#88047=DIRECTION('center_axis',(-0.0980734470899598,0.987363722027219,-0.124476822744034));
#88048=DIRECTION('ref_axis',(-0.744510117580016,0.0102046851999408,0.667533182112291));
#88049=DIRECTION('',(0.160317479600262,0.,-0.987065502251304));
#88050=DIRECTION('center_axis',(5.51791714416026E-15,-1.,-4.96514234470038E-15));
#88051=DIRECTION('ref_axis',(1.,5.51791714416026E-15,-2.12802080022765E-32));
#88052=DIRECTION('center_axis',(-0.0798423016345343,-0.987363723490078,
-0.136887122862264));
#88053=DIRECTION('ref_axis',(-0.793512025280663,-0.020156453595699,0.60822066975188));
#88054=DIRECTION('center_axis',(0.115688518554701,-0.987363722502104,0.10830072096439));
#88055=DIRECTION('ref_axis',(-0.741540431297166,-0.0133103684642173,0.6707761346701));
#88056=DIRECTION('center_axis',(0.0995325357866225,0.987363722369425,0.123313235577846));
#88057=DIRECTION('ref_axis',(-0.692946129975743,-0.0201568006358742,0.720707544250625));
#88058=DIRECTION('',(-0.998451978423991,0.,0.0556205607776269));
#88059=DIRECTION('center_axis',(-0.122539379018189,0.987363722035633,-0.100483734991179));
#88060=DIRECTION('ref_axis',(-0.583603983803612,0.0102046893186796,0.811974294177138));
#88061=DIRECTION('',(-0.0556205582211081,0.,-0.998451978566407));
#88062=DIRECTION('center_axis',(-1.72862098727961E-14,-1.,2.41409965901936E-14));
#88063=DIRECTION('ref_axis',(9.88397516767577E-33,-2.41409965901936E-14,
-1.));
#88064=DIRECTION('center_axis',(-0.107402317354723,-0.987363723483623,-0.116523043967242));
#88065=DIRECTION('ref_axis',(-0.644210689681965,-0.0201564546481271,0.764582438089906));
#88066=DIRECTION('center_axis',(0.136265238378703,-0.987363722512312,0.0808990993536073));
#88067=DIRECTION('ref_axis',(-0.580006587686311,-0.0133103675608265,0.814503033975858));
#88068=DIRECTION('center_axis',(0.123714219117736,0.987363722312337,0.0990336904776107));
#88069=DIRECTION('ref_axis',(-0.521814617623308,-0.0201568038489919,0.852820736200307));
#88070=DIRECTION('',(-0.963151949602078,0.,0.268957844239047));
#88071=DIRECTION('center_axis',(-0.141275510311441,0.987363722055667,-0.0717921343506458));
#88072=DIRECTION('ref_axis',(-0.395409175669361,0.0102046865097965,0.918448391674629));
#88073=DIRECTION('',(-0.268957842517579,0.,-0.963151950082794));
#88074=DIRECTION('center_axis',(-2.92311680908922E-15,-1.,6.8231544174374E-15));
#88075=DIRECTION('ref_axis',(2.66748257699467E-34,-6.8231544174374E-15,
-1.));
#88076=DIRECTION('center_axis',(-0.129940323516781,-0.987363723620263,-0.0907104712978803));
#88077=DIRECTION('ref_axis',(-0.464786779218364,-0.020156448623246,0.885193180860945));
#88078=DIRECTION('center_axis',(0.15047034847597,-0.987363722496393,0.0497147234487595));
#88079=DIRECTION('ref_axis',(-0.391352279647315,-0.0133103692467653,0.920144677366209));
#88080=DIRECTION('center_axis',(0.142111168500603,0.987363722413081,0.0701234301070469));
#88081=DIRECTION('ref_axis',(-0.326283630981388,-0.0201567959017054,0.945056980151238));
#88082=DIRECTION('',(-0.882816006173181,0.,0.469718957723056));
#88083=DIRECTION('center_axis',(-0.153405753362529,0.987363721980081,-0.0397436202794466));
#88084=DIRECTION('ref_axis',(-0.188725472417248,0.0102046916293933,0.981976863439071));
#88085=DIRECTION('',(-0.469718957703103,0.,-0.882816006183797));
#88086=DIRECTION('center_axis',(-5.55199781974273E-15,-1.,2.91680662988243E-14));
#88087=DIRECTION('ref_axis',(2.33192543151121E-32,-2.91680662988243E-14,
-1.));
#88088=DIRECTION('center_axis',(-0.146402458494853,-0.98736372329281,-0.0606563934966637));
#88089=DIRECTION('ref_axis',(-0.263629954398167,-0.0201564602306307,0.964413274615707));
#88090=DIRECTION('center_axis',(0.157639630785437,-0.987363722515614,0.0162057479290574));
#88091=DIRECTION('ref_axis',(-0.184398776981366,-0.013310365432533,0.982761377558067));
#88092=DIRECTION('center_axis',(0.153863152643811,0.987363722405411,0.0379342844434553));
#88093=DIRECTION('ref_axis',(-0.115495988358612,-0.0201567971821641,0.993103408613838));
#88094=DIRECTION('',(-0.761200566737353,0.,0.648516535794372));
#88095=DIRECTION('center_axis',(4.24038427100572E-16,-1.,1.48398242449089E-14));
#88096=DIRECTION('ref_axis',(0.0285626985677906,1.48458813213445E-14,0.999592002894444));
#88097=DIRECTION('center_axis',(-0.156018981952462,-0.987363723488661,-0.027766072987104));
#88098=DIRECTION('ref_axis',(-0.0501460873759626,-0.020156453209744,0.998538475630702));
#88099=DIRECTION('center_axis',(0.157437859804754,-0.987363722525233,-0.0180610005596111));
#88100=DIRECTION('ref_axis',(0.0311770128597521,-0.0133103713432087,0.999425248772438));
#88101=DIRECTION('center_axis',(-0.15836291534669,0.987363722037061,-0.00583673264922174));
#88102=DIRECTION('ref_axis',(0.0267828210981455,0.0102046897763596,0.999589188017054));
#88103=DIRECTION('',(-0.648516533598721,0.,-0.761200568607971));
#88104=DIRECTION('center_axis',(-0.152772347587519,-0.987363722802381,-0.0421128092914994));
#88105=DIRECTION('ref_axis',(-0.157501995156474,-0.0177427248486509,0.98735926452162));
#88106=DIRECTION('',(0.562367402337263,0.,0.826887480125585));
#88107=DIRECTION('',(0.826887478900179,0.,-0.562367404139061));
#88108=DIRECTION('center_axis',(0.154431764554222,-0.987363722245923,0.0355487002483153));
#88109=DIRECTION('ref_axis',(-0.290069428666578,-0.0109157762395627,0.956943348575104));
#88110=DIRECTION('center_axis',(-0.140147600738479,-0.987363722297262,-0.073969790445442));
#88111=DIRECTION('ref_axis',(-0.366072744817863,-0.017742741678619,0.930417078851867));
#88112=DIRECTION('',(0.371463198744195,1.74545579967425E-14,0.928447678643622));
#88113=DIRECTION('center_axis',(-6.93975744812286E-14,-1.,2.27170476996506E-13));
#88114=DIRECTION('ref_axis',(-2.59199074825716E-30,-2.27170476996506E-13,
-1.));
#88115=DIRECTION('center_axis',(0.149682997529586,0.98736372254829,0.0520372909185504));
#88116=DIRECTION('ref_axis',(-0.221888126663152,-0.0177430369618895,0.974910685081093));
#88117=DIRECTION('center_axis',(-0.147323592067659,0.987363722382119,-0.0583835502860794));
#88118=DIRECTION('ref_axis',(-0.294137870802051,0.0126220186732162,0.955679652187201));
#88119=DIRECTION('',(0.928447676446041,0.,-0.371463204236903));
#88120=DIRECTION('center_axis',(0.14317931371119,-0.987363722302444,0.0679158597549498));
#88121=DIRECTION('ref_axis',(-0.489002301735146,-0.0109157720263509,0.872214190906567));
#88122=DIRECTION('center_axis',(-0.120969709374198,-0.987363722292978,-0.102368009229828));
#88123=DIRECTION('ref_axis',(-0.557526335016047,-0.0177427418820099,0.829969626476827));
#88124=DIRECTION('',(0.163189789191805,1.74545580137922E-14,0.986594695254102));
#88125=DIRECTION('center_axis',(1.45762543762546E-14,-1.,-2.58676162557461E-14));
#88126=DIRECTION('ref_axis',(5.47887179583638E-31,2.58676162557461E-14,
-1.));
#88127=DIRECTION('center_axis',(0.134997009526047,0.987363722493814,0.0829981139676269));
#88128=DIRECTION('ref_axis',(-0.426277486400253,-0.0177430437136482,0.904418425834004));
#88129=DIRECTION('center_axis',(-0.131328509014908,0.987363722362473,-0.0886887956984518));
#88130=DIRECTION('ref_axis',(-0.492703966323166,0.0126220221773717,0.87010544540623));
#88131=DIRECTION('',(0.986594694898509,0.,-0.16318979134161));
#88132=DIRECTION('center_axis',(0.125231962048202,-0.987363722236187,0.0971073410894351));
#88133=DIRECTION('ref_axis',(-0.665069967527274,-0.0109157769681648,0.746701268317158));
#88134=DIRECTION('center_axis',(-0.0961354101537728,-0.98736372234748,-0.125979612266014));
#88135=DIRECTION('ref_axis',(-0.72291061702561,-0.0177427394115162,0.690713714204247));
#88136=DIRECTION('',(-0.0527141905833193,1.74545580647872E-14,0.998609640505811));
#88137=DIRECTION('center_axis',(0.,-1.,0.));
#88138=DIRECTION('ref_axis',(0.,0.,-1.));
#88139=DIRECTION('center_axis',(0.113998717626461,0.987363722533795,0.110078025980343));
#88140=DIRECTION('ref_axis',(-0.610734581675629,-0.0177430374931817,0.791636567729163));
#88141=DIRECTION('center_axis',(-0.109192650142314,0.987363722346366,-0.114847050241731));
#88142=DIRECTION('ref_axis',(-0.668231773767008,0.0126220244917432,0.743846073476179));
#88143=DIRECTION('',(0.998609640477331,0.,0.0527141911228425));
#88144=DIRECTION('center_axis',(0.10142890137495,-0.987363722244127,0.121758194640415));
#88145=DIRECTION('ref_axis',(-0.810039701366378,-0.0109157780792778,0.586273424264817));
#88146=DIRECTION('center_axis',(-0.0668059229653221,-0.98736372227003,-0.143700551849403));
#88147=DIRECTION('ref_axis',(-0.854492399176007,-0.0177427420873099,0.519160798648795));
#88148=DIRECTION('',(-0.266153317126965,1.74545580075932E-14,0.963930709015079));
#88149=DIRECTION('center_axis',(-7.22717411294479E-14,-1.,5.20692070645034E-14));
#88150=DIRECTION('ref_axis',(1.,-7.22717411294479E-14,-4.37574147480012E-31));
#88151=DIRECTION('center_axis',(0.0876699694622647,0.987363722548048,0.132010817172483));
#88152=DIRECTION('ref_axis',(-0.766634408653477,-0.0177430370136917,0.641838662053062));
#88153=DIRECTION('center_axis',(-0.0819510665657728,0.987363722349466,-0.135635181560458));
#88154=DIRECTION('ref_axis',(-0.812513804304486,0.0126220234218375,0.582805286814893));
#88155=DIRECTION('',(0.963930709595031,0.,0.266153315026547));
#88156=DIRECTION('center_axis',(0.072883141041351,-0.987363722228438,0.140715769475741));
#88157=DIRECTION('ref_axis',(-0.917132878973961,-0.0109157821110874,0.398432087068595));
#88158=DIRECTION('center_axis',(-0.034352670340833,-0.987363722390964,-0.154702209896024));
#88159=DIRECTION('ref_axis',(-0.946119067924401,-0.0177427377607601,0.323332498469633));
#88160=DIRECTION('',(-0.467147409756163,0.,0.884179448730917));
#88161=DIRECTION('center_axis',(-1.90809286004832E-13,-1.,8.24029964450493E-14));
#88162=DIRECTION('ref_axis',(1.,-1.90809286004832E-13,-8.4845030837726E-31));
#88163=DIRECTION('center_axis',(0.0572418717109346,0.987363722545232,0.147770929227133));
#88164=DIRECTION('ref_axis',(-0.886687261996754,-0.0177430360388344,0.462029094413786));
#88165=DIRECTION('center_axis',(-0.0508775416265985,0.987363722375924,-0.150081163021854));
#88166=DIRECTION('ref_axis',(-0.918803591807643,0.0126220233357556,0.394513173681547));
#88167=DIRECTION('',(0.884179450376195,0.,0.467147406642111));
#88168=DIRECTION('center_axis',(0.0409294380513989,-0.987363722261476,0.153093634951816));
#88169=DIRECTION('ref_axis',(-0.981341943275492,-0.0109157773140059,0.191960506807813));
#88170=DIRECTION('center_axis',(-0.000293123762934843,-0.98736372243561,
-0.15847016658209));
#88171=DIRECTION('ref_axis',(-0.99350625910852,-0.0177427362610183,0.112385534754992));
#88172=DIRECTION('',(-0.646298209424309,0.,0.763084939240012));
#88173=DIRECTION('center_axis',(-5.83035654598321E-14,-1.,1.12737439807136E-14));
#88174=DIRECTION('ref_axis',(1.,-5.83035654598321E-14,1.9003774831539E-31));
#88175=DIRECTION('center_axis',(0.0241372029392072,0.987363722544784,0.156621437985924));
#88176=DIRECTION('ref_axis',(-0.96527960424997,-0.017743040055254,0.260615560066199));
#88177=DIRECTION('center_axis',(-0.0174250414748936,0.987363722392953,-0.157509516004368));
#88178=DIRECTION('ref_axis',(-0.982131145014957,0.0126220211409558,0.187774062569692));
#88179=DIRECTION('',(0.763084941849124,0.,0.646298206343728));
#88180=DIRECTION('center_axis',(0.0070619211713651,-0.987363722269307,0.158313010254586));
#88181=DIRECTION('ref_axis',(-0.999664548667799,-0.0109157740318901,-0.0234869328370264));
#88182=DIRECTION('center_axis',(0.0337801346917581,-0.987363722339333,-0.154828234855351));
#88183=DIRECTION('ref_axis',(-0.994438202640106,-0.0177427401627641,-0.103816454868353));
#88184=DIRECTION('',(-0.795228820662645,0.,0.606309428252191));
#88185=DIRECTION('center_axis',(-1.48409955798332E-13,-1.,-3.80843256108542E-15));
#88186=DIRECTION('ref_axis',(-0.999670904433375,1.48458812936906E-13,-0.0256531251382206));
#88187=DIRECTION('center_axis',(-0.0100960892824427,0.987363722538594,0.158148501086578));
#88188=DIRECTION('ref_axis',(-0.998736545245237,-0.0177430383254438,0.0470159311573217));
#88189=DIRECTION('center_axis',(0.0168422419368752,0.987363722326255,-0.157572899702271));
#88190=DIRECTION('ref_axis',(-0.999535337432634,0.0126220267804277,-0.0277451556741776));
#88191=DIRECTION('',(0.606309431371119,0.,0.795228818284669));
#88192=DIRECTION('center_axis',(-0.0271357980096675,-0.987363722266527,
0.156129844739459));
#88193=DIRECTION('ref_axis',(-0.971243950925299,-0.0109157760761481,-0.237836148689955));
#88194=DIRECTION('center_axis',(0.0662738680381684,-0.987363722346358,-0.143946706143641));
#88195=DIRECTION('ref_axis',(-0.948871320917237,-0.017742740453389,-0.315164102495797));
#88196=DIRECTION('',(-0.906975416896829,0.,0.421183562291816));
#88197=DIRECTION('center_axis',(-5.76486051496427E-14,-1.,-1.4249258802016E-14));
#88198=DIRECTION('ref_axis',(1.,-5.76486051496427E-14,-7.94905549468724E-31));
#88199=DIRECTION('center_axis',(-0.0438573035860945,0.987363722504216,0.152280715800702));
#88200=DIRECTION('ref_axis',(-0.98549367499417,-0.0177430405640933,-0.168782111190805));
#88201=DIRECTION('center_axis',(0.0503219900885229,0.987363722369066,-0.150268350170727));
#88202=DIRECTION('ref_axis',(-0.970202368722082,0.0126220214997916,-0.241967039696155));
#88203=DIRECTION('',(0.421183564268127,0.,0.906975415979064));
#88204=DIRECTION('center_axis',(-0.0600646816443866,-0.98736372228547,0.146646220317949));
#88205=DIRECTION('ref_axis',(-0.897409065200425,-0.0109157738880786,-0.441064412049447));
#88206=DIRECTION('center_axis',(0.0956687123460396,-0.987363722218188,-0.126334387739427));
#88207=DIRECTION('ref_axis',(-0.858936270142699,-0.017742744429567,-0.511775027578971));
#88208=DIRECTION('',(-0.976312851284768,0.,0.216363620824314));
#88209=DIRECTION('center_axis',(-5.32376433741381E-14,-1.,-2.63088650808751E-14));
#88210=DIRECTION('ref_axis',(1.,-5.32376433741381E-14,-1.03806303605968E-30));
#88211=DIRECTION('center_axis',(-0.0755677974580308,0.987363722503259,0.139292453032636));
#88212=DIRECTION('ref_axis',(-0.926170215653369,-0.0177430413683588,-0.376688088635137));
#88213=DIRECTION('center_axis',(0.0814487424077611,0.987363722364132,-0.13593741986458));
#88214=DIRECTION('ref_axis',(-0.895503815254515,0.0126220203453105,-0.444874815500957));
#88215=DIRECTION('',(0.216363620211501,0.,0.976312851420575));
#88216=DIRECTION('center_axis',(-0.0901850061830041,-0.987363722271896,
0.130305581619351));
#88217=DIRECTION('ref_axis',(-0.781612328340454,-0.0109157730780283,-0.623668994005893));
#88218=DIRECTION('center_axis',(0.120590189003312,-0.987363722259253,-0.102814815481514));
#88219=DIRECTION('ref_axis',(-0.728838316062047,-0.0177427435776927,-0.684455918295822));
#88220=DIRECTION('',(-0.999998982187443,0.,0.0014267529843288));
#88221=DIRECTION('center_axis',(2.31686742770819E-14,-1.,1.85691490357775E-14));
#88222=DIRECTION('ref_axis',(1.,2.31686742770819E-14,-7.24715462217508E-31));
#88223=DIRECTION('center_axis',(-0.103744820256812,0.987363722562306,0.119791033211119));
#88224=DIRECTION('ref_axis',(-0.823540068225522,-0.0177430367518507,-0.5669805469978));
#88225=DIRECTION('center_axis',(0.108767043471548,0.98736372236086,-0.11525020616105));
#88226=DIRECTION('ref_axis',(-0.778932498628811,0.0126220208625128,-0.626980739073556));
#88227=DIRECTION('',(0.00142675803820793,0.,0.999998982180232));
#88228=DIRECTION('center_axis',(-0.116088374672241,-0.987363722232209,0.107872004179562));
#88229=DIRECTION('ref_axis',(-0.629268269566731,-0.0109157796553593,-0.777111504657477));
#88230=DIRECTION('center_axis',(0.139873000841585,-0.987363722359222,-0.0744877399610901));
#88231=DIRECTION('ref_axis',(-0.564660688619854,-0.0177427383955641,-0.825132414804786));
#88232=DIRECTION('',(-0.976926272040803,0.,-0.213576822236072));
#88233=DIRECTION('center_axis',(3.72703708254283E-14,-1.,4.62311855372118E-14));
#88234=DIRECTION('ref_axis',(-1.04756410853878E-30,-4.62311855372118E-14,
-1.));
#88235=DIRECTION('center_axis',(-0.127070855555912,0.987363722556134,0.0946883152684742));
#88236=DIRECTION('ref_axis',(-0.682402100079866,-0.0177430371157247,-0.730761629014892));
#88237=DIRECTION('center_axis',(0.130999521498712,0.987363722324349,-0.0891740164224692));
#88238=DIRECTION('ref_axis',(-0.625939163365759,0.0126220266765779,-0.779769740505201));
#88239=DIRECTION('',(-0.213576822851012,0.,0.976926271906364));
#88240=DIRECTION('center_axis',(-0.13656358601598,-0.987363722260568,0.0803944459413213));
#88241=DIRECTION('ref_axis',(-0.447500324708907,-0.0109157777619702,-0.894217146548462));
#88242=DIRECTION('center_axis',(0.15261550972507,-0.987363722385411,-0.0426776980234713));
#88243=DIRECTION('ref_axis',(-0.374080159221782,-0.0177427380813195,-0.927226633419243));
#88244=DIRECTION('',(-0.908173574914686,0.,-0.418593786177817));
#88245=DIRECTION('center_axis',(-3.96910079242655E-14,-1.,-7.97435311668676E-14));
#88246=DIRECTION('ref_axis',(-2.13334119177811E-30,7.97435311668676E-14,
-1.));
#88247=DIRECTION('center_axis',(-0.144455199096664,0.987363722535034,0.065158076058957));
#88248=DIRECTION('ref_axis',(-0.509355770290959,-0.0177430388022161,-0.860373107346671));
#88249=DIRECTION('center_axis',(0.147106601607187,0.987363722352517,-0.0589281557981135));
#88250=DIRECTION('ref_axis',(-0.443677609396436,0.0126220232229998,-0.896097574737272));
#88251=DIRECTION('',(-0.418593784198901,0.,0.908173575826804));
#88252=DIRECTION('center_axis',(-0.15065323545887,-0.987363722271498,0.0491577317209224));
#88253=DIRECTION('ref_axis',(-0.244807760987597,-0.0109157752669287,-0.969510188709));
#88254=DIRECTION('center_axis',(0.158221887782401,-0.987363722345595,-0.00887209233635914));
#88255=DIRECTION('ref_axis',(-0.166008055151417,-0.0177427396082325,-0.98596476651858));
#88256=DIRECTION('',(-0.796955690039799,0.,-0.604037770435913));
#88257=DIRECTION('center_axis',(-2.16205522115258E-14,-1.,-8.64115651514208E-14));
#88258=DIRECTION('ref_axis',(4.82917687363763E-31,8.64115651514208E-14,
-1.));
#88259=DIRECTION('center_axis',(-0.155084977231928,0.987363722540378,0.0325811179700883));
#88260=DIRECTION('ref_axis',(-0.312492527935681,-0.0177430392379542,-0.949754496984862));
#88261=DIRECTION('center_axis',(0.156335143187237,0.987363722338763,-0.0259268743578526));
#88262=DIRECTION('ref_axis',(-0.24067018291622,0.0126220262462275,-0.970524882477782));
#88263=DIRECTION('',(-0.604037768699346,0.,0.796955691355997));
#88264=DIRECTION('',(-0.648473045044079,0.,-0.761237617207177));
#88265=DIRECTION('',(-0.761237617213291,0.,0.648473045036901));
#88266=DIRECTION('center_axis',(-0.157369969703018,-0.987363722263388,-0.0186432988995479));
#88267=DIRECTION('ref_axis',(0.184905254470325,-0.0109157789351342,-0.98269572739455));
#88268=DIRECTION('center_axis',(0.147323590960846,-0.987363722315772,0.0583835542010283));
#88269=DIRECTION('ref_axis',(0.263331029590432,-0.0177427404521949,-0.964542359886848));
#88270=DIRECTION('',(-0.469668516573739,0.,-0.882842842492039));
#88271=DIRECTION('center_axis',(2.77683211871253E-14,-1.,-1.45838744591726E-13));
#88272=DIRECTION('ref_axis',(-1.75617357726029E-31,1.45838744591726E-13,
-1.));
#88273=DIRECTION('center_axis',(-0.154431769535767,0.987363722528783,-0.0355486707508934));
#88274=DIRECTION('ref_axis',(0.115181024600642,-0.0177430401713234,-0.993186043044013));
#88275=DIRECTION('center_axis',(0.152772346306646,0.987363722381786,0.0421128237992417));
#88276=DIRECTION('ref_axis',(0.189086477475989,0.0126220211157706,-0.981879314691309));
#88277=DIRECTION('',(-0.882842840276596,0.,0.46966852073814));
#88278=DIRECTION('center_axis',(-0.149682990353858,-0.98736372222389,-0.0520373177144283));
#88279=DIRECTION('ref_axis',(0.39183280570531,-0.0109157821600972,-0.919971683299512));
#88280=DIRECTION('center_axis',(0.131328508972608,-0.987363722350935,0.0886887958895417));
#88281=DIRECTION('ref_axis',(0.464522591751889,-0.017742740090601,-0.885383508388419));
#88282=DIRECTION('',(-0.268902815661671,0.,-0.963167314504196));
#88283=DIRECTION('center_axis',(-1.16940264748932E-14,-1.,2.72919495009907E-14));
#88284=DIRECTION('ref_axis',(1.20821244774943E-32,-2.72919495009907E-14,
-1.));
#88285=DIRECTION('center_axis',(-0.143179326462339,0.987363722500805,-0.0679158299893592));
#88286=DIRECTION('ref_axis',(0.325993798533084,-0.0177430420158487,-0.945205389202788));
#88287=DIRECTION('center_axis',(0.140147601725461,0.987363722386407,0.0739697873855303));
#88288=DIRECTION('ref_axis',(0.395740769282578,0.0126220205100963,-0.918275518635816));
#88289=DIRECTION('',(-0.963167313918257,0.,0.268902817760414));
#88290=DIRECTION('center_axis',(-0.134996993412494,-0.987363722305443,-0.0829981424173244));
#88291=DIRECTION('ref_axis',(0.58043869111259,-0.0109157701802117,-0.814230785355649));
#88292=DIRECTION('center_axis',(0.10919265044991,-0.987363722260612,0.114847050686525));
#88293=DIRECTION('ref_axis',(0.643993593304886,-0.0177427429237519,-0.764825108672436));
#88294=DIRECTION('',(-0.0555635134513151,0.,-0.998455154712992));
#88295=DIRECTION('center_axis',(8.64379451953179E-14,-1.,-1.2070004440453E-13));
#88296=DIRECTION('ref_axis',(3.17309577792907E-30,1.2070004440453E-13,-1.));
#88297=DIRECTION('center_axis',(-0.125231977120001,0.987363722511643,-0.0971073188517023));
#88298=DIRECTION('ref_axis',(0.52156346317154,-0.0177430425746461,-0.853027982146368));
#88299=DIRECTION('center_axis',(0.120969709501029,0.987363722336303,0.102368008662062));
#88300=DIRECTION('ref_axis',(0.5838906615892,0.012622023301845,-0.811734180527526));
#88301=DIRECTION('',(-0.99845515443243,0.,0.0555635184929094));
#88302=DIRECTION('center_axis',(-0.113998700166117,-0.987363722223595,-0.11007804684497));
#88303=DIRECTION('ref_axis',(0.741903905967849,-0.0109157819403093,-0.670417362554313));
#88304=DIRECTION('center_axis',(0.0819510669257577,-0.987363722306909,0.135635181652755));
#88305=DIRECTION('ref_axis',(0.793352172628083,-0.0177427411803675,-0.608504334677828));
#88306=DIRECTION('',(0.160373871797992,0.,-0.987056341474245));
#88307=DIRECTION('center_axis',(8.82912126861344E-14,-1.,-7.94372331205514E-14));
#88308=DIRECTION('ref_axis',(1.,8.82912126861344E-14,4.09990452814717E-30));
#88309=DIRECTION('center_axis',(-0.101428922427798,0.987363722514867,-0.121758174907153));
#88310=DIRECTION('ref_axis',(0.692745400016714,-0.017743039406182,-0.720963934818042));
#88311=DIRECTION('center_axis',(0.0961354074716145,0.98736372232858,0.125979614460904));
#88312=DIRECTION('ref_axis',(0.744738477174182,0.0126220251617332,-0.6672370531506));
#88313=DIRECTION('',(-0.987056341368623,0.,-0.160373872448067));
#88314=DIRECTION('center_axis',(-0.0876699454717902,-0.987363722241175,
-0.132010835400075));
#88315=DIRECTION('ref_axis',(0.868678520543038,-0.0109157792923925,-0.495255967868736));
#88316=DIRECTION('center_axis',(0.0508775419888311,-0.987363722325599,0.150081163230142));
#88317=DIRECTION('ref_axis',(0.905614485029377,-0.0177427407083583,-0.423730574371417));
#88318=DIRECTION('',(0.36881235729421,0.,-0.929503870409956));
#88319=DIRECTION('center_axis',(-1.2912958762935E-13,-1.,7.32500423227334E-14));
#88320=DIRECTION('ref_axis',(1.,-1.2912958762935E-13,-3.62494059594665E-30));
#88321=DIRECTION('center_axis',(-0.0728831642249594,0.987363722545768,-0.140715755241269));
#88322=DIRECTION('ref_axis',(0.831535330186537,-0.0177430374288357,-0.555188417813597));
#88323=DIRECTION('center_axis',(0.0668059227393821,0.987363722362798,0.143700551317036));
#88324=DIRECTION('ref_axis',(0.870763148538878,0.0126220240826978,-0.491540663276922));
#88325=DIRECTION('',(-0.929503871604648,0.,-0.368812354283272));
#88326=DIRECTION('center_axis',(-0.0572418399771415,-0.987363722286597,
-0.147770943247942));
#88327=DIRECTION('ref_axis',(0.954834693482862,-0.010915775899325,-0.296936952833434));
#88328=DIRECTION('center_axis',(0.017425041224431,-0.987363722356895,0.157509516258108));
#88329=DIRECTION('ref_axis',(0.975531269058269,-0.0177427395283381,-0.219143647600366));
#88330=DIRECTION('',(0.560005585107136,0.,-0.828488831939704));
#88331=DIRECTION('center_axis',(-1.13485762705073E-13,-1.,3.50227621756936E-14));
#88332=DIRECTION('ref_axis',(1.,-1.13485762705073E-13,1.22045136905081E-30));
#88333=DIRECTION('center_axis',(-0.0409294637811914,0.987363722509901,-0.153093626470785));
#88334=DIRECTION('ref_axis',(0.931443595764125,-0.0177430419875243,-0.363452902548632));
#88335=DIRECTION('center_axis',(0.0343526699419355,0.987363722367053,0.154702210137208));
#88336=DIRECTION('ref_axis',(0.956071902701323,0.0126220207023251,-0.292860378778798));
#88337=DIRECTION('',(-0.828488832258417,0.,-0.560005584635622));
#88338=DIRECTION('center_axis',(-0.0241371697553315,-0.987363722282063,
-0.156621444756176));
#88339=DIRECTION('ref_axis',(0.996343856436258,-0.0109157726890224,-0.0847334977935284));
#88340=DIRECTION('center_axis',(-0.0168422380496672,-0.987363722328066,
0.157572900106406));
#88341=DIRECTION('ref_axis',(0.999833296486313,-0.0177427405920249,-0.0043098020368813));
#88342=DIRECTION('',(0.725013574350737,0.,-0.688734576602023));
#88343=DIRECTION('center_axis',(-1.77542081017899E-13,-1.,1.47117976467656E-14));
#88344=DIRECTION('ref_axis',(1.,-1.77542081017899E-13,3.24326134236472E-31));
#88345=DIRECTION('center_axis',(-0.00706195171111479,0.987363722497818,
-0.158313007467113));
#88346=DIRECTION('ref_axis',(0.987798592454597,-0.0177430417900404,-0.154722736573373));
#88347=DIRECTION('center_axis',(0.000293118801652807,0.987363722357134,
0.158470167080217));
#88348=DIRECTION('ref_axis',(0.996675797480111,0.0126220232240424,-0.0804862674443004));
#88349=DIRECTION('',(-0.68873457818185,0.,-0.725013572849964));
#88350=DIRECTION('center_axis',(0.0100961238614255,-0.9873637222979,-0.158148500381796));
#88351=DIRECTION('ref_axis',(0.991265088020046,-0.0109157736626055,0.131432002031304));
#88352=DIRECTION('center_axis',(-0.0503219922735293,-0.987363722301029,
0.150268349886061));
#88353=DIRECTION('ref_axis',(0.977384229993961,-0.0177427415408041,0.210725561054484));
#88354=DIRECTION('',(0.856120735019485,0.,-0.51677585766916));
#88355=DIRECTION('center_axis',(-5.88512824280692E-14,-1.,-7.93281843200647E-15));
#88356=DIRECTION('ref_axis',(1.,-5.88512824280692E-14,1.0842198170146E-31));
#88357=DIRECTION('center_axis',(0.0271357676639449,0.987363722543269,-0.156129848263511));
#88358=DIRECTION('ref_axis',(0.997965225106375,-0.0177430396859387,0.0612420935393733));
#88359=DIRECTION('center_axis',(-0.033780134470556,0.987363722380125,0.154828234643471));
#88360=DIRECTION('ref_axis',(0.990676239571682,0.0126220219592833,0.135651291589024));
#88361=DIRECTION('',(-0.516775860806531,0.,-0.85612073312569));
#88362=DIRECTION('center_axis',(0.0438573361251434,-0.987363722295469,-0.152280707782841));
#88363=DIRECTION('ref_axis',(0.939835865763662,-0.0109157723346735,0.341451887296887));
#88364=DIRECTION('center_axis',(-0.0814487486910026,-0.98736372219626,0.135937417319212));
#88365=DIRECTION('ref_axis',(0.909233762600149,-0.0177427448865258,0.41590763391872));
#88366=DIRECTION('',(0.947196641515208,0.,-0.32065327427349));
#88367=DIRECTION('center_axis',(-5.5770050700255E-14,-1.,-2.03986396420233E-14));
#88368=DIRECTION('ref_axis',(1.,-5.5770050700255E-14,-5.63063762659705E-31));
#88369=DIRECTION('center_axis',(0.0600646471800081,0.987363722582821,-0.146646232432119));
#88370=DIRECTION('ref_axis',(0.961468112966299,-0.0177430359170283,0.274343311246094));
#88371=DIRECTION('center_axis',(-0.0662738702393048,0.987363722336531,0.143946705197631));
#88372=DIRECTION('ref_axis',(0.938353761907754,0.0126220250365005,0.345445946564067));
#88373=DIRECTION('',(-0.32065327633744,0.,-0.947196640816502));
#88374=DIRECTION('center_axis',(0.0755678252582836,-0.987363722276059,-0.139292439561156));
#88375=DIRECTION('ref_axis',(0.844460963137086,-0.0109157740894685,0.535505861418541));
#88376=DIRECTION('center_axis',(-0.108767043096074,-0.987363722378186,0.115250206366968));
#88377=DIRECTION('ref_axis',(0.79856853679574,-0.0177427385073159,0.601642325032217));
#88378=DIRECTION('',(0.993982686191135,0.,-0.109537297539496));
#88379=DIRECTION('center_axis',(-5.00810733926824E-14,-1.,-3.1910643155052E-14));
#88380=DIRECTION('ref_axis',(1.,-5.00810733926824E-14,-1.71968141652445E-31));
#88381=DIRECTION('center_axis',(0.0901849763727487,0.987363722522623,-0.130305600351315));
#88382=DIRECTION('ref_axis',(0.88001382101897,-0.0177430385210899,0.474616539323728));
#88383=DIRECTION('center_axis',(-0.095668707141692,0.98736372237429,0.126334390460485));
#88384=DIRECTION('ref_axis',(0.842154904786648,0.0126220207242787,0.539087934326699));
#88385=DIRECTION('',(-0.109537302858737,0.,-0.993982685604952));
#88386=DIRECTION('center_axis',(0.103744844987445,-0.987363722267051,-0.119791014226798));
#88387=DIRECTION('ref_axis',(0.709600004588852,-0.0109157788340079,0.704520176616645));
#88388=DIRECTION('center_axis',(-0.130999520459926,-0.987363722265585,0.0891740185991351));
#88389=DIRECTION('ref_axis',(0.650563131571766,-0.0177427423106625,0.759244892597134));
#88390=DIRECTION('',(0.994291204618493,1.7454558011431E-14,0.106700517422864));
#88391=DIRECTION('center_axis',(4.20503607033623E-14,-1.,4.19305404221689E-14));
#88392=DIRECTION('ref_axis',(1.,4.20503607033623E-14,1.91185012013183E-30));
#88393=DIRECTION('center_axis',(0.116088354229398,0.987363722546353,-0.107872023304093));
#88394=DIRECTION('ref_axis',(0.757411060199225,-0.017743038907888,0.652697227248744));
#88395=DIRECTION('center_axis',(-0.120590188318903,0.987363722333388,0.102814815572313));
#88396=DIRECTION('ref_axis',(0.706577820236583,0.0126220248222844,0.70752276884854));
#88397=DIRECTION('',(0.106700515256271,0.,-0.994291204850996));
#88398=DIRECTION('center_axis',(0.12707087651531,-0.9873637222525,-0.0946882903072925));
#88399=DIRECTION('ref_axis',(0.541558938450353,-0.0109157767576206,0.840591911692174));
#88400=DIRECTION('center_axis',(-0.147106602631027,-0.98736372225952,0.0589281548004195));
#88401=DIRECTION('ref_axis',(0.472138117688431,-0.0177427424578752,0.881346012026887));
#88402=DIRECTION('',(0.948107771776315,0.,0.317949136022339));
#88403=DIRECTION('center_axis',(-4.80801298667729E-14,-1.,-7.49847183820041E-14));
#88404=DIRECTION('ref_axis',(2.14746148769039E-30,7.49847183820041E-14,
-1.));
#88405=DIRECTION('center_axis',(0.136563571728994,0.987363722495015,-0.0803944673308284));
#88406=DIRECTION('ref_axis',(0.599392599870526,-0.0177430430396784,0.800258518007864));
#88407=DIRECTION('center_axis',(-0.139873001359505,0.987363722361872,0.0744877389534123));
#88408=DIRECTION('ref_axis',(0.537961943656821,0.012622022091116,0.842874623971624));
#88409=DIRECTION('',(0.317949136540617,0.,-0.948107771602509));
#88410=DIRECTION('center_axis',(0.144455213172839,-0.987363722247192,-0.0651580492138836));
#88411=DIRECTION('ref_axis',(0.348195179853326,-0.0109157773107122,0.937358502672597));
#88412=DIRECTION('center_axis',(-0.15633514206494,-0.98736372237218,0.0259268798525389));
#88413=DIRECTION('ref_axis',(0.271636452700257,-0.0177427388279761,0.962236370536524));
#88414=DIRECTION('',(0.857591872604232,1.74545580696915E-14,0.514330807985645));
#88415=DIRECTION('center_axis',(0.,-1.,0.));
#88416=DIRECTION('ref_axis',(0.,0.,-1.));
#88417=DIRECTION('center_axis',(0.150653225068599,0.987363722493285,-0.0491577591091539));
#88418=DIRECTION('ref_axis',(0.413347208971823,-0.0177430422692839,0.910400609229934));
#88419=DIRECTION('center_axis',(-0.15261550883066,0.987363722410109,0.0426777006504942));
#88420=DIRECTION('ref_axis',(0.344191563648143,0.0126220174954829,0.938814599475205));
#88421=DIRECTION('',(0.514330808231272,0.,-0.85759187245692));
#88422=DIRECTION('center_axis',(0.155084985394089,-0.987363722264602,-0.0325810874757932));
#88423=DIRECTION('ref_axis',(0.138550198822444,-0.0109157754770187,0.990295253069506));
#88424=DIRECTION('center_axis',(-0.158253626581311,-0.98736372226607,-0.00828671386947175));
#88425=DIRECTION('ref_axis',(0.0584333675298601,-0.0177427423121442,0.998133626652446));
#88426=DIRECTION('',(0.726975930476597,0.,0.686662942430772));
#88427=DIRECTION('center_axis',(2.4302156024229E-14,-1.,1.76485219614137E-13));
#88428=DIRECTION('ref_axis',(1.46250166471626E-31,-1.76485219614137E-13,
-1.));
#88429=DIRECTION('center_axis',(0.157698501290677,0.987363722511173,-0.0156224889039468));
#88430=DIRECTION('ref_axis',(0.207974160398467,-0.0177430411066726,0.97797338056761));
#88431=DIRECTION('center_axis',(-0.158221887463882,0.987363722382384,0.00887209392241986));
#88432=DIRECTION('ref_axis',(0.13432716864759,0.0126220202709485,0.990856647738411));
#88433=DIRECTION('center_axis',(-1.18376001797387E-14,-1.,1.47986115205468E-13));
#88434=DIRECTION('ref_axis',(5.1637282516317E-31,-1.47986115205468E-13,
-1.));
#88435=DIRECTION('center_axis',(0.158463155145865,-0.987363722292628,0.00151932934686073));
#88436=DIRECTION('ref_axis',(-0.0775732331348036,-0.0109157737333195,0.996926897713577));
#88437=DIRECTION('center_axis',(0.157369971174573,0.987363722509919,0.018643273421546));
#88438=DIRECTION('ref_axis',(-0.00712352888697095,-0.0177430419567505,0.999817203191822));
#88439=DIRECTION('center_axis',(-0.156429985687579,0.987363722414907,-0.0253483576738535));
#88440=DIRECTION('ref_axis',(-0.0818182158823528,0.0126220183822201,0.996567340525359));
#88441=DIRECTION('',(0.686662939327361,0.,-0.726975933407915));
#88442=DIRECTION('center_axis',(0.162023728744164,-0.986495108954454,-0.0239939853458685));
#88443=DIRECTION('ref_axis',(0.0324773729665821,-0.0189711050413171,0.99929240836639));
#88444=DIRECTION('center_axis',(0.153077706971466,-0.986495108938772,-0.058263330390891));
#88445=DIRECTION('ref_axis',(0.246536396631873,-0.018971104116629,0.968947832622772));
#88446=DIRECTION('center_axis',(0.13697394371636,-0.986495108875294,-0.0898083454246302));
#88447=DIRECTION('ref_axis',(0.44906765042969,-0.0189711014311051,0.893296335293081));
#88448=DIRECTION('center_axis',(0.114465436194755,-0.986495109078521,-0.117154016921752));
#88449=DIRECTION('ref_axis',(0.630601004724684,-0.0189710906652105,0.775875293174871));
#88450=DIRECTION('center_axis',(0.0866046342375456,-0.986495108953145,-0.139021715354488));
#88451=DIRECTION('ref_axis',(0.782648160233291,-0.0189711058178337,0.622175179854913));
#88452=DIRECTION('center_axis',(0.0546943161535251,-0.986495108922816,-0.154388898084867));
#88453=DIRECTION('ref_axis',(0.898099551017545,-0.0189710967552618,0.439382855776128));
#88454=DIRECTION('center_axis',(0.0202265331475369,-0.986495108893428,-0.162537034198902));
#88455=DIRECTION('ref_axis',(0.971556809872428,-0.0189711067873972,0.236045466590173));
#88456=DIRECTION('center_axis',(-0.0151870056510711,-0.986495108979521,
-0.163085115258372));
#88457=DIRECTION('ref_axis',(0.999585149477771,-0.0189711027994199,0.0216708606676361));
#88458=DIRECTION('center_axis',(-0.0498904087762942,-0.986495109002119,
-0.156007522341176));
#88459=DIRECTION('ref_axis',(0.980873999808598,-0.018971090818931,-0.1937170467786));
#88460=DIRECTION('center_axis',(-0.0822610132790794,-0.986495109022473,
-0.141635184784849));
#88461=DIRECTION('ref_axis',(0.916298269164019,-0.018971100014056,-0.400046971356214));
#88462=DIRECTION('center_axis',(-0.110785172696402,-0.986495108908185,-0.120640149249146));
#88463=DIRECTION('ref_axis',(0.808877454441714,-0.0189710978365288,-0.587671133494551));
#88464=DIRECTION('center_axis',(-0.134129138216128,-0.986495109061941,-0.0940041173474185));
#88465=DIRECTION('ref_axis',(0.663634428213268,-0.0189710911115877,-0.747816450335298));
#88466=DIRECTION('center_axis',(-0.151201382438819,-0.986495108951864,-0.062972549278554));
#88467=DIRECTION('ref_axis',(0.487360592554928,-0.018971096011209,-0.872994702355428));
#88468=DIRECTION('center_axis',(-0.16120361374351,-0.986495109028429,-0.0289964614913726));
#88469=DIRECTION('ref_axis',(0.288298316451173,-0.0189710924938625,-0.957352692784122));
#88470=DIRECTION('center_axis',(-0.163668145749564,-0.986495108828605,0.00633548136598124));
#88471=DIRECTION('ref_axis',(0.0757555315809696,-0.0189711024502777,-0.996945934695912));
#88472=DIRECTION('center_axis',(-0.158479734362203,-0.986495108855783,0.0413711735403188));
#88473=DIRECTION('ref_axis',(-0.140329497611904,-0.0189711012108083,-0.98992309267884));
#88474=DIRECTION('center_axis',(-0.145880991273112,-0.986495109095868,0.0744723849161958));
#88475=DIRECTION('ref_axis',(-0.349852873668116,-0.01897108864457,-0.936612547738819));
#88476=DIRECTION('center_axis',(-0.126461011979806,-0.986495109024855,0.104091365247475));
#88477=DIRECTION('ref_axis',(-0.543017521318959,-0.0189710911169627,-0.839507039423998));
#88478=DIRECTION('center_axis',(-0.101127849063559,-0.986495108878455,0.128843153883565));
#88479=DIRECTION('ref_axis',(-0.710791271527493,-0.0189711022124235,-0.703147115190823));
#88480=DIRECTION('center_axis',(-0.0710660688100426,-0.986495108919276,
0.147570369458886));
#88481=DIRECTION('ref_axis',(-0.845329211087288,-0.0189710997746033,-0.533908814551591));
#88482=DIRECTION('center_axis',(-0.0376813248201236,-0.986495109040278,
0.159397357567215));
#88483=DIRECTION('ref_axis',(-0.940340495999881,-0.0189710911884959,-0.339705533192815));
#88484=DIRECTION('center_axis',(-0.00253463197808244,-0.986495108968311,
0.163771107410113));
#88485=DIRECTION('ref_axis',(-0.991382506037285,-0.0189710951273427,-0.129617993630908));
#88486=DIRECTION('center_axis',(0.0327305710932476,-0.986495108991966,0.160487101197692));
#88487=DIRECTION('ref_axis',(-0.996068571300047,-0.0189710930823987,0.0865303351174733));
#88488=DIRECTION('center_axis',(0.0664653398970494,-0.986495109036314,0.149698892580411));
#88489=DIRECTION('ref_axis',(-0.954179575331009,-0.0189711015572081,0.298632609282444));
#88490=DIRECTION('center_axis',(0.0970922492532798,-0.986495108967022,0.131910936313417));
#88491=DIRECTION('ref_axis',(-0.86767420750609,-0.018971096596724,0.496771141596003));
#88492=DIRECTION('center_axis',(0.123179242181962,-0.986495108881639,0.107954964907041));
#88493=DIRECTION('ref_axis',(-0.740597354552622,-0.0189711014686376,0.67168121585967));
#88494=DIRECTION('center_axis',(0.143506499163671,-0.986495109075195,0.0789511524203817));
#88495=DIRECTION('ref_axis',(-0.578890995779445,-0.018971089074444,0.815184220151993));
#88496=DIRECTION('center_axis',(0.157123563074936,-0.986495109019346,0.0462556570329008));
#88497=DIRECTION('ref_axis',(-0.390116332765927,-0.0189710950778334,0.920570119252636));
#88498=DIRECTION('center_axis',(0.163393702153687,-0.986495108818127,0.0113972968033836));
#88499=DIRECTION('ref_axis',(-0.183100264679772,-0.0189711023189716,0.982911181313449));
#88500=DIRECTION('center_axis',(-0.160735574475915,0.986495108729145,-0.03148770476503));
#88501=DIRECTION('ref_axis',(-0.0827414017722213,0.0183223861287446,0.996402604673089));
#88502=DIRECTION('center_axis',(0.156388933187229,0.986495109513922,0.0486816236548836));
#88503=DIRECTION('ref_axis',(-0.189986493512465,-0.0183223028001626,0.981615721911043));
#88504=DIRECTION('center_axis',(-0.150208708155227,0.986495107965014,-0.0653050224365125));
#88505=DIRECTION('ref_axis',(-0.295004101909852,0.0183224712765873,0.955320295452096));
#88506=DIRECTION('center_axis',(0.142267533730559,0.986495109449251,0.0811624782700377));
#88507=DIRECTION('ref_axis',(-0.39656307898551,-0.018322309651865,0.917824611434316));
#88508=DIRECTION('center_axis',(-0.132658262707296,0.986495107927723,-0.0960686596666776));
#88509=DIRECTION('ref_axis',(-0.493472694787282,0.0183224713738039,0.869568275952));
#88510=DIRECTION('center_axis',(0.121493864981184,0.986495109445291,0.109848258122087));
#88511=DIRECTION('ref_axis',(-0.584596816960018,-0.0183223081336044,0.811117041261539));
#88512=DIRECTION('center_axis',(-0.108904868035384,0.986495107974999,-0.122340229113693));
#88513=DIRECTION('ref_axis',(-0.668867050422418,0.0183224663674009,0.743156212438158));
#88514=DIRECTION('center_axis',(0.0950392813517184,0.986495109507679,0.133397653343611));
#88515=DIRECTION('ref_axis',(-0.745295455580775,-0.0183223031322053,0.666482540730495));
#88516=DIRECTION('center_axis',(-0.0800591980640834,0.986495108016897,-0.142891310666767));
#88517=DIRECTION('ref_axis',(-0.812985930735701,0.0183224676300055,0.581994985893997));
#88518=DIRECTION('center_axis',(0.0641407625183083,0.98649510951366,0.150709526869412));
#88519=DIRECTION('ref_axis',(-0.871144905238391,-0.0183223048337039,0.490684060493894));
#88520=DIRECTION('center_axis',(-0.0474700514394284,0.986495108004734,-0.156760952086502));
#88521=DIRECTION('ref_axis',(-0.919090489904261,0.0183224666752224,0.393620322877872));
#88522=DIRECTION('center_axis',(0.030243094789543,0.986495109526178,0.160974389573263));
#88523=DIRECTION('ref_axis',(-0.956260590131882,-0.0183223037027041,0.291941735535794));
#88524=DIRECTION('center_axis',(-0.0126612612175189,0.98649510803266,-0.16330062551017));
#88525=DIRECTION('ref_axis',(-0.982219398720206,0.0183224629032323,0.186840413537536));
#88526=DIRECTION('center_axis',(-0.00506870820519181,0.986495109499761,
0.163712269333076));
#88527=DIRECTION('ref_axis',(-0.996662592361594,-0.0183223045077197,0.0795485395503481));
#88528=DIRECTION('center_axis',(0.0227395578527785,0.986495108067057,-0.162204544536908));
#88529=DIRECTION('ref_axis',(-0.99942082101588,0.0183224615593546,-0.0286759467559414));
#88530=DIRECTION('center_axis',(-0.0401435017313524,0.986495109510236,0.158795145332385));
#88531=DIRECTION('ref_axis',(-0.99046175944326,-0.0183223030114974,-0.13656425701082));
#88532=DIRECTION('center_axis',(0.05707710669577,0.986495108026889,-0.153523958163722));
#88533=DIRECTION('ref_axis',(-0.969890436299754,0.0183224663519494,-0.242851454187645));
#88534=DIRECTION('center_axis',(-0.0733412334055878,0.986495109495549,0.146452935866481));
#88535=DIRECTION('ref_axis',(-0.937948035034169,-0.0183223051985068,-0.346291462077474));
#88536=DIRECTION('center_axis',(0.0887457784509185,0.986495108087939,-0.137664768643635));
#88537=DIRECTION('ref_axis',(-0.895009054991074,0.01832245519328,-0.445671492379392));
#88538=DIRECTION('center_axis',(-0.103109611601752,0.986495109457591,0.127262747933526));
#88539=DIRECTION('ref_axis',(-0.841576901967371,-0.0183223090775577,-0.539826463842844));
#88540=DIRECTION('center_axis',(0.116264815017321,0.986495107985349,-0.115368516979126));
#88541=DIRECTION('ref_axis',(-0.77827804080034,0.018322464811729,-0.627652434466088));
#88542=DIRECTION('center_axis',(-0.12805669118874,0.9864951095139,0.102121901406854));
#88543=DIRECTION('ref_axis',(-0.705854571165698,-0.0183223035697561,-0.708119776278269));
#88544=DIRECTION('center_axis',(0.138347433593088,0.986495107922349,-0.0876777603698864));
#88545=DIRECTION('ref_axis',(-0.625155611021741,0.0183224723337327,-0.780285043439648));
#88546=DIRECTION('center_axis',(-0.147015987202331,0.986495109509443,0.072205944498196));
#88547=DIRECTION('ref_axis',(-0.537127260541591,-0.0183223033714437,-0.843302199203969));
#88548=DIRECTION('center_axis',(0.153961071525636,0.986495108040822,-0.0558872996861048));
#88549=DIRECTION('ref_axis',(-0.442801601435135,0.0183224663569708,-0.896432389526995));
#88550=DIRECTION('center_axis',(-0.159100978613269,0.986495109517672,0.038913718686559));
#88551=DIRECTION('ref_axis',(-0.343284481816298,-0.0183223033521734,-0.939052744921172));
#88552=DIRECTION('center_axis',(0.162375666691975,0.986495107908977,-0.0214835969519158));
#88553=DIRECTION('ref_axis',(-0.239742676781274,0.0183224754522504,-0.970663554391042));
#88554=DIRECTION('center_axis',(-0.163746585579862,0.986495109490697,0.00380192870451849));
#88555=DIRECTION('ref_axis',(-0.133390098075001,-0.0183223046117274,-0.990894229920256));
#88556=DIRECTION('center_axis',(0.163197752322382,0.986495107979212,0.0139246389541917));
#88557=DIRECTION('ref_axis',(-0.0254736615879604,0.0183224693088499,-0.999507568597521));
#88558=DIRECTION('center_axis',(-0.16073558406174,0.986495109510974,-0.0314876313377507));
#88559=DIRECTION('ref_axis',(0.0827414566412087,-0.018322302109249,-0.996402601661752));
#88560=DIRECTION('center_axis',(0.156388895407881,0.986495108044351,0.0486817747998856));
#88561=DIRECTION('ref_axis',(0.189986480495769,0.0183224625414125,-0.981615721448699));
#88562=DIRECTION('center_axis',(-0.150208763039716,0.986495109468233,-0.0653048734884087));
#88563=DIRECTION('ref_axis',(0.295004112724699,-0.0183223089330748,-0.955320295226096));
#88564=DIRECTION('center_axis',(0.142267467124047,0.986495108042642,0.0811626121194061));
#88565=DIRECTION('ref_axis',(0.396563065841762,0.0183224630960468,-0.917824614050133));
#88566=DIRECTION('center_axis',(-0.132658350585122,0.986495109509682,-0.096068522074175));
#88567=DIRECTION('ref_axis',(0.493472703917656,-0.0183223047110463,-0.869568274282286));
#88568=DIRECTION('center_axis',(0.121493764696758,0.986495107991744,0.109848382091712));
#88569=DIRECTION('ref_axis',(0.584596805976639,0.0183224713431901,-0.81111704549084));
#88570=DIRECTION('center_axis',(-0.108904979399665,0.98649510950515,-0.122340117640862));
#88571=DIRECTION('ref_axis',(0.668867060361115,-0.0183223051419811,-0.743156207467962));
#88572=DIRECTION('center_axis',(0.0950391544766888,0.986495107995122,0.133397754921323));
#88573=DIRECTION('ref_axis',(0.745295445944788,0.0183224694080519,-0.66648254693484));
#88574=DIRECTION('center_axis',(-0.080059332910558,0.986495109481381,-0.142891225004316));
#88575=DIRECTION('ref_axis',(0.812985939220982,-0.0183223042755116,-0.581994979183681));
#88576=DIRECTION('center_axis',(0.0641406167314776,0.98649510794872,0.150709599158611));
#88577=DIRECTION('ref_axis',(0.871144897914193,0.0183224710739945,-0.490684067289547));
#88578=DIRECTION('center_axis',(-0.0474702014876177,0.986495109526955,-0.15676089706979));
#88579=DIRECTION('ref_axis',(0.919090496426534,-0.0183223033730333,-0.393620315250032));
#88580=DIRECTION('center_axis',(0.0302429388491882,0.986495108017902,0.160974428113639));
#88581=DIRECTION('ref_axis',(0.956260584933476,0.0183224675571459,-0.291941742279695));
#88582=DIRECTION('center_axis',(-0.0126614162704048,0.986495109510479,-0.163300604560837));
#88583=DIRECTION('ref_axis',(0.982219403911675,-0.0183223025459124,-0.186840401971333));
#88584=DIRECTION('center_axis',(-0.00506887179982308,0.986495107936615,
0.163712273687112));
#88585=DIRECTION('ref_axis',(0.996662588632331,0.018322471519566,-0.0795485478064573));
#88586=DIRECTION('center_axis',(0.0227394049424628,0.986495109493483,-0.162204557298197));
#88587=DIRECTION('ref_axis',(0.999420823519324,-0.0183223041105813,0.0286759601066141));
#88588=DIRECTION('center_axis',(-0.0401436445413463,0.986495108156152,0.158795117641948));
#88589=DIRECTION('ref_axis',(0.990461758653599,0.0183224525292182,0.136564242677704));
#88590=DIRECTION('center_axis',(0.0570769529460997,0.9864951095419,-0.153524005589694));
#88591=DIRECTION('ref_axis',(0.969890437076523,-0.0183223020859195,0.242851463478775));
#88592=DIRECTION('center_axis',(-0.0733413793153341,0.986495108018749,0.14645287274479));
#88593=DIRECTION('ref_axis',(0.937948035288988,0.0183224675093107,0.34629145279937));
#88594=DIRECTION('center_axis',(0.0887456490514789,0.986495109536923,-0.137664841677775));
#88595=DIRECTION('ref_axis',(0.895009051824839,-0.018322302725518,0.445671505006139));
#88596=DIRECTION('center_axis',(-0.103109737085043,0.986495108050338,0.12726265717407));
#88597=DIRECTION('ref_axis',(0.841576906157068,0.0183224677937832,0.539826451924174));
#88598=DIRECTION('center_axis',(0.116264699940127,0.986495109476491,-0.115368620199771));
#88599=DIRECTION('ref_axis',(0.778278035980726,-0.0183223065149454,0.627652445063314));
#88600=DIRECTION('center_axis',(-0.128056799605045,0.986495107974527,0.102121780327414));
#88601=DIRECTION('ref_axis',(0.705854575921104,0.0183224696374283,0.708119767241124));
#88602=DIRECTION('center_axis',(0.138347337245002,0.986495109509675,-0.0876778945385417));
#88603=DIRECTION('ref_axis',(0.625155606942879,-0.0183223039101845,0.78028505066245));
#88604=DIRECTION('center_axis',(-0.147016064077881,0.986495108038024,0.0722058080772992));
#88605=DIRECTION('ref_axis',(0.537127269546356,0.0183224638920168,0.843302189980912));
#88606=DIRECTION('center_axis',(0.153961009504263,0.98649510950004,-0.0558874447880148));
#88607=DIRECTION('ref_axis',(0.4428015927046,-0.0183223048421035,0.896432397140768));
#88608=DIRECTION('center_axis',(-0.159101026864052,0.986495107934884,0.0389135615351019));
#88609=DIRECTION('ref_axis',(0.34328448898429,0.0183224711543863,0.939052739026724));
#88610=DIRECTION('center_axis',(0.162375635431742,0.986495109483945,-0.0214837608997327));
#88611=DIRECTION('ref_axis',(0.239742670287193,-0.0183223053354739,0.970663559206155));
#88612=DIRECTION('center_axis',(-0.16374659742247,0.986495108103312,0.00380177863617757));
#88613=DIRECTION('ref_axis',(0.133390110991654,0.0183224591380823,0.99089422532416));
#88614=DIRECTION('center_axis',(0.163197756721024,0.986495109467979,0.0139244819288294));
#88615=DIRECTION('ref_axis',(0.0254736527193002,-0.0183223088757047,0.999507571764516));
#88616=DIRECTION('center_axis',(-0.155915195591883,0.987363722014138,0.0283431161648219));
#88617=DIRECTION('ref_axis',(0.137699079904333,-0.00668761038376333,0.99045153301959));
#88618=DIRECTION('',(-0.727555834386232,0.,-0.686048473397146));
#88619=DIRECTION('center_axis',(5.09401252609433E-15,-1.,3.67634634867259E-14));
#88620=DIRECTION('ref_axis',(-6.45625538871542E-32,-3.67634634867259E-14,
-1.));
#88621=DIRECTION('center_axis',(-0.152615513946062,-0.987363722125795,0.0426776889355044));
#88622=DIRECTION('ref_axis',(0.0672126608260175,0.032713973952949,0.997202213261128));
#88623=DIRECTION('center_axis',(0.149874467494489,-0.987363722004544,-0.0514832444837739));
#88624=DIRECTION('ref_axis',(0.141986603508105,-0.0300375739723024,0.989412729134859));
#88625=DIRECTION('',(-0.513606044697416,0.,0.858026124806393));
#88626=DIRECTION('center_axis',(-0.14617705138698,0.987363722010122,0.0611976315401775));
#88627=DIRECTION('ref_axis',(0.347397555335768,-0.00668761392715165,0.937694094236864));
#88628=DIRECTION('',(-0.858026123626375,0.,-0.513606046668745));
#88629=DIRECTION('center_axis',(-5.15119010035186E-15,-1.,-1.39235567883145E-14));
#88630=DIRECTION('ref_axis',(-6.20982939421556E-32,1.39235567883145E-14,
-1.));
#88631=DIRECTION('center_axis',(-0.139873004476777,-0.987363722032271,0.0744877374688009));
#88632=DIRECTION('ref_axis',(0.280010267064326,0.0327139789846414,0.959439443590661));
#88633=DIRECTION('center_axis',(0.135303109889243,-0.987363721994079,-0.082498175399821));
#88634=DIRECTION('ref_axis',(0.351361525093086,-0.0300375743814345,0.935757886854041));
#88635=DIRECTION('',(-0.317147963824608,0.,0.948376069416508));
#88636=DIRECTION('center_axis',(-0.129603829678582,0.987363721969541,0.0911906128452898));
#88637=DIRECTION('ref_axis',(0.540852105342674,-0.00668761734633794,0.841091122245756));
#88638=DIRECTION('',(-0.948376068001928,0.,-0.317147968054664));
#88639=DIRECTION('center_axis',(-4.01195563274949E-15,-1.,-6.24533907804427E-15));
#88640=DIRECTION('ref_axis',(1.34225804296661E-33,6.24533907804427E-15,
-1.));
#88641=DIRECTION('center_axis',(-0.120590190541021,-0.987363722095157,0.102814815253828));
#88642=DIRECTION('ref_axis',(0.479714901796952,0.0327139771544658,0.876814352467315));
#88643=DIRECTION('center_axis',(0.11440513091871,-0.987363722064315,-0.109655580664077));
#88644=DIRECTION('ref_axis',(0.544307172996746,-0.0300375714644054,0.838348045697496));
#88645=DIRECTION('',(-0.105860401342829,0.,0.994381001139671));
#88646=DIRECTION('center_axis',(-0.106970483025467,0.987363722064335,0.116919613891604));
#88647=DIRECTION('ref_axis',(0.709017011728858,-0.00668761002897997,0.705159664864051));
#88648=DIRECTION('',(-0.994381001052798,0.,-0.105860402158854));
#88649=DIRECTION('center_axis',(-2.10428865491674E-14,-1.,-2.0947498637656E-14));
#88650=DIRECTION('ref_axis',(1.,-2.10428865491674E-14,1.06656828981155E-31));
#88651=DIRECTION('center_axis',(-0.0956687124477457,-0.987363722032615,
0.126334389112749));
#88652=DIRECTION('ref_axis',(0.656988601142513,0.0327139780022003,0.753190396654177));
#88653=DIRECTION('center_axis',(0.0881576982976218,-0.987363722201013,-0.131685611637061));
#88654=DIRECTION('ref_axis',(0.711801621142929,-0.0300375659622816,0.701737982988921));
#88655=DIRECTION('',(0.110377077686696,0.,0.993889782984685));
#88656=DIRECTION('center_axis',(-0.0793353121724068,0.987363722060234,0.1371815898795));
#88657=DIRECTION('ref_axis',(0.844029071912828,-0.00668760940451682,0.536255724115299));
#88658=DIRECTION('',(-0.993889783075357,0.,0.110377076870243));
#88659=DIRECTION('center_axis',(-2.50540085574457E-14,-1.,-1.59341591747121E-14));
#88660=DIRECTION('ref_axis',(1.,-2.50540085574457E-14,2.03091541231879E-31));
#88661=DIRECTION('center_axis',(-0.0662738725216956,-0.987363722042481,
0.143946706163761));
#88662=DIRECTION('ref_axis',(0.803542242785219,0.0327139775453649,0.594348096432437));
#88663=DIRECTION('center_axis',(0.0577880969639443,-0.987363721938116,-0.147558179881013));
#88664=DIRECTION('ref_axis',(0.84601301874443,-0.0300375766578798,0.532315429142777));
#88665=DIRECTION('',(0.321453447978035,0.,0.946925382901437));
#88666=DIRECTION('center_axis',(-0.0479905089208821,0.987363722033518,0.151029108007807));
#88667=DIRECTION('ref_axis',(0.939575270352825,-0.00668761048465775,0.342277062052691));
#88668=DIRECTION('',(-0.946925383165727,0.,0.321453447199499));
#88669=DIRECTION('center_axis',(-1.39468164794721E-14,-1.,-5.08787806647015E-15));
#88670=DIRECTION('ref_axis',(1.,-1.39468164794721E-14,-5.70074136491531E-32));
#88671=DIRECTION('center_axis',(-0.0337801382797952,-0.987363722000072,
0.154828236236041));
#88672=DIRECTION('ref_axis',(0.912523143460641,0.0327139788577966,0.407714738801532));
#88673=DIRECTION('center_axis',(0.0247164010991849,-0.987363722070208,-0.156531082716402));
#88674=DIRECTION('ref_axis',(0.940665786847186,-0.0300375716952866,0.338002399017841));
#88675=DIRECTION('',(0.517499010316405,0.,0.855683805106501));
#88676=DIRECTION('center_axis',(-0.0144017231991955,0.987363722024748,0.157814672316391));
#88677=DIRECTION('ref_axis',(0.991187973412547,-0.0066876108997449,0.132293904707591));
#88678=DIRECTION('',(-0.855683805531977,0.,0.517499009612883));
#88679=DIRECTION('center_axis',(-2.20717365751389E-14,-1.,-2.95615954106558E-15));
#88680=DIRECTION('ref_axis',(1.,-2.20717365751389E-14,-3.49902049063999E-32));
#88681=DIRECTION('center_axis',(0.00029311340816282,-0.987363722109961,
0.158470168630232));
#88682=DIRECTION('ref_axis',(0.978835476575937,0.0327139753810231,0.202017092373709));
#88683=DIRECTION('center_axis',(-0.0095110066128146,-0.987363722136431,
-0.158184768426366));
#88684=DIRECTION('ref_axis',(0.991334067966758,-0.0300375680597071,0.127884753561701));
#88685=DIRECTION('',(0.689346896451424,0.,0.724431402102911));
#88686=DIRECTION('center_axis',(0.0198604748347696,0.98736372197993,0.157220997507575));
#88687=DIRECTION('ref_axis',(0.996453828388622,-0.00668761527781448,-0.0838751673116389));
#88688=DIRECTION('',(-0.724431404105314,0.,0.689346894347108));
#88689=DIRECTION('center_axis',(7.3970661933122E-15,-1.,-6.19241585272321E-16));
#88690=DIRECTION('ref_axis',(1.,7.3970661933122E-15,-2.73744258678365E-33));
#88691=DIRECTION('center_axis',(0.0343526630103307,-0.987363722117046,0.154702213272049));
#88692=DIRECTION('ref_axis',(0.999378550340755,0.0327139758686177,-0.0131266485318631));
#88693=DIRECTION('center_axis',(-0.0432936985350912,-0.987363722000109,
-0.152441910724197));
#88694=DIRECTION('ref_axis',(0.995648669933615,-0.030037572720232,-0.088212642430092));
#88695=DIRECTION('',(0.828961684948636,0.,0.559305395009845));
#88696=DIRECTION('center_axis',(0.0531940151561749,0.987363721983716,0.149275842861553));
#88697=DIRECTION('ref_axis',(0.955126609739221,-0.00668761530697499,-0.296122331426671));
#88698=DIRECTION('',(-0.559305393715893,0.,0.828961685821673));
#88699=DIRECTION('center_axis',(-2.12730247814828E-14,-1.,6.58474391108148E-15));
#88700=DIRECTION('ref_axis',(1.,-2.12730247814828E-14,-4.11537089026276E-32));
#88701=DIRECTION('center_axis',(0.066805920029825,-0.987363722085958,0.143700554478858));
#88702=DIRECTION('ref_axis',(0.973191793942822,0.0327139762673729,-0.22765660095664));
#88703=DIRECTION('center_axis',(-0.0750520182188506,-0.987363722081671,
-0.139571038823626));
#88704=DIRECTION('ref_axis',(0.95340784703351,-0.0300375703472505,-0.300185312069997));
#88705=DIRECTION('',(0.929815148606726,0.,0.368026886818684));
#88706=DIRECTION('center_axis',(0.0840402591504759,0.987363722035372,0.134350717342248));
#88707=DIRECTION('ref_axis',(0.869138731961614,-0.00668761158347473,-0.494523144509402));
#88708=DIRECTION('',(-0.368026888566917,0.,0.929815147914764));
#88709=DIRECTION('center_axis',(6.45338266227362E-15,-1.,-3.66795591991993E-15));
#88710=DIRECTION('ref_axis',(1.,6.45338266227362E-15,2.19847859555268E-32));
#88711=DIRECTION('center_axis',(0.0961354053430143,-0.987363722113789,0.125979617768667));
#88712=DIRECTION('ref_axis',(0.901499670081164,0.0327139749884623,-0.431541586274148));
#88713=DIRECTION('center_axis',(-0.103300989414795,-0.987363722147405,-0.120173981265271));
#88714=DIRECTION('ref_axis',(0.86658673311804,-0.0300375681323686,-0.498121650286851));
#88715=DIRECTION('',(0.987191489212963,0.,0.15953984964733));
#88716=DIRECTION('center_axis',(0.110956879962712,0.98736372196159,0.113143498898947));
#88717=DIRECTION('ref_axis',(0.742510893754301,-0.00668761482372817,-0.669800603511342));
#88718=DIRECTION('',(-0.159539850458518,0.,0.987191489081867));
#88719=DIRECTION('center_axis',(1.65420121889355E-14,-1.,-1.49084629836801E-14));
#88720=DIRECTION('ref_axis',(1.,1.65420121889355E-14,6.43307823203382E-32));
#88721=DIRECTION('center_axis',(0.120969707670699,-0.987363722086591,0.102368013233525));
#88722=DIRECTION('ref_axis',(0.787654424115901,0.0327139760771574,-0.615248164515646));
#88723=DIRECTION('center_axis',(-0.126719727503591,-0.987363722008549,-0.0951577170955746));
#88724=DIRECTION('ref_axis',(0.739244985382749,-0.0300375738261793,-0.672766375308023));
#88725=DIRECTION('',(0.998407852567291,0.,-0.0564070911496949));
#88726=DIRECTION('center_axis',(0.132685278204196,0.98736372199092,0.0866458160796747));
#88727=DIRECTION('ref_axis',(0.58116407064798,-0.00668761625283787,-0.813758931611029));
#88728=DIRECTION('',(0.0564070903287917,0.,0.99840785261367));
#88729=DIRECTION('center_axis',(-3.02175773341056E-14,-1.,4.22705617652681E-14));
#88730=DIRECTION('ref_axis',(-3.42385489395757E-32,-4.22705617652681E-14,
-1.));
#88731=DIRECTION('center_axis',(0.140147600521612,-0.987363722064494,0.0739697939633669));
#88732=DIRECTION('ref_axis',(0.636979333125905,0.0327139770656922,-0.770186422157014));
#88733=DIRECTION('center_axis',(-0.144213188971448,-0.987363721901816,-0.0656919842817939));
#88734=DIRECTION('ref_axis',(0.577336963336558,-0.0300375769362138,-0.815953292007038));
#88735=DIRECTION('',(0.962939774722175,0.,-0.269716499788217));
#88736=DIRECTION('center_axis',(0.148209458094694,0.987363721996652,0.0560966756251662));
#88737=DIRECTION('ref_axis',(0.392642662313079,-0.00668761280541487,-0.919666795946587));
#88738=DIRECTION('',(0.269716499743162,0.,0.962939774734794));
#88739=DIRECTION('center_axis',(2.91774084025479E-15,-1.,-6.82545505654051E-15));
#88740=DIRECTION('ref_axis',(-6.44641099708178E-33,6.82545505654051E-15,
-1.));
#88741=DIRECTION('center_axis',(0.152772347138366,-0.987363722035567,0.042112828899362));
#88742=DIRECTION('ref_axis',(0.456519795472252,0.0327139780841959,-0.889111619528099));
#88743=DIRECTION('center_axis',(-0.154963396046347,-0.987363722152358,-0.0331545783146796));
#88744=DIRECTION('ref_axis',(0.388433310595543,-0.0300375678177878,-0.92098713766229));
#88745=DIRECTION('',(0.882445701968546,0.,-0.470414267510287));
#88746=DIRECTION('center_axis',(0.156803530198347,0.987363722024449,0.022924514114007));
#88747=DIRECTION('ref_axis',(0.18576171983432,-0.00668761285105647,-0.982572063147813));
#88748=DIRECTION('',(0.470414265591377,0.,0.882445702991479));
#88749=DIRECTION('center_axis',(2.76450920575637E-15,-1.,-1.45862154872855E-14));
#88750=DIRECTION('ref_axis',(3.9736416322651E-32,1.45862154872855E-14,-1.));
#88751=DIRECTION('center_axis',(0.158253627833745,-0.987363722044687,0.00828671632925747));
#88752=DIRECTION('ref_axis',(0.254713900192221,0.0327139774057854,-0.966462945348222));
#88753=DIRECTION('center_axis',(-0.158467693352313,-0.987363721969011,0.000933114730172718));
#88754=DIRECTION('ref_axis',(0.181366942943162,-0.0300375755843955,-0.982956650143059));
#88755=DIRECTION('',(0.760689450324145,0.,-0.649115983600427));
#88756=DIRECTION('',(0.649115982975009,0.,0.760689450857831));
#88757=DIRECTION('',(0.603364203507011,0.,-0.797465759720347));
#88758=DIRECTION('center_axis',(0.15193678307463,0.987363721986491,-0.0450343696959965));
#88759=DIRECTION('ref_axis',(-0.243978531110299,-0.00668761449916178,-0.969757573917096));
#88760=DIRECTION('',(0.797465757841021,0.,0.603364205990914));
#88761=DIRECTION('center_axis',(3.61559231045529E-15,-1.,1.43988779150332E-14));
#88762=DIRECTION('ref_axis',(2.43352655744764E-33,-1.43988779150332E-14,
-1.));
#88763=DIRECTION('center_axis',(0.147106605238035,-0.987363722139964,-0.0589281502955677));
#88764=DIRECTION('ref_axis',(-0.174635182534135,0.0327139741043342,-0.984089604111115));
#88765=DIRECTION('center_axis',(-0.14342958100638,-0.98736372219215,0.0673857209740856));
#88766=DIRECTION('ref_axis',(-0.248128604798918,-0.0300375668343596,-0.968261297408511));
#88767=DIRECTION('',(0.417826320448815,0.,-0.908526920867073));
#88768=DIRECTION('center_axis',(0.138703528025338,0.9873637219984,-0.0766434067274603));
#88769=DIRECTION('ref_axis',(-0.446743660603705,-0.0066876128263548,-0.894637008817032));
#88770=DIRECTION('',(0.908526921025422,0.,0.417826320104499));
#88771=DIRECTION('center_axis',(-3.31319745013849E-15,-1.,-6.64249734523797E-15));
#88772=DIRECTION('ref_axis',(-2.41067561919743E-32,6.64249734523797E-15,
-1.));
#88773=DIRECTION('center_axis',(0.130999522255125,-0.987363722009175,-0.0891740188009809));
#88774=DIRECTION('ref_axis',(-0.382102486511712,0.032713978423544,-0.923540732949701));
#88775=DIRECTION('center_axis',(-0.125590338476149,-0.987363722138999,0.0966434016644088));
#88776=DIRECTION('ref_axis',(-0.450475053156877,-0.0300375682025106,-0.8922835709458));
#88777=DIRECTION('',(0.212751341222145,0.,-0.977106374356538));
#88778=DIRECTION('center_axis',(0.118984649782232,0.987363722013483,-0.104668684752799));
#88779=DIRECTION('ref_axis',(-0.628619553791156,-0.00668761262270496,-0.777684211250824));
#88780=DIRECTION('',(0.97710637405149,0.,0.212751342623141));
#88781=DIRECTION('center_axis',(0.,-1.,0.));
#88782=DIRECTION('ref_axis',(0.,0.,-1.));
#88783=DIRECTION('center_axis',(0.108767048291564,-0.987363722066022,-0.115250204138089));
#88784=DIRECTION('ref_axis',(-0.571703099871005,0.0327139779658703,-0.819808124650843));
#88785=DIRECTION('center_axis',(-0.101878629407447,-0.987363722040434,0.121382145592017));
#88786=DIRECTION('ref_axis',(-0.631757788857494,-0.0300375715922423,-0.774583656237808));
#88787=DIRECTION('',(-0.00227165580984505,0.,-0.999997419786612));
#88788=DIRECTION('center_axis',(0.0937021788006043,0.9873637219845,-0.127799773853223));
#88789=DIRECTION('ref_axis',(-0.781101895149244,-0.00668761622474827,-0.624367764369277));
#88790=DIRECTION('',(0.99999741978848,0.,-0.00227165498764559));
#88791=DIRECTION('',(-0.217188431596517,0.,-0.976129696905409));
#88792=DIRECTION('center_axis',(4.0572621615691E-14,-1.,3.24617426702296E-14));
#88793=DIRECTION('ref_axis',(1.,4.0572621615691E-14,-2.92296430474148E-31));
#88794=DIRECTION('center_axis',(0.0814487487035971,-0.987363722049272,-0.135937418379291));
#88795=DIRECTION('ref_axis',(-0.734571511907989,0.032713977419385,-0.677742199936388));
#88796=DIRECTION('center_axis',(-0.0734031935085418,-0.987363722173652,
0.140445189729441));
#88797=DIRECTION('ref_axis',(-0.783500232034526,-0.0300375676236387,-0.620665071462136));
#88798=DIRECTION('',(0.97612969721957,0.,-0.217188430184553));
#88799=DIRECTION('center_axis',(0.0640383051982778,0.987363722029317,-0.144955082310855));
#88800=DIRECTION('ref_axis',(-0.897060779917043,-0.00668761072181317,-0.441856575143406));
#88801=DIRECTION('center_axis',(1.33149632604712E-14,-1.,6.56596881425884E-15));
#88802=DIRECTION('ref_axis',(1.,1.33149632604712E-14,8.86106816052588E-32));
#88803=DIRECTION('center_axis',(0.0503219999089623,-0.987363722182468,-0.150268348108123));
#88804=DIRECTION('ref_axis',(-0.863092177279706,0.0327139724496799,-0.503985802900377));
#88805=DIRECTION('center_axis',(-0.0414955038933948,-0.987363722188286,
0.152941175826287));
#88806=DIRECTION('ref_axis',(-0.898607075736631,-0.0300375670188769,-0.437724877067374));
#88807=DIRECTION('',(-0.42194971744984,0.,-0.906619234267617));
#88808=DIRECTION('center_axis',(0.0313800657302326,0.987363722003927,-0.155332456187748));
#88809=DIRECTION('ref_axis',(-0.971074099998923,-0.00668761233512322,-0.238684662583368));
#88810=DIRECTION('',(0.906619235714275,0.,-0.421949714341488));
#88811=DIRECTION('center_axis',(7.20757801078152E-15,-1.,1.77506829913838E-15));
#88812=DIRECTION('ref_axis',(1.,7.20757801078152E-15,-1.50447430979086E-32));
#88813=DIRECTION('center_axis',(0.0168422433773957,-0.987363722095952,-0.157572900991399));
#88814=DIRECTION('ref_axis',(-0.951255611113478,0.0327139760516595,-0.306663591083151));
#88815=DIRECTION('center_axis',(-0.00764752809376302,-0.987363722126041,
0.158285803354138));
#88816=DIRECTION('ref_axis',(-0.97169605093596,-0.0300375693087569,-0.234317154782747));
#88817=DIRECTION('',(-0.606981102892634,0.,-0.794716264292635));
#88818=DIRECTION('center_axis',(-0.00274546710291745,0.98736372205532,-0.158446655942785));
#88819=DIRECTION('ref_axis',(-0.999681074168654,-0.00668761021136266,-0.0243521214407966));
#88820=DIRECTION('',(0.794716264791645,0.,-0.606981102239283));
#88821=DIRECTION('center_axis',(5.9365248500426E-14,-1.,1.4732157731511E-15));
#88822=DIRECTION('ref_axis',(-0.999692221970019,-5.9383525444618E-14,-0.0248084931554796));
#88823=DIRECTION('center_axis',(-0.0174250350984094,-0.987363722096869,
-0.157509518565821));
#88824=DIRECTION('ref_axis',(-0.99493939068009,0.0327139763908477,-0.0950021295647155));
#88825=DIRECTION('center_axis',(0.0265580391453566,-0.98736372202936,0.15622916173712));
#88826=DIRECTION('ref_axis',(-0.999349599106874,-0.0300375724690615,-0.0199530199492971));
#88827=DIRECTION('',(-0.763630725504658,0.,-0.645653246770455));
#88828=DIRECTION('center_axis',(-0.0367426341140373,0.987363721963562,-0.154152065794214));
#88829=DIRECTION('ref_axis',(-0.981544072352426,-0.00668761746811693,0.191119098476359));
#88830=DIRECTION('',(0.645653245721824,0.,-0.76363072639128));
#88831=DIRECTION('center_axis',(2.18602574241031E-14,-1.,-4.24612529797942E-15));
#88832=DIRECTION('ref_axis',(1.,2.18602574241031E-14,1.16412908801297E-32));
#88833=DIRECTION('center_axis',(-0.0508775382972576,-0.987363722076295,
-0.150081166121724));
#88834=DIRECTION('ref_axis',(-0.992100910024825,0.0327139764061875,0.121101527965626));
#88835=DIRECTION('center_axis',(0.0595217788630251,-0.987363722020241,0.14686741735088));
#88836=DIRECTION('ref_axis',(-0.980274670496925,-0.0300375728765124,0.1953440928153));
#88837=DIRECTION('',(-0.884573827309064,0.,-0.466400197298193));
#88838=DIRECTION('center_axis',(-0.0690217385068017,0.987363722098133,-0.142649500167436));
#88839=DIRECTION('ref_axis',(-0.917511161069893,-0.00668760596951243,0.397653800734475));
#88840=DIRECTION('',(0.466400199211432,0.,-0.884573826300291));
#88841=DIRECTION('center_axis',(-4.08727706304602E-14,-1.,1.7692324809619E-14));
#88842=DIRECTION('ref_axis',(1.,-4.08727706304603E-14,-1.5709522500068E-31));
#88843=DIRECTION('center_axis',(-0.0819510664810077,-0.987363722021505,
-0.135635183999088));
#88844=DIRECTION('ref_axis',(-0.942872892860092,0.0327139788905535,0.331542611883886));
#88845=DIRECTION('center_axis',(0.0897023381954629,-0.987363722254225,0.130638319411068));
#88846=DIRECTION('ref_axis',(-0.915363188590782,-0.0300375642560458,0.401507132821424));
#88847=DIRECTION('',(-0.964155239073704,0.,-0.265338792804085));
#88848=DIRECTION('center_axis',(-0.0980734823229331,0.987363721984803,-0.124476795320935));
#88849=DIRECTION('ref_axis',(-0.810576446806066,-0.00668761541326269,0.585594654759875));
#88850=DIRECTION('',(0.265338796269035,0.,-0.964155238120138));
#88851=DIRECTION('center_axis',(-3.61138611426735E-14,-1.,2.60651256016803E-14));
#88852=DIRECTION('ref_axis',(1.,-3.61138611426735E-14,7.03962851519167E-32));
#88853=DIRECTION('center_axis',(-0.10919264797883,-0.987363722125025,-0.114847054201611));
#88854=DIRECTION('ref_axis',(-0.849557187882663,0.0327139749465049,0.526481130108288));
#88855=DIRECTION('center_axis',(0.115688529444972,-0.98736372208904,0.108300713097081));
#88856=DIRECTION('ref_axis',(-0.807650340411127,-0.0300375706146091,0.588896147028798));
#88857=DIRECTION('',(-0.998653822462692,0.,-0.0518704432278601));
#88858=DIRECTION('center_axis',(-0.122539409041195,0.987363721996483,-0.100483698762969));
#88859=DIRECTION('ref_axis',(-0.665740079912513,-0.00668761365265042,0.746153752132705));
#88860=DIRECTION('',(0.0518704469159844,0.,-0.998653822271129));
#88861=DIRECTION('center_axis',(-9.88876920374125E-15,-1.,1.10730500259122E-14));
#88862=DIRECTION('ref_axis',(2.65179613550382E-33,-1.10730500259122E-14,
-1.));
#88863=DIRECTION('center_axis',(-0.131328506916138,-0.987363722072865,-0.0886888020304502));
#88864=DIRECTION('ref_axis',(-0.716517133417842,0.0327139757254959,0.69680197567954));
#88865=DIRECTION('center_axis',(0.13626524791609,-0.987363722104922,0.0808990882611246));
#88866=DIRECTION('ref_axis',(-0.662172659358769,-0.0300375706213195,0.748749032419344));
#88867=DIRECTION('',(-0.986456463077436,0.,0.164023310699287));
#88868=DIRECTION('center_axis',(-0.141275529117461,0.987363722015998,-0.0717920978889472));
#88869=DIRECTION('ref_axis',(-0.489774445357342,-0.00668761016490139,0.871823530621416));
#88870=DIRECTION('',(-0.164023306625657,0.,-0.98645646375478));
#88871=DIRECTION('center_axis',(3.63859842182505E-15,-1.,-6.46998067506677E-15));
#88872=DIRECTION('ref_axis',(2.29970405697103E-32,6.46998067506677E-15,
-1.));
#88873=DIRECTION('center_axis',(-0.147323591451942,-0.987363722036411,-0.058383557686263));
#88874=DIRECTION('ref_axis',(-0.549973531153307,0.0327139780733239,0.834541137793327));
#88875=DIRECTION('center_axis',(0.150470353914617,-0.987363722120249,0.0497147144581797));
#88876=DIRECTION('ref_axis',(-0.485732522241045,-0.0300375683489521,0.873591243846362));
#88877=DIRECTION('',(-0.928133496571451,0.,0.372247515159002));
#88878=DIRECTION('center_axis',(-0.153405764587397,0.987363722018912,-0.039743575988041));
#88879=DIRECTION('ref_axis',(-0.290907503589963,-0.00668761014234149,0.95672780884933));
#88880=DIRECTION('',(-0.372247514395924,0.,-0.9281334968775));
#88881=DIRECTION('center_axis',(1.08133770958267E-14,-1.,-3.55045361378079E-14));
#88882=DIRECTION('ref_axis',(-5.72023480965401E-33,3.55045361378079E-14,
-1.));
#88883=DIRECTION('center_axis',(-0.156429986999111,-0.987363722017236,-0.0253483650701108));
#88884=DIRECTION('ref_axis',(-0.357713779802522,0.0327139782837103,0.933258081863878));
#88885=DIRECTION('center_axis',(0.157639635047916,-0.987363722095111,0.0162057320861793));
#88886=DIRECTION('ref_axis',(-0.286580070934241,-0.0300375700506857,0.957585300288583));
#88887=DIRECTION('',(-0.82641203914066,0.,0.563065841232956));
#88888=DIRECTION('center_axis',(-0.158362916897451,0.987363722042217,-0.00583668970149514));
#88889=DIRECTION('ref_axis',(-0.0784380504043121,-0.00668760906902361,0.996896558391948));
#88890=DIRECTION('',(-0.563065840553765,0.,-0.826412039603419));
#88891=DIRECTION('center_axis',(1.17125623364526E-15,-1.,-1.47996064969821E-14));
#88892=DIRECTION('ref_axis',(3.94381262549887E-33,1.47996064969821E-14,
-1.));
#88893=DIRECTION('center_axis',(-0.15822188942635,-0.98736372216291,0.00887208334943327));
#88894=DIRECTION('ref_axis',(-0.14872773252229,0.0327139731913081,0.988336914992462));
#88895=DIRECTION('center_axis',(0.157437861539007,-0.987363721967107,-0.0180610159538643));
#88896=DIRECTION('ref_axis',(-0.0740274533496773,-0.0300375752097382,0.996803732048632));
#88897=DIRECTION('',(-0.686048471277773,0.,0.727555836384694));
#88898=DIRECTION('',(0.761237618626307,0.,-0.648473043378173));
#88899=DIRECTION('center_axis',(0.154431769357297,-0.987363722514828,0.0355486719138206));
#88900=DIRECTION('ref_axis',(-0.188052377251641,0.00594770337842175,0.982140992034509));
#88901=DIRECTION('center_axis',(9.79631271996063E-14,-1.,-5.15165042619057E-13));
#88902=DIRECTION('ref_axis',(-2.51994924462431E-30,5.15165042619057E-13,
-1.));
#88903=DIRECTION('center_axis',(-0.179949042279907,0.983673454101297,0.00220859207834743));
#88904=DIRECTION('ref_axis',(-0.00321947738172968,-0.00283418610278911,
0.999990801134952));
#88905=DIRECTION('center_axis',(0.,1.,-4.27898457407613E-15));
#88906=DIRECTION('ref_axis',(0.,-4.27898457407613E-15,-1.));
#88907=DIRECTION('center_axis',(0.15853152106945,0.98256963623183,0.0970807230229386));
#88908=DIRECTION('ref_axis',(-0.347991529212697,-0.0364113180679517,0.936790324198944));
#88909=DIRECTION('center_axis',(-0.1527723673653,-0.987363723844037,-0.0421127131213217));
#88910=DIRECTION('ref_axis',(-0.260766127816424,-0.000828290449268767,0.965401647252873));
#88911=DIRECTION('',(0.469668518497478,0.,0.882842841468619));
#88912=DIRECTION('center_axis',(5.55366423743563E-15,-1.,-2.91677489184056E-14));
#88913=DIRECTION('ref_axis',(-1.35478984408908E-31,2.91677489184056E-14,
-1.));
#88914=DIRECTION('center_axis',(-0.14732530161365,0.987363878712072,-0.0583765922189797));
#88915=DIRECTION('ref_axis',(-0.215660138228666,0.0255338646749638,0.976134584232089));
#88916=DIRECTION('center_axis',(0.157369919791754,0.987363724405155,0.0186436067733055));
#88917=DIRECTION('ref_axis',(-0.160618010575024,0.00696334191558068,0.986992080286508));
#88918=DIRECTION('',(0.882842841300013,0.,-0.469668518814407));
#88919=DIRECTION('center_axis',(0.143179326239305,-0.987363722493451,0.0679158305664762));
#88920=DIRECTION('ref_axis',(-0.394787099410106,0.0059477047491631,0.918753378740765));
#88921=DIRECTION('center_axis',(-2.06418061594693E-13,-1.,4.8206159791424E-13));
#88922=DIRECTION('ref_axis',(-8.43588309106855E-30,-4.8206159791424E-13,
-1.));
#88923=DIRECTION('center_axis',(-0.176216739608827,0.983673453678242,-0.0365266643748751));
#88924=DIRECTION('ref_axis',(-0.218112650942901,-0.00283429096832737,0.975919483509458));
#88925=DIRECTION('center_axis',(0.,1.,-4.27898457407613E-15));
#88926=DIRECTION('ref_axis',(0.,-4.27898457407613E-15,-1.));
#88927=DIRECTION('center_axis',(0.133955657112767,0.982569636300036,0.12889061932003));
#88928=DIRECTION('ref_axis',(-0.541237908795975,-0.0364113167100376,0.840080794982007));
#88929=DIRECTION('center_axis',(-0.140147645931868,-0.98736372384866,-0.0739696841108766));
#88930=DIRECTION('ref_axis',(-0.462202379579607,-0.000828289852944301,0.886774082981042));
#88931=DIRECTION('',(0.268902817760427,0.,0.963167313918253));
#88932=DIRECTION('center_axis',(3.50820794247826E-14,-1.,-8.18758485032203E-14));
#88933=DIRECTION('ref_axis',(1.0873911167328E-31,8.18758485032203E-14,-1.));
#88934=DIRECTION('center_axis',(-0.131331675171813,0.987363878709653,-0.0886823664320867));
#88935=DIRECTION('ref_axis',(-0.42045820551751,0.0255338665054303,0.906952545106015));
#88936=DIRECTION('center_axis',(0.149682873117739,0.987363724365384,0.052037614304822));
#88937=DIRECTION('ref_axis',(-0.369036976815383,0.00696333868578459,0.929388627893256));
#88938=DIRECTION('',(0.9631673145042,0.,-0.268902815661658));
#88939=DIRECTION('center_axis',(0.125231976535853,-0.987363722499094,0.0971073197326294));
#88940=DIRECTION('ref_axis',(-0.583062014846573,0.0059477057068179,0.812405878634491));
#88941=DIRECTION('center_axis',(1.52610558579865E-13,-1.,-2.13208742943039E-13));
#88942=DIRECTION('ref_axis',(4.34777305341731E-30,2.13208742943039E-13,
-1.));
#88943=DIRECTION('center_axis',(-0.164244673331451,0.983673454241399,-0.0735542160792886));
#88944=DIRECTION('ref_axis',(-0.422807164527357,-0.00283414450632821,0.906215244436582));
#88945=DIRECTION('center_axis',(0.,1.,-4.27898457407613E-15));
#88946=DIRECTION('ref_axis',(0.,-4.27898457407613E-15,-1.));
#88947=DIRECTION('center_axis',(0.10311615443596,0.982569635229474,0.154673755431737));
#88948=DIRECTION('ref_axis',(-0.709176608070518,-0.036411345534319,0.70409001731453));
#88949=DIRECTION('center_axis',(-0.120969775086762,-0.987363723798551,-0.102367917054697));
#88950=DIRECTION('ref_axis',(-0.642026559594874,-0.000828292162798994,0.76668194885941));
#88951=DIRECTION('',(0.0555635156269576,0.,0.998455154591919));
#88952=DIRECTION('center_axis',(8.64379451955931E-14,-1.,-1.2070004440492E-13));
#88953=DIRECTION('ref_axis',(3.17309574127229E-30,1.2070004440492E-13,-1.));
#88954=DIRECTION('center_axis',(-0.109197112976554,0.987363878298483,-0.114841466156457));
#88955=DIRECTION('ref_axis',(-0.605596116332949,0.0255338871524541,0.795362410784753));
#88956=DIRECTION('center_axis',(0.134996817658912,0.987363724450577,0.08299840276205));
#88957=DIRECTION('ref_axis',(-0.560200179129411,0.00696333125741769,0.82832799742685));
#88958=DIRECTION('',(0.998455154553505,1.49610497004341E-14,-0.055563516317241));
#88959=DIRECTION('center_axis',(0.10142892175727,-0.987363722503769,0.121758175555722));
#88960=DIRECTION('ref_axis',(-0.74407359701472,0.00594770268880726,0.668071184125092));
#88961=DIRECTION('center_axis',(-7.79504734952084E-13,-1.,7.01669120585349E-13));
#88962=DIRECTION('ref_axis',(1.,-7.79504734952084E-13,-1.59279744026798E-30));
#88963=DIRECTION('center_axis',(-0.14459285205623,0.983673453495816,-0.107142167337888));
#88964=DIRECTION('ref_axis',(-0.607731631042885,-0.00283432086000192,0.794137413332994));
#88965=DIRECTION('center_axis',(0.,1.,-4.27898457407613E-15));
#88966=DIRECTION('ref_axis',(0.,-4.27898457407613E-15,-1.));
#88967=DIRECTION('center_axis',(0.0674551032578653,0.982569636602003,0.173224473652768));
#88968=DIRECTION('ref_axis',(-0.843954992283683,-0.036411307495574,0.535176781714146));
#88969=DIRECTION('center_axis',(-0.0961354912201982,-0.987363723790838,
-0.125979539091637));
#88970=DIRECTION('ref_axis',(-0.791830292288917,-0.000828293965008936,0.610740617727981));
#88971=DIRECTION('',(-0.160373869647189,0.,0.987056341823701));
#88972=DIRECTION('center_axis',(1.10364015858298E-13,-1.,-9.92965414012673E-14));
#88973=DIRECTION('ref_axis',(1.,1.10364015858298E-13,3.53523353257534E-30));
#88974=DIRECTION('center_axis',(-0.0819566430429945,0.98736387872903,-0.135630673677782));
#88975=DIRECTION('ref_axis',(-0.762417021447238,0.025533864141092,0.646582018919137));
#88976=DIRECTION('center_axis',(0.113998471850588,0.987363724368407,0.110078264053714));
#88977=DIRECTION('ref_axis',(-0.725169043306024,0.00696334205636933,0.688535671187798));
#88978=DIRECTION('',(0.987056341019167,0.,0.160373874598871));
#88979=DIRECTION('center_axis',(0.0728831631304263,-0.987363722530532,0.140715755915086));
#88980=DIRECTION('ref_axis',(-0.870293126478398,0.00594770050821674,0.492498222192852));
#88981=DIRECTION('center_axis',(1.8242369488553E-12,-1.,-1.03538802890571E-12));
#88982=DIRECTION('ref_axis',(1.,1.8242369488553E-12,4.32938170593567E-29));
#88983=DIRECTION('center_axis',(-0.118179854965378,0.983673454033135,-0.135720513228048));
#88984=DIRECTION('ref_axis',(-0.764239288201414,-0.00283419611140209,0.644926567681778));
#88985=DIRECTION('center_axis',(0.,1.,-4.27898457407613E-15));
#88986=DIRECTION('ref_axis',(0.,-4.27898457407613E-15,-1.));
#88987=DIRECTION('center_axis',(0.0286398862805303,0.982569636100756,0.183675439639233));
#88988=DIRECTION('ref_axis',(-0.939270981848649,-0.0364113211302585,0.341239268476863));
#88989=DIRECTION('center_axis',(-0.0668060207260926,-0.987363723825072,
-0.143700495716029));
#88990=DIRECTION('ref_axis',(-0.904608919750942,-0.000828292839112309,0.426241734509898));
#88991=DIRECTION('',(-0.368812355268781,0.,0.929503871213614));
#88992=DIRECTION('center_axis',(0.,-1.,0.));
#88993=DIRECTION('ref_axis',(0.,0.,-1.));
#88994=DIRECTION('center_axis',(-0.0508839561738066,0.987363878729922,-0.150077959685978));
#88995=DIRECTION('ref_axis',(-0.883588156432343,0.0255338646246355,0.467568167832054));
#88996=DIRECTION('center_axis',(0.0876696764382493,0.987363724373119,0.132010998122337));
#88997=DIRECTION('ref_axis',(-0.856229809932433,0.00696333997322604,0.516548182147114));
#88998=DIRECTION('',(0.929503870800998,-1.49610497208486E-14,0.36881235630868));
#88999=DIRECTION('center_axis',(0.040929462489895,-0.987363722493695,0.153093626920526));
#89000=DIRECTION('ref_axis',(-0.955818717023452,0.0059477052689164,0.293896588938483));
#89001=DIRECTION('center_axis',(1.25260320433439E-12,-1.,-3.86890133542238E-13));
#89002=DIRECTION('ref_axis',(1.,1.25260320433439E-12,9.01406401442751E-30));
#89003=DIRECTION('center_axis',(-0.0862408680956417,0.983673454504075,-0.157952675109125));
#89004=DIRECTION('ref_axis',(-0.885011957399521,-0.00283407536007535,0.465559666720305));
#89005=DIRECTION('center_axis',(0.,1.,-4.27898457407613E-15));
#89006=DIRECTION('ref_axis',(0.,-4.27898457407613E-15,-1.));
#89007=DIRECTION('center_axis',(-0.0115145015438457,0.982569635704634,0.185537940177905));
#89008=DIRECTION('ref_axis',(-0.990667703801824,-0.0364113341316314,0.131345785584377));
#89009=DIRECTION('center_axis',(-0.0343527775896078,-0.987363723829323,
-0.15470217690056));
#89010=DIRECTION('ref_axis',(-0.975089038524001,-0.000828289881604484,0.221812264958932));
#89011=DIRECTION('',(-0.560005583301831,0.,0.828488833159975));
#89012=DIRECTION('center_axis',(-2.55342966086297E-13,-1.,7.88012148952781E-14));
#89013=DIRECTION('ref_axis',(1.,-2.55342966086297E-13,-6.56380829255718E-31));
#89014=DIRECTION('center_axis',(-0.0174319786951678,0.987363878487336,-0.157507769894744));
#89015=DIRECTION('ref_axis',(-0.963443691424393,0.025533878586369,0.26669134687664));
#89016=DIRECTION('center_axis',(0.0572415384935087,0.987363724423093,0.147771045757462));
#89017=DIRECTION('ref_axis',(-0.94725422437822,0.00696333293275186,0.320407469313818));
#89018=DIRECTION('',(0.828488831038156,0.,0.560005586440912));
#89019=DIRECTION('center_axis',(0.00706195074453439,-0.98736372248627,0.158313007582248));
#89020=DIRECTION('ref_axis',(-0.996651285552064,0.00594770480154678,0.081552681225151));
#89021=DIRECTION('center_axis',(-5.22595194025683E-13,-1.,4.34288782212213E-14));
#89022=DIRECTION('ref_axis',(1.,-5.22595194025683E-13,8.12900788325336E-31));
#89023=DIRECTION('center_axis',(-0.0502692615742574,0.983673455286747,-0.172799116621036));
#89024=DIRECTION('ref_axis',(-0.964402445769318,-0.00283388505453427,0.26442369729216));
#89025=DIRECTION('center_axis',(0.,1.,-4.27898457407613E-15));
#89026=DIRECTION('ref_axis',(0.,-4.27898457407613E-15,-1.));
#89027=DIRECTION('center_axis',(-0.0511301072340958,0.982569648595428,0.178724922138149));
#89028=DIRECTION('ref_axis',(-0.995741923384931,-0.0364109742150284,-0.0846892140144853));
#89029=DIRECTION('center_axis',(-0.000293231080172163,-0.987363723819408,
-0.158470157761663));
#89030=DIRECTION('ref_axis',(-0.99997507892601,-0.000828292153617314,0.00701109542287292));
#89031=DIRECTION('',(-0.725013572849968,0.,0.688734578181845));
#89032=DIRECTION('center_axis',(8.87710405090975E-14,-1.,-7.35589882339766E-15));
#89033=DIRECTION('ref_axis',(1.,8.87710405090975E-14,-3.44266811200455E-31));
#89034=DIRECTION('center_axis',(0.0168351068554852,0.987363878107483,-0.157572686039542));
#89035=DIRECTION('ref_axis',(-0.998249669190184,0.0255338992760699,0.0533443338082583));
#89036=DIRECTION('center_axis',(0.0241368608849463,0.987363724418675,0.156621478886847));
#89037=DIRECTION('ref_axis',(-0.99398608115497,0.00696333673097982,0.109284868173762));
#89038=DIRECTION('',(0.688734576602033,0.,0.725013574350727));
#89039=DIRECTION('center_axis',(-0.0271357688700418,-0.987363722528924,
0.156129848144604));
#89040=DIRECTION('ref_axis',(-0.990881548149455,0.00594770300098519,-0.134604540658744));
#89041=DIRECTION('center_axis',(-2.33870895678053E-12,-1.,-3.14680407007958E-13));
#89042=DIRECTION('ref_axis',(1.,-2.33870895678053E-12,1.39936086943571E-29));
#89043=DIRECTION('center_axis',(-0.0119474158641637,0.983673454794409,-0.179565569046522));
#89044=DIRECTION('ref_axis',(-0.998698529282127,-0.00283400570072031,0.0509236293031502));
#89045=DIRECTION('center_axis',(0.,1.,-1.15648231693495E-15));
#89046=DIRECTION('ref_axis',(0.,-1.15648231693495E-15,-1.));
#89047=DIRECTION('center_axis',(-0.0883556907948313,0.982569633847177,0.163554842623486));
#89048=DIRECTION('ref_axis',(-0.954256320475309,-0.0364113920932505,-0.29676435998744));
#89049=DIRECTION('center_axis',(0.0337800228186421,-0.987363723842413,-0.1548282496782));
#89050=DIRECTION('ref_axis',(-0.978103395941278,-0.000828291187283654,-0.20811790115665));
#89051=DIRECTION('',(-0.856120733893417,0.,0.51677585953467));
#89052=DIRECTION('center_axis',(2.94256412139621E-14,-1.,3.96640921599374E-15));
#89053=DIRECTION('ref_axis',(1.,2.94256412139621E-14,-2.02248610404404E-31));
#89054=DIRECTION('center_axis',(0.0503150650657662,0.987363876577224,-0.15026965581189));
#89055=DIRECTION('ref_axis',(-0.986378597171141,0.0255339838968591,-0.162497011384971));
#89056=DIRECTION('center_axis',(-0.0100964402476896,0.987363724433846,0.158148466848242));
#89057=DIRECTION('ref_axis',(-0.994240255523169,0.00696332969227714,-0.106947773875007));
#89058=DIRECTION('',(0.516775858941039,0.,0.856120734251748));
#89059=DIRECTION('center_axis',(-0.060064648265057,-0.987363722569294,0.14664623207877));
#89060=DIRECTION('ref_axis',(-0.938779290848018,0.00594769916006849,-0.3444678039376));
#89061=DIRECTION('center_axis',(2.46264932681847E-13,-1.,9.00085221191213E-14));
#89062=DIRECTION('ref_axis',(1.,2.46264932681847E-13,-2.27872523730751E-30));
#89063=DIRECTION('center_axis',(0.026932910420601,0.98367345360326,-0.177935817115363));
#89064=DIRECTION('ref_axis',(-0.986296594519741,-0.00283429344636968,-0.164957553386989));
#89065=DIRECTION('center_axis',(0.,1.,6.24500451401115E-15));
#89066=DIRECTION('ref_axis',(0.,6.24500451401115E-15,-1.));
#89067=DIRECTION('center_axis',(-0.121449392028066,0.982569635669132,0.140737188536086));
#89068=DIRECTION('ref_axis',(-0.868150771829313,-0.036411333705666,-0.494963081603004));
#89069=DIRECTION('center_axis',(0.066273764426829,-0.987363723798804,-0.143946743884176));
#89070=DIRECTION('ref_axis',(-0.910496684258415,-0.000828293773487352,-0.413515540075408));
#89071=DIRECTION('',(-0.947196640816497,0.,0.320653276337453));
#89072=DIRECTION('center_axis',(-1.39425126750654E-13,-1.,-5.09965991050609E-14));
#89073=DIRECTION('ref_axis',(1.,-1.39425126750654E-13,2.37851799223888E-30));
#89074=DIRECTION('center_axis',(0.0814421546484781,0.987363878604472,-0.135940231989459));
#89075=DIRECTION('ref_axis',(-0.928385569322247,0.0255338686512898,-0.370740146498738));
#89076=DIRECTION('center_axis',(-0.0438576377861118,0.987363724437607,0.152280607013892));
#89077=DIRECTION('ref_axis',(-0.948004858277966,0.00696332974445473,-0.318179667358307));
#89078=DIRECTION('',(0.320653274273476,0.,0.947196641515213));
#89079=DIRECTION('center_axis',(-0.0901849776072001,-0.98736372250566,0.13030559962548));
#89080=DIRECTION('ref_axis',(-0.842780756740556,0.00594770166763986,-0.538224136315614));
#89081=DIRECTION('center_axis',(1.76926578827669E-12,-1.,1.12675082955071E-12));
#89082=DIRECTION('ref_axis',(1.,1.76926578827669E-12,-4.04402725272487E-29));
#89083=DIRECTION('center_axis',(0.0645545535556254,0.983673455265295,-0.167985841729802));
#89084=DIRECTION('ref_axis',(-0.927776503494073,-0.00283389108700792,-0.373125620435824));
#89085=DIRECTION('center_axis',(-7.60100351384829E-30,1.,-4.27898457407613E-15));
#89086=DIRECTION('ref_axis',(-1.77635683940025E-15,-4.27898457407613E-15,
-1.));
#89087=DIRECTION('center_axis',(-0.148864294762263,0.982569636291619,0.111338814358196));
#89088=DIRECTION('ref_axis',(-0.741451459750958,-0.0364113156534541,-0.670017872094139));
#89089=DIRECTION('center_axis',(0.0956686121200815,-0.987363723836582,-0.126334450988536));
#89090=DIRECTION('ref_axis',(-0.800316162506508,-0.000828290255901962,-0.599577646319564));
#89091=DIRECTION('',(-0.993982685952451,0.,0.109537299705404));
#89092=DIRECTION('center_axis',(0.,-1.,0.));
#89093=DIRECTION('ref_axis',(0.,0.,-1.));
#89094=DIRECTION('center_axis',(0.108761234480361,0.987363878205077,-0.115254353020345));
#89095=DIRECTION('ref_axis',(-0.826982255347822,0.0255338944294636,-0.561647905342034));
#89096=DIRECTION('center_axis',(-0.0755680941385575,0.987363724415618,0.139292278523919));
#89097=DIRECTION('ref_axis',(-0.857441809996997,0.00696333571685899,-0.514533822430332));
#89098=DIRECTION('',(0.109537300692827,0.,0.993982685843636));
#89099=DIRECTION('center_axis',(-0.116088355286957,-0.987363722529239,0.107872022322625));
#89100=DIRECTION('ref_axis',(-0.707374732400917,0.00594770236913799,-0.706813704449241));
#89101=DIRECTION('center_axis',(1.11426240627337E-12,-1.,1.11056089515527E-12));
#89102=DIRECTION('ref_axis',(1.,1.11426240627337E-12,3.64970774101204E-29));
#89103=DIRECTION('center_axis',(0.0991569279023106,0.983673453428792,-0.150181359257569));
#89104=DIRECTION('ref_axis',(-0.825874670625604,-0.00283432932651998,-0.563846605910082));
#89105=DIRECTION('center_axis',(0.,1.,-4.27898457407613E-15));
#89106=DIRECTION('ref_axis',(0.,-4.27898457407613E-15,-1.));
#89107=DIRECTION('center_axis',(-0.169318486318183,0.982569636205712,0.0767343482248568));
#89108=DIRECTION('ref_axis',(-0.580082699670365,-0.0364113198382961,-0.813743373140927));
#89109=DIRECTION('center_axis',(0.120590108538849,-0.987363723795561,-0.102814895103539));
#89110=DIRECTION('ref_axis',(-0.652713741417794,-0.000828293707041192,-0.75760417481289));
#89111=DIRECTION('',(-0.994291204850995,0.,-0.106700515256288));
#89112=DIRECTION('center_axis',(-1.47176262462041E-13,-1.,-1.46756891477855E-13));
#89113=DIRECTION('ref_axis',(1.,-1.47176262462041E-13,6.44798894018817E-30));
#89114=DIRECTION('center_axis',(0.130994717001781,0.987363878694593,-0.0891793427133922));
#89115=DIRECTION('ref_axis',(-0.686910176005267,0.0255338649006621,-0.726293626464978));
#89116=DIRECTION('center_axis',(-0.103745077874136,0.987363724403459,0.119790794926074));
#89117=DIRECTION('ref_axis',(-0.726785732907313,0.00696333438935478,-0.686828952808894));
#89118=DIRECTION('',(-0.106700517422838,0.,0.994291204618495));
#89119=DIRECTION('center_axis',(-0.136563572302587,-0.987363722483103,0.0803944665027728));
#89120=DIRECTION('ref_axis',(-0.538892649528834,0.00594770583704457,-0.842353451396187));
#89121=DIRECTION('center_axis',(-4.24736902889226E-13,-1.,-6.62065039069767E-13));
#89122=DIRECTION('ref_axis',(1.77844195838957E-29,6.62065039069767E-13,
-1.));
#89123=DIRECTION('center_axis',(0.129123319223923,0.983673453902652,-0.125354315920209));
#89124=DIRECTION('ref_axis',(-0.685355812260115,-0.00283422476887034,-0.728202841089787));
#89125=DIRECTION('center_axis',(0.,1.,-4.27898457407613E-15));
#89126=DIRECTION('ref_axis',(0.,-4.27898457407613E-15,-1.));
#89127=DIRECTION('center_axis',(-0.181855534063347,0.982569635880059,0.038541865251469));
#89128=DIRECTION('ref_axis',(-0.391589916338328,-0.0364113275118482,-0.919419138723448));
#89129=DIRECTION('center_axis',(0.139872940537657,-0.987363723824141,-0.0744878337815988));
#89130=DIRECTION('ref_axis',(-0.474591153553507,-0.000828290669261229,-0.88020597072692));
#89131=DIRECTION('',(-0.948107772469134,0.,-0.317949133956387));
#89132=DIRECTION('center_axis',(4.80801298666205E-14,-1.,7.49847183817704E-14));
#89133=DIRECTION('ref_axis',(2.14746147750984E-30,-7.49847183817705E-14,
-1.));
#89134=DIRECTION('center_axis',(0.147103062861328,0.987363878429286,-0.0589343742640444));
#89135=DIRECTION('ref_axis',(-0.514718935115872,0.0255338794681674,-0.856978668831663));
#89136=DIRECTION('center_axis',(-0.127071055085179,0.987363724395657,0.0946880283197176));
#89137=DIRECTION('ref_axis',(-0.562145965376946,0.0069633349371206,-0.827008721584588));
#89138=DIRECTION('',(-0.317949138606538,-1.49610497417568E-14,0.9481077709097));
#89139=DIRECTION('center_axis',(-0.150653225448128,-0.987363722481458,0.049157758183571));
#89140=DIRECTION('ref_axis',(-0.345212548031876,0.00594770514329176,-0.938505685376955));
#89141=DIRECTION('center_axis',(-1.8165491871178E-13,-1.,-4.91928138225692E-13));
#89142=DIRECTION('ref_axis',(5.43771059840649E-30,4.91928138225691E-13,
-1.));
#89143=DIRECTION('center_axis',(0.153052046561606,0.983673454582958,-0.0946657582874232));
#89144=DIRECTION('ref_axis',(-0.512790461815737,-0.00283405764388026,-0.858509120736684));
#89145=DIRECTION('center_axis',(0.,1.,-4.27898457407613E-15));
#89146=DIRECTION('ref_axis',(0.,-4.27898457407613E-15,-1.));
#89147=DIRECTION('center_axis',(-0.185889211649551,0.982569636439812,-0.00145276937064705));
#89148=DIRECTION('ref_axis',(-0.184786826538217,-0.0364113103312805,-0.982103887181949));
#89149=DIRECTION('center_axis',(0.152615469816189,-0.987363723872379,-0.0426778063359844));
#89150=DIRECTION('ref_axis',(-0.274277213979071,-0.000828286521980904,-0.961650312657005));
#89151=DIRECTION('',(-0.85759187372498,0.,-0.514330806116917));
#89152=DIRECTION('center_axis',(3.08365452100123E-14,-1.,8.35674239769942E-14));
#89153=DIRECTION('ref_axis',(-1.42611513161612E-30,-8.35674239769942E-14,
-1.));
#89154=DIRECTION('center_axis',(0.156333027251661,0.987363878204671,-0.0259336963613628));
#89155=DIRECTION('ref_axis',(-0.318460008541339,0.0255338945707047,-0.947592340190602));
#89156=DIRECTION('center_axis',(-0.144455329569359,0.987363724393657,0.0651577586362149));
#89157=DIRECTION('ref_axis',(-0.371220879538658,0.00696333928487479,-0.928518481507261));
#89158=DIRECTION('',(-0.514330810099968,0.,0.857591871336191));
#89159=DIRECTION('center_axis',(-0.157698501364659,-0.987363722506079,0.0156224884790626));
#89160=DIRECTION('ref_axis',(-0.135390689940926,0.00594770349990451,-0.990774437447998));
#89161=DIRECTION('center_axis',(1.07486897960175E-13,-1.,7.79216493293677E-13));
#89162=DIRECTION('ref_axis',(-6.24504444031443E-30,-7.79216493293677E-13,
-1.));
#89163=DIRECTION('center_axis',(0.169824166749787,0.983673455248736,-0.059550699632786));
#89164=DIRECTION('ref_axis',(-0.316247594399455,-0.00283389191344847,-0.948672455641662));
#89165=DIRECTION('center_axis',(0.,1.,-6.93889390918615E-16));
#89166=DIRECTION('ref_axis',(0.,-6.93889390918615E-16,-1.));
#89167=DIRECTION('center_axis',(-0.181230923707162,0.982569636964586,-0.0413794732630985));
#89168=DIRECTION('ref_axis',(0.0306566983224309,-0.0364112919812353,-0.998866549977636));
#89169=DIRECTION('center_axis',(0.158221872134797,-0.987363723844001,-0.00887220463401044));
#89170=DIRECTION('ref_axis',(-0.0611383729137627,-0.000828289971577882,
-0.998128956244222));
#89171=DIRECTION('',(-0.726975931972861,0.,-0.686662940846665));
#89172=DIRECTION('center_axis',(8.10071867472569E-15,-1.,5.8828406537924E-14));
#89173=DIRECTION('ref_axis',(-2.96027912643716E-31,-5.8828406537924E-14,
-1.));
#89174=DIRECTION('center_axis',(0.158253025172948,0.987363878522611,0.00827957803249001));
#89175=DIRECTION('ref_axis',(-0.107310253376575,0.0255338744852763,-0.993897646024995));
#89176=DIRECTION('center_axis',(-0.155085035730741,0.987363724409335,0.0325807828776812));
#89177=DIRECTION('ref_axis',(-0.162937899276276,0.00696334414091573,-0.986611753841302));
#89178=DIRECTION('',(-0.686662940911435,-1.49610497356062E-14,0.726975931911682));
#89179=DIRECTION('center_axis',(-0.157369971134395,-0.987363722499165,-0.0186432743302372));
#89180=DIRECTION('ref_axis',(0.0807618870172637,0.00594770483092212,-0.996715677820237));
#89181=DIRECTION('center_axis',(-1.45914037233135E-13,-1.,1.82957882068821E-12));
#89182=DIRECTION('ref_axis',(-5.57821049776919E-30,-1.82957882068821E-12,
-1.));
#89183=DIRECTION('center_axis',(0.178655370734987,0.983673453557913,-0.021651680604346));
#89184=DIRECTION('ref_axis',(-0.104917442185756,-0.0028343060231339,-0.994476896179376));
#89185=DIRECTION('center_axis',(-1.17815554464648E-28,1.,-4.27898457407613E-15));
#89186=DIRECTION('ref_axis',(-2.75335310107039E-14,-4.27898457407613E-15,
-1.));
#89187=DIRECTION('center_axis',(-0.168098470378799,0.982569635535979,-0.0793713775803403));
#89188=DIRECTION('ref_axis',(0.244666740213606,-0.0364113367971972,-0.968923320384998));
#89189=DIRECTION('center_axis',(0.156429994655349,-0.987363723877192,0.0253482453730552));
#89190=DIRECTION('ref_axis',(0.154859228584172,-0.000828287352707057,-0.987936198983708));
#89191=DIRECTION('',(-0.56236740413906,0.,-0.82688747890018));
#89192=DIRECTION('center_axis',(-7.1025601078218E-15,-1.,8.87916691229752E-14));
#89193=DIRECTION('ref_axis',(1.85894219214295E-31,-8.87916691229752E-14,
-1.));
#89194=DIRECTION('center_axis',(0.152773294212726,0.987363878745721,0.0421057184192046));
#89195=DIRECTION('ref_axis',(0.108857216014725,0.0255338639803358,-0.993729403968584));
#89196=DIRECTION('center_axis',(-0.158463138768053,0.987363724435778,-0.00151964472347802));
#89197=DIRECTION('ref_axis',(0.0529638481076019,0.00696333330908011,-0.998572152016499));
#89198=DIRECTION('',(-0.826887480125574,0.,0.562367402337279));
#89199=DIRECTION('center_axis',(-0.149682997251398,-0.987363722535522,-0.0520372919610015));
#89200=DIRECTION('ref_axis',(0.293138125971869,0.00594769977683875,-0.956051601101669));
#89201=DIRECTION('center_axis',(-1.53087973129973E-13,-1.,5.01553352378593E-13));
#89202=DIRECTION('ref_axis',(-1.5439867913458E-30,-5.01553352378593E-13,
-1.));
#89203=DIRECTION('center_axis',(0.179132969840175,0.983673453912093,0.017260219723152));
#89204=DIRECTION('ref_axis',(0.111318599148628,-0.00283423072957411,-0.993780728641766));
#89205=DIRECTION('center_axis',(5.42341871852767E-29,1.,1.3877787795361E-15));
#89206=DIRECTION('ref_axis',(-3.90798504668055E-14,1.3877787795361E-15,
-1.));
#89207=DIRECTION('center_axis',(-0.147105795085869,0.982569626528976,-0.113652162649302));
#89208=DIRECTION('ref_axis',(0.447236418309252,-0.0364116177255003,-0.893674314407953));
#89209=DIRECTION('center_axis',(0.147323624967262,-0.987363723844384,0.0583834425385917));
#89210=DIRECTION('ref_axis',(0.36361578510832,-0.000828287599040628,-0.931548643260089));
#89211=DIRECTION('',(-0.371463200767281,0.,-0.928447677834204));
#89212=DIRECTION('center_axis',(-7.80722712912228E-14,-1.,2.55566786620522E-13));
#89213=DIRECTION('ref_axis',(1.23397180528547E-30,-2.55566786620522E-13,
-1.));
#89214=DIRECTION('center_axis',(0.140149924152897,0.987363872412991,0.0739633842760113));
#89215=DIRECTION('ref_axis',(0.319934693632977,0.025534215437582,-0.947095452239087));
#89216=DIRECTION('center_axis',(-0.154431681661387,0.987363724384509,-0.0355490009534356));
#89217=DIRECTION('ref_axis',(0.266389055963699,0.0069633360032921,-0.96384043431186));
#89218=DIRECTION('',(-0.928447677255466,0.,0.3714632022138));
#89219=DIRECTION('center_axis',(-0.134997009578242,-0.987363722498697,-0.0829981138246456));
#89220=DIRECTION('ref_axis',(0.491807553744111,0.00594770547493303,-0.870683613535833));
#89221=DIRECTION('center_axis',(3.85992086760888E-13,-1.,-6.85377023961864E-13));
#89222=DIRECTION('ref_axis',(1.33719385355037E-30,6.85377023961864E-13,
-1.));
#89223=DIRECTION('center_axis',(0.171234423252512,0.983673454841072,0.0553652105063214));
#89224=DIRECTION('ref_axis',(0.322349575412552,-0.00283399345383913,-0.946616458610588));
#89225=DIRECTION('center_axis',(-1.06414049193876E-28,1.,-4.27898457407613E-15));
#89226=DIRECTION('ref_axis',(-2.48689957516035E-14,-4.27898457407613E-15,
-1.));
#89227=DIRECTION('center_axis',(-0.119234878010352,0.982569636402058,-0.142618208818457));
#89228=DIRECTION('ref_axis',(0.628893860402292,-0.0364113135319287,-0.776638093705931));
#89229=DIRECTION('center_axis',(0.131328564306877,-0.98736372382475,0.0886886975438091));
#89230=DIRECTION('ref_axis',(0.555370071831342,-0.00082829114203254,-0.831602908393083));
#89231=DIRECTION('',(-0.163189791341605,0.,-0.98659469489851));
#89232=DIRECTION('center_axis',(5.83050175047892E-14,-1.,-1.03470465022567E-13));
#89233=DIRECTION('ref_axis',(2.02332272046579E-30,1.03470465022567E-13,
-1.));
#89234=DIRECTION('center_axis',(0.120973533980727,0.987363878077678,0.102361986809662));
#89235=DIRECTION('ref_axis',(0.516052284274361,0.0255339002001935,-0.856176418640329));
#89236=DIRECTION('center_axis',(-0.143179166359676,0.987363724446293,-0.0679161392313565));
#89237=DIRECTION('ref_axis',(0.467358252587167,0.0069633313518086,-0.884040596214424));
#89238=DIRECTION('',(-0.986594695254103,0.,0.163189789191801));
#89239=DIRECTION('center_axis',(-0.113998716707124,-0.98736372251679,-0.110078027084955));
#89240=DIRECTION('ref_axis',(0.667480605241743,0.00594770079844067,-0.74460342900186));
#89241=DIRECTION('center_axis',(-8.73839331637463E-13,-1.,9.77293987086083E-13));
#89242=DIRECTION('ref_axis',(-4.44913230794167E-30,-9.77293987086083E-13,
-1.));
#89243=DIRECTION('center_axis',(0.155329156822049,0.983673454978525,0.0908811697303888));
#89244=DIRECTION('ref_axis',(0.518307778400948,-0.0028339603480268,-0.855189461767286));
#89245=DIRECTION('center_axis',(1.52533651582418E-28,1.,-6.36065274470406E-15));
#89246=DIRECTION('ref_axis',(2.39808173319034E-14,-6.36065274470406E-15,
-1.));
#89247=DIRECTION('center_axis',(-0.0857885343236945,0.982569636375351,-0.164915848394877));
#89248=DIRECTION('ref_axis',(0.781144903269328,-0.0364113132365839,-0.623287137974738));
#89249=DIRECTION('center_axis',(0.109192725242245,-0.987363723808637,0.114846966267784));
#89250=DIRECTION('ref_axis',(0.721155873171584,-0.000828293443733472,-0.692772343934212));
#89251=DIRECTION('',(0.0527141884073562,0.,-0.998609640620675));
#89252=DIRECTION('center_axis',(3.95924850534664E-14,-1.,-4.42587639328991E-14));
#89253=DIRECTION('ref_axis',(1.36628995448307E-30,4.42587639328991E-14,
-1.));
#89254=DIRECTION('center_axis',(0.0961404457214033,0.987363878266434,0.12597454739413));
#89255=DIRECTION('ref_axis',(0.68803988955902,0.0255338903723136,-0.725223504044143));
#89256=DIRECTION('center_axis',(-0.125231756383122,0.987363724377778,-0.0971075845443635));
#89257=DIRECTION('ref_axis',(0.646474270713916,0.00696333327397,-0.762904010537778));
#89258=DIRECTION('',(-0.998609640362467,0.,-0.0527141932988016));
#89259=DIRECTION('center_axis',(-0.0876699683262286,-0.987363722531034,
-0.132010818054195));
#89260=DIRECTION('ref_axis',(0.811943006995923,0.00594770035885419,-0.58370641443354));
#89261=DIRECTION('center_axis',(-1.4888983012459E-12,-1.,1.0732340937512E-12));
#89262=DIRECTION('ref_axis',(1.,-1.4888983012459E-12,-4.69499685681978E-29));
#89263=DIRECTION('center_axis',(0.132160981848279,0.983673454392736,0.122147492810783));
#89264=DIRECTION('ref_axis',(0.690030470301091,-0.00283410202124129,-0.723774770161125));
#89265=DIRECTION('center_axis',(-2.4703261420007E-28,1.,-4.27898457407613E-15));
#89266=DIRECTION('ref_axis',(-5.77315972805081E-14,-4.27898457407613E-15,
-1.));
#89267=DIRECTION('center_axis',(-0.048330800738981,0.982569635885247,-0.179502212622192));
#89268=DIRECTION('ref_axis',(0.896870480711448,-0.0364113271556149,-0.440791964630915));
#89269=DIRECTION('center_axis',(0.0819511579642553,-0.987363723811783,0.135635115692239));
#89270=DIRECTION('ref_axis',(0.853221223833652,-0.000828292888265932,-0.52154851848193));
#89271=DIRECTION('',(0.266153315026551,0.,-0.96393070959503));
#89272=DIRECTION('center_axis',(0.,-1.,0.));
#89273=DIRECTION('ref_axis',(0.,0.,-1.));
#89274=DIRECTION('center_axis',(0.0668119404962166,0.987363878416488,0.143696681261193));
#89275=DIRECTION('ref_axis',(0.827855514450642,0.0255338802774692,-0.560359945170637));
#89276=DIRECTION('center_axis',(-0.101428648131142,0.987363724383358,-0.121758388253595));
#89277=DIRECTION('ref_axis',(0.795361873886099,0.00696333474618824,-0.606094878329793));
#89278=DIRECTION('',(-0.963930709015073,0.,-0.266153317126987));
#89279=DIRECTION('center_axis',(-0.0572418717027848,-0.987363722547846,
-0.147770929212829));
#89280=DIRECTION('ref_axis',(0.918439855202016,0.00594769809152563,-0.395515938065601));
#89281=DIRECTION('center_axis',(2.40686042267118E-13,-1.,-1.04010479394898E-13));
#89282=DIRECTION('ref_axis',(1.,2.40686042267118E-13,2.52683201209334E-30));
#89283=DIRECTION('center_axis',(0.102812939313603,0.983673454849758,0.147702517695669));
#89284=DIRECTION('ref_axis',(0.829488134170337,-0.00283399370384824,-0.558517147230324));
#89285=DIRECTION('center_axis',(3.80050175692414E-28,1.,-4.27898457407613E-15));
#89286=DIRECTION('ref_axis',(8.88178419700125E-14,-4.27898457407613E-15,
-1.));
#89287=DIRECTION('center_axis',(-0.00861320750497983,0.982569636773598,
-0.185695238353267));
#89288=DIRECTION('ref_axis',(0.970659390064181,-0.0364113029242347,-0.237685854647665));
#89289=DIRECTION('center_axis',(0.0508776450489319,-0.987363723838188,0.150081118341584));
#89290=DIRECTION('ref_axis',(0.945390901075399,-0.000828292330195558,-0.325937659830314));
#89291=DIRECTION('',(0.467147407829532,0.,-0.884179449748833));
#89292=DIRECTION('center_axis',(1.63550816575494E-13,-1.,-7.06311398100092E-14));
#89293=DIRECTION('ref_axis',(1.,1.63550816575494E-13,1.71046772606188E-30));
#89294=DIRECTION('center_axis',(0.0343593611981407,0.987363878193159,0.154699729597115));
#89295=DIRECTION('ref_axis',(0.928961537110486,0.0255338952362097,-0.369294574511176));
#89296=DIRECTION('center_axis',(-0.0728828540416005,0.987363724372173,-0.140715903083703));
#89297=DIRECTION('ref_axis',(0.907059237206504,0.00696334084921954,-0.420945426489672));
#89298=DIRECTION('',(-0.884179449358273,0.,-0.467147408568753));
#89299=DIRECTION('center_axis',(-0.0241372016724106,-0.987363722529379,
-0.156621438278268));
#89300=DIRECTION('ref_axis',(0.981991477421219,0.00594770310859909,-0.188831573365852));
#89301=DIRECTION('center_axis',(0.,-1.,0.));
#89302=DIRECTION('ref_axis',(0.,0.,-1.));
#89303=DIRECTION('center_axis',(0.0686577849377437,0.983673453837433,0.166350968686623));
#89304=DIRECTION('ref_axis',(0.930159821925432,-0.00283423621027203,-0.367143940138951));
#89305=DIRECTION('center_axis',(1.82424084332359E-28,1.,-4.27898457407613E-15));
#89306=DIRECTION('ref_axis',(4.2632564145606E-14,-4.27898457407613E-15,
-1.));
#89307=DIRECTION('center_axis',(0.031507168033603,0.982569636191183,-0.183205372185503));
#89308=DIRECTION('ref_axis',(0.999061345195437,-0.0364113191898648,-0.0234658128164505));
#89309=DIRECTION('center_axis',(0.0174251520844417,-0.987363723855214,0.15750949460143));
#89310=DIRECTION('ref_axis',(0.993355149241018,-0.00082829030093904,-0.115086321565737));
#89311=DIRECTION('',(0.646298207761542,0.,-0.763084940648299));
#89312=DIRECTION('center_axis',(5.83035654598128E-14,-1.,-1.12737439807098E-14));
#89313=DIRECTION('ref_axis',(1.,5.83035654598128E-14,1.90037748068761E-31));
#89314=DIRECTION('center_axis',(0.000300225257138507,0.98736387884835,0.158469178739384));
#89315=DIRECTION('ref_axis',(0.98663034989482,0.0255338596358639,-0.160961407419668));
#89316=DIRECTION('center_axis',(-0.0409291257697323,0.987363724396822,-0.153093704667965));
#89317=DIRECTION('ref_axis',(0.976343520524065,0.0069633328823719,-0.21611303043973));
#89318=DIRECTION('',(-0.763084940440831,0.,-0.646298208006501));
#89319=DIRECTION('',(0.795228819341496,0.,-0.606309429984995));
#89320=DIRECTION('',(-0.606309429638273,0.,-0.795228819605849));
#89321=DIRECTION('center_axis',(0.0438573042826761,-0.987363722495775,-0.152280715654819));
#89322=DIRECTION('ref_axis',(0.970519647114226,0.00594770341361158,0.240948623962417));
#89323=DIRECTION('center_axis',(-5.09105898905421E-13,-1.,-1.25709930644235E-13));
#89324=DIRECTION('ref_axis',(1.,-5.09105898905421E-13,-1.1652925221308E-30));
#89325=DIRECTION('center_axis',(-0.00753699341927212,0.983673454470314,
0.179804695991614));
#89326=DIRECTION('ref_axis',(0.998349928692214,-0.00283408599568885,0.0573531850625539));
#89327=DIRECTION('center_axis',(2.50833115956993E-28,1.,-4.27898457407613E-15));
#89328=DIRECTION('ref_axis',(5.86197757002083E-14,-4.27898457407613E-15,
-1.));
#89329=DIRECTION('center_axis',(0.105521068239957,0.982569636245178,-0.153043177196886));
#89330=DIRECTION('ref_axis',(0.916576558659195,-0.0364113166791358,0.398197976054825));
#89331=DIRECTION('center_axis',(-0.0503218807322454,-0.987363723831604,
0.150268377182156));
#89332=DIRECTION('ref_axis',(0.949868207862548,-0.000828290154810337,0.312649486849749));
#89333=DIRECTION('',(0.906975415979067,0.,-0.421183564268121));
#89334=DIRECTION('center_axis',(0.,-1.,0.));
#89335=DIRECTION('ref_axis',(0.,0.,-1.));
#89336=DIRECTION('center_axis',(-0.0662670360058364,0.987363878238492,0.14394878217215));
#89337=DIRECTION('ref_axis',(0.963027392457796,0.025533892898744,0.268190718872546));
#89338=DIRECTION('center_axis',(0.0271361056266256,0.987363724411646,-0.156129777708749));
#89339=DIRECTION('ref_axis',(0.976848887222061,0.00696333644544283,0.213817126251775));
#89340=DIRECTION('',(-0.421183562291818,0.,-0.906975416896828));
#89341=DIRECTION('center_axis',(0.0755677988040467,-0.987363722485756,-0.139292452426475));
#89342=DIRECTION('ref_axis',(0.896032605267977,0.0059477050242739,0.443948414910591));
#89343=DIRECTION('center_axis',(-1.41053807967382E-12,-1.,-6.9664085453623E-13));
#89344=DIRECTION('ref_axis',(1.,-1.41053807967382E-12,-2.42403792294253E-29));
#89345=DIRECTION('center_axis',(-0.0460132468312074,0.983673453550403,0.173980797492924));
#89346=DIRECTION('ref_axis',(0.962679834130023,-0.00283432164793642,0.270627980039365));
#89347=DIRECTION('center_axis',(1.5582057203389E-28,1.,-4.27898457407613E-15));
#89348=DIRECTION('ref_axis',(3.64153152077052E-14,-4.27898457407613E-15,
-1.));
#89349=DIRECTION('center_axis',(0.135953811406594,0.982569635914727,-0.126781196328247));
#89350=DIRECTION('ref_axis',(0.809546713012962,-0.0364113265778112,0.585925195521368));
#89351=DIRECTION('center_axis',(-0.0814486413983933,-0.987363723826403,
0.135937469764647));
#89352=DIRECTION('ref_axis',(0.860450419908865,-0.000828289274779208,0.509533501170958));
#89353=DIRECTION('',(0.976312850813305,0.,-0.216363622951729));
#89354=DIRECTION('center_axis',(-1.33094108435448E-13,-1.,-6.57721627022386E-14));
#89355=DIRECTION('ref_axis',(1.,-1.33094108435448E-13,1.11854033061799E-30));
#89356=DIRECTION('center_axis',(-0.0956624610075087,0.98736387863115,0.126337899018621));
#89357=DIRECTION('ref_axis',(0.882859272566599,0.0255338678676378,0.468942988469701));
#89358=DIRECTION('center_axis',(0.0600649648957384,0.987363724432964,-0.146646089841971));
#89359=DIRECTION('ref_axis',(0.908046341563117,0.00696333706420843,0.418811835447339));
#89360=DIRECTION('',(-0.21636361808406,0.,-0.976312851892043));
#89361=DIRECTION('center_axis',(0.103744821263164,-0.987363722547432,-0.119791032462169));
#89362=DIRECTION('ref_axis',(0.779648074778519,0.00594769971540888,0.626189671235676));
#89363=DIRECTION('center_axis',(4.09267768806296E-13,-1.,3.27859260674821E-13));
#89364=DIRECTION('ref_axis',(1.,4.09267768806296E-13,2.71155125619176E-30));
#89365=DIRECTION('center_axis',(0.16002949161871,0.982569636160366,-0.0945910773167529));
#89366=DIRECTION('ref_axis',(0.664663364509743,-0.0364113192768025,0.746255202800699));
#89367=DIRECTION('center_axis',(-0.0823382876057148,0.983673453893709,0.160021693838619));
#89368=DIRECTION('ref_axis',(0.881995891203354,-0.00283423637138487,0.471248570294481));
#89369=DIRECTION('center_axis',(-1.56128720824992E-28,1.,-4.39463280580791E-15));
#89370=DIRECTION('ref_axis',(-3.5527136788005E-14,-4.39463280580791E-15,
-1.));
#89371=DIRECTION('center_axis',(-0.108766955552993,-0.987363723823093,0.115250276606735));
#89372=DIRECTION('ref_axis',(0.73079892771557,-0.000828290184863653,0.682592294993976));
#89373=DIRECTION('',(0.999998982184334,0.,-0.00142675516336331));
#89374=DIRECTION('center_axis',(2.31686742770906E-14,-1.,1.85691490357841E-14));
#89375=DIRECTION('ref_axis',(1.,2.31686742770906E-14,-7.24715462277955E-31));
#89376=DIRECTION('center_axis',(-0.120584843313759,0.987363878562272,0.102819584094973));
#89377=DIRECTION('ref_axis',(0.761409632159749,0.0255338730448354,0.647768008921162));
#89378=DIRECTION('center_axis',(0.0901852594295258,0.987363724414169,-0.130305390113422));
#89379=DIRECTION('ref_axis',(0.796784555967793,0.00696333089617327,0.604223372101773));
#89380=DIRECTION('',(-0.00142675585914351,0.,-0.999998982183341));
#89381=DIRECTION('center_axis',(0.127070856507359,-0.987363722538901,-0.0946883141713354));
#89382=DIRECTION('ref_axis',(0.626808067237821,0.0059477006431547,0.779150994161367));
#89383=DIRECTION('center_axis',(-1.15226743321196E-12,-1.,-1.42861098163512E-12));
#89384=DIRECTION('ref_axis',(-2.34737927052863E-29,1.42861098163512E-12,
-1.));
#89385=DIRECTION('center_axis',(-0.114813363762878,0.983673454762913,0.13858003426269));
#89386=DIRECTION('ref_axis',(0.76007077865168,-0.00283402119491597,0.649834117112741));
#89387=DIRECTION('center_axis',(0.,1.,-4.27898457407613E-15));
#89388=DIRECTION('ref_axis',(0.,-4.27898457407613E-15,-1.));
#89389=DIRECTION('center_axis',(0.17662236999008,0.982569636655051,-0.0579779918818218));
#89390=DIRECTION('ref_axis',(0.488701096710683,-0.0364113059965099,0.871691146490203));
#89391=DIRECTION('center_axis',(-0.130999450776611,-0.987363723786601,0.0891741041249308));
#89392=DIRECTION('ref_axis',(0.566976085211815,-0.000828295465522612,0.82373383609301));
#89393=DIRECTION('',(0.976926272506191,0.,0.213576820107329));
#89394=DIRECTION('center_axis',(3.72703708255265E-14,-1.,4.6231185537332E-14));
#89395=DIRECTION('ref_axis',(-1.04756410394469E-30,-4.6231185537332E-14,
-1.));
#89396=DIRECTION('center_axis',(-0.139868816840048,0.987363878289649,0.0744935294142248));
#89397=DIRECTION('ref_axis',(0.60435732197669,0.0255338886823933,0.796304117722568));
#89398=DIRECTION('center_axis',(0.116088579768143,0.987363724373446,-0.107871763862534));
#89399=DIRECTION('ref_axis',(0.648266013062696,0.00696333901246309,0.761382090817478));
#89400=DIRECTION('',(0.213576824979769,0.,-0.976926271440973));
#89401=DIRECTION('center_axis',(0.144455199395496,-0.987363722528263,-0.065158075499038));
#89402=DIRECTION('ref_axis',(0.444659211184389,0.00594770136013063,0.895680082818306));
#89403=DIRECTION('center_axis',(-1.16888399219326E-13,-1.,-2.34702002391639E-13));
#89404=DIRECTION('ref_axis',(-3.88788071104734E-30,2.34702002391639E-13,
-1.));
#89405=DIRECTION('center_axis',(-0.14191956762245,0.983673453820766,0.110658811552366));
#89406=DIRECTION('ref_axis',(0.602605669735964,-0.00283423879207645,0.798034068127759));
#89407=DIRECTION('center_axis',(0.,1.,-1.61907524309175E-15));
#89408=DIRECTION('ref_axis',(0.,-1.61907524309175E-15,-1.));
#89409=DIRECTION('center_axis',(0.184956653255885,0.982569629181649,-0.018653692026481));
#89410=DIRECTION('ref_axis',(0.289887718521787,-0.0364115390294351,0.956367769467239));
#89411=DIRECTION('center_axis',(-0.14710655139176,-0.987363723814766,0.0589282566538495));
#89412=DIRECTION('ref_axis',(0.376642076271981,-0.000828292363707701,0.926358494489737));
#89413=DIRECTION('',(0.90817357582681,0.,0.418593784198889));
#89414=DIRECTION('center_axis',(6.61516798739843E-14,-1.,1.32905885278519E-13));
#89415=DIRECTION('ref_axis',(1.72437707524548E-30,-1.32905885278519E-13,
-1.));
#89416=DIRECTION('center_axis',(-0.152612751853645,0.987363874356831,0.042684043701661));
#89417=DIRECTION('ref_axis',(0.419045901386645,0.0255341087752613,0.9076059397228));
#89418=DIRECTION('center_axis',(0.136563732792872,0.987363724405006,-0.0803941702784063));
#89419=DIRECTION('ref_axis',(0.469435287154992,0.00696333778263528,0.882939422101332));
#89420=DIRECTION('',(0.418593786177838,0.,-0.908173574914676));
#89421=DIRECTION('center_axis',(0.155084977486587,-0.987363722529484,-0.0325811170880482));
#89422=DIRECTION('ref_axis',(0.241718583101083,0.00594770221519151,0.970328166870345));
#89423=DIRECTION('center_axis',(3.18508154599476E-13,-1.,1.27171196046668E-12));
#89424=DIRECTION('ref_axis',(-1.33343971397308E-29,-1.27171196046668E-12,
-1.));
#89425=DIRECTION('center_axis',(-0.162389976522538,0.983673454176114,0.0775630780348588));
#89426=DIRECTION('ref_axis',(0.416963315730168,-0.00283415624667476,0.908918896763443));
#89427=DIRECTION('center_axis',(0.,1.,-4.27898457407613E-15));
#89428=DIRECTION('ref_axis',(0.,-4.27898457407613E-15,-1.));
#89429=DIRECTION('center_axis',(0.184642449885204,0.982569635942888,0.021542428448301));
#89430=DIRECTION('ref_axis',(0.0775194882547595,-0.036411326478108,0.996325721962865));
#89431=DIRECTION('center_axis',(-0.156335115827123,-0.987363723801012,0.0259269836486918));
#89432=DIRECTION('ref_axis',(0.168696700721925,-0.000828295499094795,0.985667660569273));
#89433=DIRECTION('',(0.796955691356011,0.,0.604037768699328));
#89434=DIRECTION('center_axis',(3.60342536859394E-14,-1.,1.44019275252605E-13));
#89435=DIRECTION('ref_axis',(1.34143802813749E-30,-1.44019275252605E-13,
-1.));
#89436=DIRECTION('center_axis',(-0.158220517681057,0.987363878676579,0.00887912549075674));
#89437=DIRECTION('ref_axis',(0.214140432742777,0.0255338675260978,0.97646909663025));
#89438=DIRECTION('center_axis',(0.150653321523514,0.987363724405075,-0.0491574251041693));
#89439=DIRECTION('ref_axis',(0.268654254564643,0.00696333221351926,0.963211505074976));
#89440=DIRECTION('',(0.604037770435926,0.,-0.796955690039789));
#89441=DIRECTION('center_axis',(0.158463153889849,-0.98736372254709,0.0015192949799761));
#89442=DIRECTION('ref_axis',(0.0274754649281728,0.00594770014627042,0.999604783747032));
#89443=DIRECTION('center_axis',(3.01449049754687E-14,-1.,1.04835990607084E-12));
#89444=DIRECTION('ref_axis',(-1.4108466334676E-30,-1.04835990607084E-12,
-1.));
#89445=DIRECTION('center_axis',(-0.175267182846845,0.983673454681373,0.0408405334458729));
#89446=DIRECTION('ref_axis',(0.211824227594113,-0.00283403766675145,0.977303670736307));
#89447=DIRECTION('center_axis',(0.,1.,-4.27898457407613E-15));
#89448=DIRECTION('ref_axis',(0.,-4.27898457407613E-15,-1.));
#89449=DIRECTION('center_axis',(0.175694629832079,0.982569636637783,0.0607314268370501));
#89450=DIRECTION('ref_axis',(-0.138473451533026,-0.0364113059094351,0.989696579777105));
#89451=DIRECTION('center_axis',(-0.158253622888124,-0.987363723835983,-0.00828659734288716));
#89452=DIRECTION('ref_axis',(-0.04713674460817,-0.000828289383721378,0.998888102464155));
#89453=DIRECTION('',(0.64847304670282,0.,0.76123761579415));
#89454=DIRECTION('center_axis',(3.38552468895019E-15,-1.,1.18718787206932E-13));
#89455=DIRECTION('ref_axis',(0.0285055878552679,1.187670502004E-13,0.99959363316351));
#89456=DIRECTION('center_axis',(-0.156430158416636,0.987363878238024,-0.0253412211330566));
#89457=DIRECTION('ref_axis',(-0.000778046602915284,0.0255338905306592,0.999673654288164));
#89458=DIRECTION('center_axis',(0.157698523550761,0.98736372441666,-0.015622143770062));
#89459=DIRECTION('ref_axis',(0.0553112685315642,0.00696333467226083,0.998444878570505));
#89460=DIRECTION('center_axis',(-0.15910099913347,-0.986495109064463,0.0389136462776974));
#89461=DIRECTION('ref_axis',(0.0348288484460351,0.0337827392776246,0.998822145250506));
#89462=DIRECTION('center_axis',(0.153085996405273,-0.986495981700291,-0.0582267618349548));
#89463=DIRECTION('ref_axis',(0.142839315879286,-0.0362134380952001,0.989083169779196));
#89464=DIRECTION('center_axis',(-0.147016025755211,-0.986495109314144,0.0722058686702008));
#89465=DIRECTION('ref_axis',(0.248731805575957,0.0337827286644027,0.967983066039335));
#89466=DIRECTION('center_axis',(0.136989899164217,-0.986495981735127,-0.0897744147707253));
#89467=DIRECTION('ref_axis',(0.352123454896517,-0.0362134363722373,0.935252724956123));
#89468=DIRECTION('center_axis',(-0.12805674336805,-0.986495109232666,0.102121838692806));
#89469=DIRECTION('ref_axis',(0.451004340964367,0.0337827324183721,0.891882173508164));
#89470=DIRECTION('center_axis',(0.114488302547269,-0.986495981577749,-0.117124322456091));
#89471=DIRECTION('ref_axis',(0.544942693575336,-0.036213442345283,0.837690902011215));
#89472=DIRECTION('center_axis',(-0.10310967042645,-0.986495109194319,0.127262702313903));
#89473=DIRECTION('ref_axis',(0.632188414504733,0.0337827335010053,0.774077861382944));
#89474=DIRECTION('center_axis',(0.086633361464682,-0.986495981838967,-0.13899762047209));
#89475=DIRECTION('ref_axis',(0.712281020862011,-0.0362134416118077,0.700959580836441));
#89476=DIRECTION('center_axis',(-0.073341303578005,-0.986495109199416,0.146452902719994));
#89477=DIRECTION('ref_axis',(0.783812058775744,0.0337827346231783,0.62007852999367));
#89478=DIRECTION('center_axis',(0.0547275474985977,-0.986495981988411,-0.154371542278719));
#89479=DIRECTION('ref_axis',(0.846313876508417,-0.0362134352149882,0.531452170509469));
#89480=DIRECTION('center_axis',(-0.040143577861672,-0.986495109147448,0.158795128340351));
#89481=DIRECTION('ref_axis',(0.898785522715291,0.0337827367069714,0.437085015595352));
#89482=DIRECTION('center_axis',(0.0202627271776249,-0.986495981683972,-0.1625272285148));
#89483=DIRECTION('ref_axis',(0.9407740341983,-0.0362134386515169,0.337094650564627));
#89484=DIRECTION('center_axis',(-0.00506879005578622,-0.986495109267344,
0.163712268199367));
#89485=DIRECTION('ref_axis',(0.971732775009283,0.0337827312287656,0.23365389156503));
#89486=DIRECTION('center_axis',(-0.0151495567526714,-0.986495981610252,
-0.163083319800101));
#89487=DIRECTION('ref_axis',(0.991244645617973,-0.0362134411919114,0.126974955053111));
#89488=DIRECTION('center_axis',(0.0302430200186485,-0.986495109092999,0.160974406275479));
#89489=DIRECTION('ref_axis',(0.999242882453265,0.0337827374707905,0.0192973706880221));
#89490=DIRECTION('center_axis',(-0.0498534591473214,-0.986495981670541,
-0.156013815923214));
#89491=DIRECTION('ref_axis',(0.99536575872004,-0.0362134386964945,-0.0890819466864886));
#89492=DIRECTION('center_axis',(0.0641406912897081,-0.986495109175036,0.150709559400234));
#89493=DIRECTION('ref_axis',(0.980029503274231,0.0337827344540997,-0.195961474695582));
#89494=DIRECTION('center_axis',(-0.0822262684116405,-0.986495981776016,
-0.141649280700155));
#89495=DIRECTION('ref_axis',(0.952944675122492,-0.0362134351371844,-0.300973476026134));
#89496=DIRECTION('center_axis',(0.0950392159144675,-0.98649510921924,0.133397702097462));
#89497=DIRECTION('ref_axis',(0.914991035274494,0.0337827328184258,-0.402057374426374));
#89498=DIRECTION('center_axis',(-0.110754276086024,-0.986495981633421,-0.120661379694472));
#89499=DIRECTION('ref_axis',(0.865964958740324,-0.0362134402304153,-0.498791817275051));
#89500=DIRECTION('center_axis',(0.121493814933346,-0.986495109215181,0.109848315542248));
#89501=DIRECTION('ref_axis',(0.807168602240863,0.0337827331963323,-0.589353522509468));
#89502=DIRECTION('center_axis',(-0.134103531952518,-0.986495981849886,-0.0940314868110145));
#89503=DIRECTION('ref_axis',(0.738493679513785,-0.0362134399459039,-0.673287213665516));
#89504=DIRECTION('center_axis',(0.142267496094858,-0.986495109287407,0.0811625462077628));
#89505=DIRECTION('ref_axis',(0.661603860893941,0.0337827300359943,-0.74909215614739));
#89506=DIRECTION('center_axis',(-0.151182255928033,-0.986495981692509,-0.0630047902706147));
#89507=DIRECTION('ref_axis',(0.576491261957089,-0.0362134382866778,-0.816300442101179));
#89508=DIRECTION('center_axis',(0.156388911180492,-0.986495109171287,0.0486817012943271));
#89509=DIRECTION('ref_axis',(0.48510326018357,0.0337827340495557,-0.873804070624192));
#89510=DIRECTION('center_axis',(-0.161191868028005,-0.986495981537598,-0.0290320528349762));
#89511=DIRECTION('ref_axis',(0.387532750534317,-0.0362134429097134,-0.92114437186357));
#89512=DIRECTION('center_axis',(0.163197752494024,-0.986495109143777,0.0139245544383681));
#89513=DIRECTION('ref_axis',(0.285919770480985,0.0337827368528131,-0.957657878127066));
#89514=DIRECTION('center_axis',(-0.16366432424346,-0.986495981676962,0.00629818268533493));
#89515=DIRECTION('ref_axis',(0.180453638313151,-0.0362134381069366,-0.982916614632198));
#89516=DIRECTION('center_axis',(0.16237564746021,-0.98649510913597,-0.021483685966046));
#89517=DIRECTION('ref_axis',(0.0733669880836664,0.0337827359901104,-0.996732668175652));
#89518=DIRECTION('center_axis',(-0.158484018513546,-0.9864959819173,0.0413339271884475));
#89519=DIRECTION('ref_axis',(-0.0350632868139038,-0.0362134385253087,-0.998728768379073));
#89520=DIRECTION('center_axis',(0.153961037350102,-0.986495109136799,-0.0558873744888276));
#89521=DIRECTION('ref_axis',(-0.142616351467159,0.0337827368293704,-0.989201346029469));
#89522=DIRECTION('center_axis',(-0.145893179781864,-0.986495981719679,0.0744369407220874));
#89523=DIRECTION('ref_axis',(-0.248940685134136,-0.0362134373496924,-0.967841475780134));
#89524=DIRECTION('center_axis',(0.138347381237093,-0.986495109182415,-0.087677828805308));
#89525=DIRECTION('ref_axis',(-0.351931111039965,0.0337827344076185,-0.935416067821224));
#89526=DIRECTION('center_axis',(-0.126480538531204,-0.986495981840687,0.104059363754717));
#89527=DIRECTION('ref_axis',(-0.451177899420923,-0.0362134328151596,-0.89169899089203));
#89528=DIRECTION('center_axis',(0.116264754633397,-0.986495109150601,-0.115368567868286));
#89529=DIRECTION('ref_axis',(-0.544789961245158,0.0337827349730038,-0.837891774004402));
#89530=DIRECTION('center_axis',(-0.101153799865448,-0.986495981532177,0.128816098348177));
#89531=DIRECTION('ref_axis',(-0.63231853649629,-0.0362134428581971,-0.773861651045939));
#89532=DIRECTION('center_axis',(0.0887457169003776,-0.986495109151898,-0.137664800698008));
#89533=DIRECTION('ref_axis',(-0.712175035857152,0.0337827361605426,-0.701188594487511));
#89534=DIRECTION('center_axis',(-0.0710972307886002,-0.986495981675317,
0.147549523593419));
#89535=DIRECTION('ref_axis',(-0.783892659372715,-0.0362134382290662,-0.61983940296919));
#89536=DIRECTION('center_axis',(0.0570770288023917,-0.986495109144716,-0.15352397994009));
#89537=DIRECTION('ref_axis',(-0.84625960139423,0.0337827355307125,-0.531698611835822));
#89538=DIRECTION('center_axis',(-0.037716230030684,-0.986495981658015,0.159383701064012));
#89539=DIRECTION('ref_axis',(-0.89881283339374,-0.0362134394467856,-0.436834153117806));
#89540=DIRECTION('center_axis',(0.0227394843068792,-0.98649510919204,-0.162204548005417));
#89541=DIRECTION('ref_axis',(-0.940774006315102,0.033782733441347,-0.337346996374748));
#89542=DIRECTION('center_axis',(-0.00257165909992377,-0.986495981600037,
0.163765273658531));
#89543=DIRECTION('ref_axis',(-0.971705519356601,-0.036213441281663,-0.233403021236782));
#89544=DIRECTION('center_axis',(-0.0126613353093978,-0.986495109225122,
-0.163300612561919));
#89545=DIRECTION('ref_axis',(-0.991298865155135,0.0337827334408555,-0.127221408824948));
#89546=DIRECTION('center_axis',(0.0326931560685295,-0.986495981648445,0.160489363316543));
#89547=DIRECTION('ref_axis',(-0.999162334596164,-0.0362134394397524,-0.0190582246887204));
#89548=DIRECTION('center_axis',(-0.0474701296012096,-0.986495109081729,
-0.156760921640161));
#89549=DIRECTION('ref_axis',(-0.99547169045246,0.0337827378314939,0.0888529129085293));
#89550=DIRECTION('center_axis',(0.0664292714792586,-0.986495981820537,0.149709150497458));
#89551=DIRECTION('ref_axis',(-0.979899429874397,-0.0362134335515134,0.196177711685712));
#89552=DIRECTION('center_axis',(-0.0800592635377692,-0.986495109206595,
-0.142891265769669));
#89553=DIRECTION('ref_axis',(-0.953097367008042,0.0337827328533723,0.300772565177237));
#89554=DIRECTION('center_axis',(0.0970592346613633,-0.986495982026382,0.131928702005114));
#89555=DIRECTION('ref_axis',(-0.914817516009326,-0.0362134347011463,0.402240599081785));
#89556=DIRECTION('center_axis',(-0.108904925617401,-0.986495109062015,-0.122340169090091));
#89557=DIRECTION('ref_axis',(-0.866157268702823,0.0337827385282152,0.498628431249964));
#89558=DIRECTION('center_axis',(0.123150817142994,-0.986495981721548,0.107979416021075));
#89559=DIRECTION('ref_axis',(-0.806959753962968,-0.0362134370030227,0.589495158983052));
#89560=DIRECTION('center_axis',(-0.132658304626744,-0.986495109226923,-0.0960685884403372));
#89561=DIRECTION('ref_axis',(-0.73871662136084,0.0337827326810044,0.673168983463906));
#89562=DIRECTION('center_axis',(0.14348400268928,-0.986495981690008,0.0789811311752993));
#89563=DIRECTION('ref_axis',(-0.661369448832978,-0.0362134378285858,0.749185583864905));
#89564=DIRECTION('center_axis',(-0.150208734751247,-0.986495109188334,-0.0653049427832723));
#89565=DIRECTION('ref_axis',(-0.576734403862306,0.0337827341053085,0.816232904432283));
#89566=DIRECTION('center_axis',(0.157108035070394,-0.98649598169556,0.0462897765692665));
#89567=DIRECTION('ref_axis',(-0.484854242613642,-0.0362134380174296,0.873844923499879));
#89568=DIRECTION('center_axis',(-0.160735569747072,-0.986495109243657,-0.03148771278498));
#89569=DIRECTION('ref_axis',(-0.387784725587891,0.0337827325626061,0.921130682140883));
#89570=DIRECTION('center_axis',(0.163385869707142,-0.986495981745934,0.0114339660295916));
#89571=DIRECTION('ref_axis',(-0.285667791249065,-0.036213435650009,0.957644245072931));
#89572=DIRECTION('center_axis',(-0.163746589113287,-0.986495109212928,0.00380184859480349));
#89573=DIRECTION('ref_axis',(-0.180702665110739,0.0337827324230032,0.982957412003141));
#89574=DIRECTION('center_axis',(0.162023961952625,-0.986495981990144,-0.0239564870228622));
#89575=DIRECTION('ref_axis',(-0.0731238305327095,-0.0362134362190338,0.996665185729608));
#89576=DIRECTION('center_axis',(0.16319774342888,0.986495109427954,0.0139246405501089));
#89577=DIRECTION('ref_axis',(-0.0798755533746233,-0.000856196801981241,
0.996804475762491));
#89578=DIRECTION('center_axis',(0.973816438935882,-0.151617915519108,0.169391708627898));
#89579=DIRECTION('ref_axis',(0.169168347992191,-0.0144665692539132,-0.985480993429916));
#89580=DIRECTION('center_axis',(-0.150208759619426,0.98649511125754,-0.0653048543262073));
#89581=DIRECTION('ref_axis',(-0.191922264154987,0.0357021715627206,0.980760520956737));
#89582=DIRECTION('center_axis',(0.156388881046733,0.986495109575236,0.0486817899126005));
#89583=DIRECTION('ref_axis',(-0.292291612279632,-0.000856205215915049,0.956328855730915));
#89584=DIRECTION('center_axis',(0.914635050695517,-0.151616585406996,0.374773444988745));
#89585=DIRECTION('ref_axis',(0.377062722092037,-0.0144669911495919,-0.926074732284399));
#89586=DIRECTION('center_axis',(-0.132658347021188,0.98649511115752,-0.0960685100744156));
#89587=DIRECTION('ref_axis',(-0.398269746671797,0.0357021763042036,0.916573272299125));
#89588=DIRECTION('center_axis',(0.142267445830776,0.986495109679402,0.0811626295496392));
#89589=DIRECTION('ref_axis',(-0.491040433772505,-0.000856212491145792,0.871136360910667));
#89590=DIRECTION('center_axis',(0.81268611159476,-0.151618552778232,0.562630516835359));
#89591=DIRECTION('ref_axis',(0.567325574073311,-0.0144672535242214,-0.823366498940693));
#89592=DIRECTION('center_axis',(-0.108904975984984,0.986495111019657,-0.122340108468259));
#89593=DIRECTION('ref_axis',(-0.585994582538218,0.0357021804983287,0.809528074586376));
#89594=DIRECTION('center_axis',(0.121493750910025,0.986495109592467,0.109848382964701));
#89595=DIRECTION('ref_axis',(-0.666828746114267,-0.000856205849967259,0.745210500642078));
#89596=DIRECTION('center_axis',(0.672736999254258,-0.151616243451158,0.724180533124259));
#89597=DIRECTION('ref_axis',(0.731061415364102,-0.0144684889231733,-0.682158243953788));
#89598=DIRECTION('center_axis',(-0.0800593355874687,0.98649511117952,-0.142891211780848));
#89599=DIRECTION('ref_axis',(-0.746318960904179,0.0357021749296351,0.664630245550261));
#89600=DIRECTION('center_axis',(0.0950391340827275,0.98649510969273,0.133397756896935));
#89601=DIRECTION('ref_axis',(-0.811436892359336,-0.000856211206739125,0.584439420830417));
#89602=DIRECTION('center_axis',(0.501331437055608,-0.151617256389218,0.851867946212772));
#89603=DIRECTION('ref_axis',(0.860613852619957,-0.0144631736525661,-0.509052662586622));
#89604=DIRECTION('center_axis',(-0.0474702053501761,0.986495111159743,-0.156760885625015));
#89605=DIRECTION('ref_axis',(-0.871746295781278,0.0357021754480533,0.48865504239688));
#89606=DIRECTION('center_axis',(0.0641406006060916,0.986495109654567,0.150709594855518));
#89607=DIRECTION('ref_axis',(-0.918103148144516,-0.000856207867161581,0.396340606392049));
#89608=DIRECTION('center_axis',(0.306484138460259,-0.151617050064071,0.939723226807841));
#89609=DIRECTION('ref_axis',(0.949924348094148,-0.0144650718554515,-0.312144989698896));
#89610=DIRECTION('center_axis',(-0.0126614270578941,0.986495111308531,-0.163300592862446));
#89611=DIRECTION('ref_axis',(-0.95641174064724,0.0357021704228837,0.28983087720119));
#89612=DIRECTION('center_axis',(0.0302429216759704,0.986495109620983,0.160974421515921));
#89613=DIRECTION('ref_axis',(-0.981839921055421,-0.000856207544026785,0.189709346977227));
#89614=DIRECTION('center_axis',(0.0973058256837251,-0.15161590629393,0.983638243078561));
#89615=DIRECTION('ref_axis',(0.994817503161179,-0.0144686949397451,-0.100641901168938));
#89616=DIRECTION('center_axis',(0.0227393955501278,0.986495111215857,-0.162204548139775));
#89617=DIRECTION('ref_axis',(-0.996356436764088,0.0357021755039037,0.077454538815092));
#89618=DIRECTION('center_axis',(-0.00506888908118924,0.986495109651181,
0.163712262820435));
#89619=DIRECTION('ref_axis',(-0.999666951145614,-0.000856213425135731,-0.0257925122042029));
#89620=DIRECTION('center_axis',(-0.11642200968098,-0.151617410714182,0.98155900303047));
#89621=DIRECTION('ref_axis',(0.993194280741403,-0.0144667153514315,0.115567447187813));
#89622=DIRECTION('center_axis',(0.05707694568674,0.986495111122913,-0.153523998129494));
#89623=DIRECTION('ref_axis',(-0.989712613066804,0.035702176775246,-0.138543488154395));
#89624=DIRECTION('center_axis',(-0.0401436782549925,0.986495109645519,0.158795099866574));
#89625=DIRECTION('ref_axis',(-0.970750665684117,-0.000856213207028468,-0.240088342017658));
#89626=DIRECTION('center_axis',(-0.324706330221997,-0.151617247467825,0.933583423901712));
#89627=DIRECTION('ref_axis',(0.945130314425094,-0.0144655603581925,0.326373155020824));
#89628=DIRECTION('center_axis',(0.0887456442119272,0.986495110966998,-0.13766483454979));
#89629=DIRECTION('ref_axis',(-0.936790926669358,0.0357021811528901,-0.348063376371161));
#89630=DIRECTION('center_axis',(-0.0733413910929646,0.986495109609041,0.146452856134646));
#89631=DIRECTION('ref_axis',(-0.896443158535087,-0.000856210127143939,-0.443157906868258));
#89632=DIRECTION('center_axis',(-0.517807853003868,-0.151616633390584,0.841954525996998));
#89633=DIRECTION('ref_axis',(0.852873205617176,-0.0144678116141435,0.52191759652974));
#89634=DIRECTION('center_axis',(0.11626469073227,0.986495110956794,-0.11536861682135));
#89635=DIRECTION('ref_axis',(-0.840065938070627,0.0357021814785561,-0.541308206044569));
#89636=DIRECTION('center_axis',(-0.103109741182452,0.986495109566161,0.12726264210418));
#89637=DIRECTION('ref_axis',(-0.780218965265864,-0.000856204815038207,-0.625505901772941));
#89638=DIRECTION('center_axis',(-0.686697081643996,-0.151616832959728,0.710956717406117));
#89639=DIRECTION('ref_axis',(0.720736642217765,-0.0144674666221049,0.69305799539014));
#89640=DIRECTION('center_axis',(0.138347322440688,0.986495111252765,-0.0876778982862104));
#89641=DIRECTION('ref_axis',(-0.704060402225739,0.0357021718200587,-0.709242063716656));
#89642=DIRECTION('center_axis',(-0.128056801010502,0.986495109612048,0.102121762746588));
#89643=DIRECTION('ref_axis',(-0.627512599215102,-0.000856208303257674,-0.778605936744415));
#89644=DIRECTION('center_axis',(-0.823477034226635,-0.151617428283846,0.546715400864012));
#89645=DIRECTION('ref_axis',(0.554899244324145,-0.0144667771566563,0.831791765411989));
#89646=DIRECTION('center_axis',(0.153960995333326,0.986495111267986,-0.0558874526198495));
#89647=DIRECTION('ref_axis',(-0.535133782798231,0.0357021721389029,-0.844012552876212));
#89648=DIRECTION('center_axis',(-0.147016065904781,0.986495109664312,0.0722057821388122));
#89649=DIRECTION('ref_axis',(-0.445464441648733,-0.000856212141019005,-0.895299222677732));
#89650=DIRECTION('center_axis',(-0.921752483970463,-0.151616266908719,0.356910165031687));
#89651=DIRECTION('ref_axis',(0.363115154710566,-0.014466659431284,0.931631955325933));
#89652=DIRECTION('center_axis',(0.162375622483093,0.986495111326117,-0.0214837741772698));
#89653=DIRECTION('ref_axis',(-0.341184903466239,0.0357021701338604,-0.939317952928861));
#89654=DIRECTION('center_axis',(-0.159101021164541,0.986495109713174,0.0389135397566582));
#89655=DIRECTION('ref_axis',(-0.24258685993834,-0.000856214665175483,-0.970129312144367));
#89656=DIRECTION('center_axis',(-0.976927465576519,-0.151616791789489,0.150416340367998));
#89657=DIRECTION('ref_axis',(0.154352777054545,-0.0144685980696197,0.987909854129135));
#89658=DIRECTION('center_axis',(0.163197748067908,0.986495111005709,0.0139244744028963));
#89659=DIRECTION('ref_axis',(-0.131282594828393,0.0357021809331137,-0.990701889859782));
#89660=DIRECTION('center_axis',(-0.163746588668221,0.986495109665289,0.0038017503851117));
#89661=DIRECTION('ref_axis',(-0.0283661934961215,-0.00085621129693069,-0.999597231873296));
#89662=DIRECTION('center_axis',(-0.986422439235276,-0.151617296518004,-0.0631107500327789));
#89663=DIRECTION('ref_axis',(0.061627591074778,0.0144662562400417,-0.997994372453431));
#89664=DIRECTION('center_axis',(0.156388925054473,0.986495110977037,0.0486816201323364));
#89665=DIRECTION('ref_axis',(0.0847583428158461,0.0357021810443611,-0.995761707233105));
#89666=DIRECTION('center_axis',(-0.160735548481539,0.986495109636285,-0.0314878090383231));
#89667=DIRECTION('ref_axis',(0.18718084923227,-0.000856211651976638,-0.982325097196592));
#89668=DIRECTION('center_axis',(-0.949793410970233,-0.15161801438972,-0.273686781175212));
#89669=DIRECTION('ref_axis',(0.274726623805539,0.0144617426827047,-0.961413615553155));
#89670=DIRECTION('center_axis',(0.142267532453734,0.986495111258958,0.081162458511939));
#89671=DIRECTION('ref_axis',(0.296836072343588,0.0357021720284353,-0.954260813964445));
#89672=DIRECTION('center_axis',(-0.150208694038284,0.98649510964934,-0.0653050294636678));
#89673=DIRECTION('ref_axis',(0.393975523838057,-0.000856207535000212,-0.919120532642583));
#89674=DIRECTION('center_axis',(-0.86875330672716,-0.151616186464143,-0.471466037008706));
#89675=DIRECTION('ref_axis',(0.474978502938863,0.0144685084660171,-0.879878448428375));
#89676=DIRECTION('center_axis',(0.121493865171389,0.986495111116108,0.1098482429069));
#89677=DIRECTION('ref_axis',(0.495034075137913,0.0357021764711176,-0.86813974626645));
#89678=DIRECTION('center_axis',(-0.132658243309647,0.986495109701154,-0.0960686682415635));
#89679=DIRECTION('ref_axis',(0.5823483421027,-0.000856213693593766,-0.812938912433368));
#89680=DIRECTION('center_axis',(-0.747091071425321,-0.15161663426736,-0.647199603839499));
#89681=DIRECTION('ref_axis',(0.653021700873013,0.0144674351368952,-0.75720099809065));
#89682=DIRECTION('center_axis',(0.0950392811829329,0.986495111174896,0.133397641134548));
#89683=DIRECTION('ref_axis',(0.67008483719993,0.0357021758568535,-0.741425428208279));
#89684=DIRECTION('center_axis',(-0.108904843685435,0.986495109715039,-0.122340236758661));
#89685=DIRECTION('ref_axis',(0.743491198027751,-0.000856213060135157,-0.668745172210204));
#89686=DIRECTION('center_axis',(-0.590495723145099,-0.15161685077541,-0.792670884736089));
#89687=DIRECTION('ref_axis',(0.800530337746882,0.0144663375264769,-0.599117604002281));
#89688=DIRECTION('center_axis',(0.064140767632109,0.986495111200935,0.150709513648669));
#89689=DIRECTION('ref_axis',(0.813803175955572,0.0357021742051885,-0.5800428825196));
#89690=DIRECTION('center_axis',(-0.080059177130819,0.986495109654734,-0.14289131108794));
#89691=DIRECTION('ref_axis',(0.869869229684662,-0.000856210562327918,-0.493281653978015));
#89692=DIRECTION('center_axis',(-0.406289357632402,-0.151615763752866,-0.901078031058512));
#89693=DIRECTION('ref_axis',(0.910606840740203,0.0144689391276382,-0.413020376492091));
#89694=DIRECTION('center_axis',(0.0302430998549555,0.986495111138554,0.160974378740519));
#89695=DIRECTION('ref_axis',(0.919468984642088,0.0357021757538406,-0.3915381730147));
#89696=DIRECTION('center_axis',(-0.0474700325199218,0.986495109610278,-0.156760947711994));
#89697=DIRECTION('ref_axis',(0.955573144978911,-0.0008562078867857,-0.294752831204668));
#89698=DIRECTION('center_axis',(-0.203085546924405,-0.151616938372349,-0.967351313964586));
#89699=DIRECTION('ref_axis',(0.978104545608466,0.0144676709904371,-0.20761065569033));
#89700=DIRECTION('center_axis',(-0.00506870252952517,0.986495111106572,
0.1637122598265));
#89701=DIRECTION('ref_axis',(0.982141444060542,0.035702178222545,-0.184725575730159));
#89702=DIRECTION('center_axis',(-0.0126612356724127,0.986495109661314,-0.16330061765211));
#89703=DIRECTION('ref_axis',(0.996595521728744,-0.000856211888700642,-0.0824416943749574));
#89704=DIRECTION('center_axis',(0.00961444697794412,-0.151616752732667,
-0.988392595429625));
#89705=DIRECTION('ref_axis',(0.99986717095386,0.0144667495042641,0.00750690398936496));
#89706=DIRECTION('center_axis',(-0.0401434933614616,0.986495111113504,0.158795137488191));
#89707=DIRECTION('ref_axis',(0.998890061332806,0.0357021761084332,0.0307245828558428));
#89708=DIRECTION('center_axis',(0.0227395785448257,0.986495109616514,-0.162204532212591));
#89709=DIRECTION('ref_axis',(0.991018199734975,-0.000856207842489773,0.133724323524857));
#89710=DIRECTION('center_axis',(0.221864784232945,-0.151617150572385,-0.963217658252578));
#89711=DIRECTION('ref_axis',(0.974877146343857,0.0144698250946434,0.222272746188522));
#89712=DIRECTION('center_axis',(-0.0733412205126192,0.986495111186581,0.146452930932413));
#89713=DIRECTION('ref_axis',(0.968931689381041,0.0357021750131451,0.244738096773943));
#89714=DIRECTION('center_axis',(0.0570771171246619,0.986495109600125,-0.153523944177369));
#89715=DIRECTION('ref_axis',(0.939101967721057,-0.000856204949422194,0.343637543256733));
#89716=DIRECTION('center_axis',(0.423741222458399,-0.15161624686651,-0.893003857816737));
#89717=DIRECTION('ref_axis',(0.904302870344119,0.0144688320150039,0.426646190171093));
#89718=DIRECTION('center_axis',(-0.103109596719155,0.986495111163184,0.127262746770411));
#89719=DIRECTION('ref_axis',(0.893667149003531,0.0357021778745687,0.447307926698055));
#89720=DIRECTION('center_axis',(0.0887457984091327,0.986495109631058,-0.137664744719671));
#89721=DIRECTION('ref_axis',(0.843274370259044,-0.000856207903572526,0.537482654019867));
#89722=DIRECTION('center_axis',(0.605803742148127,-0.151616591887001,-0.781034080603335));
#89723=DIRECTION('ref_axis',(0.791444387993897,0.014467573311151,0.611069938743063));
#89724=DIRECTION('center_axis',(-0.12805668263688,0.986495111047565,0.102121897315367));
#89725=DIRECTION('ref_axis',(0.776615725781708,0.0357021808280826,0.628962136183625));
#89726=DIRECTION('center_axis',(0.116264825596677,0.986495109676501,-0.115368491856844));
#89727=DIRECTION('ref_axis',(0.70801620387057,-0.000856214333401109,0.706195668319852));
#89728=DIRECTION('center_axis',(0.759539707374844,-0.151616246287053,-0.632544027544929));
#89729=DIRECTION('ref_axis',(0.641578860804063,0.0144678318516811,0.766920626408543));
#89730=DIRECTION('center_axis',(-0.147015974594736,0.986495111199057,0.0722059470841616));
#89731=DIRECTION('ref_axis',(0.623250614101209,0.0357021752331852,0.781206775896167));
#89732=DIRECTION('center_axis',(0.138347432562809,0.986495109665889,-0.0876777423783469));
#89733=DIRECTION('ref_axis',(0.539651981929142,-0.000856210824512759,0.841887762889432));
#89734=DIRECTION('center_axis',(0.877760395337333,-0.151616069138643,-0.454476903655395));
#89735=DIRECTION('ref_axis',(0.461713547141786,0.0144657771560889,0.88691112388842));
#89736=DIRECTION('center_axis',(-0.159100969104174,0.986495111013716,0.0389137196390765));
#89737=DIRECTION('ref_axis',(0.440742995292145,0.0357021793475845,0.89692305494437));
#89738=DIRECTION('center_axis',(0.153961068617493,0.986495109630638,-0.0558872796349529));
#89739=DIRECTION('ref_axis',(0.346054238115806,-0.000856208532924168,0.938214117986421));
#89740=DIRECTION('center_axis',(0.954937805615096,-0.151616804017654,-0.255159033048994));
#89741=DIRECTION('ref_axis',(0.260259650356053,0.0144675620557106,0.965430268867052));
#89742=DIRECTION('center_axis',(-0.163746575713377,0.986495111104787,0.00380193483594564));
#89743=DIRECTION('ref_axis',(0.237626725609359,0.0357021776226121,0.970700207988634));
#89744=DIRECTION('center_axis',(0.162375657399043,0.986495109627207,-0.0214835882904524));
#89745=DIRECTION('ref_axis',(0.136275379499101,-0.000856207475975685,0.990670625309509));
#89746=DIRECTION('center_axis',(0.987463458080041,-0.151617315741383,-0.0439102325658274));
#89747=DIRECTION('ref_axis',(-0.0466361827048427,-0.0144684783683654,-0.998807153356655));
#89748=DIRECTION('center_axis',(-0.160735575477852,0.986495110602581,-0.0314876409564998));
#89749=DIRECTION('ref_axis',(0.0233992914794688,0.0357021926497558,0.999088497881073));
#89750=DIRECTION('center_axis',(0.155084985271922,0.987363722734215,-0.0325810738257533));
#89751=DIRECTION('ref_axis',(0.107082710721225,0.0159846151395328,0.994121614865825));
#89752=DIRECTION('',(-0.603474775605395,0.,0.797382088592425));
#89753=DIRECTION('center_axis',(-0.146198072099652,0.987366228112447,0.0611069169353534));
#89754=DIRECTION('ref_axis',(0.247230525195829,-0.0233430562761571,0.968675471525465));
#89755=DIRECTION('',(-0.797382090536838,0.,-0.603474773036207));
#89756=DIRECTION('center_axis',(1.80679789905059E-15,-1.,7.19968963237278E-15));
#89757=DIRECTION('ref_axis',(1.06096449896609E-33,-7.19968963237278E-15,
-1.));
#89758=DIRECTION('center_axis',(-0.152615518807593,-0.987363722561521,0.042677661469956));
#89759=DIRECTION('ref_axis',(0.172020652255709,0.0159849136234662,0.984963642848796));
#89760=DIRECTION('center_axis',(0.157698499589188,-0.987363722825346,-0.0156224862231631));
#89761=DIRECTION('ref_axis',(0.239264796343388,0.0228559962932019,0.970685304650381));
#89762=DIRECTION('center_axis',(0.144455217640186,0.987363722794169,-0.0651580310212521));
#89763=DIRECTION('ref_axis',(0.318285939670239,0.0159846116596834,0.947859985862006));
#89764=DIRECTION('',(-0.417952293183597,0.,0.908468976147547));
#89765=DIRECTION('center_axis',(-0.129643867607601,0.987366228493109,0.0911065223956936));
#89766=DIRECTION('ref_axis',(0.449687003600112,-0.0233430424028127,0.892881123758663));
#89767=DIRECTION('',(-0.908468978721806,0.,-0.41795228758814));
#89768=DIRECTION('center_axis',(-3.31227642057055E-15,-1.,-6.64295675440539E-15));
#89769=DIRECTION('ref_axis',(-2.25783646485001E-32,6.64295675440539E-15,
-1.));
#89770=DIRECTION('center_axis',(-0.139873017737398,-0.987363722559547,0.074487705578756));
#89771=DIRECTION('ref_axis',(0.379736972377725,0.0159849124034919,0.924956385125727));
#89772=DIRECTION('center_axis',(0.150653221823371,-0.987363722937459,-0.0491577601332619));
#89773=DIRECTION('ref_axis',(0.442339566449922,0.0228559928591386,0.896556362725355));
#89774=DIRECTION('center_axis',(0.127070885021152,0.987363722838332,-0.0946882727837558));
#89775=DIRECTION('ref_axis',(0.514606469984781,0.0159846100172811,0.857277477420466));
#89776=DIRECTION('',(-0.212886825056998,0.,0.977076864794757));
#89777=DIRECTION('center_axis',(-0.107027651167834,0.987366228258172,0.116846108966996));
#89778=DIRECTION('ref_axis',(0.631116620567509,-0.0233430513871423,0.775336645074502));
#89779=DIRECTION('',(-0.977076865850031,0.,-0.212886820213656));
#89780=DIRECTION('center_axis',(-4.66287657085733E-15,-1.,-5.77560659059213E-15));
#89781=DIRECTION('ref_axis',(-3.17308563966652E-32,5.77560659059213E-15,
-1.));
#89782=DIRECTION('center_axis',(-0.120590206990325,-0.987363722543746,0.102814791652694));
#89783=DIRECTION('ref_axis',(0.569697214377223,0.0159849163266524,0.821699194584528));
#89784=DIRECTION('center_axis',(0.136563569902727,-0.987363722841019,-0.0803944661836044));
#89785=DIRECTION('ref_axis',(0.624731028720287,0.0228559958350036,0.780505442138928));
#89786=DIRECTION('center_axis',(0.103744859203304,0.987363722854479,-0.119790997073363));
#89787=DIRECTION('ref_axis',(0.686864572632723,0.0159846093646422,0.726609627740733));
#89788=DIRECTION('',(0.00213299544959006,0.,0.999997725162619));
#89789=DIRECTION('center_axis',(-0.0794069421389742,0.987366228166386,0.137122095289646));
#89790=DIRECTION('ref_axis',(0.783035924871884,-0.0233430546583344,0.621538286961673));
#89791=DIRECTION('',(-0.999997725152042,0.,0.00213300040793875));
#89792=DIRECTION('center_axis',(0.,-1.,0.));
#89793=DIRECTION('ref_axis',(0.,0.,-1.));
#89794=DIRECTION('center_axis',(-0.0956687346801696,-0.987363722549481,
0.126334368237338));
#89795=DIRECTION('ref_axis',(0.733019047310366,0.0159849154507234,0.680020263490902));
#89796=DIRECTION('center_axis',(0.116088355865392,-0.987363722833826,-0.107872018912213));
#89797=DIRECTION('ref_axis',(0.777910762482154,0.0228559958636816,0.627958954922623));
#89798=DIRECTION('center_axis',(0.0755678354376402,0.987363722748056,-0.139292430693023));
#89799=DIRECTION('ref_axis',(0.827005651956269,0.0159846135455113,0.561966319063863));
#89800=DIRECTION('',(0.217053076899228,0.,0.976159803417749));
#89801=DIRECTION('center_axis',(-0.0480732588543953,0.987366228278341,0.15098640017737));
#89802=DIRECTION('ref_axis',(0.898341339026026,-0.0233430501545939,0.438677490425948));
#89803=DIRECTION('',(-0.976159801597278,-3.11688536720188E-15,0.217053085086487));
#89804=DIRECTION('center_axis',(-2.66281056931374E-14,-1.,-1.31356300836969E-14));
#89805=DIRECTION('ref_axis',(1.,-2.66281056931374E-14,-1.31798834488888E-33));
#89806=DIRECTION('center_axis',(-0.0662738964320985,-0.987363722501457,
0.143946692007056));
#89807=DIRECTION('ref_axis',(0.862065724724343,0.0159849174326958,0.506544340280457));
#89808=DIRECTION('center_axis',(0.0901849798542257,-0.987363722846656,-0.130305595486476));
#89809=DIRECTION('ref_axis',(0.894716254152115,0.0228559966907545,0.44604980436189));
#89810=DIRECTION('center_axis',(0.0438573488328245,0.98736372284281,-0.152280700574112));
#89811=DIRECTION('ref_axis',(0.928476866871779,0.0159846104613722,0.371046088663339));
#89812=DIRECTION('',(0.421824000481475,0.,0.906677733606492));
#89813=DIRECTION('center_axis',(-0.0144917194007374,0.987366228279528,0.157790751699423));
#89814=DIRECTION('ref_axis',(0.971641310970371,-0.0233430506088162,0.2353046212977));
#89815=DIRECTION('',(-0.90667773151446,0.,0.421824004978135));
#89816=DIRECTION('center_axis',(-1.44146637799513E-14,-1.,-3.55213537512284E-15));
#89817=DIRECTION('ref_axis',(1.,-1.44146637799513E-14,4.42351985979486E-32));
#89818=DIRECTION('center_axis',(-0.0337801645495731,-0.987363722504886,
0.154828227285267));
#89819=DIRECTION('ref_axis',(0.950803166929402,0.0159849187336526,0.309382966774351));
#89820=DIRECTION('center_axis',(0.0600646558957432,-0.987363722771998,-0.146646227588527));
#89821=DIRECTION('ref_axis',(0.96968580795722,0.0228559986227534,0.243283861308783));
#89822=DIRECTION('center_axis',(0.0100961397987127,0.987363722827371,-0.158148496058732));
#89823=DIRECTION('ref_axis',(0.986533534493181,0.015984610039757,0.162776157843428));
#89824=DIRECTION('',(0.606870901804627,0.,0.794800420572888));
#89825=DIRECTION('',(-0.794800418951332,0.,0.606870903928329));
#89826=DIRECTION('',(0.763541191686738,0.,0.645759125833771));
#89827=DIRECTION('center_axis',(0.0531022914963808,0.987366228202565,0.14929192222915));
#89828=DIRECTION('ref_axis',(0.980639616445277,-0.0233430534609367,-0.194424907131723));
#89829=DIRECTION('',(-0.645759120372939,0.,0.763541196305195));
#89830=DIRECTION('center_axis',(2.91477949412441E-14,-1.,-5.65745894309366E-15));
#89831=DIRECTION('ref_axis',(1.,2.91477949412441E-14,2.51222001147484E-32));
#89832=DIRECTION('center_axis',(0.0343526394915633,-0.987363722496745,0.154702216071179));
#89833=DIRECTION('ref_axis',(0.99283211913855,0.0159849199594086,-0.118443512024708));
#89834=DIRECTION('center_axis',(-0.00706194962898739,-0.987363722828293,
-0.158313005498892));
#89835=DIRECTION('ref_axis',(0.982215246104916,0.0228559963878828,-0.186362050182373));
#89836=DIRECTION('center_axis',(-0.0572418275962692,0.987363722673098,-0.147770945461416));
#89837=DIRECTION('ref_axis',(0.963701520646536,0.0159846159200898,-0.266503041553829));
#89838=DIRECTION('',(0.884509147436183,0.,0.466522848424079));
#89839=DIRECTION('center_axis',(0.0839541446999537,0.987366228048496,0.134386135062308));
#89840=DIRECTION('ref_axis',(0.915917198838005,-0.0233430588070783,-0.400687891604266));
#89841=DIRECTION('',(-0.466522844039702,0.,0.884509149748666));
#89842=DIRECTION('center_axis',(-1.36250746154898E-14,-1.,5.8955524984798E-15));
#89843=DIRECTION('ref_axis',(1.,-1.36250746154898E-14,4.41891060473253E-32));
#89844=DIRECTION('center_axis',(0.0668058915450112,-0.987363722561284,0.1437005644554));
#89845=DIRECTION('ref_axis',(0.944158402242533,0.0159849137173079,-0.329103925847561));
#89846=DIRECTION('center_axis',(-0.0409294619246427,-0.987363722825878,
-0.153093624929265));
#89847=DIRECTION('ref_axis',(0.91918926717849,0.0228559962494711,-0.393152253636317));
#89848=DIRECTION('center_axis',(-0.087669925550576,0.987363722823561,-0.132010844274079));
#89849=DIRECTION('ref_axis',(0.883880438918321,0.0159846103812733,-0.467439688011742));
#89850=DIRECTION('',(0.964118437085268,0.,0.265472483079246));
#89851=DIRECTION('center_axis',(0.110880384200007,0.987366228253681,0.113196606414501));
#89852=DIRECTION('ref_axis',(0.808367512052446,-0.0233430518259719,-0.588215153995193));
#89853=DIRECTION('',(-0.265472477562517,0.,0.964118438604313));
#89854=DIRECTION('center_axis',(2.40783168675084E-14,-1.,-1.73734121004002E-14));
#89855=DIRECTION('ref_axis',(1.,2.40783168675084E-14,-9.42922941613875E-32));
#89856=DIRECTION('center_axis',(0.0961353783624827,-0.987363722591995,0.125979634609644));
#89857=DIRECTION('ref_axis',(0.851336887325996,0.0159849109908428,-0.524375806934968));
#89858=DIRECTION('center_axis',(-0.0728831555135252,-0.987363722760217,
-0.140715758248592));
#89859=DIRECTION('ref_axis',(0.813183020583973,0.022855998889668,-0.581559092740093));
#89860=DIRECTION('center_axis',(-0.113998684177927,0.987363722714032,-0.11007805900355));
#89861=DIRECTION('ref_axis',(0.762730088964751,0.0159846145330615,-0.646519375955627));
#89862=DIRECTION('',(0.998646620316722,0.,0.0520089197156425));
#89863=DIRECTION('center_axis',(0.132621977585668,0.987366228627553,0.0867141374117852));
#89864=DIRECTION('ref_axis',(0.663019460029588,-0.0233430386172312,-0.748238129321266));
#89865=DIRECTION('',(-0.0520089118984696,0.,0.998646620723836));
#89866=DIRECTION('center_axis',(2.47257614362469E-14,-1.,-2.76791971940485E-14));
#89867=DIRECTION('ref_axis',(-2.56103310374099E-31,2.76791971940485E-14,
-1.));
#89868=DIRECTION('center_axis',(0.120969685022707,-0.987363722555055,0.102368035478518));
#89869=DIRECTION('ref_axis',(0.718707806582739,0.015984912252531,-0.695128456716675));
#89870=DIRECTION('center_axis',(-0.101428918117671,-0.987363722837366,-0.12175817588243));
#89871=DIRECTION('ref_axis',(0.669153238850915,0.0228559961940831,-0.742772876708154));
#89872=DIRECTION('center_axis',(-0.134996984321599,0.98736372281309,-0.0829981511646479));
#89873=DIRECTION('ref_axis',(0.605915329882612,0.0159846104207681,-0.795368534229851));
#89874=DIRECTION('',(0.986479197453235,0.,-0.163886524742036));
#89875=DIRECTION('center_axis',(0.148162328874504,0.987366228449234,0.0561769990335785));
#89876=DIRECTION('ref_axis',(0.486669352553433,-0.0233430445479536,-0.873274323197731));
#89877=DIRECTION('',(0.163886529632327,0.,0.986479196640797));
#89878=DIRECTION('center_axis',(3.63949553544791E-15,-1.,-6.46947615618595E-15));
#89879=DIRECTION('ref_axis',(2.4838904804171E-32,6.46947615618595E-15,-1.));
#89880=DIRECTION('center_axis',(0.140147584032476,-0.987363722542777,0.0739698188204495));
#89881=DIRECTION('ref_axis',(0.552472745197975,0.0159849147106998,-0.833377674476047));
#89882=DIRECTION('center_axis',(-0.125231975789276,-0.987363722872431,-0.0971073168994375));
#89883=DIRECTION('ref_axis',(0.493834594623234,0.0228559948635626,-0.869255426587665));
#89884=DIRECTION('center_axis',(-0.149682979297111,0.987363722804785,-0.0520373384966535));
#89885=DIRECTION('ref_axis',(0.420768643212658,0.0159846115427924,-0.907027144622918));
#89886=DIRECTION('',(0.928185103589142,0.,-0.372118816341251));
#89887=DIRECTION('center_axis',(0.15677476827983,0.987366228614418,0.0230130967613378));
#89888=DIRECTION('ref_axis',(0.287563128866355,-0.0233430385249353,-0.957477179607439));
#89889=DIRECTION('',(0.372118820942155,0.,0.928185101744593));
#89890=DIRECTION('center_axis',(-1.73092801110785E-14,-1.,5.68048588195008E-14));
#89891=DIRECTION('ref_axis',(1.26963893944953E-31,-5.68048588195008E-14,
-1.));
#89892=DIRECTION('center_axis',(0.152772335842607,-0.987363722537882,0.04211285809975));
#89893=DIRECTION('ref_axis',(0.360404675471254,0.0159849146053789,-0.932659076192109));
#89894=DIRECTION('center_axis',(-0.143179323934672,-0.987363722859305,-0.0679158301062707));
#89895=DIRECTION('ref_axis',(0.29542479569763,0.0228559960548419,-0.955092557573011));
#89896=DIRECTION('center_axis',(-0.157369964369956,0.987363722781334,-0.018643316485656));
#89897=DIRECTION('ref_axis',(0.215947280176704,0.0159846133760726,-0.976274174768288));
#89898=DIRECTION('',(0.826490105990571,0.,-0.562951245402029));
#89899=DIRECTION('center_axis',(0.158056597898232,0.987366228339418,-0.0112268871744602));
#89900=DIRECTION('ref_axis',(0.0750107703523085,-0.0233430480212223,-0.996909467524626));
#89901=DIRECTION('',(0.562951250126444,0.,0.826490102772607));
#89902=DIRECTION('center_axis',(-5.866541577634E-16,-1.,7.39972205357027E-15));
#89903=DIRECTION('ref_axis',(1.03531391909646E-33,-7.39972205357027E-15,
-1.));
#89904=DIRECTION('center_axis',(0.158253623048332,-0.987363722546709,0.00828674790145633));
#89905=DIRECTION('ref_axis',(0.1514844822469,0.0159849132724407,-0.988330377043052));
#89906=DIRECTION('center_axis',(-0.154431767114578,-0.987363722967648,-0.0355486690796414));
#89907=DIRECTION('ref_axis',(0.0832012598696812,0.0228559917419084,-0.996270622871914));
#89908=DIRECTION('center_axis',(-0.157698504332179,0.987363722731131,0.0156224443002877));
#89909=DIRECTION('ref_axis',(0.0010284646078306,0.0159846134183868,-0.999871708967913));
#89910=DIRECTION('',(0.686149350632658,0.,-0.727460699025302));
#89911=DIRECTION('center_axis',(0.151947872945319,0.987366228211681,-0.0449419102223341));
#89912=DIRECTION('ref_axis',(-0.141049007625289,-0.0233430530033732,-0.98972737626298));
#89913=DIRECTION('',(0.727460703861421,0.,0.686149345505369));
#89914=DIRECTION('center_axis',(-4.07113198674605E-15,-1.,-2.94113358440815E-14));
#89915=DIRECTION('ref_axis',(3.16446087767206E-32,2.94113358440815E-14,
-1.));
#89916=DIRECTION('center_axis',(0.156335146712011,-0.987363722543461,-0.0259268453085564));
#89917=DIRECTION('ref_axis',(-0.0645189579561007,0.0159849158098743,-0.997788447783803));
#89918=DIRECTION('center_axis',(-0.158463151597848,-0.987363722911652,-0.00151929711410159));
#89919=DIRECTION('ref_axis',(-0.132912675267693,0.0228559931629575,-0.990864180566499));
#89920=DIRECTION('center_axis',(-0.150653237015209,0.98736372274595,0.0491577174215569));
#89921=DIRECTION('ref_axis',(-0.213938443152542,0.0159846135185208,-0.976716353232672));
#89922=DIRECTION('',(0.513725012558988,0.,-0.857954900604495));
#89923=DIRECTION('center_axis',(0.13873423522595,0.987366228330945,-0.0765554905137078));
#89924=DIRECTION('ref_axis',(-0.350513489393465,-0.0233430488791305,-0.936266733266885));
#89925=DIRECTION('',(0.85795490315098,0.,0.513725008306187));
#89926=DIRECTION('center_axis',(-2.57462974808217E-15,-1.,-6.96213552645962E-15));
#89927=DIRECTION('ref_axis',(-1.45992716183616E-32,6.96213552645962E-15,
-1.));
#89928=DIRECTION('center_axis',(0.147106613134323,-0.987363722546931,-0.0589281237646008));
#89929=DIRECTION('ref_axis',(-0.277505562222682,0.0159849140967657,-0.960591039650481));
#89930=DIRECTION('center_axis',(-0.155084976578354,-0.987363722815579,0.0325811127411562));
#89931=DIRECTION('ref_axis',(-0.342811757964815,0.0228559970767686,-0.939126030945101));
#89932=DIRECTION('center_axis',(-0.136563593350173,0.987363722837714,0.0803944263947326));
#89933=DIRECTION('ref_axis',(-0.418901823414549,0.0159846099984002,-0.907890827458437));
#89934=DIRECTION('',(0.317279463900984,0.,-0.948332084128078));
#89935=DIRECTION('center_axis',(0.119033538070446,0.987366228337816,-0.104589425624143));
#89936=DIRECTION('ref_axis',(-0.543588350657022,-0.0233430493212615,-0.839027298172332));
#89937=DIRECTION('',(0.94833208570079,0.,0.317279459200228));
#89938=DIRECTION('center_axis',(-2.00554483640518E-14,-1.,-3.12294768742199E-14));
#89939=DIRECTION('ref_axis',(8.93331168178509E-32,3.12294768742199E-14,
-1.));
#89940=DIRECTION('center_axis',(0.130999534218378,-0.987363722518234,-0.0891739955901007));
#89941=DIRECTION('ref_axis',(-0.477516315597614,0.0159849202558936,-0.878477461670186));
#89942=DIRECTION('center_axis',(-0.144455198836582,-0.987363722863686,0.065158071655359));
#89943=DIRECTION('ref_axis',(-0.53668134664747,0.0228559953510044,-0.843475391245751));
#89944=DIRECTION('center_axis',(-0.116088384632717,0.9873637227041,0.107871989141148));
#89945=DIRECTION('ref_axis',(-0.604277824084843,0.0159846144351275,-0.796613333694992));
#89946=DIRECTION('',(0.105998282549184,0.,-0.994366312832763));
#89947=DIRECTION('center_axis',(0.0937668866521125,0.987366224079759,-0.127732965651197));
#89948=DIRECTION('ref_axis',(-0.711245635399542,-0.0233431675720497,-0.702555864435566));
#89949=DIRECTION('',(0.994366313661193,0.,0.105998274777704));
#89950=DIRECTION('center_axis',(-0.0901851111012612,0.987363726530036,0.130305476739748));
#89951=DIRECTION('ref_axis',(-0.761398490165991,0.0159844698817519,-0.648087058886034));
#89952=DIRECTION('',(-0.110239262352301,0.,-0.993905078483866));
#89953=DIRECTION('center_axis',(0.,-1.,0.));
#89954=DIRECTION('ref_axis',(0.,0.,-1.));
#89955=DIRECTION('center_axis',(0.108767068287796,-0.987363722515168,-0.115250181418807));
#89956=DIRECTION('ref_axis',(-0.655198934415205,0.0159849158473419,-0.755287255821606));
#89957=DIRECTION('center_axis',(-0.127070814589076,-0.987363725701319,0.0946883374491268));
#89958=DIRECTION('ref_axis',(-0.705456317279217,0.0228559462351422,-0.708384775480488));
#89959=DIRECTION('',(0.993905077902487,0.,-0.110239267593957));
#89960=DIRECTION('center_axis',(0.0641159492092076,0.987366228179104,-0.144903680106382));
#89961=DIRECTION('ref_axis',(-0.845645844217114,-0.0233430542732531,-0.533233727342448));
#89962=DIRECTION('center_axis',(-1.87888493708443E-14,-1.,-1.19532248295311E-14));
#89963=DIRECTION('ref_axis',(1.,-1.87888493708443E-14,4.76728741383965E-32));
#89964=DIRECTION('center_axis',(-0.0600646941590119,0.98736372279682,0.146646211749191));
#89965=DIRECTION('ref_axis',(-0.882916956320006,0.0159846117320783,-0.469257008930492));
#89966=DIRECTION('center_axis',(0.0814487732550144,-0.987363722548193,-0.135937400045126));
#89967=DIRECTION('ref_axis',(-0.802245181914049,0.0159849145847606,-0.596780655351204));
#89968=DIRECTION('center_axis',(-0.103744825459418,-0.987363722817008,0.119791026606059));
#89969=DIRECTION('ref_axis',(-0.841244922299314,0.0228559975989328,-0.540170884146285));
#89970=DIRECTION('',(-0.321322141912006,0.,-0.946969947314634));
#89971=DIRECTION('center_axis',(0.0314669536807221,0.98736622841628,-0.155298943361071));
#89972=DIRECTION('ref_axis',(-0.940504603145758,-0.0233430461605324,-0.338978161033402));
#89973=DIRECTION('',(0.946969945721879,0.,-0.321322146606022));
#89974=DIRECTION('center_axis',(4.18383330129325E-14,-1.,1.52694357023645E-14));
#89975=DIRECTION('ref_axis',(1.,4.18383330129325E-14,-3.94743002442807E-32));
#89976=DIRECTION('center_axis',(0.0503220214576929,-0.987363722544967,-0.15026833851));
#89977=DIRECTION('ref_axis',(-0.911779336272946,0.0159849164455385,-0.410369253711697));
#89978=DIRECTION('center_axis',(-0.0755677933538741,-0.987363722995076,
0.139292451772985));
#89979=DIRECTION('ref_axis',(-0.937697856654406,0.0228559913020375,-0.346699197125309));
#89980=DIRECTION('center_axis',(-0.0271358127651529,0.987363722766446,0.156129839013432));
#89981=DIRECTION('ref_axis',(-0.963151234653621,0.0159846131294028,-0.268484992743187));
#89982=DIRECTION('',(-0.517380356258675,0.,-0.85575555327304));
#89983=DIRECTION('center_axis',(-0.00265341486369742,0.987366228230536,
-0.158432606301121));
#89984=DIRECTION('ref_axis',(-0.991386412655018,-0.0233430525964717,-0.128872350403382));
#89985=DIRECTION('',(0.855755550708218,0.,-0.517380360500933));
#89986=DIRECTION('center_axis',(-7.35710890037785E-15,-1.,-9.86406654151451E-16));
#89987=DIRECTION('ref_axis',(1.,-7.35710890037785E-15,-1.32634067597866E-32));
#89988=DIRECTION('center_axis',(0.0168422667212721,-0.987363722512522,-0.157572895886017));
#89989=DIRECTION('ref_axis',(-0.97867970097764,0.0159849196179625,-0.204769444105129));
#89990=DIRECTION('center_axis',(-0.0438573043102228,-0.987363722881878,
0.152280713143452));
#89991=DIRECTION('ref_axis',(-0.99030508060059,0.0228559947707262,-0.137016242977614));
#89992=DIRECTION('center_axis',(0.00706190712797093,0.987363722756913,0.15831300783993));
#89993=DIRECTION('ref_axis',(-0.998349631045912,0.0159846127507674,-0.055158919004085));
#89994=DIRECTION('',(-0.689246440251492,0.,-0.724526979898366));
#89995=DIRECTION('center_axis',(-0.0366497041828464,0.987366228300195,-0.154158134380116));
#89996=DIRECTION('ref_axis',(-0.995912095239017,-0.0233430501912213,0.0872593866836232));
#89997=DIRECTION('',(0.72452697791723,0.,-0.689246442334036));
#89998=DIRECTION('center_axis',(1.47943040872764E-14,-1.,-1.23643184723331E-15));
#89999=DIRECTION('ref_axis',(1.,1.47943040872764E-14,-1.07193378809406E-32));
#90000=DIRECTION('center_axis',(-0.0174250066718511,-0.987363722557856,
-0.157509518820862));
#90001=DIRECTION('ref_axis',(-0.999818091054278,0.0159849156030328,0.0104051561133797));
#90002=DIRECTION('center_axis',(-0.0100960932873028,-0.98736372289329,0.15814849861645));
#90003=DIRECTION('ref_axis',(-0.996606740262811,0.0228559949662293,0.0790734390098031));
#90004=DIRECTION('center_axis',(0.0409294185715571,0.987363722834022,0.153093636467149));
#90005=DIRECTION('ref_axis',(-0.986866308739757,0.015984610806164,0.160746324660136));
#90006=DIRECTION('',(-0.828884125374412,0.,-0.559420330969743));
#90007=DIRECTION('center_axis',(-0.0689322896726502,0.987366228486843,-0.142675401818788));
#90008=DIRECTION('ref_axis',(-0.953870035607405,-0.0233430431880731,0.299310971240695));
#90009=DIRECTION('',(0.559420330169213,0.,-0.828884125914696));
#90010=DIRECTION('center_axis',(2.1273937814866E-14,-1.,-6.58179424376849E-15));
#90011=DIRECTION('ref_axis',(1.,2.1273937814866E-14,-3.51258760307531E-32));
#90012=DIRECTION('center_axis',(-0.0508775060489346,-0.987363722578911,
-0.150081173747259));
#90013=DIRECTION('ref_axis',(-0.974206098104539,0.0159849106349481,0.22509322745903));
#90014=DIRECTION('center_axis',(0.0241371969397669,-0.987363722764837,0.156621437523263));
#90015=DIRECTION('ref_axis',(-0.956308175974158,0.02285599868685,0.291465737075571));
#90016=DIRECTION('center_axis',(0.0728831202615189,0.987363722755467,0.140715776540549));
#90017=DIRECTION('ref_axis',(-0.929238214197301,0.0159846130470007,0.36913525085143));
#90018=DIRECTION('',(-0.929764109056227,0.,-0.368155811458791));
#90019=DIRECTION('center_axis',(-0.0979916831930273,0.987366228552848,-0.124521326439782));
#90020=DIRECTION('ref_axis',(-0.867226073189164,-0.0233430412166463,0.497367108288898));
#90021=DIRECTION('',(0.368155805866007,0.,-0.929764111270784));
#90022=DIRECTION('center_axis',(-1.29077824990975E-14,-1.,7.33412221364675E-15));
#90023=DIRECTION('ref_axis',(1.,-1.29077824990975E-14,9.53777731518876E-32));
#90024=DIRECTION('center_axis',(-0.0819510393273368,-0.987363722536242,
-0.135635196658328));
#90025=DIRECTION('ref_axis',(-0.903041310616502,0.0159849165097872,0.429256186634747));
#90026=DIRECTION('center_axis',(0.0572418606350587,-0.987363722728211,0.147770932294974));
#90027=DIRECTION('ref_axis',(-0.87129370493947,0.0228560001693836,0.490229418730771));
#90028=DIRECTION('center_axis',(0.101428888140416,0.98736372270075,0.121758201962396));
#90029=DIRECTION('ref_axis',(-0.828159973897691,0.0159846158621332,0.5602638215069));
#90030=DIRECTION('',(-0.987169358123944,0.,-0.159676730869468));
#90031=DIRECTION('center_axis',(-0.122469100495229,0.987366228387713,-0.100544768453219));
#90032=DIRECTION('ref_axis',(-0.740031582688813,-0.0233430463661472,0.672166912908869));
#90033=DIRECTION('',(0.159676728323573,0.,-0.987169358535748));
#90034=DIRECTION('center_axis',(-2.20587724970193E-14,-1.,1.98748924161972E-14));
#90035=DIRECTION('ref_axis',(1.,-2.20587724970193E-14,-2.24130318029432E-32));
#90036=DIRECTION('center_axis',(-0.109192625785226,-0.987363722537315,-0.114847071757986));
#90037=DIRECTION('ref_axis',(-0.789651315668535,0.015984914242963,0.613347603060122));
#90038=DIRECTION('center_axis',(0.0876699622063691,-0.987363722805213,0.132010820067767));
#90039=DIRECTION('ref_axis',(-0.745538508437029,0.022855997249937,0.666070518659399));
#90040=DIRECTION('center_axis',(0.125231945564004,0.987363722864882,0.0971073559554355));
#90041=DIRECTION('ref_axis',(-0.688357894533299,0.0159846077203131,0.725195078133954));
#90042=DIRECTION('',(-0.998415664339409,0.,0.056268652033768));
#90043=DIRECTION('center_axis',(-0.14121998947165,0.987366228605458,-0.0718668573339754));
#90044=DIRECTION('ref_axis',(-0.578234039457966,-0.0233430387658572,0.815536938558457));
#90045=DIRECTION('',(-0.056268656982825,0.,-0.99841566406049));
#90046=DIRECTION('center_axis',(3.02234385184713E-14,-1.,-4.22663719263823E-14));
#90047=DIRECTION('ref_axis',(9.23861481743029E-32,4.22663719263823E-14,
-1.));
#90048=DIRECTION('center_axis',(-0.131328487682649,-0.987363722542341,-0.0886888252843569));
#90049=DIRECTION('ref_axis',(-0.639338102878694,0.0159849129887714,0.768759567591984));
#90050=DIRECTION('center_axis',(0.113998714502946,-0.987363722957852,0.110078025411463));
#90051=DIRECTION('ref_axis',(-0.584922758664488,0.022855991758488,0.810766902406025));
#90052=DIRECTION('center_axis',(0.143179307552888,0.987363722692716,0.0679158670640089));
#90053=DIRECTION('ref_axis',(-0.516368963541762,0.015984615356825,0.856217020131404));
#90054=DIRECTION('',(-0.962977163988183,0.,0.269582977276527));
#90055=DIRECTION('center_axis',(-0.153367597967407,0.987366228380772,-0.0398285192649395));
#90056=DIRECTION('ref_axis',(-0.389398912992463,-0.0233430469757092,0.920773364470421));
#90057=DIRECTION('',(-0.269582982049911,0.,-0.962977162651886));
#90058=DIRECTION('center_axis',(1.16747489638502E-14,-1.,-2.7300201939915E-14));
#90059=DIRECTION('ref_axis',(-8.42829456997971E-32,2.7300201939915E-14,
-1.));
#90060=DIRECTION('center_axis',(-0.147323577180954,-0.987363722544773,-0.0583835851000591));
#90061=DIRECTION('ref_axis',(-0.459130151320057,0.0159849151889484,0.888225189147));
#90062=DIRECTION('center_axis',(0.134997007515849,-0.98736372284086,0.0829981131086931));
#90063=DIRECTION('ref_axis',(-0.396956672600795,0.0228559966621038,0.917552725184927));
#90064=DIRECTION('center_axis',(0.154431756929921,0.987363722830919,0.0355487171218024));
#90065=DIRECTION('ref_axis',(-0.32023519511529,0.0159846109873066,0.947203205242179));
#90066=DIRECTION('',(-0.882510921618163,0.,0.470291902146594));
#90067=DIRECTION('center_axis',(-0.158343905549733,0.987366228052689,-0.00592783908880724));
#90068=DIRECTION('ref_axis',(-0.182355925401121,-0.0233430585632933,0.982955450713821));
#90069=DIRECTION('',(-0.47029190652181,0.,-0.882510919286601));
#90070=DIRECTION('center_axis',(6.91632924006171E-15,-1.,-3.64645803905207E-14));
#90071=DIRECTION('ref_axis',(-4.47855630928108E-32,3.64645803905207E-14,
-1.));
#90072=DIRECTION('center_axis',(-0.156429978770521,-0.987363722548624,-0.0253483951519218));
#90073=DIRECTION('ref_axis',(-0.257453783759328,0.0159849151389363,0.966158388524369));
#90074=DIRECTION('center_axis',(0.149682993082578,-0.987363722771226,0.0520372994801409));
#90075=DIRECTION('ref_axis',(-0.190429332313761,0.0228559990774562,0.981434803082052));
#90076=DIRECTION('center_axis',(0.158463151356584,0.987363722873948,0.00151934677967927));
#90077=DIRECTION('ref_axis',(-0.109127584832606,0.0159846093646868,0.993899221496858));
#90078=DIRECTION('',(-0.760779449282708,0.,0.649010500338092));
#90079=DIRECTION('center_axis',(-1.30101311407807E-15,-1.,-4.45186381807587E-14));
#90080=DIRECTION('ref_axis',(0.0292115385231254,-4.4537644533499E-14,0.999573251951608));
#90081=DIRECTION('center_axis',(-0.158221888563446,-0.987363722509994,0.00887206011162575));
#90082=DIRECTION('ref_axis',(-0.043739163848306,0.0159849177378449,0.998915095466459));
#90083=DIRECTION('center_axis',(0.15736996898241,-0.987363722822644,0.0186432753636452));
#90084=DIRECTION('ref_axis',(0.0250022698571692,0.0228559967621556,0.999426080265068));
#90085=DIRECTION('center_axis',(-0.155916223281314,0.987366228337048,0.0282499992418257));
#90086=DIRECTION('ref_axis',(0.0332138191420049,-0.0233430483582581,0.999175632364674));
#90087=DIRECTION('',(-0.649010505774152,0.,-0.760779444645279));
#90088=DIRECTION('',(0.562951245198508,0.,0.826490106129196));
#90089=DIRECTION('',(0.826490103338819,0.,-0.562951249295166));
#90090=DIRECTION('center_axis',(-1.42506245924468E-14,-1.,4.67670932993191E-14));
#90091=DIRECTION('ref_axis',(-3.31795861312863E-31,-4.67670932993191E-14,
-1.));
#90092=DIRECTION('',(0.37211881550646,0.,0.928185103923818));
#90093=DIRECTION('',(0.928185102079726,0.,-0.372118820106224));
#90094=DIRECTION('center_axis',(-1.19854977313491E-14,-1.,2.13051207289039E-14));
#90095=DIRECTION('ref_axis',(5.98310716154639E-31,-2.13051207289039E-14,
-1.));
#90096=DIRECTION('',(0.163886525562536,0.,0.986479197316923));
#90097=DIRECTION('',(0.986479196610463,0.,-0.163886529814916));
#90098=DIRECTION('center_axis',(-9.77115277883001E-14,-1.,1.09382946720462E-13));
#90099=DIRECTION('ref_axis',(2.26219721903079E-31,-1.09382946720462E-13,
-1.));
#90100=DIRECTION('',(-0.0520089175441786,0.,0.998646620429811));
#90101=DIRECTION('',(0.998646620676925,0.,0.0520089127992341));
#90102=DIRECTION('center_axis',(1.98235311947545E-14,-1.,-1.43034240564314E-14));
#90103=DIRECTION('ref_axis',(1.,1.98235311947545E-14,1.54468048409161E-31));
#90104=DIRECTION('',(-0.26547248098734,0.,0.964118437661279));
#90105=DIRECTION('',(0.964118438699595,0.,0.26547247721648));
#90106=DIRECTION('center_axis',(2.2434881337443E-14,-1.,-9.70754468690818E-15));
#90107=DIRECTION('ref_axis',(1.,2.2434881337443E-14,1.17354887193027E-31));
#90108=DIRECTION('',(-0.466522846721843,0.,0.884509148334006));
#90109=DIRECTION('',(0.884509150646384,0.,0.466522842337664));
#90110=DIRECTION('center_axis',(7.19916042948402E-14,-1.,-1.39732541140984E-14));
#90111=DIRECTION('ref_axis',(1.,7.19916042948402E-14,-3.12122083665017E-31));
#90112=DIRECTION('',(-0.645759126094484,0.,0.763541191466242));
#90113=DIRECTION('',(0.763541194667127,0.,0.645759122309779));
#90114=DIRECTION('center_axis',(-1.22187195728407E-13,-1.,-3.04916613055291E-15));
#90115=DIRECTION('ref_axis',(-0.999688772476419,1.22225235586043E-13,-0.0249471077399778));
#90116=DIRECTION('',(-0.794800422092897,0.,0.606870899813917));
#90117=DIRECTION('',(0.606870906241242,0.,0.794800417185304));
#90118=DIRECTION('center_axis',(7.12050275826231E-14,-1.,1.75467080845981E-14));
#90119=DIRECTION('ref_axis',(1.,7.12050275826231E-14,-3.78306478629417E-31));
#90120=DIRECTION('',(-0.90667773424271,0.,0.421823999113974));
#90121=DIRECTION('',(0.421824003608526,0.,0.906677732151658));
#90122=DIRECTION('center_axis',(2.19227566982768E-14,-1.,1.0814483979915E-14));
#90123=DIRECTION('ref_axis',(1.,2.19227566982768E-14,2.75543852127815E-31));
#90124=DIRECTION('',(-0.976159802699631,0.,0.21705308012884));
#90125=DIRECTION('',(0.217053081215155,0.,0.976159802458085));
#90126=DIRECTION('center_axis',(-5.7256261525697E-14,-1.,-4.58231761920508E-14));
#90127=DIRECTION('ref_axis',(1.,-5.7256261525697E-14,2.12756564536858E-30));
#90128=DIRECTION('',(-0.999997725164459,0.,0.00213299458671958));
#90129=DIRECTION('',(0.00213299954307815,0.,0.999997725153887));
#90130=DIRECTION('center_axis',(-1.07489698006143E-13,-1.,-1.33140605152815E-13));
#90131=DIRECTION('ref_axis',(2.95819333941865E-30,1.33140605152815E-13,
-1.));
#90132=DIRECTION('',(-0.977076864643459,0.,-0.212886825751402));
#90133=DIRECTION('',(-0.212886820908111,0.,0.977076865698722));
#90134=DIRECTION('center_axis',(3.27237231887067E-14,-1.,6.56292683412567E-14));
#90135=DIRECTION('ref_axis',(7.14654171068158E-31,-6.56292683412567E-14,
-1.));
#90136=DIRECTION('',(-0.908468975825409,0.,-0.417952293883803));
#90137=DIRECTION('',(-0.417952286130219,0.,0.90846897939254));
#90138=DIRECTION('center_axis',(1.19002053855136E-14,-1.,4.7419683964371E-14));
#90139=DIRECTION('ref_axis',(-4.27944612850522E-31,-4.7419683964371E-14,
-1.));
#90140=DIRECTION('',(-0.797382087238903,0.,-0.603474777393829));
#90141=DIRECTION('',(-0.603474773441189,0.,0.79738209023034));
#90142=DIRECTION('',(-0.649010502445557,0.,-0.760779447484858));
#90143=DIRECTION('',(-0.760779446212336,0.,0.649010503937226));
#90144=DIRECTION('center_axis',(3.18873609751326E-14,-1.,-1.68117970770856E-13));
#90145=DIRECTION('ref_axis',(-2.02423822237375E-31,1.68117970770856E-13,
-1.));
#90146=DIRECTION('',(-0.470291902230301,0.,-0.882510921573555));
#90147=DIRECTION('',(-0.882510919242011,0.,0.470291906605484));
#90148=DIRECTION('center_axis',(2.88352484393563E-14,-1.,-6.74282682904716E-14));
#90149=DIRECTION('ref_axis',(-1.18951982070183E-30,6.74282682904716E-14,
-1.));
#90150=DIRECTION('',(-0.269582977795074,0.,-0.962977163843017));
#90151=DIRECTION('',(-0.962977162506631,0.,0.269582982568776));
#90152=DIRECTION('center_axis',(4.26561810885819E-14,-1.,-5.96531070916475E-14));
#90153=DIRECTION('ref_axis',(9.5407336789931E-31,5.96531070916475E-14,-1.));
#90154=DIRECTION('',(-0.0562686524745445,0.,-0.998415664314567));
#90155=DIRECTION('',(-0.998415664035649,0.,0.0562686574235875));
#90156=DIRECTION('center_axis',(-1.81608525738086E-14,-1.,1.6362877447134E-14));
#90157=DIRECTION('ref_axis',(1.,-1.81608525738086E-14,1.48384009782733E-31));
#90158=DIRECTION('',(0.159676734244938,0.,-0.987169357577955));
#90159=DIRECTION('',(-0.98716935888988,0.,-0.15967672613422));
#90160=DIRECTION('center_axis',(4.25075937781184E-14,-1.,-2.41525519782833E-14));
#90161=DIRECTION('ref_axis',(1.,4.25075937781184E-14,8.40301947026E-31));
#90162=DIRECTION('',(0.368155812360744,0.,-0.929764108699083));
#90163=DIRECTION('',(-0.929764111872095,0.,-0.368155804347418));
#90164=DIRECTION('center_axis',(-1.6347056178951E-13,-1.,5.05750092776146E-14));
#90165=DIRECTION('ref_axis',(1.,-1.6347056178951E-13,-7.14902888199201E-31));
#90166=DIRECTION('',(0.559420334090901,0.,-0.828884123267918));
#90167=DIRECTION('',(-0.828884127273306,0.,-0.559420328156181));
#90168=DIRECTION('',(0.724526980936292,0.,-0.689246439160437));
#90169=DIRECTION('',(-0.689246444718413,0.,-0.724526975648959));
#90170=DIRECTION('center_axis',(0.,-1.,0.));
#90171=DIRECTION('ref_axis',(0.,0.,-1.));
#90172=DIRECTION('',(0.855755553808345,0.,-0.517380355373272));
#90173=DIRECTION('',(-0.517380359614475,0.,-0.85575555124416));
#90174=DIRECTION('center_axis',(-2.29634960358735E-14,-1.,-8.38082210911572E-15));
#90175=DIRECTION('ref_axis',(1.,-2.29634960358735E-14,4.3992465533463E-31));
#90176=DIRECTION('',(0.946969946451846,0.,-0.321322144454732));
#90177=DIRECTION('',(-0.32132214795012,0.,-0.946969945265805));
#90178=DIRECTION('center_axis',(-1.44374952654912E-13,-1.,-9.18494919385524E-14));
#90179=DIRECTION('ref_axis',(1.,-1.44374952654912E-13,8.12637320795991E-31));
#90180=DIRECTION('',(0.99390507839176,0.,-0.11023926318272));
#90181=DIRECTION('',(-0.110239267677687,0.,-0.9939050778932));
#90182=DIRECTION('center_axis',(-1.38576708982774E-13,-1.,-1.37986798379914E-13));
#90183=DIRECTION('ref_axis',(1.,-1.38576708982774E-13,-8.59017661330448E-31));
#90184=DIRECTION('',(0.994366313149823,0.,0.105998279574848));
#90185=DIRECTION('',(0.105998278540145,0.,-0.994366313260121));
#90186=DIRECTION('center_axis',(-2.6418444921436E-14,-1.,-4.11376599337965E-14));
#90187=DIRECTION('ref_axis',(-7.95516692322674E-31,4.11376599337965E-14,
-1.));
#90188=DIRECTION('',(0.948332083835448,0.,0.317279464775641));
#90189=DIRECTION('',(0.31727946007514,0.,-0.948332085408075));
#90190=DIRECTION('center_axis',(3.39148311317661E-14,-1.,9.17101384722506E-14));
#90191=DIRECTION('ref_axis',(7.13691189980589E-32,-9.17101384722506E-14,
-1.));
#90192=DIRECTION('',(0.857954900607374,0.,0.513725012554179));
#90193=DIRECTION('',(0.513725008301434,0.,-0.857954903153826));
#90194=DIRECTION('center_axis',(3.3517380830713E-15,-1.,2.421417305627E-14));
#90195=DIRECTION('ref_axis',(3.95306254274215E-32,-2.421417305627E-14,-1.));
#90196=DIRECTION('',(0.727460699689289,0.,0.686149349928695));
#90197=DIRECTION('center_axis',(7.72782051473817E-15,-1.,-9.74743349916755E-14));
#90198=DIRECTION('ref_axis',(-0.0790325797119564,-9.77801881363366E-14,
0.99687203358509));
#90199=DIRECTION('',(0.686149346322776,0.,-0.727460703090433));
#90200=DIRECTION('center_axis',(0.163197749987252,-0.986495109897446,0.0139245304238548));
#90201=DIRECTION('ref_axis',(0.0254674151392068,0.0183213284312142,0.999507748689645));
#90202=DIRECTION('center_axis',(-0.159101001719421,-0.98649511023429,0.0389136060486979));
#90203=DIRECTION('ref_axis',(0.139799307721241,0.016506827496646,0.990042260818526));
#90204=DIRECTION('center_axis',(0.162375647399524,-0.986495108859253,-0.0214836991311003));
#90205=DIRECTION('ref_axis',(0.239736643839447,0.0183213442783557,0.970665065789653));
#90206=DIRECTION('center_axis',(-0.147016033672384,-0.986495110214053,0.07220584025551));
#90207=DIRECTION('ref_axis',(0.349360698698762,0.0165068277187146,0.936842904036412));
#90208=DIRECTION('center_axis',(0.153961016969689,-0.986495110699525,-0.0558874030492672));
#90209=DIRECTION('ref_axis',(0.44279603111771,0.0183213213359592,0.896435164421225));
#90210=DIRECTION('center_axis',(-0.128056758497475,-0.986495110176503,0.10212181060365));
#90211=DIRECTION('ref_axis',(0.542586372947516,0.0165068288788752,0.839837813206825));
#90212=DIRECTION('center_axis',(0.138347353699881,-0.986495110711692,-0.08767785504999));
#90213=DIRECTION('ref_axis',(0.625150766853485,0.0183213200643359,0.780288951564483));
#90214=DIRECTION('center_axis',(-0.103109690306681,-0.986495110153458,0.127262678771813));
#90215=DIRECTION('ref_axis',(0.710441310111489,0.0165068311346094,0.703562839704432));
#90216=DIRECTION('center_axis',(0.116264744835321,-0.986495108930328,-0.115368579625991));
#90217=DIRECTION('ref_axis',(0.778274147036787,0.0183213421848879,0.627657295404671));
#90218=DIRECTION('center_axis',(-0.0733413333033863,-0.986495110181623,
0.14645288121792));
#90219=DIRECTION('ref_axis',(0.845076800566642,0.0165068261280715,0.53439005027716));
#90220=DIRECTION('center_axis',(0.0887456881072436,-0.98649511049776,-0.137664809615185));
#90221=DIRECTION('ref_axis',(0.895006296275743,0.0183213269098285,0.445677078844134));
#90222=DIRECTION('center_axis',(-0.0401436161497176,-0.986495110223755,
0.158795111974661));
#90223=DIRECTION('ref_axis',(0.940197438546159,0.0165068233288879,0.340229777260648));
#90224=DIRECTION('center_axis',(0.0570769958322964,-0.986495110611188,-0.153523982774612));
#90225=DIRECTION('ref_axis',(0.969888944115819,0.0183213240737779,0.242857499711427));
#90226=DIRECTION('center_axis',(-0.00506882451432805,-0.986495110238031,
0.163712261283321));
#90227=DIRECTION('ref_axis',(0.991355489517604,0.0165068248546079,0.13016073961272));
#90228=DIRECTION('center_axis',(0.0227394654220306,-0.986495108959915,-0.162204552064625));
#90229=DIRECTION('ref_axis',(0.999420662940406,0.018321340512334,0.0286821716331137));
#90230=DIRECTION('center_axis',(0.0302429834585616,-0.98649511018174,0.160974406472092));
#90231=DIRECTION('ref_axis',(0.996158860300694,0.0165068293684157,-0.0859944744075077));
#90232=DIRECTION('center_axis',(-0.0126613729172467,-0.986495110734072,
-0.163300600530499));
#90233=DIRECTION('ref_axis',(0.982220582776599,0.0183213198539688,-0.186834300942859));
#90234=DIRECTION('center_axis',(0.0641406633763457,-0.986495110174397,0.150709564738432));
#90235=DIRECTION('ref_axis',(0.954382949533046,0.0165068348330388,-0.298128680345246));
#90236=DIRECTION('center_axis',(-0.0474701529819279,-0.986495110541529,
-0.156760905373532));
#90237=DIRECTION('ref_axis',(0.919092959171724,0.018321326784228,-0.39361461022913));
#90238=DIRECTION('center_axis',(0.0950391876824385,-0.986495110247086,0.1333977146103));
#90239=DIRECTION('ref_axis',(0.867981153072863,0.0165068300635194,-0.496322720083975));
#90240=DIRECTION('center_axis',(-0.0800592794799243,-0.986495108881716,
-0.14289125908049));
#90241=DIRECTION('ref_axis',(0.812989570484355,0.0183213433664377,-0.581989936906914));
#90242=DIRECTION('center_axis',(0.121493790101314,-0.986495110177343,0.109848334366111));
#90243=DIRECTION('ref_axis',(0.740993521301427,0.0165068299297818,-0.671309262527325));
#90244=DIRECTION('center_axis',(-0.108904939865407,-0.986495110542266,-0.122340144470716));
#90245=DIRECTION('ref_axis',(0.668871694283925,0.0183213263347191,-0.743152060877913));
#90246=DIRECTION('center_axis',(0.142267476719983,-0.986495110210635,0.081162568947983));
#90247=DIRECTION('ref_axis',(0.579357859691649,0.016506829044998,-0.81490612650071));
#90248=DIRECTION('center_axis',(-0.132658318227354,-0.986495110593608,-0.0960685556256334));
#90249=DIRECTION('ref_axis',(0.493478119854653,0.0183213248467722,-0.869565221406983));
#90250=DIRECTION('center_axis',(0.156388896590567,-0.986495110143674,0.0486817284595133));
#90251=DIRECTION('ref_axis',(0.390632064234538,0.0165068316523958,-0.920398889015335));
#90252=DIRECTION('center_axis',(-0.150208740918382,-0.98649511067299,-0.0653049061709711));
#90253=DIRECTION('ref_axis',(0.295010055448863,0.0183213220749732,-0.955318479011834));
#90254=DIRECTION('center_axis',(0.163197743665263,-0.986495110172428,0.013924585037137));
#90255=DIRECTION('ref_axis',(0.183640749222092,0.0165068333459602,-0.98285482126204));
#90256=DIRECTION('center_axis',(-0.160735568247925,-0.986495110467,-0.0314876821109071));
#90257=DIRECTION('ref_axis',(0.0827476521059804,0.0183213293856647,-0.996402105056232));
#90258=DIRECTION('center_axis',(0.162375645555574,-0.986495110193824,-0.0214836517865426));
#90259=DIRECTION('ref_axis',(-0.0319374034875196,0.0165068301898106,-0.999353554461863));
#90260=DIRECTION('center_axis',(-0.163746580379318,-0.98649511053951,0.00380188055031853));
#90261=DIRECTION('ref_axis',(-0.133383942944882,0.0183213273159671,-0.990895076549408));
#90262=DIRECTION('center_axis',(0.153961042610572,-0.986495110180794,-0.0558873415689909));
#90263=DIRECTION('ref_axis',(-0.24602219607511,0.0165068322773698,-0.969123626544388));
#90264=DIRECTION('center_axis',(-0.159100984330676,-0.986495110516032,0.0389136700013237));
#90265=DIRECTION('ref_axis',(-0.343278649941192,0.0183213262598227,-0.939054895891946));
#90266=DIRECTION('center_axis',(0.138347393324552,-0.986495110212549,-0.0876777981420205));
#90267=DIRECTION('ref_axis',(-0.448603267737991,0.0165068303046711,-0.893578554312988));
#90268=DIRECTION('center_axis',(-0.147016018594641,-0.986495108895638,0.0722058889673391));
#90269=DIRECTION('ref_axis',(-0.537122031167507,0.0183213433011018,-0.843305550802398));
#90270=DIRECTION('center_axis',(0.11626477814819,-0.98649511025318,-0.115368534742875));
#90271=DIRECTION('ref_axis',(-0.630208146839801,0.0165068232943342,-0.776250743279176));
#90272=DIRECTION('center_axis',(-0.128056731448253,-0.986495108989023,0.102121855993341));
#90273=DIRECTION('ref_axis',(-0.705850180445786,0.0183213393733161,-0.708124177872934));
#90274=DIRECTION('center_axis',(0.0887457420157033,-0.986495110165441,-0.137664777244423));
#90275=DIRECTION('ref_axis',(-0.782345196015598,0.0165068299203812,-0.622626307537109));
#90276=DIRECTION('center_axis',(-0.103109656079333,-0.986495108998286,0.127262715457674));
#90277=DIRECTION('ref_axis',(-0.841573562645043,0.018321339942445,-0.53983170262559));
#90278=DIRECTION('center_axis',(0.0570770554641016,-0.986495110139405,-0.153523963636272));
#90279=DIRECTION('ref_axis',(-0.897900651127143,0.0165068329766776,-0.439888559945053));
#90280=DIRECTION('center_axis',(-0.0733412699599285,-0.986495110625006,
0.146452909952731));
#90281=DIRECTION('ref_axis',(-0.937945899781614,0.0183213239878117,-0.346297297376391));
#90282=DIRECTION('center_axis',(0.02273951420849,-0.986495110181865,-0.162204537793588));
#90283=DIRECTION('ref_axis',(-0.971471270290504,0.0165068302411123,-0.236582111655858));
#90284=DIRECTION('center_axis',(-0.04014354410436,-0.986495110627204,0.158795127681432));
#90285=DIRECTION('ref_axis',(-0.990460928077634,0.0183213224042447,-0.13657041808881));
#90286=DIRECTION('center_axis',(-0.0126613009638283,-0.986495110234729,
-0.163300609125851));
#90287=DIRECTION('ref_axis',(-0.99961697252754,0.016506827654815,-0.0222133490417421));
#90288=DIRECTION('center_axis',(-0.00506877555090952,-0.98649510877511,
0.163712271614556));
#90289=DIRECTION('ref_axis',(-0.996663104595291,0.0183213468885308,0.0795423420994461));
#90290=DIRECTION('center_axis',(-0.0474700944980979,-0.986495110139843,
-0.156760925611329));
#90291=DIRECTION('ref_axis',(-0.981021696401571,0.0165068314900331,0.193194088169239));
#90292=DIRECTION('center_axis',(0.0302430480139253,-0.986495110576138,0.160974391926792));
#90293=DIRECTION('ref_axis',(-0.956262422213734,0.0183213243394206,0.29193579591474));
#90294=DIRECTION('center_axis',(-0.0800592318971633,-0.986495110224997,
-0.142891276466436));
#90295=DIRECTION('ref_axis',(-0.916554935759703,0.0165068276718343,0.399567984671869));
#90296=DIRECTION('center_axis',(0.0641407206136267,-0.986495110682394,0.150709537053553));
#90297=DIRECTION('ref_axis',(-0.871147972385388,0.0183213211698033,0.490678651868431));
#90298=DIRECTION('center_axis',(-0.108904892632709,-0.986495110251071,-0.122340188864435));
#90299=DIRECTION('ref_axis',(-0.809231086683801,0.0165068288872051,0.58725852309238));
#90300=DIRECTION('center_axis',(0.0950392389666235,-0.986495110605007,0.133397675425997));
#90301=DIRECTION('ref_axis',(-0.74529960925457,0.0183213254219731,0.666477922724952));
#90302=DIRECTION('center_axis',(-0.132658279393603,-0.986495110257214,-0.0960686127043377));
#90303=DIRECTION('ref_axis',(-0.664068490537254,0.0165068261774196,0.747489507996682));
#90304=DIRECTION('center_axis',(0.121493832547443,-0.986495110620513,0.109848283440187));
#90305=DIRECTION('ref_axis',(-0.584601866466365,0.0183213234933828,0.811113424145781));
#90306=DIRECTION('center_axis',(-0.150208717742504,-0.986495110197418,-0.0653049666620904));
#90307=DIRECTION('ref_axis',(-0.487854788014172,0.016506833265213,0.872768715220248));
#90308=DIRECTION('center_axis',(0.142267507527001,-0.986495108892044,0.0811625309741451));
#90309=DIRECTION('ref_axis',(-0.396568793550313,0.0183213435490668,0.917822161615531));
#90310=DIRECTION('center_axis',(-0.160735557249265,-0.986495110220616,-0.0314877459749657));
#90311=DIRECTION('ref_axis',(-0.28882953792318,0.016506825465469,0.957238226741982));
#90312=DIRECTION('center_axis',(0.156388912663549,-0.986495110500926,0.0486816695859882));
#90313=DIRECTION('ref_axis',(-0.189992599186342,0.018321327088903,0.981614558382321));
#90314=DIRECTION('center_axis',(-0.163746587452144,-0.98649510959552,0.00380182086643908));
#90315=DIRECTION('ref_axis',(-0.0762989170803437,0.0165068292334505,0.996948343617173));
#90316=DIRECTION('center_axis',(-0.163664333248049,0.986495979512518,0.00629828771255697));
#90317=DIRECTION('ref_axis',(-0.0757555104791332,-0.0189332063975585,0.996946656711157));
#90318=DIRECTION('center_axis',(0.163197764356552,0.986495107104501,0.0139245598818328));
#90319=DIRECTION('ref_axis',(-0.183634611457542,0.0165058305046527,0.98285598489005));
#90320=DIRECTION('center_axis',(-0.161191922426216,0.98649597748642,-0.0290318884617355));
#90321=DIRECTION('ref_axis',(-0.288298455888899,-0.0189332806778659,0.957353399333208));
#90322=DIRECTION('center_axis',(0.156388923028194,0.986495107029387,0.0486817066377158));
#90323=DIRECTION('ref_axis',(-0.390626320339424,0.0165058307684231,0.920401344745175));
#90324=DIRECTION('center_axis',(-0.1511823468822,0.98649597751628,-0.0630046374117834));
#90325=DIRECTION('ref_axis',(-0.487360881411285,-0.0189332810357842,0.872995362037643));
#90326=DIRECTION('center_axis',(0.142267505986882,0.986495107181025,0.0811625544704576));
#90327=DIRECTION('ref_axis',(-0.5793527766561,0.0165058262039459,0.814909760576098));
#90328=DIRECTION('center_axis',(-0.13410359443023,0.986495979823994,-0.094031418961912));
#90329=DIRECTION('ref_axis',(-0.663634846270329,-0.0189331951519553,0.747817039747755));
#90330=DIRECTION('center_axis',(0.121493822324455,0.986495107119942,0.109848326183918));
#90331=DIRECTION('ref_axis',(-0.740989340052899,0.0165058281422236,0.671313902407293));
#90332=DIRECTION('center_axis',(-0.110754427179715,0.986495977338123,-0.120661276123679));
#90333=DIRECTION('ref_axis',(-0.808877993467493,-0.0189332878563786,0.587671610931606));
#90334=DIRECTION('center_axis',(0.0950392208017098,0.986495107120491,0.133397714136095));
#90335=DIRECTION('ref_axis',(-0.867978066280491,0.0165058276362661,0.496328151639641));
#90336=DIRECTION('center_axis',(-0.0822263620131329,0.986495979699681,-0.141649240825542));
#90337=DIRECTION('ref_axis',(-0.916298899956403,-0.0189331999132928,0.400047322050441));
#90338=DIRECTION('center_axis',(0.0641406948191214,0.986495107043704,0.150709571849138));
#90339=DIRECTION('ref_axis',(-0.954381102941002,0.0165058315162098,0.298134647223489));
#90340=DIRECTION('center_axis',(-0.0498536337343701,0.98649597752984,-0.156013786316864));
#90341=DIRECTION('ref_axis',(-0.980874689975391,-0.0189332811454051,0.193717251247147));
#90342=DIRECTION('center_axis',(0.0302430199761457,0.986495106974469,0.160974419266395));
#90343=DIRECTION('ref_axis',(-0.996158339361333,0.0165058333444339,0.0860006999185329));
#90344=DIRECTION('center_axis',(-0.0151496822461874,0.986495978873035,-0.163083324699898));
#90345=DIRECTION('ref_axis',(-0.999585868728208,-0.0189332301313235,-0.0216708060687373));
#90346=DIRECTION('center_axis',(-0.00506879156494291,0.986495107120187,
0.163712281090948));
#90347=DIRECTION('ref_axis',(-0.991356319237998,0.0165058285717886,-0.130154546328768));
#90348=DIRECTION('center_axis',(0.0202625533420198,0.986495977468237,-0.162527275775636));
#90349=DIRECTION('ref_axis',(-0.971557521471604,-0.0189332835680874,-0.236045574509002));
#90350=DIRECTION('center_axis',(-0.040143584424462,0.98649510707811,0.158795139536779));
#90351=DIRECTION('ref_axis',(-0.94019957963103,0.0165058313262934,-0.340223908615873));
#90352=DIRECTION('center_axis',(0.054727380587086,0.986495977283348,-0.154371631519033));
#90353=DIRECTION('ref_axis',(-0.898100225644532,-0.0189332899024866,-0.43938310758461));
#90354=DIRECTION('center_axis',(-0.0733413127678706,0.986495107140305,0.146452911987861));
#90355=DIRECTION('ref_axis',(-0.845080151221418,0.0165058292689584,-0.534384782354184));
#90356=DIRECTION('center_axis',(0.0866332565622247,0.986495978515498,-0.138997709442183));
#90357=DIRECTION('ref_axis',(-0.782648764505326,-0.0189332432368636,-0.622175573065048));
#90358=DIRECTION('center_axis',(-0.103109680670976,0.986495107096398,0.12726271027601));
#90359=DIRECTION('ref_axis',(-0.71044571539837,0.0165058293165022,-0.70355841482472));
#90360=DIRECTION('center_axis',(0.11448819137911,0.986495977279155,-0.117124467327646));
#90361=DIRECTION('ref_axis',(-0.630601510825,-0.0189332895128348,-0.775875805199164));
#90362=DIRECTION('center_axis',(-0.128056754262896,0.986495107061115,0.102121846008249));
#90363=DIRECTION('ref_axis',(-0.542591628058386,0.0165058298040078,-0.839834437697949));
#90364=DIRECTION('center_axis',(0.136989821620645,0.986495977428063,-0.0897745804256088));
#90365=DIRECTION('ref_axis',(-0.449068033188857,-0.0189332841864589,-0.893296945207923));
#90366=DIRECTION('center_axis',(-0.14701603772493,0.986495107128574,0.0722058741588577));
#90367=DIRECTION('ref_axis',(-0.349366558275532,0.016505826638935,-0.936840736542597));
#90368=DIRECTION('center_axis',(0.153085958069839,0.986495977607133,-0.0582269319712594));
#90369=DIRECTION('ref_axis',(-0.246536634745093,-0.0189332775614308,-0.968948511908319));
#90370=DIRECTION('center_axis',(-0.159101011931081,0.986495106883992,0.0389136492306638));
#90371=DIRECTION('ref_axis',(-0.139805499905608,0.0165058369330538,-0.990041402943979));
#90372=DIRECTION('center_axis',(0.162023962704327,0.98649597747952,-0.0239566676796347));
#90373=DIRECTION('ref_axis',(-0.0324774595201144,-0.0189332820365999,-0.999293122889596));
#90374=DIRECTION('center_axis',(-0.163746601402507,0.986495107191856,0.00380184371816674));
#90375=DIRECTION('ref_axis',(0.0762927159752781,0.016505826028842,-0.996948834793552));
#90376=DIRECTION('center_axis',(0.163385893887828,0.986495979129472,0.0114338462408331));
#90377=DIRECTION('ref_axis',(0.183100325011878,-0.0189332213510897,-0.982911900482345));
#90378=DIRECTION('center_axis',(-0.160735581661557,0.986495107149784,-0.0314877175650721));
#90379=DIRECTION('ref_axis',(0.288823563605248,0.0165058287140023,-0.957240046553021));
#90380=DIRECTION('center_axis',(0.15710806840229,0.986495980083366,0.0462896977983183));
#90381=DIRECTION('ref_axis',(0.390116541163451,-0.0189331856892312,-0.920570811393845));
#90382=DIRECTION('center_axis',(-0.150208745852932,0.986495107055466,-0.0653049494671993));
#90383=DIRECTION('ref_axis',(0.487849340789981,0.016505830189358,-0.872771779023899));
#90384=DIRECTION('center_axis',(0.143484048841015,0.986495980220824,0.0789810656825073));
#90385=DIRECTION('ref_axis',(0.578891344290511,-0.0189331794489455,-0.815184854018694));
#90386=DIRECTION('center_axis',(-0.132658315821449,0.986495107001696,-0.0960685958319888));
#90387=DIRECTION('ref_axis',(0.664063827017501,0.0165058308092504,-0.747493673014138));
#90388=DIRECTION('center_axis',(0.123150951914379,0.986495977546296,0.107979300458746));
#90389=DIRECTION('ref_axis',(0.740597838944811,-0.0189332788902449,-0.671681748970999));
#90390=DIRECTION('center_axis',(-0.10890493398378,0.986495106879436,-0.12234017924181));
#90391=DIRECTION('ref_axis',(0.809227427902569,0.0165058359713355,-0.587263592698441));
#90392=DIRECTION('center_axis',(0.0970593980376401,0.986495977400082,0.131928616403066));
#90393=DIRECTION('ref_axis',(0.867674794371259,-0.0189332842684578,-0.496771559129146));
#90394=DIRECTION('center_axis',(-0.0800592662611623,0.986495107147041,-0.142891278462583));
#90395=DIRECTION('ref_axis',(0.916552454181826,0.0165058269382781,-0.399573718367906));
#90396=DIRECTION('center_axis',(0.0664293728880749,0.986495979621629,0.149709119989594));
#90397=DIRECTION('ref_axis',(0.954180240376983,-0.0189332022433862,-0.298632889559966));
#90398=DIRECTION('center_axis',(-0.047470133162406,0.98649510690294,-0.15676093427286));
#90399=DIRECTION('ref_axis',(0.981020504823173,0.0165058359565571,-0.193200223850445));
#90400=DIRECTION('center_axis',(0.0326931799835002,0.986495981711792,0.16048935805546));
#90401=DIRECTION('ref_axis',(0.996069280944152,-0.0189331239650817,-0.0865304823534663));
#90402=DIRECTION('center_axis',(-0.0126613348343359,0.986495107103492,-0.163300625415466));
#90403=DIRECTION('ref_axis',(0.99961712783561,0.0165058300291245,0.022207100502665));
#90404=DIRECTION('center_axis',(-0.00257148638013054,0.986495977523527,
0.163765300926962));
#90405=DIRECTION('ref_axis',(0.991383225516875,-0.0189332809941951,0.129618019713895));
#90406=DIRECTION('center_axis',(0.0227394880264797,0.986495107075598,-0.162204560355739));
#90407=DIRECTION('ref_axis',(0.971472764423259,0.0165058297100802,0.236576046060061));
#90408=DIRECTION('center_axis',(-0.0377160676873686,0.986495977585325,0.159383764688175));
#90409=DIRECTION('ref_axis',(0.940341194310948,-0.0189332781904157,0.33970570978249));
#90410=DIRECTION('center_axis',(0.0570770334185452,0.986495106966099,-0.153523992222986));
#90411=DIRECTION('ref_axis',(0.897903414895677,0.0165058338156129,0.43988295598799));
#90412=DIRECTION('center_axis',(-0.0710970874986947,0.986495977655359,0.147549619514932));
#90413=DIRECTION('ref_axis',(0.845329852688694,-0.018933275537671,0.533909141362766));
#90414=DIRECTION('center_axis',(0.0887457235084081,0.986495106948599,-0.137664812226802));
#90415=DIRECTION('ref_axis',(0.782349100079219,0.0165058346295532,0.622621428340222));
#90416=DIRECTION('center_axis',(-0.101153678319687,0.986495977432116,0.12881622519175));
#90417=DIRECTION('ref_axis',(0.710791828123047,-0.0189332835167351,0.703147571885711));
#90418=DIRECTION('center_axis',(0.116264764031022,0.986495106987654,-0.115368576892616));
#90419=DIRECTION('ref_axis',(0.630213007616838,0.0165058336096042,0.776246818020784));
#90420=DIRECTION('center_axis',(-0.126480445892826,0.986495977695225,0.104059515652792));
#90421=DIRECTION('ref_axis',(0.543017965192465,-0.0189332758823195,0.839507606006401));
#90422=DIRECTION('center_axis',(0.13834739311538,0.986495107082014,-0.0876778336948641));
#90423=DIRECTION('ref_axis',(0.448608856798898,0.0165058310964719,0.893575766872289));
#90424=DIRECTION('center_axis',(-0.145893125991885,0.986495977858703,0.0744370973165731));
#90425=DIRECTION('ref_axis',(0.349853187284538,-0.0189332677462982,0.936613195892145));
#90426=DIRECTION('center_axis',(0.153961049669868,0.986495106924751,-0.0558873795957304));
#90427=DIRECTION('ref_axis',(0.246028258851622,0.0165058354854542,0.969122104402415));
#90428=DIRECTION('center_axis',(-0.158484009812962,0.986495980522315,0.0413339938418896));
#90429=DIRECTION('ref_axis',(0.140329675865358,-0.0189331681346543,0.989923793640656));
#90430=DIRECTION('center_axis',(0.162375647171994,0.986495113156432,-0.0214835035307127));
#90431=DIRECTION('ref_axis',(0.0319435454120738,0.0165056650919532,0.999353377402798));
#90432=DIRECTION('center_axis',(-0.158253626588392,0.987363722264226,-0.00828671395391741));
#90433=DIRECTION('ref_axis',(0.132153477991923,0.0294968937920318,0.990790286342806));
#90434=DIRECTION('',(-0.726975930476597,0.,-0.686662942430772));
#90435=DIRECTION('center_axis',(-3.03776950303028E-15,-1.,-2.20606524517768E-14));
#90436=DIRECTION('ref_axis',(2.28515888441093E-33,2.20606524517768E-14,
-1.));
#90437=DIRECTION('center_axis',(-0.158221889114687,-0.987363722231891,0.00887208123073));
#90438=DIRECTION('ref_axis',(0.061138418742882,-0.00082842314327428,0.998128953326531));
#90439=DIRECTION('center_axis',(0.157698501290688,-0.987363722511171,-0.0156224889039391));
#90440=DIRECTION('ref_axis',(0.135390691994632,0.00594770339583162,0.990774437167981));
#90441=DIRECTION('center_axis',(0.155084985279889,0.987363722259802,-0.0325810881648317));
#90442=DIRECTION('ref_axis',(0.210647662491098,-0.00082873789506162,0.977561699065863));
#90443=DIRECTION('',(-0.514330808231265,0.,0.857591872456925));
#90444=DIRECTION('center_axis',(-0.156335142091049,0.98736372237026,0.0259268797681987));
#90445=DIRECTION('ref_axis',(0.3420544268796,0.0294968903025397,0.939217068900767));
#90446=DIRECTION('',(-0.857591872604236,0.,-0.514330807985639));
#90447=DIRECTION('center_axis',(-1.54182726050674E-14,-1.,-4.17837119886613E-14));
#90448=DIRECTION('ref_axis',(8.92452105586287E-32,4.17837119886613E-14,
-1.));
#90449=DIRECTION('center_axis',(-0.152615513172356,-0.987363722259592,0.0426776886068243));
#90450=DIRECTION('ref_axis',(0.274277257963118,-0.000828420576119193,0.961650299996616));
#90451=DIRECTION('center_axis',(0.150653225068809,-0.987363722493281,-0.049157759108585));
#90452=DIRECTION('ref_axis',(0.345212550285589,0.00594770451630662,0.93850568455194));
#90453=DIRECTION('center_axis',(0.144455213653567,0.987363722246305,-0.0651580481615592));
#90454=DIRECTION('ref_axis',(0.415869706492917,-0.000828737827710053,0.909423828814216));
#90455=DIRECTION('',(-0.31794913654061,0.,0.948107771602512));
#90456=DIRECTION('center_axis',(-0.147106602674719,0.987363722257596,0.0589281547235814));
#90457=DIRECTION('ref_axis',(0.535961290935937,0.0294968942300542,0.843727105081415));
#90458=DIRECTION('',(-0.948107771776315,0.,-0.317949136022339));
#90459=DIRECTION('center_axis',(-1.20200324666943E-14,-1.,-1.87461795955026E-14));
#90460=DIRECTION('ref_axis',(1.34216343081091E-31,1.87461795955026E-14,
-1.));
#90461=DIRECTION('center_axis',(-0.139873008188513,-0.987363722211362,0.0744877281249787));
#90462=DIRECTION('ref_axis',(0.474591193787211,-0.000828424723521796,0.880205948907475));
#90463=DIRECTION('center_axis',(0.136563571729436,-0.987363722495009,-0.0803944673301516));
#90464=DIRECTION('ref_axis',(0.538892651517533,0.00594770519656905,0.842353450128447));
#90465=DIRECTION('center_axis',(0.127070876965365,0.9873637222521,-0.094688289707496));
#90466=DIRECTION('ref_axis',(0.601646145372297,-0.000828738403524133,0.798762310672778));
#90467=DIRECTION('',(-0.106700515256271,0.,0.994291204850996));
#90468=DIRECTION('center_axis',(-0.130999520502367,0.987363722264207,0.0891740185520412));
#90469=DIRECTION('ref_axis',(0.704807200182574,0.0294968937672872,0.708785400406133));
#90470=DIRECTION('',(-0.994291204618494,0.,-0.106700517422851));
#90471=DIRECTION('center_axis',(-4.20503607035944E-14,-1.,-4.19305404223952E-14));
#90472=DIRECTION('ref_axis',(1.,-4.20503607035944E-14,-5.12746317913781E-31));
#90473=DIRECTION('center_axis',(-0.120590197321097,-0.987363722182784,0.102814806460049));
#90474=DIRECTION('ref_axis',(0.652713776020247,-0.000828427761268574,0.757604144854577));
#90475=DIRECTION('center_axis',(0.116088354225877,-0.987363722546377,-0.107872023307662));
#90476=DIRECTION('ref_axis',(0.707374734234289,0.0059477013187499,0.706813702623252));
#90477=DIRECTION('center_axis',(0.103744844714906,0.987363722262932,-0.119791014496784));
#90478=DIRECTION('ref_axis',(0.759290278625285,-0.000828735251910435,0.650751554729621));
#90479=DIRECTION('',(0.109537302858737,0.,0.993982685604952));
#90480=DIRECTION('center_axis',(-0.108767043158536,0.987363722376516,0.115250206322328));
#90481=DIRECTION('ref_axis',(0.840697110508886,0.0294968901382479,0.540701675468258));
#90482=DIRECTION('',(-0.993982686191135,0.,0.109537297539497));
#90483=DIRECTION('center_axis',(1.87804025222973E-14,-1.,1.19664911831704E-14));
#90484=DIRECTION('ref_axis',(1.,1.87804025222973E-14,1.48804922800187E-31));
#90485=DIRECTION('center_axis',(-0.0956687178831378,-0.987363722223788,
0.126334383502602));
#90486=DIRECTION('ref_axis',(0.800316189860067,-0.000828424311078544,0.599577609622829));
#90487=DIRECTION('center_axis',(0.0901849763702522,-0.98736372252264,-0.130305600352908));
#90488=DIRECTION('ref_axis',(0.842780758136601,0.0059477006296843,0.538224134141081));
#90489=DIRECTION('center_axis',(0.0755678242784833,0.987363722270313,-0.139292440133444));
#90490=DIRECTION('ref_axis',(0.881430841406361,-0.000828739094572826,0.472312380749423));
#90491=DIRECTION('',(0.32065327633744,0.,0.947196640816502));
#90492=DIRECTION('center_axis',(-0.0814487487602662,0.98736372219462,0.135937417289623));
#90493=DIRECTION('ref_axis',(0.937276955390323,0.0294968964833239,0.347335345152346));
#90494=DIRECTION('',(-0.947196641515213,0.,0.320653274273476));
#90495=DIRECTION('center_axis',(4.87987943628401E-14,-1.,1.7848809686811E-14));
#90496=DIRECTION('ref_axis',(1.,4.87987943628401E-14,8.49501243221605E-32));
#90497=DIRECTION('center_axis',(-0.0662738822247424,-0.987363722186029,
0.143946700711793));
#90498=DIRECTION('ref_axis',(0.910496703083341,-0.000828427828625555,0.413515498357315));
#90499=DIRECTION('center_axis',(0.060064647181345,-0.987363722582784,-0.146646232431821));
#90500=DIRECTION('ref_axis',(0.938779291700636,0.0059476984014665,0.344467801627056));
#90501=DIRECTION('center_axis',(0.0438573363386594,0.98736372229545,-0.152280707721466));
#90502=DIRECTION('ref_axis',(0.962356678422975,-0.000828742191178215,0.271788404243224));
#90503=DIRECTION('',(0.516775860806559,0.,0.856120733125673));
#90504=DIRECTION('center_axis',(-0.0503219923558105,0.987363722299207,0.150268349870477));
#90505=DIRECTION('ref_axis',(0.990030773344163,0.029496893116985,0.137727996892442));
#90506=DIRECTION('',(-0.856120735019485,0.,0.51677585766916));
#90507=DIRECTION('center_axis',(-4.41384618210966E-14,-1.,-5.94961382401061E-15));
#90508=DIRECTION('ref_axis',(1.,-4.41384618210967E-14,6.09873644106572E-32));
#90509=DIRECTION('center_axis',(-0.0337801471428057,-0.987363722229621,
0.154828232838452));
#90510=DIRECTION('ref_axis',(0.978103405358154,-0.000828425242064668,0.208117856366055));
#90511=DIRECTION('center_axis',(0.027135767662474,-0.98736372254328,-0.156129848263698));
#90512=DIRECTION('ref_axis',(0.990881548486045,0.0059477021680321,0.134604538217762));
#90513=DIRECTION('center_axis',(0.0100961228227622,0.987363722292352,-0.158148500482742));
#90514=DIRECTION('ref_axis',(0.998283786987473,-0.000828739584164497,0.0585559034483356));
#90515=DIRECTION('',(0.68873457818185,0.,0.725013572849964));
#90516=DIRECTION('center_axis',(-0.0168422378220747,0.98736372233166,0.157572900108212));
#90517=DIRECTION('ref_axis',(0.996491852157853,0.0294968921553463,-0.078319358629834));
#90518=DIRECTION('',(-0.725013574350738,0.,0.688734576602022));
#90519=DIRECTION('center_axis',(-1.47951734182214E-14,-1.,1.22598313723652E-15));
#90520=DIRECTION('ref_axis',(1.,-1.47951734182214E-14,-9.56296692960351E-33));
#90521=DIRECTION('center_axis',(0.000293106042264333,-0.987363722206634,
0.158470168041523));
#90522=DIRECTION('ref_axis',(0.999975078494077,-0.000828426208563937,-0.00701114118961083));
#90523=DIRECTION('center_axis',(-0.00706195171612666,-0.987363722497847,
-0.158313007466707));
#90524=DIRECTION('ref_axis',(0.996651285363972,0.00594770418828643,-0.0815526835685473));
#90525=DIRECTION('center_axis',(-0.0241371713095924,0.987363722274126,-0.156621444566684));
#90526=DIRECTION('ref_axis',(0.987532254978932,-0.000828740157184411,-0.157414607219208));
#90527=DIRECTION('',(0.828488832258417,0.,0.560005584635622));
#90528=DIRECTION('center_axis',(0.0174250411497456,0.98736372235522,0.157509516276869));
#90529=DIRECTION('ref_axis',(0.956358079489829,0.029496890978043,-0.290704587540608));
#90530=DIRECTION('',(-0.560005585107112,0.,0.82848883193972));
#90531=DIRECTION('center_axis',(2.83714406763352E-14,-1.,-8.75569054394514E-15));
#90532=DIRECTION('ref_axis',(1.,2.83714406763352E-14,7.62782111538623E-32));
#90533=DIRECTION('center_axis',(0.0343526576848451,-0.98736372221655,0.154702213819542));
#90534=DIRECTION('ref_axis',(0.975089028263676,-0.000828423936585177,-0.221812309562794));
#90535=DIRECTION('center_axis',(-0.04092946378296,-0.987363722509905,-0.153093626470282));
#90536=DIRECTION('ref_axis',(0.955818716277087,0.00594770429341317,-0.293896591385574));
#90537=DIRECTION('center_axis',(-0.0572418406899089,0.987363722281683,-0.147770943004677));
#90538=DIRECTION('ref_axis',(0.930604812491207,-0.000828737692389969,-0.36602458409517));
#90539=DIRECTION('',(0.929503871604654,0.,0.368812354283258));
#90540=DIRECTION('center_axis',(0.050877542500497,0.987363722335174,0.15008116299369));
#90541=DIRECTION('ref_axis',(0.871506065916983,0.0294968919960261,-0.489496793076807));
#90542=DIRECTION('',(-0.36881235729421,0.,0.929503870409956));
#90543=DIRECTION('center_axis',(-6.45647938148473E-15,-1.,3.6625021161468E-15));
#90544=DIRECTION('ref_axis',(1.,-6.45647938148473E-15,3.32938379193174E-32));
#90545=DIRECTION('center_axis',(0.0668059115608821,-0.987363722212296,0.143700557547979));
#90546=DIRECTION('ref_axis',(0.904608900141983,-0.000828426894375263,-0.426241775865285));
#90547=DIRECTION('center_axis',(-0.0728831642277669,-0.987363722545787,
-0.140715755239683));
#90548=DIRECTION('ref_axis',(0.870293125245226,0.00594769960714374,-0.492498224382871));
#90549=DIRECTION('center_axis',(-0.0876699468935738,0.987363722232711,-0.132010834519156));
#90550=DIRECTION('ref_axis',(0.830163322499443,-0.000828733271870356,-0.557519659902545));
#90551=DIRECTION('',(0.987056341368623,0.,0.160373872448067));
#90552=DIRECTION('center_axis',(0.0819510668802593,0.987363722305636,0.135635181689508));
#90553=DIRECTION('ref_axis',(0.745903397621654,0.0294968927910069,-0.665400672326192));
#90554=DIRECTION('',(-0.160373871797992,0.,0.987056341474245));
#90555=DIRECTION('center_axis',(-3.31092047575097E-14,-1.,2.97889624204003E-14));
#90556=DIRECTION('ref_axis',(1.,-3.31092047575097E-14,1.45918977073932E-31));
#90557=DIRECTION('center_axis',(0.0961353978983388,-0.987363722178085,0.125979622945795));
#90558=DIRECTION('ref_axis',(0.791830264249037,-0.000828428021104229,-0.610740653900094));
#90559=DIRECTION('center_axis',(-0.101428922433329,-0.98736372251491,-0.121758174902198));
#90560=DIRECTION('ref_axis',(0.744073595414287,0.00594770212191701,-0.668071185912642));
#90561=DIRECTION('center_axis',(-0.113998699590731,0.987363722223241,-0.110078047444021));
#90562=DIRECTION('ref_axis',(0.690904319089775,-0.000828733047382951,-0.722945734522744));
#90563=DIRECTION('',(0.99845515443243,0.,-0.0555635184929094));
#90564=DIRECTION('center_axis',(0.109192650405688,0.987363722259072,0.114847050741811));
#90565=DIRECTION('ref_axis',(0.585423114535646,0.0294968943341152,-0.810191156574808));
#90566=DIRECTION('',(0.0555635134513151,0.,0.998455154712992));
#90567=DIRECTION('center_axis',(-2.59313835586931E-14,-1.,3.62100133214983E-14));
#90568=DIRECTION('ref_axis',(-3.14205114703E-31,-3.62100133214983E-14,-1.));
#90569=DIRECTION('center_axis',(0.12096970197302,-0.987363722185803,0.102368019009623));
#90570=DIRECTION('ref_axis',(0.642026524434684,-0.000828426218626936,-0.766681978158037));
#90571=DIRECTION('center_axis',(-0.125231977122196,-0.987363722511663,-0.0971073188486758));
#90572=DIRECTION('ref_axis',(0.583062012892976,0.00594770501934991,-0.812405880041617));
#90573=DIRECTION('center_axis',(-0.134996993587324,0.987363722305787,-0.0829981421288752));
#90574=DIRECTION('ref_axis',(0.519339399190732,-0.000828743577750021,-0.854567669428403));
#90575=DIRECTION('',(0.963167313918254,0.,-0.268902817760423));
#90576=DIRECTION('center_axis',(0.131328508942538,0.987363722349456,0.0886887959505408));
#90577=DIRECTION('ref_axis',(0.397569097381128,0.0294968917635576,-0.917098002496922));
#90578=DIRECTION('',(0.26890281566168,0.,0.963167314504194));
#90579=DIRECTION('center_axis',(1.75410397124104E-14,-1.,-4.09379242516552E-14));
#90580=DIRECTION('ref_axis',(2.71847771329592E-32,4.09379242516552E-14,
-1.));
#90581=DIRECTION('center_axis',(0.140147596603562,-0.987363722235991,0.0739697990975683));
#90582=DIRECTION('ref_axis',(0.462202338885112,-0.000828423573841437,-0.886774104066822));
#90583=DIRECTION('center_axis',(-0.143179326464291,-0.987363722500833,-0.0679158299848488));
#90584=DIRECTION('ref_axis',(0.394787097393298,0.00594770447014546,-0.918753379609191));
#90585=DIRECTION('center_axis',(-0.14968299022118,0.987363722223763,-0.0520373180984657));
#90586=DIRECTION('ref_axis',(0.323490742166045,-0.000828732599108519,-0.946230972297536));
#90587=DIRECTION('',(0.882842840276593,0.,-0.469668520738146));
#90588=DIRECTION('center_axis',(0.147323590943391,0.987363722314182,0.0583835542719632));
#90589=DIRECTION('ref_axis',(0.191125190999067,0.0294968922969366,-0.981122364799821));
#90590=DIRECTION('',(0.469668516573729,0.,0.882842842492045));
#90591=DIRECTION('center_axis',(-5.55366423744242E-15,-1.,2.9167748918442E-14));
#90592=DIRECTION('ref_axis',(2.50888775606184E-32,-2.9167748918442E-14,
-1.));
#90593=DIRECTION('center_axis',(0.152772343819061,-0.987363722231285,0.0421128363520289));
#90594=DIRECTION('ref_axis',(0.260766083603314,-0.000828424504378514,-0.965401659080318));
#90595=DIRECTION('center_axis',(-0.154431769537021,-0.98736372252885,-0.0355486707435878));
#90596=DIRECTION('ref_axis',(0.188052374858954,0.00594770257096927,-0.982140992497531));
#90597=DIRECTION('center_axis',(-0.157369969829508,0.987363722258356,-0.0186432980983465));
#90598=DIRECTION('ref_axis',(0.112516019003451,-0.000828734656997782,-0.993649565322948));
#90599=DIRECTION('',(0.761237617213275,0.,-0.64847304503692));
#90600=DIRECTION('',(0.648473045044079,0.,0.761237617207177));
#90601=DIRECTION('',(0.604037768699326,0.,-0.796955691356012));
#90602=DIRECTION('center_axis',(0.158221887796976,0.987363722343933,-0.00887209226136718));
#90603=DIRECTION('ref_axis',(-0.238502061658727,0.0294968912689423,-0.970693927038799));
#90604=DIRECTION('',(0.796955690039799,0.,0.604037770435913));
#90605=DIRECTION('center_axis',(9.00856342149284E-15,-1.,3.60048188131825E-14));
#90606=DIRECTION('ref_axis',(8.38398771006801E-32,-3.60048188131825E-14,
-1.));
#90607=DIRECTION('center_axis',(0.156335146200545,-0.987363722188261,-0.025926861919585));
#90608=DIRECTION('ref_axis',(-0.168696745814464,-0.000828429555302509,-0.985667652739037));
#90609=DIRECTION('center_axis',(-0.155084977231241,-0.987363722540395,0.0325811179728436));
#90610=DIRECTION('ref_axis',(-0.241718585361551,0.00594770165660325,-0.970328166310664));
#90611=DIRECTION('center_axis',(-0.150653235101027,0.987363722265028,0.0491577329475541));
#90612=DIRECTION('ref_axis',(-0.315105849132713,-0.000828737892779795,-0.949056171696838));
#90613=DIRECTION('',(0.41859378419889,0.,-0.908173575826809));
#90614=DIRECTION('center_axis',(0.15261550975314,0.987363722383874,-0.0426776979586559));
#90615=DIRECTION('ref_axis',(-0.441596517075355,0.0294968897379356,-0.896728749178202));
#90616=DIRECTION('',(0.908173574914674,0.,0.418593786177842));
#90617=DIRECTION('center_axis',(3.30758399370139E-15,-1.,6.64529426392992E-15));
#90618=DIRECTION('ref_axis',(-1.48148693090119E-32,-6.64529426392992E-15,
-1.));
#90619=DIRECTION('center_axis',(0.147106607223193,-0.987363722202016,-0.0589281443001684));
#90620=DIRECTION('ref_axis',(-0.376642118627037,-0.000828426419835203,-0.926358477148994));
#90621=DIRECTION('center_axis',(-0.144455199094643,-0.98736372253506,0.065158076063034));
#90622=DIRECTION('ref_axis',(-0.444659213194536,0.00594770107279819,-0.895680081822279));
#90623=DIRECTION('center_axis',(-0.136563586161633,0.987363722257796,0.0803944457279543));
#90624=DIRECTION('ref_axis',(-0.511757872330982,-0.000828736723875154,-0.859129322804611));
#90625=DIRECTION('',(0.213576822851012,0.,-0.976926271906364));
#90626=DIRECTION('center_axis',(0.139873000884617,0.987363722357622,-0.0744877399014954));
#90627=DIRECTION('ref_axis',(-0.624042411827881,0.02949689083002,-0.780833530063485));
#90628=DIRECTION('',(0.976926272040803,0.,0.213576822236072));
#90629=DIRECTION('center_axis',(-0.116088374656384,0.987363722186289,0.107872004616938));
#90630=DIRECTION('ref_axis',(-0.684480663267202,-0.000828733527300141,-0.729030544500044));
#90631=DIRECTION('',(-0.00142675803820793,0.,-0.999998982180232));
#90632=DIRECTION('center_axis',(5.59055571639679E-14,-1.,6.93467795473339E-14));
#90633=DIRECTION('ref_axis',(-7.40605167681581E-31,-6.93467795473339E-14,
-1.));
#90634=DIRECTION('center_axis',(0.13099952945553,-0.987363722173848,-0.0891740064000336));
#90635=DIRECTION('ref_axis',(-0.566976122848868,-0.000828429521764835,-0.823733810052612));
#90636=DIRECTION('center_axis',(-0.127070855582807,-0.987363722543795,0.0946883153610486));
#90637=DIRECTION('ref_axis',(-0.626808068839661,0.00594769944621863,-0.779150992881863));
#90638=DIRECTION('',(0.999998982187443,0.,-0.00142675298437618));
#90639=DIRECTION('center_axis',(0.120590189058315,0.987363722257648,-0.102814815432416));
#90640=DIRECTION('ref_axis',(-0.777308772805231,0.0294968950432108,-0.628427406231488));
#90641=DIRECTION('center_axis',(5.79216856928677E-15,-1.,4.64228725895709E-15));
#90642=DIRECTION('ref_axis',(1.,5.79216856928677E-15,-4.5294716458435E-32));
#90643=DIRECTION('center_axis',(-0.0901850056978048,0.987363722272389,0.130305581951427));
#90644=DIRECTION('ref_axis',(-0.825197905853612,-0.000828740984372925,-0.564843101545194));
#90645=DIRECTION('center_axis',(0.108767053397027,-0.987363722210359,-0.115250198083277));
#90646=DIRECTION('ref_axis',(-0.730798958875046,-0.000828424236561228,-0.682592261471249));
#90647=DIRECTION('center_axis',(-0.103744820254132,-0.987363722562327,0.119791033213271));
#90648=DIRECTION('ref_axis',(-0.77964807635652,0.00594769884537839,-0.626189669279223));
#90649=DIRECTION('',(-0.216363620211502,0.,-0.976312851420575));
#90650=DIRECTION('center_axis',(0.095668712408137,0.987363722216639,-0.126334387704511));
#90651=DIRECTION('ref_axis',(-0.894229041770426,0.0294968962556897,-0.44663671363383));
#90652=DIRECTION('',(0.976312851284768,0.,-0.216363620824314));
#90653=DIRECTION('center_axis',(1.33094108435812E-14,-1.,6.57721627024115E-15));
#90654=DIRECTION('ref_axis',(1.,1.33094108435812E-14,-6.4878940055379E-32));
#90655=DIRECTION('center_axis',(0.0814487538371677,-0.98736372221363,-0.135937414109653));
#90656=DIRECTION('ref_axis',(-0.860450443134181,-0.000828423328988154,-0.509533461732377));
#90657=DIRECTION('center_axis',(-0.0755677974550038,-0.987363722503276,
0.139292453034161));
#90658=DIRECTION('ref_axis',(-0.896032606438773,0.00594770394761603,-0.443948412561966));
#90659=DIRECTION('center_axis',(-0.0600646822450734,0.987363722285192,0.146646220073785));
#90660=DIRECTION('ref_axis',(-0.927329806319798,-0.000828740673294093,-0.374244229748146));
#90661=DIRECTION('',(-0.421183564268117,0.,-0.906975415979069));
#90662=DIRECTION('center_axis',(0.066273868112041,0.987363722344678,-0.143946706121153));
#90663=DIRECTION('ref_axis',(-0.969336154742115,0.0294968920441755,-0.243961784854727));
#90664=DIRECTION('',(0.906975416896828,0.,-0.421183562291816));
#90665=DIRECTION('center_axis',(2.88243025748643E-14,-1.,7.12462940101803E-15));
#90666=DIRECTION('ref_axis',(1.,2.88243025748643E-14,7.26131034139924E-33));
#90667=DIRECTION('center_axis',(0.0503220024830037,-0.987363722218607,-0.150268347008667));
#90668=DIRECTION('ref_axis',(-0.949868222071152,-0.000828424185777103,-0.31264944332712));
#90669=DIRECTION('center_axis',(-0.0438573035848928,-0.987363722504221,
0.152280715801018));
#90670=DIRECTION('ref_axis',(-0.970519647663539,0.00594770305628532,-0.240948621758651));
#90671=DIRECTION('center_axis',(-0.0271357991671827,0.987363722265874,0.156129844542407));
#90672=DIRECTION('ref_axis',(-0.98610079774319,-0.000828739050910494,-0.166146110041224));
#90673=DIRECTION('',(-0.606309431371119,0.,-0.795228818284669));
#90674=DIRECTION('center_axis',(0.0337801347624371,0.98736372233779,-0.154828234849766));
#90675=DIRECTION('ref_axis',(-0.999118186429611,0.029496891799609,-0.0298794732176964));
#90676=DIRECTION('',(0.795228820662645,0.,-0.606309428252191));
#90677=DIRECTION('center_axis',(2.2261493369811E-14,-1.,5.7126488416311E-16));
#90678=DIRECTION('ref_axis',(-0.999670904435999,-2.2268821940597E-14,-0.025653125035977));
#90679=DIRECTION('center_axis',(0.0168422547261848,-0.987363722175753,-0.157572899278337));
#90680=DIRECTION('ref_axis',(-0.994871219550474,-0.000828429980520805,-0.101146281265901));
#90681=DIRECTION('center_axis',(-0.0100960892783663,-0.987363722538625,
0.158148501086643));
#90682=DIRECTION('ref_axis',(-0.999626268953331,0.00594770075836641,-0.026682340117246));
#90683=DIRECTION('center_axis',(0.00706192035904516,0.987363722268906,0.158313010293318));
#90684=DIRECTION('ref_axis',(-0.998762811448472,-0.000828741003265544,0.0497208171281756));
#90685=DIRECTION('',(-0.763084941849124,0.,-0.646298206343728));
#90686=DIRECTION('center_axis',(-0.000293123686553503,0.987363722433932,
-0.158470166592687));
#90687=DIRECTION('ref_axis',(-0.982182562075402,0.0294968878401235,0.185599968649636));
#90688=DIRECTION('',(0.646298209424309,0.,-0.763084939240012));
#90689=DIRECTION('center_axis',(-2.91517827299545E-14,-1.,5.63687199036495E-15));
#90690=DIRECTION('ref_axis',(1.,-2.91517827299545E-14,4.7509437268998E-32));
#90691=DIRECTION('center_axis',(-0.0174250288915529,-0.987363722242448,
-0.157509518339896));
#90692=DIRECTION('ref_axis',(-0.993355143863366,-0.000828424355271347,0.115086367017463));
#90693=DIRECTION('center_axis',(0.0241372029417864,-0.987363722544807,0.15662143798538));
#90694=DIRECTION('ref_axis',(-0.981991476957315,0.00594770218863757,0.188831575807297));
#90695=DIRECTION('center_axis',(0.0409294387520858,0.987363722256636,0.153093634795702));
#90696=DIRECTION('ref_axis',(-0.964723785918027,-0.000828736195093086,0.26326285358992));
#90697=DIRECTION('',(-0.884179450376195,0.,-0.467147406642111));
#90698=DIRECTION('center_axis',(-0.034352670268466,0.987363722389285,-0.154702209922811));
#90699=DIRECTION('ref_axis',(-0.919321172442398,0.0294968898590875,0.39240096252147));
#90700=DIRECTION('',(0.467147409756163,0.,-0.884179448730917));
#90701=DIRECTION('center_axis',(-1.36292347146493E-14,-1.,5.88592831751186E-15));
#90702=DIRECTION('ref_axis',(1.,-1.36292347146493E-14,6.86030150678352E-32));
#90703=DIRECTION('center_axis',(-0.0508775298392963,-0.987363722225418,
-0.150081168007915));
#90704=DIRECTION('ref_axis',(-0.945390886052626,-0.000828426384568328,0.325937703063571));
#90705=DIRECTION('center_axis',(0.0572418717131348,-0.987363722545251,0.14777092922616));
#90706=DIRECTION('ref_axis',(-0.918439854452641,0.00594769839045913,0.395515939801251));
#90707=DIRECTION('center_axis',(0.0728831399834482,0.987363722227794,0.140715770028199));
#90708=DIRECTION('ref_axis',(-0.885575348115344,-0.000828733305052812,0.46449501182628));
#90709=DIRECTION('',(-0.963930709595031,0.,-0.266153315026547));
#90710=DIRECTION('center_axis',(-0.0668059229005943,0.987363722268358,-0.143700551890982));
#90711=DIRECTION('ref_axis',(-0.813473347210432,0.0294968936793228,0.580853722241259));
#90712=DIRECTION('',(0.266153317126985,0.,-0.963930709015074));
#90713=DIRECTION('center_axis',(-1.80679352823365E-14,-1.,1.30173017661079E-14));
#90714=DIRECTION('ref_axis',(1.,-1.80679352823365E-14,-2.73483845405841E-32));
#90715=DIRECTION('center_axis',(-0.0819510561257991,-0.987363722198956,
-0.135635188963959));
#90716=DIRECTION('ref_axis',(-0.853221199866751,-0.000828426942305628,0.521548557477386));
#90717=DIRECTION('center_axis',(0.0876699694749035,-0.987363722548255,0.132010817162542));
#90718=DIRECTION('ref_axis',(-0.811943005497672,0.00594769930014769,0.583706416528414));
#90719=DIRECTION('center_axis',(0.101428901188324,0.987363722241381,0.12175819481815));
#90720=DIRECTION('ref_axis',(-0.765018391449837,-0.000828736539028817,0.644007898972717));
#90721=DIRECTION('',(-0.998609640477332,0.,-0.0527141911228325));
#90722=DIRECTION('center_axis',(-0.0961354100920676,0.987363722345577,-0.125979612328009));
#90723=DIRECTION('ref_axis',(-0.669588411565198,0.0294968912752532,0.742146409074847));
#90724=DIRECTION('',(0.052714190583305,0.,-0.998609640505812));
#90725=DIRECTION('center_axis',(-1.48471818950882E-14,-1.,1.65970364748812E-14));
#90726=DIRECTION('ref_axis',(-2.24967672759341E-32,-1.65970364748812E-14,
-1.));
#90727=DIRECTION('center_axis',(-0.10919264153557,-0.987363722195851,-0.114847059718733));
#90728=DIRECTION('ref_axis',(-0.721155841383537,-0.000828427497757081,0.692772376864352));
#90729=DIRECTION('center_axis',(0.113998717628287,-0.98736372253384,0.110078025978054));
#90730=DIRECTION('ref_axis',(-0.667480603309877,0.00594769975790412,0.744603430741944));
#90731=DIRECTION('center_axis',(0.125231961938295,0.987363722236169,0.0971073412313598));
#90732=DIRECTION('ref_axis',(-0.608690023979306,-0.000828737862473461,0.793407693371842));
#90733=DIRECTION('',(-0.986594694898508,0.,0.163189791341617));
#90734=DIRECTION('center_axis',(-0.120969709327324,0.987363722291078,-0.102368009303536));
#90735=DIRECTION('ref_axis',(-0.494394267007933,0.0294968931826504,0.868737153598406));
#90736=DIRECTION('',(-0.163189789191804,0.,-0.986594695254102));
#90737=DIRECTION('center_axis',(3.64406359406342E-14,-1.,-6.46690406393619E-14));
#90738=DIRECTION('ref_axis',(2.63573539539379E-31,6.46690406393619E-14,
-1.));
#90739=DIRECTION('center_axis',(-0.131328502646515,-0.987363722211956,-0.0886888068043261));
#90740=DIRECTION('ref_axis',(-0.555370033707088,-0.000828425196019373,0.831602933720103));
#90741=DIRECTION('center_axis',(0.134997009525635,-0.987363722493808,0.0829981139683667));
#90742=DIRECTION('ref_axis',(-0.491807552156378,0.00594770592011851,0.870683614429627));
#90743=DIRECTION('center_axis',(0.143179313670225,0.987363722302484,0.0679158598407304));
#90744=DIRECTION('ref_axis',(-0.423899990380177,-0.000828742487650782,0.905708623863975));
#90745=DIRECTION('',(-0.928447676446041,0.,0.371463204236903));
#90746=DIRECTION('center_axis',(-0.140147600709755,0.98736372229544,-0.0739697905241924));
#90747=DIRECTION('ref_axis',(-0.296082794574062,0.0294968934003906,0.954706715194221));
#90748=DIRECTION('',(-0.37146319874419,0.,-0.928447678643624));
#90749=DIRECTION('center_axis',(-1.08433710126974E-14,-1.,3.54953870307208E-14));
#90750=DIRECTION('ref_axis',(9.3471061085303E-32,-3.54953870307208E-14,
-1.));
#90751=DIRECTION('center_axis',(-0.147323588236072,-0.987363722231606,-0.0583835625000502));
#90752=DIRECTION('ref_axis',(-0.363615742431591,-0.000828421653191901,0.931548659799094));
#90753=DIRECTION('center_axis',(0.149682997529542,-0.987363722548287,0.0520372909187366));
#90754=DIRECTION('ref_axis',(-0.293138123667199,0.00594769907183128,0.956051601812698));
#90755=DIRECTION('center_axis',(0.15443176489187,0.987363722239235,0.0355486989672672));
#90756=DIRECTION('ref_axis',(-0.219288862023536,-0.00082873654431964,0.97565962722056));
#90757=DIRECTION('',(-0.826887478900176,0.,0.562367404139065));
#90758=DIRECTION('center_axis',(-0.152772346096393,0.987363722316901,-0.0421128260832527));
#90759=DIRECTION('ref_axis',(-0.0839268221560271,0.0294968927169789,0.996035251305311));
#90760=DIRECTION('',(-0.562367402337263,0.,-0.826887480125585));
#90761=DIRECTION('center_axis',(3.55128005392468E-15,-1.,-4.43958345616782E-14));
#90762=DIRECTION('ref_axis',(4.64735541056336E-32,4.43958345616782E-14,
-1.));
#90763=DIRECTION('center_axis',(-0.156429984571224,-0.987363722264397,-0.0253483704257581));
#90764=DIRECTION('ref_axis',(-0.154859183348945,-0.000828421406732601,0.987936205961939));
#90765=DIRECTION('center_axis',(0.157369971174602,-0.987363722509918,0.0186432734213431));
#90766=DIRECTION('ref_axis',(-0.0807618847282569,0.00594770427846209,0.996715678009008));
#90767=DIRECTION('center_axis',(0.158463155145726,0.987363722292644,0.00151932935097974));
#90768=DIRECTION('ref_axis',(-0.00442403238197619,-0.000828740020282138,
0.999989870512428));
#90769=DIRECTION('',(-0.686662939327357,0.,0.726975933407919));
#90770=DIRECTION('center_axis',(-0.16366813813436,0.986495111156834,0.00633531556422871));
#90771=DIRECTION('ref_axis',(-0.0335577555675336,-0.011985490160195,0.99936491086434));
#90772=DIRECTION('',(-0.649115980606237,0.,-0.760689452879165));
#90773=DIRECTION('',(-0.760689448176683,0.,0.649115986117006));
#90774=DIRECTION('',(0.47041426357662,-5.87988638135427E-14,0.882445704065506));
#90775=DIRECTION('center_axis',(-0.161203571543763,0.986495111286343,-0.0289966192801806));
#90776=DIRECTION('ref_axis',(-0.247607116033172,-0.0119854840352497,0.96878638732291));
#90777=DIRECTION('',(-0.88244570195255,0.,0.470414267540294));
#90778=DIRECTION('',(0.26971649656114,0.,0.962939775626069));
#90779=DIRECTION('center_axis',(-0.151201311299598,0.986495111047301,-0.0629726872624588));
#90780=DIRECTION('ref_axis',(-0.45007863477848,-0.0119854954962003,0.892908489383795));
#90781=DIRECTION('',(-0.96293977383831,0.,0.269716502943784));
#90782=DIRECTION('',(0.0564070978796147,0.,0.998407852187071));
#90783=DIRECTION('center_axis',(-0.134129035688083,0.986495111227673,-0.0940042409111719));
#90784=DIRECTION('ref_axis',(-0.631504978925667,-0.0119854855253044,0.775279181797638));
#90785=DIRECTION('',(-0.998407852456459,0.,0.0564070931114327));
#90786=DIRECTION('',(-0.159539851947166,0.,0.987191488841287));
#90787=DIRECTION('center_axis',(-0.110785028158436,0.986495111480653,-0.120640260944295));
#90788=DIRECTION('ref_axis',(-0.783402851553951,-0.0119854703909857,0.621398680942151));
#90789=DIRECTION('',(-0.987191489609563,0.,-0.159539847193271));
#90790=DIRECTION('',(-0.368026896765542,0.,0.929815144669695));
#90791=DIRECTION('center_axis',(-0.0822608656811558,0.986495111070506,-0.14163525624426));
#90792=DIRECTION('ref_axis',(-0.898669672447652,-0.0119854910711511,0.438462276400848));
#90793=DIRECTION('',(-0.929815148084192,0.,-0.368026888138859));
#90794=DIRECTION('',(-0.559305396851014,0.,0.828961683706388));
#90795=DIRECTION('center_axis',(-0.0498902987825146,0.986495110498608,-0.156007548053709));
#90796=DIRECTION('ref_axis',(-0.971915701787856,-0.0119855316084904,0.235023861874241));
#90797=DIRECTION('',(-0.828961686239684,0.,-0.559305393096348));
#90798=DIRECTION('',(-0.724431406155912,0.,0.689346892192145));
#90799=DIRECTION('center_axis',(-0.0151868356753008,0.986495111189406,-0.163085117719467));
#90800=DIRECTION('ref_axis',(-0.999716036541778,-0.0119854881813905,0.0205959790797065));
#90801=DIRECTION('',(-0.689346895693392,0.,-0.724431402824231));
#90802=DIRECTION('',(-0.855683806145248,-5.87988641770928E-14,0.51749900859884));
#90803=DIRECTION('center_axis',(0.0202266966104539,0.986495111081771,-0.162537000575233));
#90804=DIRECTION('ref_axis',(-0.980770758190615,-0.0119854951240054,-0.194794937780318));
#90805=DIRECTION('',(-0.517499012391679,0.,-0.855683803851421));
#90806=DIRECTION('',(-0.94692537997107,0.,0.3214534566102));
#90807=DIRECTION('center_axis',(0.0546944451109593,0.98649511090908,-0.154388839708337));
#90808=DIRECTION('ref_axis',(-0.915965732122738,-0.0119855084629822,-0.401077455317225));
#90809=DIRECTION('',(-0.321453447458394,0.,-0.94692538307784));
#90810=DIRECTION('',(-0.993889783294678,0.,0.110377074895372));
#90811=DIRECTION('center_axis',(0.0866047677771553,0.98649511109968,-0.139021616933104));
#90812=DIRECTION('ref_axis',(-0.808331161615902,-0.0119854949252138,-0.588606049129707));
#90813=DIRECTION('',(-0.110377078468133,0.,-0.993889782897902));
#90814=DIRECTION('',(-0.994381001341741,0.,-0.105860399444722));
#90815=DIRECTION('center_axis',(0.114465528291893,0.986495110946573,-0.117153911208147));
#90816=DIRECTION('ref_axis',(-0.662899930242844,-0.0119855040691067,-0.748612069216254));
#90817=DIRECTION('',(0.105860400614547,0.,-0.994381001217203));
#90818=DIRECTION('',(-0.948376065643579,0.,-0.317147975106899));
#90819=DIRECTION('center_axis',(0.136974028313873,0.986495111363286,-0.0898081890687445));
#90820=DIRECTION('ref_axis',(-0.486472225758986,-0.0119854780315482,-0.873613828806214));
#90821=DIRECTION('',(0.317147963438495,0.,-0.948376069545629));
#90822=DIRECTION('',(-0.858026121541977,0.,-0.513606050150923));
#90823=DIRECTION('center_axis',(0.153077755278516,0.986495111131323,-0.0582631663479477));
#90824=DIRECTION('ref_axis',(-0.287297626645643,-0.0119854883113736,-0.957766371195877));
#90825=DIRECTION('',(0.513606042133383,0.,-0.858026126341198));
#90826=DIRECTION('',(-0.727555834536971,0.,-0.686048473237286));
#90827=DIRECTION('center_axis',(0.162023739988641,0.986495111162649,-0.0239938186266064));
#90828=DIRECTION('ref_axis',(-0.0746893088985458,-0.011985493682322,-0.997134822918871));
#90829=DIRECTION('',(0.686048470544795,0.,-0.727555837075855));
#90830=DIRECTION('',(-0.563065839593039,0.,-0.826412040257998));
#90831=DIRECTION('center_axis',(0.163393676940142,0.986495111128934,0.0113974582558265));
#90832=DIRECTION('ref_axis',(0.141411395860443,-0.0119854934156252,-0.989878358723124));
#90833=DIRECTION('',(0.826412038991147,0.,-0.563065841452396));
#90834=DIRECTION('',(-0.372247517812012,0.,-0.928133495507406));
#90835=DIRECTION('center_axis',(0.157123506083844,0.986495111154749,0.0462558050810983));
#90836=DIRECTION('ref_axis',(0.350899859315066,-0.0119854902499051,-0.936336284011325));
#90837=DIRECTION('',(0.92813349665939,0.,-0.372247514939744));
#90838=DIRECTION('',(-0.164023309346219,0.,-0.986456463302418));
#90839=DIRECTION('center_axis',(0.143506410560108,0.986495111275205,0.0789512859824004));
#90840=DIRECTION('ref_axis',(0.543980638303175,-0.0119854820197903,-0.839012165210984));
#90841=DIRECTION('',(0.986456463205108,0.,-0.164023309931453));
#90842=DIRECTION('',(0.0518704518711036,0.,-0.998653822013758));
#90843=DIRECTION('center_axis',(0.123179135122855,0.986495110884298,0.10795506876364));
#90844=DIRECTION('ref_axis',(0.711625489987081,-0.0119855067328437,-0.70245676708891));
#90845=DIRECTION('',(0.998653822433025,0.,0.0518704437990247));
#90846=DIRECTION('',(0.265338806748466,0.,-0.964155235236163));
#90847=DIRECTION('center_axis',(0.0970921231458836,0.986495110928653,0.13191101446388));
#90848=DIRECTION('ref_axis',(0.845995519867885,-0.0119855017409327,-0.533055276787957));
#90849=DIRECTION('',(0.964155239221636,0.,0.265338792266545));
#90850=DIRECTION('',(0.466400207442933,0.,-0.884573821960151));
#90851=DIRECTION('center_axis',(0.0664651877326862,0.986495111037399,0.149698946953442));
#90852=DIRECTION('ref_axis',(0.940807742843184,-0.0119854948486083,-0.338728709913328));
#90853=DIRECTION('',(0.884573827264078,0.,0.466400197383513));
#90854=DIRECTION('',(0.64565324338827,0.,-0.763630728364311));
#90855=DIRECTION('center_axis',(0.0327304299207421,0.98649511092306,0.160487118118879));
#90856=DIRECTION('ref_axis',(0.991628840021233,-0.0119855044504921,-0.12856356918354));
#90857=DIRECTION('',(0.763630725765876,0.,0.645653246461506));
#90858=DIRECTION('',(0.794716263103415,0.,-0.606981104449672));
#90859=DIRECTION('center_axis',(-0.0025347845356527,0.986495111068613,0.16377109239754));
#90860=DIRECTION('ref_axis',(0.996082475343742,-0.011985496666978,0.0876130708440827));
#90861=DIRECTION('',(0.606981103327021,0.,0.794716263960863));
#90862=DIRECTION('',(0.906619240092249,0.,-0.421949704934786));
#90863=DIRECTION('center_axis',(-0.0376814598423203,0.986495110935352,0.159397313919649));
#90864=DIRECTION('ref_axis',(0.953960400957062,-0.0119855033800166,0.299693011454338));
#90865=DIRECTION('',(0.421949718059285,0.,0.906619233983975));
#90866=DIRECTION('',(0.976129695249212,0.,-0.217188439040112));
#90867=DIRECTION('center_axis',(-0.0710662151983521,0.986495111309187,0.147570282985618));
#90868=DIRECTION('ref_axis',(0.867232196854255,-0.0119854844820484,0.497759645713745));
#90869=DIRECTION('',(0.217188431817788,0.,0.976129696856176));
#90870=DIRECTION('',(0.999997419781085,0.,-0.00227165824295009));
#90871=DIRECTION('center_axis',(-0.101127941833338,0.986495110572297,0.128843068100324));
#90872=DIRECTION('ref_axis',(0.739953182791551,-0.0119855304879602,0.67255158488816));
#90873=DIRECTION('',(0.0022716547051695,0.,0.999997419789121));
#90874=DIRECTION('',(0.97710637494025,-5.87988649286476E-14,0.21275133854132));
#90875=DIRECTION('center_axis',(-0.126461110862709,0.986495111429362,0.10409122232609));
#90876=DIRECTION('ref_axis',(0.578074774319208,-0.0119854720937904,0.815895767702276));
#90877=DIRECTION('',(-0.212751343062777,0.,0.977106373955766));
#90878=DIRECTION('',(0.908526924453842,0.,0.417826312649698));
#90879=DIRECTION('center_axis',(-0.145881042620839,0.986495110847264,0.0744722611332655));
#90880=DIRECTION('ref_axis',(0.389166237075605,-0.0119855091973612,0.921089565400506));
#90881=DIRECTION('',(-0.417826321376943,0.,0.908526920440232));
#90882=DIRECTION('',(0.797465763094675,5.87988639674914E-14,0.603364199047166));
#90883=DIRECTION('center_axis',(-0.158479760463402,0.986495111024107,0.0413710218510204));
#90884=DIRECTION('ref_axis',(0.182060721254228,-0.0119855011715295,0.983214239897927));
#90885=DIRECTION('',(-0.603364204891872,0.,0.797465758672558));
#90886=DIRECTION('center_axis',(-0.163746597512067,-0.986495108034302,0.00380179268390596));
#90887=DIRECTION('ref_axis',(0.0283600360616785,-0.000855145953452464,0.999597407499629));
#90888=DIRECTION('center_axis',(0.162375635431753,-0.986495109483943,-0.0214837608997425));
#90889=DIRECTION('ref_axis',(0.136269316546588,0.000855014963594679,0.990671460332505));
#90890=DIRECTION('center_axis',(-0.159101026864079,-0.986495107934883,0.0389135615350055));
#90891=DIRECTION('ref_axis',(0.242580940584724,-0.000855181560874777,0.97013079320756));
#90892=DIRECTION('center_axis',(0.153961009504166,-0.986495109500042,-0.0558874447882335));
#90893=DIRECTION('ref_axis',(0.346048496507044,0.000855014604045322,0.938216236810705));
#90894=DIRECTION('center_axis',(-0.147016064197888,-0.986495108037815,0.0722058078358147));
#90895=DIRECTION('ref_axis',(0.445458974655576,-0.000855174140654233,0.895301943802197));
#90896=DIRECTION('center_axis',(0.138347337083997,-0.986495109514399,-0.0876778947394444));
#90897=DIRECTION('ref_axis',(0.539646833411019,0.000855013109175183,0.841891064296351));
#90898=DIRECTION('center_axis',(-0.128056799604856,-0.986495107974529,0.102121780327624));
#90899=DIRECTION('ref_axis',(0.627507843518583,-0.000855179310340608,0.778609770675275));
#90900=DIRECTION('center_axis',(0.11626469994015,-0.98649510947649,-0.115368620199751));
#90901=DIRECTION('ref_axis',(0.708011881683628,0.000855015934826577,0.706200003074597));
#90902=DIRECTION('center_axis',(-0.103109737085179,-0.986495108050338,0.127262657173965));
#90903=DIRECTION('ref_axis',(0.780215142492183,-0.00085517714781326,0.625510671450094));
#90904=DIRECTION('center_axis',(0.088745649050942,-0.986495109536929,-0.137664841678073));
#90905=DIRECTION('ref_axis',(0.843271084078966,0.000855012026633975,0.537487811685735));
#90906=DIRECTION('center_axis',(-0.0733413800842794,-0.986495108018088,
0.146452872364165));
#90907=DIRECTION('ref_axis',(0.896440450959432,-0.000855178141471557,0.443163385845443));
#90908=DIRECTION('center_axis',(0.0570769521492894,-0.986495109556937,-0.153524005789303));
#90909=DIRECTION('ref_axis',(0.939099866070296,0.000855010557289998,0.343643289624137));
#90910=DIRECTION('center_axis',(-0.0401436454668397,-0.986495108155403,
0.158795117412634));
#90911=DIRECTION('ref_axis',(0.970749199943287,-0.000855162464340449,0.24009427212374));
#90912=DIRECTION('center_axis',(0.0227394040315997,-0.986495109510181,-0.162204557324335));
#90913=DIRECTION('ref_axis',(0.991017381969255,0.000855012561476741,0.133730391416173));
#90914=DIRECTION('center_axis',(-0.00506887156786354,-0.986495107936793,
0.16371227369322));
#90915=DIRECTION('ref_axis',(0.999666794490313,-0.000855181416868911,0.0257986173700359));
#90916=DIRECTION('center_axis',(-0.0126614160523676,-0.986495109506412,
-0.163300604602312));
#90917=DIRECTION('ref_axis',(0.996596027291127,0.000855012433976403,-0.0824355951108559));
#90918=DIRECTION('center_axis',(0.0302429388489829,-0.986495108017901,0.160974428113681));
#90919=DIRECTION('ref_axis',(0.98184108050694,-0.000855177729948001,-0.189703350787523));
#90920=DIRECTION('center_axis',(-0.0474702014878469,-0.98649510952696,-0.156760897069694));
#90921=DIRECTION('ref_axis',(0.955574949598001,0.000855013104886688,-0.294746984129386));
#90922=DIRECTION('center_axis',(0.0641406153199245,-0.986495107947539,0.150709599767088));
#90923=DIRECTION('ref_axis',(0.918105569468972,-0.000855182164299372,-0.396334999682744));
#90924=DIRECTION('center_axis',(-0.0800593341064972,-0.986495109508332,
-0.14289122414819));
#90925=DIRECTION('ref_axis',(0.869872250224507,0.000855012302154065,-0.493276329498301));
#90926=DIRECTION('center_axis',(0.0950391544766352,-0.986495107995121,0.133397754921367));
#90927=DIRECTION('ref_axis',(0.811440461235714,-0.000855179597100089,-0.584434467273644));
#90928=DIRECTION('center_axis',(-0.108904979399598,-0.986495109505147,-0.122340117640953));
#90929=DIRECTION('ref_axis',(0.743495289462457,0.000855014424802706,-0.668740624979125));
#90930=DIRECTION('center_axis',(0.121493764696541,-0.986495107991742,0.109848382091963));
#90931=DIRECTION('ref_axis',(0.666833302232419,-0.000855180911470078,-0.745206424891396));
#90932=DIRECTION('center_axis',(-0.132658350585395,-0.986495109509689,-0.096068522073723));
#90933=DIRECTION('ref_axis',(0.582353317866532,0.000855013809294289,-0.812935349287524));
#90934=DIRECTION('center_axis',(0.142267467271949,-0.986495108042873,0.0811626118573438));
#90935=DIRECTION('ref_axis',(0.491045754943609,-0.000855172111768815,-0.871133362483908));
#90936=DIRECTION('center_axis',(-0.15020876295495,-0.98649510946296,-0.065304873763033));
#90937=DIRECTION('ref_axis',(0.393981151766117,0.000855018383492621,-0.919118121351444));
#90938=DIRECTION('center_axis',(0.156388895407794,-0.986495108044346,0.0486817748002624));
#90939=DIRECTION('ref_axis',(0.292297455320061,-0.000855171931315512,-0.956327070773585));
#90940=DIRECTION('center_axis',(-0.160735584061753,-0.986495109510977,-0.0314876313375955));
#90941=DIRECTION('ref_axis',(0.187186863093603,0.000855011532842735,-0.982323952288885));
#90942=DIRECTION('center_axis',(0.163197752237843,-0.986495107978401,0.0139246400024645));
#90943=DIRECTION('ref_axis',(0.0798816522042827,-0.00085517970948843,-0.996803987907742));
#90944=DIRECTION('center_axis',(-0.163746585445659,-0.986495109509131,0.00380192970154928));
#90945=DIRECTION('ref_axis',(-0.0283600731337881,0.000855012924968857,-0.999597406561634));
#90946=DIRECTION('center_axis',(0.162375666692026,-0.986495107908973,-0.0214835969517151));
#90947=DIRECTION('ref_axis',(-0.136269329215492,-0.000855186051645274,-0.990671458442191));
#90948=DIRECTION('center_axis',(-0.159100978613244,-0.986495109517671,0.038913718686673));
#90949=DIRECTION('ref_axis',(-0.242580928943249,0.000855013151542972,-0.970130796266947));
#90950=DIRECTION('center_axis',(0.153961071525624,-0.986495108040822,-0.0558872996861401));
#90951=DIRECTION('ref_axis',(-0.346048507034067,-0.000855176233634949,-0.938216232780643));
#90952=DIRECTION('center_axis',(-0.147015987202403,-0.986495109509439,0.0722059444980999));
#90953=DIRECTION('ref_axis',(-0.44545896531509,0.000855013599121798,-0.895301948602903));
#90954=DIRECTION('center_axis',(0.138347433851548,-0.98649510792198,-0.0876777599662118));
#90955=DIRECTION('ref_axis',(-0.53964684376128,-0.000855183119961669,-0.841891057489222));
#90956=DIRECTION('center_axis',(-0.128056690864764,-0.986495109522306,0.102121901731897));
#90957=DIRECTION('ref_axis',(-0.627507834604862,0.000855012399275419,-0.778609778042451));
#90958=DIRECTION('center_axis',(0.11626481501738,-0.986495107985349,-0.115368516979069));
#90959=DIRECTION('ref_axis',(-0.708011890947838,-0.000855174620436058,-0.706199993594474));
#90960=DIRECTION('center_axis',(-0.103109611601658,-0.986495109457592,0.127262747933594));
#90961=DIRECTION('ref_axis',(-0.780215135878132,0.000855018570317058,-0.625510679916748));
#90962=DIRECTION('center_axis',(0.0887457784508654,-0.986495108087938,-0.137664768643676));
#90963=DIRECTION('ref_axis',(-0.843271090120732,-0.000855164333534696,-0.53748780196443));
#90964=DIRECTION('center_axis',(-0.0733412334058362,-0.98649510949555,0.146452935866354));
#90965=DIRECTION('ref_axis',(-0.896440445725003,0.000855014316550816,-0.443163396749862));
#90966=DIRECTION('center_axis',(0.0570771080566019,-0.986495108025782,-0.153523957664907));
#90967=DIRECTION('ref_axis',(-0.939099869820112,-0.000855177615941849,-0.343643278961039));
#90968=DIRECTION('center_axis',(-0.0401435003578533,-0.986495109535651,
0.158795145521716));
#90969=DIRECTION('ref_axis',(-0.970749197330676,0.00085501093554261,-0.24009428322671));
#90970=DIRECTION('center_axis',(0.0227395578524956,-0.986495108067061,-0.162204544536924));
#90971=DIRECTION('ref_axis',(-0.991017383362208,-0.000855170717919725,-0.133730380082331));
#90972=DIRECTION('center_axis',(-0.00506870820541044,-0.986495109499761,
0.163712269333069));
#90973=DIRECTION('ref_axis',(-0.999666794273265,0.000855013666306463,-0.0257986313405084));
#90974=DIRECTION('center_axis',(-0.0126612612176662,-0.986495108032662,
-0.163300625510142));
#90975=DIRECTION('ref_axis',(-0.996596026193594,-0.000855172538075693,0.0824356067186258));
#90976=DIRECTION('center_axis',(0.0302430947892424,-0.986495109526178,0.160974389573322));
#90977=DIRECTION('ref_axis',(-0.981841082996727,0.000855013054772608,0.1897033386435));
#90978=DIRECTION('center_axis',(-0.047470051408464,-0.986495108004711,-0.156760952096022));
#90979=DIRECTION('ref_axis',(-0.955574946429071,-0.00085517663212848,0.2947469939287));
#90980=DIRECTION('center_axis',(0.0641407625449427,-0.986495109514227,0.150709526854366));
#90981=DIRECTION('ref_axis',(-0.91810557395525,0.000855014026993956,0.396334989653089));
#90982=DIRECTION('center_axis',(-0.0800591980642029,-0.986495108016899,
-0.142891310666684));
#90983=DIRECTION('ref_axis',(-0.86987224425126,-0.000855177493715284,0.493276339745513));
#90984=DIRECTION('center_axis',(0.0950392813517479,-0.98649510950768,0.13339765334358));
#90985=DIRECTION('ref_axis',(-0.811440468144587,0.00085501312675468,0.584434457924793));
#90986=DIRECTION('center_axis',(-0.108904866952338,-0.986495107973881,-0.122340230086816));
#90987=DIRECTION('ref_axis',(-0.743495281044057,-0.000855177465418444,0.668740634130094));
#90988=DIRECTION('center_axis',(0.12149386579588,-0.986495109470824,0.109848256991724));
#90989=DIRECTION('ref_axis',(-0.666833310280483,0.000855016297068395,0.745206417878634));
#90990=DIRECTION('center_axis',(-0.132658262045057,-0.98649510792685,-0.0960686605901103));
#90991=DIRECTION('ref_axis',(-0.582353307756762,-0.000855182272220577,0.812935356352545));
#90992=DIRECTION('center_axis',(0.14226753416166,-0.986495109469175,0.0811624772722081));
#90993=DIRECTION('ref_axis',(-0.491045764644718,0.000855018131842603,0.871133357166673));
#90994=DIRECTION('center_axis',(-0.150208707700356,-0.986495107964131,-0.0653050234961099));
#90995=DIRECTION('ref_axis',(-0.393981140864148,-0.00085518191775455,0.919118125872443));
#90996=DIRECTION('center_axis',(0.156388933396878,-0.986495109534142,0.0486816225716499));
#90997=DIRECTION('ref_axis',(-0.292297465065824,0.000855011415688201,0.956327067938356));
#90998=DIRECTION('center_axis',(-0.160735562560586,-0.986495108038274,-0.0314877872338775));
#90999=DIRECTION('ref_axis',(-0.187186850714603,-0.000855172938858934,0.982323954507266));
#91000=DIRECTION('center_axis',(0.163197751262729,-0.986495109399359,0.0139245507624154));
#91001=DIRECTION('ref_axis',(-0.0798816770250956,0.000855085481519109,0.996803985999493));
#91002=DIRECTION('center_axis',(0.158463153892069,0.987363722548616,0.00151929375646194));
#91003=DIRECTION('ref_axis',(0.101017485130246,-0.0177430368692817,0.994726420851792));
#91004=DIRECTION('',(-0.604037770435915,0.,0.796955690039797));
#91005=DIRECTION('center_axis',(-0.15633514620055,0.987363722188261,0.0259268619195614));
#91006=DIRECTION('ref_axis',(0.240670182334486,0.0126220391173118,0.970524882454647));
#91007=DIRECTION('',(-0.796955691356011,0.,-0.604037768699328));
#91008=DIRECTION('center_axis',(-7.96270415248623E-15,1.,-3.17928001485767E-14));
#91009=DIRECTION('ref_axis',(3.14577109114985E-32,3.17928001485767E-14,
1.));
#91010=DIRECTION('center_axis',(0.184642396044489,-0.982569664103368,0.0215416054820449));
#91011=DIRECTION('ref_axis',(0.0522415413826683,0.031699892166001,0.998131222931447));
#91012=DIRECTION('center_axis',(1.88381627626997E-28,-1.,-3.78747958921603E-15));
#91013=DIRECTION('ref_axis',(-4.9737991503207E-14,-3.78747958921603E-15,
1.));
#91014=DIRECTION('center_axis',(-0.162390103070865,-0.98367345539406,0.0775627976399995));
#91015=DIRECTION('ref_axis',(0.394106230517453,0.0074048752412329,0.919035062927409));
#91016=DIRECTION('center_axis',(0.155084977674505,0.987363722502644,-0.0325811170069363));
#91017=DIRECTION('ref_axis',(0.312492526540577,-0.0177430400714078,0.949754497428315));
#91018=DIRECTION('',(-0.418593786177838,0.,0.908173574914676));
#91019=DIRECTION('center_axis',(9.0085634535061E-16,-1.,3.60048189652994E-15));
#91020=DIRECTION('ref_axis',(8.38412477077618E-34,-3.60048189652994E-15,
-1.));
#91021=DIRECTION('center_axis',(0.15065330845072,-0.987363724130564,-0.0491574706822454));
#91022=DIRECTION('ref_axis',(0.31510504360133,0.000828877171355419,0.949056439027542));
#91023=DIRECTION('center_axis',(-0.158221887569141,-0.987363722368478,0.0088720935928883));
#91024=DIRECTION('ref_axis',(0.166010951647992,-0.0177432069293348,0.985964270417945));
#91025=DIRECTION('center_axis',(-0.147106607223195,0.987363722202016,0.0589281443001649));
#91026=DIRECTION('ref_axis',(0.443677608797757,0.0126220360875831,0.896097574852487));
#91027=DIRECTION('',(-0.90817357582681,0.,-0.418593784198889));
#91028=DIRECTION('center_axis',(0.,1.,0.));
#91029=DIRECTION('ref_axis',(0.,0.,1.));
#91030=DIRECTION('center_axis',(0.184956602125193,-0.982569635358866,-0.0186538736204669));
#91031=DIRECTION('ref_axis',(0.265588707980032,0.0317007184657399,0.963565100365436));
#91032=DIRECTION('center_axis',(6.63290272699835E-29,-1.,5.33427468744545E-15));
#91033=DIRECTION('ref_axis',(1.24344978758017E-14,5.33427468744545E-15,
1.));
#91034=DIRECTION('center_axis',(-0.141919738091628,-0.983673454952057,0.110658582869502));
#91035=DIRECTION('ref_axis',(0.582457617398201,0.00740498728053316,0.812827343350472));
#91036=DIRECTION('center_axis',(0.144455200230007,0.987363722485691,-0.0651580742940492));
#91037=DIRECTION('ref_axis',(0.509355769148195,-0.0177430407164443,0.860373107983731));
#91038=DIRECTION('',(-0.213576824979769,0.,0.976926271440973));
#91039=DIRECTION('center_axis',(-6.61516801299152E-15,-1.,-1.32905885845373E-14));
#91040=DIRECTION('ref_axis',(3.63699579032327E-32,1.32905885845373E-14,
-1.));
#91041=DIRECTION('center_axis',(0.136563713886832,-0.987363724124565,-0.0803942058379));
#91042=DIRECTION('ref_axis',(0.511757143220611,0.000828875461218203,0.859129756979787));
#91043=DIRECTION('center_axis',(-0.152615509753122,-0.987363722383875,0.042677697958692));
#91044=DIRECTION('ref_axis',(0.374082881170212,-0.0177432067346035,0.927225526304235));
#91045=DIRECTION('center_axis',(-0.130999529455584,0.987363722173848,0.0891740063999588));
#91046=DIRECTION('ref_axis',(0.625939162818685,0.0126220395445972,0.779769740736058));
#91047=DIRECTION('',(-0.976926272506191,0.,-0.213576820107329));
#91048=DIRECTION('center_axis',(4.11524096047451E-14,1.,5.10218223628352E-14));
#91049=DIRECTION('ref_axis',(2.86061668474823E-31,-5.10218223628352E-14,
1.));
#91050=DIRECTION('center_axis',(0.176622045565574,-0.982569659761808,-0.0579785885978333));
#91051=DIRECTION('ref_axis',(0.466517537295754,0.0317000146039319,0.883943717930964));
#91052=DIRECTION('center_axis',(1.81653712354604E-28,-1.,-3.78747958921603E-15));
#91053=DIRECTION('ref_axis',(-4.79616346638068E-14,-3.78747958921603E-15,
1.));
#91054=DIRECTION('center_axis',(-0.114813486257611,-0.983673455401698,0.138579928241639));
#91055=DIRECTION('ref_axis',(0.743573933005707,0.00740488385359206,0.668612723367975));
#91056=DIRECTION('center_axis',(0.127070856773876,0.987363722510942,-0.0946883141052263));
#91057=DIRECTION('ref_axis',(0.682402099044296,-0.0177430385966853,0.730761629945973));
#91058=DIRECTION('',(0.00142675585917094,0.,0.999998982183341));
#91059=DIRECTION('center_axis',(2.32939818588969E-15,-1.,2.88944910854677E-15));
#91060=DIRECTION('ref_axis',(-4.09201826591339E-33,-2.88944910854677E-15,
-1.));
#91061=DIRECTION('center_axis',(0.116088551147125,-0.987363724096045,-0.107871797202751));
#91062=DIRECTION('ref_axis',(0.684480046866591,0.000828873339334421,0.729031123073972));
#91063=DIRECTION('center_axis',(-0.139873024001403,-0.987363721404996,0.0744877091202357));
#91064=DIRECTION('ref_axis',(0.564663102944633,-0.0177432449166011,0.825130751719246));
#91065=DIRECTION('center_axis',(-0.108767053397066,0.987363722210358,0.115250198083242));
#91066=DIRECTION('ref_axis',(0.778932498160699,0.0126220337349359,0.626980739395977));
#91067=DIRECTION('',(-0.999998982184334,0.,0.00142675516336331));
#91068=DIRECTION('center_axis',(-1.2789618240954E-13,1.,-1.02456022673949E-13));
#91069=DIRECTION('ref_axis',(-1.,-1.2789618240954E-13,-2.64322747769899E-31));
#91070=DIRECTION('center_axis',(0.16002890506933,-0.982569666692213,-0.094591752487546));
#91071=DIRECTION('ref_axis',(0.645632421359425,0.031699816815584,0.762990103542257));
#91072=DIRECTION('center_axis',(9.0826856177302E-29,-1.,-3.78747958921603E-15));
#91073=DIRECTION('ref_axis',(-2.39808173319034E-14,-3.78747958921603E-15,
1.));
#91074=DIRECTION('center_axis',(-0.0823386068103901,-0.983673455332332,
0.160021520749787));
#91075=DIRECTION('ref_axis',(0.869921560179819,0.00740490164403627,0.493134511635469));
#91076=DIRECTION('center_axis',(0.10374482146474,0.987363722520539,-0.119791032509259));
#91077=DIRECTION('ref_axis',(0.823540067399997,-0.0177430379354208,0.566980548159839));
#91078=DIRECTION('',(0.21636361808406,0.,0.976312851892043));
#91079=DIRECTION('center_axis',(-5.79216859279781E-15,-1.,-4.64228727930433E-15));
#91080=DIRECTION('ref_axis',(1.,-5.79216859279781E-15,2.18142135758451E-32));
#91081=DIRECTION('center_axis',(0.0901852223248424,-0.987363724138682,-0.13030541788127));
#91082=DIRECTION('ref_axis',(0.825197426429906,0.00082887969264323,0.564843801746921));
#91083=DIRECTION('center_axis',(-0.120590218143034,-0.987363721307667,0.102814790442288));
#91084=DIRECTION('ref_axis',(0.72884031643368,-0.017743249949096,0.68445377508061));
#91085=DIRECTION('center_axis',(-0.0814487538372487,0.987363722213629,0.135937414109611));
#91086=DIRECTION('ref_axis',(0.895503814866252,0.0126220332170288,0.444874815917308));
#91087=DIRECTION('',(-0.976312850813305,0.,0.216363622951729));
#91088=DIRECTION('center_axis',(0.,1.,0.));
#91089=DIRECTION('ref_axis',(0.,0.,1.));
#91090=DIRECTION('center_axis',(0.135953801314679,-0.982569636304925,-0.126781204126226));
#91091=DIRECTION('ref_axis',(0.794558088009599,0.0317006896209387,0.606360050676236));
#91092=DIRECTION('center_axis',(-3.13926580987588E-28,-1.,1.4137996331574E-14));
#91093=DIRECTION('ref_axis',(-2.22044604925032E-14,1.4137996331574E-14,
1.));
#91094=DIRECTION('center_axis',(-0.0460137206069841,-0.983673455505685,
0.17398066113625));
#91095=DIRECTION('ref_axis',(0.955592620402268,0.00740485812587767,0.294597881711432));
#91096=DIRECTION('center_axis',(0.0755677989895925,0.987363722458875,-0.139292452516357));
#91097=DIRECTION('ref_axis',(0.926170215102622,-0.0177430427789482,0.376688089922825));
#91098=DIRECTION('',(0.421183562291818,0.,0.906975416896828));
#91099=DIRECTION('center_axis',(-3.32735272456251E-15,-1.,-1.64430407496874E-15));
#91100=DIRECTION('ref_axis',(1.,-3.32735272456251E-15,-4.05495624528595E-33));
#91101=DIRECTION('center_axis',(0.0600649742539953,-0.987363724111366,-0.146646088174221));
#91102=DIRECTION('ref_axis',(0.927329485697342,0.00082892748148247,0.374245023795285));
#91103=DIRECTION('center_axis',(-0.0956687490241227,-0.987363721208003,
0.126334367859443));
#91104=DIRECTION('ref_axis',(0.858937762698334,-0.017743254060679,0.511772504875085));
#91105=DIRECTION('center_axis',(-0.0503220025106176,0.987363722217997,0.150268347003433));
#91106=DIRECTION('ref_axis',(0.970202368441141,0.0126220344007601,0.24196704014966));
#91107=DIRECTION('',(-0.906975415979067,0.,0.421183564268121));
#91108=DIRECTION('center_axis',(-3.1819119793911E-14,1.,-7.85687094207709E-15));
#91109=DIRECTION('ref_axis',(-1.,-3.1819119793911E-14,-5.25025999428999E-32));
#91110=DIRECTION('center_axis',(0.105520483328886,-0.982569658070307,-0.153043440361353));
#91111=DIRECTION('ref_axis',(0.906331316741022,0.0317000622763659,0.421377088065025));
#91112=DIRECTION('center_axis',(0.,-1.,-3.78747958921603E-15));
#91113=DIRECTION('ref_axis',(0.,-3.78747958921603E-15,1.));
#91114=DIRECTION('center_axis',(-0.00753719114751718,-0.983673455252781,
0.179804683422486));
#91115=DIRECTION('ref_axis',(0.996581232016566,0.00740491377047555,0.0822861789390829));
#91116=DIRECTION('center_axis',(0.0438573044439995,0.987363722468911,-0.152280715782539));
#91117=DIRECTION('ref_axis',(0.985493674732238,-0.0177430411866941,0.16878211265474));
#91118=DIRECTION('',(0.60630942963828,0.,0.795228819605844));
#91119=DIRECTION('center_axis',(-1.08091135104046E-14,-1.,-2.67173603827549E-15));
#91120=DIRECTION('ref_axis',(1.,-1.08091135104046E-14,1.06766753801264E-32));
#91121=DIRECTION('center_axis',(0.0271360641083462,-0.987363724133007,-0.15612978668693));
#91122=DIRECTION('ref_axis',(0.986100656652269,0.000828877203283326,0.166146946744577));
#91123=DIRECTION('center_axis',(-0.0662738681119184,-0.987363722344681,
0.143946706121192));
#91124=DIRECTION('ref_axis',(0.948872239264686,-0.0177432091114833,0.315161311209428));
#91125=DIRECTION('',(-0.795228819341497,0.,0.606309429984995));
#91126=DIRECTION('center_axis',(-1.96585202152636E-13,1.,-4.99806869102813E-15));
#91127=DIRECTION('ref_axis',(0.999676955525532,1.96648728437366E-13,0.0254162269269747));
#91128=DIRECTION('center_axis',(0.0701542349175453,-0.98256963793636,-0.172149034062771));
#91129=DIRECTION('ref_axis',(0.975725371780959,0.0317006430670899,0.216691181389651));
#91130=DIRECTION('center_axis',(0.0312917311449239,-0.983673455209738,0.177221220731855));
#91131=DIRECTION('ref_axis',(0.990970812698885,0.00740492932440456,-0.133873131735283));
#91132=DIRECTION('',(0.763084940440831,0.,0.646298208006501));
#91133=DIRECTION('center_axis',(0.0174250288914855,0.987363722242448,0.157509518339908));
#91134=DIRECTION('ref_axis',(0.98213114496707,0.0126220340066069,-0.187774061955342));
#91135=DIRECTION('',(-0.646298207761542,0.,0.763084940648299));
#91136=DIRECTION('center_axis',(-1.93063591611731E-13,1.,3.73787918254193E-14));
#91137=DIRECTION('ref_axis',(-1.,-1.93063591611731E-13,-9.54092960034444E-32));
#91138=DIRECTION('center_axis',(0.0315066138997435,-0.982569654868572,-0.183205367312284));
#91139=DIRECTION('ref_axis',(0.999495669260652,0.0317001500081216,0.0018728637601358));
#91140=DIRECTION('center_axis',(2.96028271985281E-28,-1.,-3.78747958921603E-15));
#91141=DIRECTION('ref_axis',(-7.8159700933611E-14,-3.78747958921603E-15,
1.));
#91142=DIRECTION('center_axis',(0.068657441857252,-0.983673455295322,0.166351101664464));
#91143=DIRECTION('ref_axis',(0.939023699618817,0.007404896535104,-0.343772685159094));
#91144=DIRECTION('center_axis',(-0.0241372015785544,0.98736372250249,-0.156621438462242));
#91145=DIRECTION('ref_axis',(0.965279604598994,-0.017743041285082,-0.260615558689739));
#91146=DIRECTION('',(0.88417944935828,0.,0.46714740856874));
#91147=DIRECTION('center_axis',(1.82198642830546E-14,-1.,-3.52304500584695E-15));
#91148=DIRECTION('ref_axis',(1.,1.82198642830546E-14,1.85586446763344E-32));
#91149=DIRECTION('center_axis',(-0.040929172955792,-0.987363724123068,-0.153093693818459));
#91150=DIRECTION('ref_axis',(0.964724009230363,0.00082887542359837,-0.263262034824671));
#91151=DIRECTION('center_axis',(0.000293123686674066,-0.987363722433934,
0.158470166592671));
#91152=DIRECTION('ref_axis',(0.993505920544914,-0.0177432049224071,-0.112388453683129));
#91153=DIRECTION('center_axis',(0.0508775298393055,0.987363722225417,0.150081168007913));
#91154=DIRECTION('ref_axis',(0.918803591899418,0.0126220361989575,-0.394513173056262));
#91155=DIRECTION('',(-0.467147407829532,0.,0.884179449748833));
#91156=DIRECTION('center_axis',(-1.50428781314511E-13,1.,6.50065517177513E-14));
#91157=DIRECTION('ref_axis',(-1.,-1.50428781314511E-13,-4.30966703185921E-32));
#91158=DIRECTION('center_axis',(-0.00861387361504059,-0.982569659926227,
-0.185695084947884));
#91159=DIRECTION('ref_axis',(0.976530624481854,0.0317000071570993,-0.213032976309585));
#91160=DIRECTION('center_axis',(0.,-1.,-3.78747958921603E-15));
#91161=DIRECTION('ref_axis',(0.,-3.78747958921603E-15,1.));
#91162=DIRECTION('center_axis',(0.102812836377922,-0.983673455335804,0.147702586110218));
#91163=DIRECTION('ref_axis',(0.843168882821576,0.00740489427710891,-0.537597807456616));
#91164=DIRECTION('center_axis',(-0.057241870175252,0.987363722501593,-0.147770930113592));
#91165=DIRECTION('ref_axis',(0.886687262551847,-0.0177430376327503,-0.462029093287289));
#91166=DIRECTION('',(0.963930709015073,0.,0.266153317126987));
#91167=DIRECTION('center_axis',(-1.02219260794816E-14,-1.,4.41444625500047E-15));
#91168=DIRECTION('ref_axis',(1.,-1.02219260794816E-14,6.68170667667052E-33));
#91169=DIRECTION('center_axis',(-0.0728828940410096,-0.987363724094902,
-0.140715884311807));
#91170=DIRECTION('ref_axis',(0.885575742122918,0.000828871478840528,-0.464494260390282));
#91171=DIRECTION('center_axis',(0.0343526343809698,-0.98736372143583,0.154702223977148));
#91172=DIRECTION('ref_axis',(0.946118111358501,-0.0177432443320615,-0.323335269712409));
#91173=DIRECTION('center_axis',(0.0819510561257198,0.987363722198955,0.135635188964013));
#91174=DIRECTION('ref_axis',(0.812513804514755,0.0126220362890575,-0.582805286243079));
#91175=DIRECTION('',(-0.266153315026551,0.,0.96393070959503));
#91176=DIRECTION('center_axis',(-1.59524822387274E-13,1.,1.14989370356372E-13));
#91177=DIRECTION('ref_axis',(-1.,-1.59524822387274E-13,-4.15996612950641E-31));
#91178=DIRECTION('center_axis',(-0.0483314596884342,-0.982569660846991,
-0.179501898562145));
#91179=DIRECTION('ref_axis',(0.907904086854337,0.0316999857459318,-0.417977607028057));
#91180=DIRECTION('center_axis',(1.34558305447855E-28,-1.,-3.78747958921603E-15));
#91181=DIRECTION('ref_axis',(-3.5527136788005E-14,-3.78747958921603E-15,
1.));
#91182=DIRECTION('center_axis',(0.132160818328594,-0.983673455323674,0.122147662238378));
#91183=DIRECTION('ref_axis',(0.707888425321867,0.00740489260537495,-0.706285455648657));
#91184=DIRECTION('center_axis',(-0.0876699682442016,0.987363722503006,-0.132010818318304));
#91185=DIRECTION('ref_axis',(0.76663440952793,-0.0177430384823854,-0.641838660967984));
#91186=DIRECTION('',(0.998609640362466,0.,0.0527141932988275));
#91187=DIRECTION('center_axis',(-6.02264512002837E-15,-1.,4.33910060592838E-15));
#91188=DIRECTION('ref_axis',(1.,-6.02264512002837E-15,-2.39473183021396E-32));
#91189=DIRECTION('center_axis',(-0.101428677285743,-0.98736372409962,-0.121758366267762));
#91190=DIRECTION('ref_axis',(0.765018938900932,0.000828885390579215,-0.644007248462237));
#91191=DIRECTION('center_axis',(0.0668059229005948,-0.987363722268358,0.143700551890981));
#91192=DIRECTION('ref_axis',(0.854490866293006,-0.0177432107440181,-0.51916330561233));
#91193=DIRECTION('center_axis',(0.109192641535518,0.98736372219585,0.114847059718792));
#91194=DIRECTION('ref_axis',(0.668231774075443,0.0126220373665493,-0.743846072980629));
#91195=DIRECTION('',(-0.0527141884073562,0.,0.998609640620675));
#91196=DIRECTION('center_axis',(1.31075898179972E-13,1.,-1.46594096344531E-13));
#91197=DIRECTION('ref_axis',(9.98802094496757E-32,1.46594096344531E-13,
1.));
#91198=DIRECTION('center_axis',(-0.0857885195141726,-0.982569635728196,
-0.164915859954485));
#91199=DIRECTION('ref_axis',(0.796825030841459,0.0317007065913415,-0.603377937470469));
#91200=DIRECTION('center_axis',(0.,-1.,7.99418401626902E-15));
#91201=DIRECTION('ref_axis',(0.,7.99418401626902E-15,1.));
#91202=DIRECTION('center_axis',(0.155329165193681,-0.983673454911944,0.0908811561427037));
#91203=DIRECTION('ref_axis',(0.539507892095231,0.00740500281159215,-0.841947979569));
#91204=DIRECTION('center_axis',(-0.11399871667095,0.987363722488542,-0.110078027375789));
#91205=DIRECTION('ref_axis',(0.610734582760325,-0.0177430389816003,-0.791636566858978));
#91206=DIRECTION('',(0.986594695254103,0.,-0.163189789191801));
#91207=DIRECTION('center_axis',(-1.2372651633228E-14,-1.,1.38308637850188E-14));
#91208=DIRECTION('ref_axis',(4.39963560667966E-32,-1.38308637850188E-14,
-1.));
#91209=DIRECTION('center_axis',(-0.125231787326932,-0.987363724103911,-0.0971075474232446));
#91210=DIRECTION('ref_axis',(0.60869069698727,0.000828875038098951,-0.793407176906866));
#91211=DIRECTION('center_axis',(0.0961354100921401,-0.987363722345579,0.125979612327939));
#91212=DIRECTION('ref_axis',(0.722908581050635,-0.0177432080803394,-0.690715833038721));
#91213=DIRECTION('center_axis',(0.131328502646465,0.987363722211955,0.08868880680441));
#91214=DIRECTION('ref_axis',(0.492703966766174,0.0126220350460105,-0.870105444968697));
#91215=DIRECTION('',(0.163189791341605,0.,0.98659469489851));
#91216=DIRECTION('center_axis',(0.,1.,0.));
#91217=DIRECTION('ref_axis',(0.,0.,1.));
#91218=DIRECTION('center_axis',(-0.119235357666559,-0.982569661740983,-0.142617633230741));
#91219=DIRECTION('ref_axis',(0.648487187440979,0.0316999532797268,-0.760565237627221));
#91220=DIRECTION('center_axis',(0.,-1.,-3.78747958921603E-15));
#91221=DIRECTION('ref_axis',(0.,-3.78747958921603E-15,1.));
#91222=DIRECTION('center_axis',(0.171234386949594,-0.983673455275735,0.0553653150618104));
#91223=DIRECTION('ref_axis',(0.345900567498622,0.00740490675994489,-0.93824195427406));
#91224=DIRECTION('center_axis',(-0.134997008872396,0.987363722451529,-0.0829981155338303));
#91225=DIRECTION('ref_axis',(0.426277487512531,-0.0177430452325937,-0.904418425279958));
#91226=DIRECTION('',(0.928447677255466,0.,-0.3714632022138));
#91227=DIRECTION('center_axis',(1.27542226361885E-14,-1.,-2.26341643165069E-14));
#91228=DIRECTION('ref_axis',(5.07241172839367E-32,2.26341643165069E-14,
-1.));
#91229=DIRECTION('center_axis',(-0.143179187504052,-0.987363724170279,-0.0679160986679622));
#91230=DIRECTION('ref_axis',(0.423900758702251,0.000828879569203518,-0.90570826413935));
#91231=DIRECTION('center_axis',(0.120969689331929,-0.987363721339821,0.102368042107466));
#91232=DIRECTION('ref_axis',(0.557523896409954,-0.0177432483395472,-0.829971253761372));
#91233=DIRECTION('center_axis',(0.147323588236072,0.987363722231605,0.0583835625000547));
#91234=DIRECTION('ref_axis',(0.294137871286664,0.0126220315474288,-0.955679651868013));
#91235=DIRECTION('',(0.371463200767281,0.,0.928447677834204));
#91236=DIRECTION('center_axis',(-9.56800049051936E-15,1.,3.13470915944282E-14));
#91237=DIRECTION('ref_axis',(6.09885243099091E-33,-3.13470915944282E-14,
1.));
#91238=DIRECTION('center_axis',(-0.147106180063853,-0.982569655018706,-0.113651418044136));
#91239=DIRECTION('ref_axis',(0.469826904776602,0.03170015665596,-0.882189197177128));
#91240=DIRECTION('center_axis',(0.,-1.,-3.78747958921603E-15));
#91241=DIRECTION('ref_axis',(0.,-3.78747958921603E-15,1.));
#91242=DIRECTION('center_axis',(0.179132923581415,-0.983673455474697,0.017260610755237));
#91243=DIRECTION('ref_axis',(0.136119321091654,0.00740486877593419,-0.990664775968116));
#91244=DIRECTION('center_axis',(-0.149682997370563,0.987363722508653,-0.05203729212805));
#91245=DIRECTION('ref_axis',(0.221888128067994,-0.017743037961803,-0.974910684743155));
#91246=DIRECTION('',(0.82688748012557,0.,-0.562367402337284));
#91247=DIRECTION('center_axis',(-6.5060226382221E-15,-1.,2.12972323065662E-14));
#91248=DIRECTION('ref_axis',(-2.27817423217471E-32,-2.12972323065662E-14,
-1.));
#91249=DIRECTION('center_axis',(-0.154431689931071,-0.987363724094681,-0.0355489730782223));
#91250=DIRECTION('ref_axis',(0.219289691904165,0.000828887532608173,-0.975659440568293));
#91251=DIRECTION('center_axis',(0.140147588783667,-0.987363721370841,0.0739698254617974));
#91252=DIRECTION('ref_axis',(0.366070013200346,-0.0177432466485635,-0.930418143972841));
#91253=DIRECTION('center_axis',(0.156429984571215,0.987363722264396,0.0253483704258555));
#91254=DIRECTION('ref_axis',(0.0818182164522016,0.0126220312518529,-0.996567340315574));
#91255=DIRECTION('',(0.56236740413906,0.,0.82688747890018));
#91256=DIRECTION('center_axis',(2.60560789866602E-15,1.,-3.26710515559638E-14));
#91257=DIRECTION('ref_axis',(7.18875342422977E-33,3.26710515559638E-14,
1.));
#91258=DIRECTION('center_axis',(-0.168098486533422,-0.982569637630382,-0.0793713174394452));
#91259=DIRECTION('ref_axis',(0.269198093291677,0.0317006521827105,-0.962562961690983));
#91260=DIRECTION('center_axis',(0.,-1.,-3.78747958921603E-15));
#91261=DIRECTION('ref_axis',(0.,-3.78747958921603E-15,1.));
#91262=DIRECTION('center_axis',(0.178655412465466,-0.98367345523271,-0.0216512601789133));
#91263=DIRECTION('ref_axis',(-0.0800267183951851,0.00740491324750828,-0.996765213880729));
#91264=DIRECTION('center_axis',(-0.15736997128655,0.987363722472243,-0.0186432744716927));
#91265=DIRECTION('ref_axis',(0.00712353035048156,-0.0177430427862771,-0.999817203166674));
#91266=DIRECTION('',(0.68666294091143,0.,-0.726975931911687));
#91267=DIRECTION('center_axis',(-2.95940006317246E-16,-1.,3.69965289557878E-15));
#91268=DIRECTION('ref_axis',(3.22728447839295E-34,-3.69965289557878E-15,
-1.));
#91269=DIRECTION('center_axis',(-0.158463140916245,-0.987363724157911,-0.00151960125661887));
#91270=DIRECTION('ref_axis',(0.00442488112967827,0.000828879242715846,-0.999989866641752));
#91271=DIRECTION('center_axis',(0.152772346096398,-0.987363722316901,0.0421128260832276));
#91272=DIRECTION('ref_axis',(0.157499094830202,-0.017743210008238,-0.987359718454359));
#91273=DIRECTION('center_axis',(0.158221889065703,0.987363722232188,-0.0088720820712651));
#91274=DIRECTION('ref_axis',(-0.134327168570016,0.0126220323727302,-0.990856647594769));
#91275=DIRECTION('',(0.726975931972861,0.,0.686662940846665));
#91276=DIRECTION('center_axis',(-8.9572421130411E-15,1.,-6.49347121175939E-14));
#91277=DIRECTION('ref_axis',(-4.34106576186858E-32,6.49347121175939E-14,
1.));
#91278=DIRECTION('center_axis',(-0.181230912891191,-0.982569629730098,-0.0413796924189044));
#91279=DIRECTION('ref_axis',(0.0559818735015593,0.0317008821641159,-0.99792839618345));
#91280=DIRECTION('center_axis',(0.,-1.,-1.48029736755923E-14));
#91281=DIRECTION('ref_axis',(0.,-1.48029736755923E-14,1.));
#91282=DIRECTION('center_axis',(0.169824197772912,-0.98367345564293,-0.0595506046508672));
#91283=DIRECTION('ref_axis',(-0.292430796806876,0.00740481273193738,-0.956258018438173));
#91284=DIRECTION('center_axis',(-0.157698501543129,0.987363722479201,0.0156224883762656));
#91285=DIRECTION('ref_axis',(-0.207974158912054,-0.0177430414407734,-0.977973380877647));
#91286=DIRECTION('',(0.514330810099969,0.,-0.857591871336191));
#91287=DIRECTION('center_axis',(2.02517967483958E-15,-1.,1.47071016964003E-14));
#91288=DIRECTION('ref_axis',(1.07744368455052E-32,-1.47071016964003E-14,
-1.));
#91289=DIRECTION('center_axis',(-0.155085103499708,-0.987363723836278,0.0325804776613727));
#91290=DIRECTION('ref_axis',(-0.210646778580884,0.00082922245084035,-0.977561889121923));
#91291=DIRECTION('center_axis',(0.158253630647629,-0.987363721274912,0.00828675431046068));
#91292=DIRECTION('ref_axis',(-0.0584362933306146,-0.0177432508835518,-0.998133446323617));
#91293=DIRECTION('center_axis',(0.152615513172385,0.987363722259592,-0.0426776886067419));
#91294=DIRECTION('ref_axis',(-0.344191563026183,0.0126220303639586,-0.938814599530218));
#91295=DIRECTION('',(0.85759187372498,0.,0.514330806116917));
#91296=DIRECTION('center_axis',(-4.54137237097151E-14,1.,-1.2298201840572E-13));
#91297=DIRECTION('ref_axis',(3.20542588349696E-31,1.2298201840572E-13,1.));
#91298=DIRECTION('center_axis',(-0.185889240027947,-0.982569630822743,-0.00145293726336171));
#91299=DIRECTION('ref_axis',(-0.159852068098868,0.0317008511488114,-0.986631832225656));
#91300=DIRECTION('center_axis',(0.,-1.,-1.15792791941926E-14));
#91301=DIRECTION('ref_axis',(0.,-1.15792791941926E-14,1.));
#91302=DIRECTION('center_axis',(0.153051994296784,-0.983673454167874,-0.0946658471003188));
#91303=DIRECTION('ref_axis',(-0.491161130555647,0.00740519063348927,-0.871037259239224));
#91304=DIRECTION('center_axis',(-0.150653226017932,0.987363722442911,0.0491577572115231));
#91305=DIRECTION('ref_axis',(-0.413347207736676,-0.017743044202828,-0.910400609753041));
#91306=DIRECTION('',(0.31794913860653,0.,-0.948107770909703));
#91307=DIRECTION('center_axis',(-1.28485605524992E-15,-1.,-3.48197601383281E-15));
#91308=DIRECTION('ref_axis',(-2.47587532992437E-33,3.48197601383282E-15,
-1.));
#91309=DIRECTION('center_axis',(-0.144455314496109,-0.987363724113352,0.0651577963013036));
#91310=DIRECTION('ref_axis',(-0.415868934776334,0.000828876094051006,-0.909424181585479));
#91311=DIRECTION('center_axis',(0.156335142091041,-0.987363722370261,-0.0259268797682325));
#91312=DIRECTION('ref_axis',(-0.271639278391324,-0.0177432074989289,-0.962235564205923));
#91313=DIRECTION('center_axis',(0.139873008188529,0.987363722211361,-0.0744877281249552));
#91314=DIRECTION('ref_axis',(-0.537961943085501,0.0126220349637511,-0.8428746241435));
#91315=DIRECTION('',(0.948107772469132,0.,0.317949133956394));
#91316=DIRECTION('center_axis',(-5.30921149349349E-14,1.,-8.27581331014178E-14));
#91317=DIRECTION('ref_axis',(-2.7805240325011E-31,8.27581331014178E-14,
1.));
#91318=DIRECTION('center_axis',(-0.181855215515493,-0.982569664512228,0.0385426383391284));
#91319=DIRECTION('ref_axis',(-0.368211691435434,0.0316998820363428,-0.929201413994371));
#91320=DIRECTION('center_axis',(0.,-1.,-3.78747958921603E-15));
#91321=DIRECTION('ref_axis',(0.,-3.78747958921603E-15,1.));
#91322=DIRECTION('center_axis',(0.129123558039704,-0.983673455292137,-0.125354059020023));
#91323=DIRECTION('ref_axis',(-0.666925320249561,0.00740490243755575,-0.74508776974925));
#91324=DIRECTION('center_axis',(-0.136563572509073,0.987363722456192,0.0803944664825342));
#91325=DIRECTION('ref_axis',(-0.599392598698392,-0.0177430439695527,-0.800258518865175));
#91326=DIRECTION('',(0.106700517422838,0.,-0.994291204618495));
#91327=DIRECTION('center_axis',(1.40233712663849E-14,-1.,2.18705429551819E-14));
#91328=DIRECTION('ref_axis',(-2.0037589829547E-32,-2.18705429551819E-14,
-1.));
#91329=DIRECTION('center_axis',(-0.127071029273013,-0.987363724119497,0.0946880658392329));
#91330=DIRECTION('ref_axis',(-0.601645467602814,0.000828876144709256,-0.79876282104097));
#91331=DIRECTION('center_axis',(0.147106623059428,-0.987363721277475,-0.0589281202580531));
#91332=DIRECTION('ref_axis',(-0.472140697430878,-0.0177432505213094,-0.881344619822701));
#91333=DIRECTION('',(0.994291204851001,0.,0.106700515256233));
#91334=DIRECTION('center_axis',(0.120590197321115,0.987363722182783,-0.102814806460033));
#91335=DIRECTION('ref_axis',(-0.706577819713666,0.0126220377017149,-0.707522769140992));
#91336=DIRECTION('center_axis',(0.,1.,0.));
#91337=DIRECTION('ref_axis',(0.,0.,1.));
#91338=DIRECTION('center_axis',(-0.169318498668954,-0.982569635474812,0.0767343303312521));
#91339=DIRECTION('ref_axis',(-0.559353793109933,0.0317007163076125,-0.828322641679626));
#91340=DIRECTION('center_axis',(-2.38609880511614E-28,-1.,1.16804714017285E-14));
#91341=DIRECTION('ref_axis',(-2.04281036531029E-14,1.16804714017285E-14,
1.));
#91342=DIRECTION('center_axis',(0.0991572193433959,-0.983673454833043,-0.150181157636075));
#91343=DIRECTION('ref_axis',(-0.811504822713002,0.00740500677956439,-0.584298800775882));
#91344=DIRECTION('center_axis',(-0.116088355566142,0.987363722501146,0.107872022279315));
#91345=DIRECTION('ref_axis',(-0.757411059269865,-0.017743040388858,-0.652697228286945));
#91346=DIRECTION('',(-0.109537300692827,0.,-0.993982685843636));
#91347=DIRECTION('center_axis',(5.25629510911856E-15,-1.,5.24131757556537E-15));
#91348=DIRECTION('ref_axis',(1.,5.25629510911856E-15,2.9872547149238E-32));
#91349=DIRECTION('center_axis',(-0.103745042602045,-0.987363724129464,0.119790827731908));
#91350=DIRECTION('ref_axis',(-0.75928972628638,0.000828874316998394,-0.650752199015356));
#91351=DIRECTION('center_axis',(0.130999520502375,-0.987363722264207,-0.0891740185520346));
#91352=DIRECTION('ref_axis',(-0.650565357517768,-0.0177432109538035,-0.759242974325629));
#91353=DIRECTION('center_axis',(0.0956687178831353,0.987363722223788,-0.126334383502603));
#91354=DIRECTION('ref_axis',(-0.842154904346286,0.0126220335947149,-0.539087934713282));
#91355=DIRECTION('',(0.993982685952451,0.,-0.109537299705404));
#91356=DIRECTION('center_axis',(8.29343359167699E-14,1.,5.28164464733621E-14));
#91357=DIRECTION('ref_axis',(-1.,8.293433591677E-14,3.76666855861367E-31));
#91358=DIRECTION('center_axis',(-0.148864271522895,-0.982569637327251,0.11133883629063));
#91359=DIRECTION('ref_axis',(-0.724341307884093,0.0317006605829815,-0.688712376693903));
#91360=DIRECTION('center_axis',(-7.06431103601238E-29,-1.,-3.78747958921603E-15));
#91361=DIRECTION('ref_axis',(1.86517468137026E-14,-3.78747958921603E-15,
1.));
#91362=DIRECTION('center_axis',(0.0645545855673779,-0.983673455399648,-0.167985828641407));
#91363=DIRECTION('ref_axis',(-0.918139262285609,0.00740487866414407,-0.396188670738585));
#91364=DIRECTION('center_axis',(-0.0901849778030904,0.987363722478745,0.130305599693841));
#91365=DIRECTION('ref_axis',(-0.880013820330849,-0.0177430398882603,-0.474616540548502));
#91366=DIRECTION('',(-0.320653274273476,0.,-0.947196641515213));
#91367=DIRECTION('center_axis',(6.26013419967124E-15,-1.,3.98883041207536E-15));
#91368=DIRECTION('ref_axis',(1.,6.26013419967124E-15,-2.68710427983303E-33));
#91369=DIRECTION('center_axis',(-0.075568076442598,-0.987363724119251,0.139292290225014));
#91370=DIRECTION('ref_axis',(-0.881430438857171,0.000828899162159362,-0.472313131706323));
#91371=DIRECTION('center_axis',(0.108767073254341,-0.98736372146031,-0.115250185768753));
#91372=DIRECTION('ref_axis',(-0.798570293939769,-0.0177432430057322,-0.601639977864329));
#91373=DIRECTION('center_axis',(0.0662738822247929,0.987363722186029,-0.143946700711773));
#91374=DIRECTION('ref_axis',(-0.938353761552175,0.0126220379022938,-0.345445947059849));
#91375=DIRECTION('',(0.947196640816497,0.,-0.320653276337453));
#91376=DIRECTION('center_axis',(3.07831179698849E-14,1.,1.12510657658258E-14));
#91377=DIRECTION('ref_axis',(-1.,3.07831179698849E-14,3.56206623346533E-32));
#91378=DIRECTION('center_axis',(-0.121449338297179,-0.982569637779582,0.140737220168932));
#91379=DIRECTION('ref_axis',(-0.855459416436917,0.0317006491305122,-0.516898689952018));
#91380=DIRECTION('center_axis',(0.,-1.,-1.46295013157071E-14));
#91381=DIRECTION('ref_axis',(0.,-1.46295013157071E-14,1.));
#91382=DIRECTION('center_axis',(0.0269333624616044,-0.983673455422475,-0.177935738635387));
#91383=DIRECTION('ref_axis',(-0.981842529371897,0.00740486370994217,-0.18955319968292));
#91384=DIRECTION('center_axis',(-0.0600646491167124,0.987363722533973,0.146646231967762));
#91385=DIRECTION('ref_axis',(-0.961468112563275,-0.0177430377158196,-0.274343312542203));
#91386=DIRECTION('',(-0.516775858941057,0.,-0.856120734251737));
#91387=DIRECTION('center_axis',(-2.43993972821388E-14,-1.,-8.92440488461752E-15));
#91388=DIRECTION('ref_axis',(1.,-2.43993972821388E-14,2.12366322857769E-32));
#91389=DIRECTION('center_axis',(-0.0438576345564159,-0.987363724127006,
0.152280609957948));
#91390=DIRECTION('ref_axis',(-0.962356445818495,0.000828922493000271,-0.271789227305084));
#91391=DIRECTION('center_axis',(0.081448785342375,-0.987363721224333,-0.135937402418504));
#91392=DIRECTION('ref_axis',(-0.909234973830211,-0.0177432523881513,-0.415904964335202));
#91393=DIRECTION('center_axis',(0.0337801471428685,0.987363722229621,-0.154828232838441));
#91394=DIRECTION('ref_axis',(-0.990676239327606,0.0126220348238584,-0.135651292174523));
#91395=DIRECTION('',(0.856120733893417,0.,-0.51677585953467));
#91396=DIRECTION('center_axis',(2.27374502308751E-13,1.,3.0593931262345E-14));
#91397=DIRECTION('ref_axis',(-1.,2.27374502308751E-13,1.1524214611489E-31));
#91398=DIRECTION('center_axis',(-0.0883550911670293,-0.982569655107274,
0.163555038831696));
#91399=DIRECTION('ref_axis',(-0.946577232895948,0.0317001444348233,-0.320915320615675));
#91400=DIRECTION('center_axis',(0.,-1.,-3.78747958921603E-15));
#91401=DIRECTION('ref_axis',(0.,-3.78747958921603E-15,1.));
#91402=DIRECTION('center_axis',(-0.0119472795883105,-0.983673455333531,
-0.179565575160247));
#91403=DIRECTION('ref_axis',(-0.999635931190591,0.0074048951126651,0.02594556997045));
#91404=DIRECTION('center_axis',(-0.027135769578797,0.987363722495344,0.15612984823378));
#91405=DIRECTION('ref_axis',(-0.997965224992306,-0.0177430414057831,-0.0612420948999103));
#91406=DIRECTION('',(-0.688734576602034,0.,-0.725013574350727));
#91407=DIRECTION('center_axis',(-1.83910258353765E-14,-1.,-2.47900577328738E-15));
#91408=DIRECTION('ref_axis',(1.,-1.83910258353765E-14,-7.33039533389768E-33));
#91409=DIRECTION('center_axis',(-0.0100963937174092,-0.9873637241587,0.158148471536609));
#91410=DIRECTION('ref_axis',(-0.998283737173725,0.000828878972048249,-0.0585567507133987));
#91411=DIRECTION('center_axis',(0.0503219923558111,-0.987363722299207,-0.150268349870476));
#91412=DIRECTION('ref_axis',(-0.97738484116564,-0.0177432102047794,-0.210722686845167));
#91413=DIRECTION('center_axis',(-0.000293106042224026,0.987363722206634,
-0.158470168041525));
#91414=DIRECTION('ref_axis',(-0.996675797363578,0.0126220360918558,0.0804862668693937));
#91415=DIRECTION('',(0.725013572849968,0.,-0.688734578181845));
#91416=DIRECTION('center_axis',(-1.30648829703912E-13,1.,1.08572221678296E-14));
#91417=DIRECTION('ref_axis',(-1.,-1.30648829703912E-13,-5.11450308930103E-32));
#91418=DIRECTION('center_axis',(-0.0511306135194889,-0.98256963095643,0.178724874271229));
#91419=DIRECTION('ref_axis',(-0.993434052898061,0.0317008474190799,-0.109926515524896));
#91420=DIRECTION('center_axis',(0.,-1.,-5.37764278031254E-15));
#91421=DIRECTION('ref_axis',(0.,-5.37764278031254E-15,1.));
#91422=DIRECTION('center_axis',(-0.0502691671596196,-0.983673455672302,
-0.172799141892518));
#91423=DIRECTION('ref_axis',(-0.970687468112846,0.00740480799607863,0.240231155488238));
#91424=DIRECTION('center_axis',(0.0070619506335549,0.987363722459408,0.158313007754735));
#91425=DIRECTION('ref_axis',(-0.987798592664615,-0.0177430426809696,0.154722735130385));
#91426=DIRECTION('',(-0.828488831038146,0.,-0.560005586440927));
#91427=DIRECTION('center_axis',(1.10963801102532E-14,-1.,-9.19487355021671E-16));
#91428=DIRECTION('ref_axis',(1.,1.10963801102532E-14,-5.37912607381295E-33));
#91429=DIRECTION('center_axis',(0.0241365891185764,-0.987363723876408,0.156621524186918));
#91430=DIRECTION('ref_axis',(-0.98753239609518,0.00082919088419808,0.157413719557698));
#91431=DIRECTION('center_axis',(0.0168422735472509,-0.987363721427545,-0.157572901954963));
#91432=DIRECTION('ref_axis',(-0.999833274907587,-0.0177432441231643,0.00431273411593884));
#91433=DIRECTION('center_axis',(-0.0343526576847958,0.98736372221655,-0.154702213819554));
#91434=DIRECTION('ref_axis',(-0.956071902708856,0.0126220335741101,0.292860378199444));
#91435=DIRECTION('',(0.560005583301831,0.,-0.828488833159975));
#91436=DIRECTION('center_axis',(3.1315081560836E-14,1.,-9.67225379250271E-15));
#91437=DIRECTION('ref_axis',(-1.,3.1315081560836E-14,2.24514060136425E-32));
#91438=DIRECTION('center_axis',(-0.0115144350220054,-0.982569637967496,
0.185537932322604));
#91439=DIRECTION('ref_axis',(-0.993839068512918,0.0317006448509257,0.106202518865662));
#91440=DIRECTION('center_axis',(0.,-1.,-3.33934269153158E-15));
#91441=DIRECTION('ref_axis',(0.,-3.33934269153158E-15,1.));
#91442=DIRECTION('center_axis',(-0.0862406661628375,-0.983673455403097,
-0.157952779763834));
#91443=DIRECTION('ref_axis',(-0.896350737297868,0.00740487292010241,0.44328379578167));
#91444=DIRECTION('center_axis',(0.0409294624178168,0.987363722466824,0.1530936271131));
#91445=DIRECTION('ref_axis',(-0.931443596256056,-0.0177430432852071,0.363452901224581));
#91446=DIRECTION('',(-0.929503870801002,0.,-0.368812356308672));
#91447=DIRECTION('center_axis',(0.,-1.,0.));
#91448=DIRECTION('ref_axis',(0.,0.,-1.));
#91449=DIRECTION('center_axis',(0.0572415509645948,-0.987363724119703,0.147771042953751));
#91450=DIRECTION('ref_axis',(-0.930605124983861,0.000828910731059022,0.366023789200609));
#91451=DIRECTION('center_axis',(-0.0174250074421581,-0.987363721465215,
-0.157509525584966));
#91452=DIRECTION('ref_axis',(-0.97553061766179,-0.0177432425678975,0.219146506583115));
#91453=DIRECTION('center_axis',(-0.0668059115608627,0.987363722212296,-0.143700557547988));
#91454=DIRECTION('ref_axis',(-0.870763148687641,0.0126220369484988,0.491540662683014));
#91455=DIRECTION('',(0.368812355268781,0.,-0.929503871213614));
#91456=DIRECTION('center_axis',(-1.14014813092713E-13,1.,6.47117539700905E-14));
#91457=DIRECTION('ref_axis',(-1.,-1.14014813092713E-13,-1.69361705489593E-31));
#91458=DIRECTION('center_axis',(0.0286403209154908,-0.982569651704975,0.183675288392918));
#91459=DIRECTION('ref_axis',(-0.94777325181453,0.0317002440392639,0.317365652950603));
#91460=DIRECTION('center_axis',(-2.01837458171782E-29,-1.,-3.78747958921603E-15));
#91461=DIRECTION('ref_axis',(5.32907051820075E-15,-3.78747958921603E-15,
1.));
#91462=DIRECTION('center_axis',(-0.118179585967429,-0.983673455420277,-0.13572073740626));
#91463=DIRECTION('ref_axis',(-0.780101643914051,0.00740487350271539,0.625608977725706));
#91464=DIRECTION('center_axis',(0.0728831627478859,0.987363722498741,0.140715756336291));
#91465=DIRECTION('ref_axis',(-0.831535330925473,-0.0177430390696153,0.555188416654417));
#91466=DIRECTION('',(-0.987056341019165,0.,-0.160373874598885));
#91467=DIRECTION('center_axis',(1.61411985227139E-14,-1.,-9.15625532613643E-15));
#91468=DIRECTION('ref_axis',(1.,1.61411985227139E-14,-5.66390648337493E-32));
#91469=DIRECTION('center_axis',(0.0876697142084478,-0.987363724095884,0.132010975112361));
#91470=DIRECTION('ref_axis',(-0.830163795586117,0.000828872077927888,0.557518955255452));
#91471=DIRECTION('center_axis',(-0.0508775087218593,-0.987363721389257,
-0.150081180667713));
#91472=DIRECTION('ref_axis',(-0.905613234397984,-0.0177432462315155,0.423733226094427));
#91473=DIRECTION('center_axis',(-0.0961353978983087,0.987363722178085,-0.125979622945822));
#91474=DIRECTION('ref_axis',(-0.744738477439971,0.0126220380236425,0.667237052610632));
#91475=DIRECTION('',(0.160373869647189,0.,-0.987056341823701));
#91476=DIRECTION('center_axis',(1.46157135101623E-13,1.,-1.31562957702813E-13));
#91477=DIRECTION('ref_axis',(-1.,1.46157135101623E-13,5.63522651253288E-32));
#91478=DIRECTION('center_axis',(0.0674550899212748,-0.982569636071288,0.173224481856493));
#91479=DIRECTION('ref_axis',(-0.85739063654192,0.0317006985960046,0.513688974067739));
#91480=DIRECTION('center_axis',(0.,-1.,-9.12175427525787E-15));
#91481=DIRECTION('ref_axis',(0.,-9.12175427525787E-15,1.));
#91482=DIRECTION('center_axis',(-0.144592641615338,-0.983673454856816,-0.107142438840795));
#91483=DIRECTION('ref_axis',(-0.627375861967964,0.00740500910540536,0.778681381349332));
#91484=DIRECTION('center_axis',(0.101428920968401,0.987363722463645,0.121758176538255));
#91485=DIRECTION('ref_axis',(-0.692745400955484,-0.0177430414082981,0.720963933866743));
#91486=DIRECTION('',(-0.998455154553505,3.11688535425711E-16,0.055563516317241));
#91487=DIRECTION('center_axis',(1.37955020419649E-14,-1.,-1.24120677249046E-14));
#91488=DIRECTION('ref_axis',(1.,1.37955020419649E-14,5.52387648803174E-32));
#91489=DIRECTION('center_axis',(0.11399850328062,-0.987363724090544,0.110078233996695));
#91490=DIRECTION('ref_axis',(-0.690904932361026,0.000828870840717851,0.722945148273599));
#91491=DIRECTION('center_axis',(-0.0819510668801886,-0.987363722305634,
-0.135635181689564));
#91492=DIRECTION('ref_axis',(-0.793350377678185,-0.0177432098191626,0.608506661215138));
#91493=DIRECTION('center_axis',(-0.120969701972986,0.987363722185803,-0.102368019009666));
#91494=DIRECTION('ref_axis',(-0.583890661941005,0.0126220361724893,0.811734180074336));
#91495=DIRECTION('',(-0.0555635156269576,0.,-0.998455154591919));
#91496=DIRECTION('center_axis',(-1.90763212459409E-14,1.,2.66510948801363E-14));
#91497=DIRECTION('ref_axis',(-6.7895573354269E-32,-2.66510948801363E-14,
1.));
#91498=DIRECTION('center_axis',(0.10311612646859,-0.982569634025935,0.154673781722226));
#91499=DIRECTION('ref_axis',(-0.726917383075444,0.0317007582126674,0.68599284260952));
#91500=DIRECTION('center_axis',(0.,-1.,-4.5247370677682E-15));
#91501=DIRECTION('ref_axis',(0.,-4.5247370677682E-15,1.));
#91502=DIRECTION('center_axis',(-0.164244541101588,-0.983673455463523,-0.0735544950005185));
#91503=DIRECTION('ref_axis',(-0.445314682867744,0.00740486179507685,0.895343510192706));
#91504=DIRECTION('center_axis',(0.125231976596983,0.987363722472282,0.0971073199264145));
#91505=DIRECTION('ref_axis',(-0.521563464398509,-0.0177430435487255,0.853027981375906));
#91506=DIRECTION('',(-0.963167314504198,3.11688536629873E-16,0.268902815661666));
#91507=DIRECTION('center_axis',(-4.32189727882296E-15,-1.,6.03500224482245E-15));
#91508=DIRECTION('ref_axis',(-2.95538501758547E-32,-6.03500224482245E-15,
-1.));
#91509=DIRECTION('center_axis',(0.134996780744609,-0.98736372407516,0.0829984672691258));
#91510=DIRECTION('ref_axis',(-0.519340140134093,0.000828997761539845,0.854567218893992));
#91511=DIRECTION('center_axis',(-0.109192627375346,-0.987363721318639,-0.114847080723355));
#91512=DIRECTION('ref_axis',(-0.643991344872343,-0.0177432487589253,0.76482699014417));
#91513=DIRECTION('center_axis',(-0.140147596738918,0.987363722235712,-0.0739697988448428));
#91514=DIRECTION('ref_axis',(-0.395740769540629,0.0126220331102005,0.918275518351413));
#91515=DIRECTION('',(-0.268902817760427,0.,-0.963167313918253));
#91516=DIRECTION('center_axis',(-1.29011271314033E-14,1.,3.01288458702476E-14));
#91517=DIRECTION('ref_axis',(3.29010680199035E-32,-3.01288458702476E-14,
1.));
#91518=DIRECTION('center_axis',(0.133955574882366,-0.982569631427832,0.128890741923958));
#91519=DIRECTION('ref_axis',(-0.562454294716541,0.0317008349676485,0.826220444807118));
#91520=DIRECTION('center_axis',(0.,-1.,7.19910242023359E-15));
#91521=DIRECTION('ref_axis',(0.,7.19910242023359E-15,1.));
#91522=DIRECTION('center_axis',(-0.176216709575444,-0.983673454206282,-0.036526795045364));
#91523=DIRECTION('ref_axis',(-0.24243108626749,0.00740519116528956,0.970140366934069));
#91524=DIRECTION('center_axis',(0.143179326339322,0.987363722466588,0.0679158307461498));
#91525=DIRECTION('ref_axis',(-0.325993799946702,-0.0177430425423517,0.94520538870536));
#91526=DIRECTION('',(-0.882842841300016,0.,0.469668518814402));
#91527=DIRECTION('center_axis',(1.31557798442278E-14,-1.,-3.07034433151806E-14));
#91528=DIRECTION('ref_axis',(1.5289773705897E-32,3.07034433151806E-14,-1.));
#91529=DIRECTION('center_axis',(0.149682890516781,-0.987363724091402,0.0520375694561118));
#91530=DIRECTION('ref_axis',(-0.323491544844115,0.000828869996302542,0.946230697762917));
#91531=DIRECTION('center_axis',(-0.13132850894257,-0.987363722349457,-0.0886887959504751));
#91532=DIRECTION('ref_axis',(-0.464519985807728,-0.0177432087395852,0.885384866218534));
#91533=DIRECTION('center_axis',(-0.152772343819054,0.987363722231284,-0.0421128363520662));
#91534=DIRECTION('ref_axis',(-0.189086478016743,0.01262203398202,0.981879314421778));
#91535=DIRECTION('',(-0.469668518497478,0.,-0.882842841468619));
#91536=DIRECTION('center_axis',(3.67361741914096E-14,1.,-1.93186898753132E-13));
#91537=DIRECTION('ref_axis',(-1.78965190703203E-31,1.93186898753132E-13,
1.));
#91538=DIRECTION('center_axis',(0.158531736849135,-0.982569656573641,0.0970801647730095));
#91539=DIRECTION('ref_axis',(-0.371691321544402,0.0317001055356064,0.927814994919573));
#91540=DIRECTION('center_axis',(0.,-1.,-3.78747958921603E-15));
#91541=DIRECTION('ref_axis',(0.,-3.78747958921603E-15,1.));
#91542=DIRECTION('center_axis',(-0.179949039173256,-0.983673455413316,0.00220826081986253));
#91543=DIRECTION('ref_axis',(-0.0282116802862476,0.00740488220223463,0.999574543901053));
#91544=DIRECTION('center_axis',(0.154431769493381,0.987363722487946,0.035548672069278));
#91545=DIRECTION('ref_axis',(-0.11518102602311,-0.017743041274024,0.993186042859349));
#91546=DIRECTION('',(-0.761237618626322,0.,0.648473043378155));
#91547=DIRECTION('center_axis',(-1.38841606632461E-15,-1.,7.29193725991163E-15));
#91548=DIRECTION('ref_axis',(-8.46747865150748E-33,-7.29193725991163E-15,
-1.));
#91549=DIRECTION('center_axis',(0.157369926272718,-0.987363724124777,0.0186435669165276));
#91550=DIRECTION('ref_axis',(-0.112516862267976,0.000828873940512268,0.993649469719257));
#91551=DIRECTION('center_axis',(-0.147323582410273,-0.987363721358974,-0.0583835919583681));
#91552=DIRECTION('ref_axis',(-0.263328199075575,-0.017743247115542,0.96454312332493));
#91553=DIRECTION('center_axis',(-7.5362264330552E-15,1.,-2.62089983140031E-13));
#91554=DIRECTION('ref_axis',(-2.13409324614581E-32,2.62089983140031E-13,
1.));
#91555=DIRECTION('center_axis',(0.175694642098467,-0.982569639383468,0.0607313469283601));
#91556=DIRECTION('ref_axis',(-0.163548662564118,0.0317006050560886,0.986025814374333));
#91557=DIRECTION('center_axis',(-3.36395763619637E-30,-1.,-3.78747958921603E-15));
#91558=DIRECTION('ref_axis',(8.88178419700125E-16,-3.78747958921603E-15,
1.));
#91559=DIRECTION('center_axis',(-0.17526714169692,-0.983673452813486,0.040840755029578));
#91560=DIRECTION('ref_axis',(0.187326942949257,0.00740528131793076,0.982269707490712));
#91561=DIRECTION('center_axis',(-4.23190585545145E-16,-1.,-1.48398484630621E-14));
#91562=DIRECTION('ref_axis',(0.0285055883760776,-1.48458813372039E-14,0.999593633148658));
#91563=DIRECTION('center_axis',(0.157698522826405,-0.987363724124184,-0.0156221695673659));
#91564=DIRECTION('ref_axis',(0.103718979496377,0.000828895785446709,0.994606297096498));
#91565=DIRECTION('center_axis',(-0.158253626383321,0.987363722223235,-0.00828672275433531));
#91566=DIRECTION('ref_axis',(0.0264092846868512,0.0126220326853917,0.999571525191278));
#91567=DIRECTION('center_axis',(-0.156429985617351,-0.987363722284086,-0.0253483632029913));
#91568=DIRECTION('ref_axis',(-0.0498234664665366,-0.0177432101527035,0.998600420930582));
#91569=DIRECTION('',(-0.64847304670282,0.,-0.76123761579415));
#91570=DIRECTION('center_axis',(0.,1.,0.));
#91571=DIRECTION('ref_axis',(1.,0.,0.));
#91572=DIRECTION('center_axis',(0.987464241017343,0.151612438471943,-0.0439094660936956));
#91573=DIRECTION('ref_axis',(0.0466366821965845,-0.0144775320618018,0.998806998843668));
#91574=DIRECTION('center_axis',(0.162375657399389,-0.986495109627198,-0.0214835882882429));
#91575=DIRECTION('ref_axis',(0.0319374621849617,-0.0165067558142742,0.999353553814501));
#91576=DIRECTION('center_axis',(-0.163746575713113,-0.986495111104823,0.00380193483800228));
#91577=DIRECTION('ref_axis',(0.133383938187138,-0.018321271348547,0.990895078224664));
#91578=DIRECTION('center_axis',(-0.954918750289514,-0.151717240595822,0.255170647315678));
#91579=DIRECTION('ref_axis',(0.265259226515505,-0.0501190367766773,0.962873628728596));
#91580=DIRECTION('center_axis',(0.15396106861831,-0.986495109630634,-0.055887279632775));
#91581=DIRECTION('ref_axis',(0.246022253877083,-0.0165067551769565,0.969123613183978));
#91582=DIRECTION('center_axis',(-0.159100969103341,-0.986495111013762,0.0389137196413171));
#91583=DIRECTION('ref_axis',(0.343278644332733,-0.0183212726723349,0.939054898987672));
#91584=DIRECTION('center_axis',(-0.877738926131253,-0.151718219821126,0.454484278417046));
#91585=DIRECTION('ref_axis',(0.466046492607051,-0.050113017262808,0.883339884885475));
#91586=DIRECTION('center_axis',(0.138347432677136,-0.986495109670028,-0.0876777421513839));
#91587=DIRECTION('ref_axis',(0.448603321542154,-0.0165067518838875,0.893578528750322));
#91588=DIRECTION('center_axis',(-0.147015974375736,-0.986495111209942,0.0722059473813417));
#91589=DIRECTION('ref_axis',(0.537122028018301,-0.01832126851174,0.843305554433047));
#91590=DIRECTION('center_axis',(-0.759517343082594,-0.151717542940859,0.632546593320007));
#91591=DIRECTION('ref_axis',(0.645042837663815,-0.0501177349543966,0.76250111489863));
#91592=DIRECTION('center_axis',(0.116264825694713,-0.986495109676388,-0.115368491759009));
#91593=DIRECTION('ref_axis',(0.63020819332302,-0.0165067493985915,0.77625070711261));
#91594=DIRECTION('center_axis',(-0.128056682568447,-0.986495111049509,0.1021218973824));
#91595=DIRECTION('ref_axis',(0.705850176713648,-0.0183212736053562,0.708124183294703));
#91596=DIRECTION('center_axis',(-0.605781406098869,-0.151717652691486,0.781031780330776));
#91597=DIRECTION('ref_axis',(0.793877240007919,-0.0501164462036934,0.606009298292791));
#91598=DIRECTION('center_axis',(0.088745798476136,-0.98649510963067,-0.13766474467926));
#91599=DIRECTION('ref_axis',(0.782345232961454,-0.0165067550744596,0.622626263098017));
#91600=DIRECTION('center_axis',(-0.103109596717397,-0.986495111163224,0.127262746771532));
#91601=DIRECTION('ref_axis',(0.84157356154396,-0.0183212714890313,0.539831706665364));
#91602=DIRECTION('center_axis',(-0.423719721590489,-0.151718143346513,0.89299675392174));
#91603=DIRECTION('ref_axis',(0.905590981485017,-0.0501174226749332,0.421180742909058));
#91604=DIRECTION('center_axis',(0.0570771178683077,-0.986495109613493,-0.153523943814994));
#91605=DIRECTION('ref_axis',(0.897900677527084,-0.0165067578719576,0.439888508875784));
#91606=DIRECTION('center_axis',(-0.0733412197425735,-0.986495111214254,
0.146452931131635));
#91607=DIRECTION('ref_axis',(0.937945899306877,-0.0183212681314,0.346297301617368));
#91608=DIRECTION('center_axis',(-0.221845691935971,-0.151717064722958,0.963206323298025));
#91609=DIRECTION('ref_axis',(0.97496017035715,-0.0501146364887038,0.216659154957188));
#91610=DIRECTION('center_axis',(0.0227395794411443,-0.986495109631334,-0.162204531996806));
#91611=DIRECTION('ref_axis',(0.971471285321496,-0.0165067549892282,0.236582055184933));
#91612=DIRECTION('center_axis',(-0.0401434924859694,-0.986495111144129,
0.158795137519262));
#91613=DIRECTION('ref_axis',(0.990460928248932,-0.0183212682441811,0.136570424112209));
#91614=DIRECTION('center_axis',(-0.00959814429645489,-0.151717275059204,
0.98837732879436));
#91615=DIRECTION('ref_axis',(0.998741475234698,-0.0501142782739623,0.0020061802260189));
#91616=DIRECTION('center_axis',(-0.0126612359133152,-0.986495109657588,
-0.163300617655936));
#91617=DIRECTION('ref_axis',(0.999616975098312,-0.0165067521155393,0.0222132894884525));
#91618=DIRECTION('center_axis',(-0.00506870264982865,-0.986495111101261,
0.163712259854776));
#91619=DIRECTION('ref_axis',(0.996663106113405,-0.0183212719598163,-0.0795423403361688));
#91620=DIRECTION('center_axis',(0.203098203142765,-0.151717556225375,0.96733288118061));
#91621=DIRECTION('ref_axis',(0.975822735790439,-0.0501139682928271,-0.212740636683284));
#91622=DIRECTION('center_axis',(-0.0474700324896744,-0.986495109609932,
-0.15676094772333));
#91623=DIRECTION('ref_axis',(0.981021686439629,-0.0165067559608459,-0.193194145208377));
#91624=DIRECTION('center_axis',(0.0302430998611894,-0.986495111138674,0.160974378738608));
#91625=DIRECTION('ref_axis',(0.956262424554126,-0.0183212694076787,-0.291935791695976));
#91626=DIRECTION('center_axis',(0.406297869111721,-0.151717737149366,0.901057029154954));
#91627=DIRECTION('ref_axis',(0.907275678259906,-0.0501130613714625,-0.417539848060047));
#91628=DIRECTION('center_axis',(-0.0800591757629436,-0.986495109678747,
-0.14289131168855));
#91629=DIRECTION('ref_axis',(0.916554913499942,-0.0165067516025223,-0.399568038875291));
#91630=DIRECTION('center_axis',(0.0641407687737649,-0.986495111249863,0.150709512842522));
#91631=DIRECTION('ref_axis',(0.871147975542361,-0.0183212658419171,-0.490678648329429));
#91632=DIRECTION('center_axis',(0.59049944203833,-0.151716819930788,0.792648986312674));
#91633=DIRECTION('ref_axis',(0.796304714906656,-0.0501187538296143,-0.602815818913203));
#91634=DIRECTION('center_axis',(-0.108904843684088,-0.986495109715032,-0.12234023675991));
#91635=DIRECTION('ref_axis',(0.809231052919238,-0.0165067504602018,-0.587258571823746));
#91636=DIRECTION('center_axis',(0.0950392811868488,-0.98649511117499,0.133397641131062));
#91637=DIRECTION('ref_axis',(0.745299613138979,-0.0183212695901069,-0.666477919915952));
#91638=DIRECTION('center_axis',(0.747089985754375,-0.151717860052369,0.647177135046238));
#91639=DIRECTION('ref_axis',(0.648100772001506,-0.050112252039179,-0.759904040999003));
#91640=DIRECTION('center_axis',(-0.132658243305986,-0.986495109701146,-0.096068668246692));
#91641=DIRECTION('ref_axis',(0.664068447290981,-0.0165067500876924,-0.747489548096887));
#91642=DIRECTION('center_axis',(0.121493865175172,-0.986495111116229,0.109848242901632));
#91643=DIRECTION('ref_axis',(0.584601872230696,-0.0183212697798802,-0.811113421204469));
#91644=DIRECTION('center_axis',(0.868747407713005,-0.15171756058632,0.471444295120506));
#91645=DIRECTION('ref_axis',(0.469591427508971,-0.050113881662551,-0.881460430237681));
#91646=DIRECTION('center_axis',(-0.150208694183325,-0.986495109644507,-0.0653050292030545));
#91647=DIRECTION('ref_axis',(0.487854736953721,-0.0165067565324189,-0.872768745212955));
#91648=DIRECTION('center_axis',(0.142267532383275,-0.986495111250233,0.0811624587414861));
#91649=DIRECTION('ref_axis',(0.396568795870637,-0.0183212660190013,-0.917822162160608));
#91650=DIRECTION('center_axis',(0.949783202322275,-0.15171717529495,0.273667256548837));
#91651=DIRECTION('ref_axis',(0.269124975424485,-0.0501127201189362,-0.961800635727099));
#91652=DIRECTION('center_axis',(-0.160735548480359,-0.986495109636274,-0.0314878090446884));
#91653=DIRECTION('ref_axis',(0.288829481865451,-0.0165067519944678,-0.957238244923346));
#91654=DIRECTION('center_axis',(0.156388925054862,-0.986495110977077,0.0486816201302798));
#91655=DIRECTION('ref_axis',(0.189992605884798,-0.0183212744051801,-0.98161455806914));
#91656=DIRECTION('center_axis',(0.986408331523745,-0.15171604175971,0.0630939472002521));
#91657=DIRECTION('ref_axis',(0.0560742479695429,-0.0501144507194969,-0.99716810044432));
#91658=DIRECTION('center_axis',(-0.163746588592943,-0.986495109681682,0.00380174937369959));
#91659=DIRECTION('ref_axis',(0.0762988819238041,-0.0165067512497135,-0.99694834759899));
#91660=DIRECTION('center_axis',(0.163197747944136,-0.986495111039129,0.0139244734858598));
#91661=DIRECTION('ref_axis',(-0.0254674285246704,-0.0183212728921532,-0.999507749366633));
#91662=DIRECTION('center_axis',(0.97690981282241,-0.151717025902171,-0.150429922763672));
#91663=DIRECTION('ref_axis',(0.159598986590751,0.0501170508921964,0.985908943406578));
#91664=DIRECTION('center_axis',(-0.159101021139896,-0.986495109712914,0.0389135398640145));
#91665=DIRECTION('ref_axis',(-0.139799366336145,-0.0165067486026133,-0.990042253857169));
#91666=DIRECTION('center_axis',(0.162375622482608,-0.986495111326154,-0.0214837741792473));
#91667=DIRECTION('ref_axis',(-0.239736640226715,-0.0183212636861886,-0.97066506820311));
#91668=DIRECTION('center_axis',(0.921732155192996,-0.15171733944031,-0.356919715057081));
#91669=DIRECTION('ref_axis',(0.367808905001473,0.050116359261509,0.928549923232989));
#91670=DIRECTION('center_axis',(-0.147016065905711,-0.986495109664305,0.0722057821370199));
#91671=DIRECTION('ref_axis',(-0.3493607543486,-0.016506751405448,-0.936842884628482));
#91672=DIRECTION('center_axis',(0.153960995330712,-0.986495111268092,-0.0558874526251794));
#91673=DIRECTION('ref_axis',(-0.44279602738596,-0.0183212658114637,-0.896435167399337));
#91674=DIRECTION('center_axis',(0.823455469926704,-0.151716935206564,-0.546720276393073));
#91675=DIRECTION('ref_axis',(0.558820565354594,0.050117521772302,0.827772800802355));
#91676=DIRECTION('center_axis',(-0.128056801261591,-0.986495109619452,0.102121762360211));
#91677=DIRECTION('ref_axis',(-0.542586422548281,-0.016506754690969,-0.839837782619852));
#91678=DIRECTION('center_axis',(0.138347322118367,-0.98649511126866,-0.0876778986159592));
#91679=DIRECTION('ref_axis',(-0.625150763581123,-0.0183212647737682,-0.780288955484459));
#91680=DIRECTION('center_axis',(0.68667463949011,-0.151717825667281,-0.710956848800207));
#91681=DIRECTION('ref_axis',(0.723702229126702,0.0501140848303044,0.688290390793496));
#91682=DIRECTION('center_axis',(-0.103109741187975,-0.986495109566151,0.12726264209978));
#91683=DIRECTION('ref_axis',(-0.71044135220098,-0.0165067586843161,-0.703562798903254));
#91684=DIRECTION('center_axis',(0.116264690677343,-0.986495110958096,-0.115368616865576));
#91685=DIRECTION('ref_axis',(-0.778274144616829,-0.0183212748608229,-0.627657300370527));
#91686=DIRECTION('center_axis',(0.517785944433882,-0.151717455051538,-0.841949837923494));
#91687=DIRECTION('ref_axis',(0.854744488964346,0.0501132715862331,0.51662415603222));
#91688=DIRECTION('center_axis',(-0.0733413911618107,-0.986495109608882,
0.146452856101237));
#91689=DIRECTION('ref_axis',(-0.845076832735351,-0.016506753357528,-0.534390001653831));
#91690=DIRECTION('center_axis',(0.0887456442096499,-0.986495110967044,-0.137664834550924));
#91691=DIRECTION('ref_axis',(-0.895006294111261,-0.0183212747084494,-0.445677085336778));
#91692=DIRECTION('center_axis',(0.324686099978472,-0.151717310764794,-0.933574203850486));
#91693=DIRECTION('ref_axis',(0.945819951730904,0.0501143506520829,0.320800827253406));
#91694=DIRECTION('center_axis',(-0.0401436795793762,-0.986495109668196,
0.158795099390891));
#91695=DIRECTION('ref_axis',(-0.940197459534588,-0.0165067489361094,-0.340229722870104));
#91696=DIRECTION('center_axis',(0.0570769443776299,-0.986495111169136,-0.153523998319181));
#91697=DIRECTION('ref_axis',(-0.96988894388744,-0.0183212688445451,-0.242857504790015));
#91698=DIRECTION('center_axis',(0.116404160762717,-0.15171785945768,-0.981545598777106));
#91699=DIRECTION('ref_axis',(0.99266997303653,0.0501125960185313,0.109977508391213));
#91700=DIRECTION('center_axis',(-0.00506888908992799,-0.986495109651168,
0.163712262820244));
#91701=DIRECTION('ref_axis',(-0.991355498490221,-0.0165067503541939,-0.130160680721753));
#91702=DIRECTION('center_axis',(0.0227393958052857,-0.986495111211627,-0.162204548129732));
#91703=DIRECTION('ref_axis',(-0.999420664067506,-0.0183212690319746,-0.0286821780191654));
#91704=DIRECTION('center_axis',(-0.0973205419698992,-0.151717505250181,
-0.983621121525634));
#91705=DIRECTION('ref_axis',(0.993103478144611,0.0501177905127186,-0.105989097416662));
#91706=DIRECTION('center_axis',(0.030242922023399,-0.986495109621249,0.160974421449018));
#91707=DIRECTION('ref_axis',(-0.996158856524345,-0.0165067564987743,0.0859945321401235));
#91708=DIRECTION('center_axis',(-0.0126614273468348,-0.986495111313728,
-0.163300592808647));
#91709=DIRECTION('ref_axis',(-0.98222058466164,-0.018321263438133,0.186834296565104));
#91710=DIRECTION('center_axis',(-0.306494682242744,-0.15171728831044,-0.939703609753972));
#91711=DIRECTION('ref_axis',(0.947101109183711,0.0501142032663003,-0.316998510428627));
#91712=DIRECTION('center_axis',(0.0641406002607645,-0.986495109654418,0.150709595003457));
#91713=DIRECTION('ref_axis',(-0.954382933050281,-0.0165067548247208,0.298128737540512));
#91714=DIRECTION('center_axis',(-0.0474702053972094,-0.986495111161419,
-0.156760885600221));
#91715=DIRECTION('ref_axis',(-0.919092961586165,-0.0183212694610228,0.393614607259574));
#91716=DIRECTION('center_axis',(-0.501337540466072,-0.151717802549987,-0.851846452659652));
#91717=DIRECTION('ref_axis',(0.856813384458168,0.0501114100958997,-0.513185805329357));
#91718=DIRECTION('center_axis',(0.0950391340828693,-0.986495109692731,0.133397756896831));
#91719=DIRECTION('ref_axis',(-0.867981124429243,-0.0165067517519525,0.496322772781127));
#91720=DIRECTION('center_axis',(-0.0800593355866944,-0.986495111179507,
-0.142891211781377));
#91721=DIRECTION('ref_axis',(-0.812989574428096,-0.018321268404428,0.581989933757686));
#91722=DIRECTION('center_axis',(-0.672738355704087,-0.151718004685065,-0.724157960543792));
#91723=DIRECTION('ref_axis',(0.726461248877051,0.0501149835492891,-0.685377663995442));
#91724=DIRECTION('center_axis',(0.12149374987299,-0.986495109615189,0.109848383907616));
#91725=DIRECTION('ref_axis',(-0.740993483164264,-0.0165067564236307,0.671309306430696));
#91726=DIRECTION('center_axis',(-0.108904976768055,-0.986495111066147,-0.12234010739631));
#91727=DIRECTION('ref_axis',(-0.668871699073879,-0.0183212724760737,0.743152057894534));
#91728=DIRECTION('center_axis',(-0.812682678127263,-0.151717508345289,-0.562608800440765));
#91729=DIRECTION('ref_axis',(0.562140841754344,0.0501169055115351,-0.825521634976132));
#91730=DIRECTION('center_axis',(0.142267445198958,-0.986495109697153,0.0811626304413822));
#91731=DIRECTION('ref_axis',(-0.579357812530632,-0.0165067500527332,0.814906161629925));
#91732=DIRECTION('center_axis',(-0.132658347439609,-0.986495111193847,-0.0960685091236052));
#91733=DIRECTION('ref_axis',(-0.49347812376278,-0.0183212686064254,0.869565220374077));
#91734=DIRECTION('center_axis',(-0.914626796186742,-0.151718440025845,-0.374752369776762));
#91735=DIRECTION('ref_axis',(0.371535595523368,0.0501154652021563,-0.927065122527359));
#91736=DIRECTION('center_axis',(0.156388880614704,-0.986495109593218,0.0486817909360894));
#91737=DIRECTION('ref_axis',(-0.390632011378624,-0.0165067574930132,0.920398912778235));
#91738=DIRECTION('center_axis',(-0.150208759826364,-0.98649511129442,-0.0653048532931189));
#91739=DIRECTION('ref_axis',(-0.295010059307927,-0.0183212646087627,0.955318478922223));
#91740=DIRECTION('center_axis',(-0.973804122239227,-0.151717542567578,-0.169373311909354));
#91741=DIRECTION('ref_axis',(0.163558175448119,0.0501137165392175,-0.985260036060892));
#91742=DIRECTION('center_axis',(0.163197741587199,-0.986495109592965,0.0139246504444709));
#91743=DIRECTION('ref_axis',(-0.183640690842074,-0.0165067579730875,0.982854833435876));
#91744=DIRECTION('center_axis',(-0.160735575288252,-0.986495110973083,-0.0314876303166706));
#91745=DIRECTION('ref_axis',(-0.0827476582594976,-0.0183212754840253,0.996402105536318));
#91746=DIRECTION('',(-0.727460699689282,0.,-0.686149349928702));
#91747=DIRECTION('center_axis',(-1.25690178608446E-15,1.,-9.080314930603E-15));
#91748=DIRECTION('ref_axis',(-5.55903758767046E-33,9.080314930603E-15,1.));
#91749=DIRECTION('',(-0.513725008301344,0.,0.85795490315388));
#91750=DIRECTION('',(-0.857954900607409,0.,-0.51372501255412));
#91751=DIRECTION('center_axis',(1.05983846877379E-15,1.,2.86594181608156E-15));
#91752=DIRECTION('ref_axis',(-3.99900629564538E-33,-2.86594181608156E-15,
1.));
#91753=DIRECTION('',(-0.317279460074916,0.,0.94833208540815));
#91754=DIRECTION('',(-0.948332083835433,0.,-0.317279464775685));
#91755=DIRECTION('center_axis',(-3.30230561415707E-15,1.,-5.14220749173894E-15));
#91756=DIRECTION('ref_axis',(1.24299482632711E-32,5.14220749173894E-15,
1.));
#91757=DIRECTION('',(-0.105998278540163,0.,0.994366313260119));
#91758=DIRECTION('',(-0.994366313149823,0.,-0.105998279574853));
#91759=DIRECTION('center_axis',(4.33052217016942E-15,1.,4.31208746369059E-15));
#91760=DIRECTION('ref_axis',(-1.,4.33052217016942E-15,8.38946777378104E-34));
#91761=DIRECTION('',(0.110239267677841,0.,0.993905077893183));
#91762=DIRECTION('',(-0.993905078391756,0.,0.110239263182761));
#91763=DIRECTION('center_axis',(5.15624828916998E-15,1.,3.28033898500044E-15));
#91764=DIRECTION('ref_axis',(-1.,5.15624828916998E-15,-1.49357535274459E-32));
#91765=DIRECTION('',(0.321322147950303,0.,0.946969945265743));
#91766=DIRECTION('',(-0.946969946451846,0.,0.321322144454732));
#91767=DIRECTION('center_axis',(-5.74087398687763E-15,1.,-2.09520551914698E-15));
#91768=DIRECTION('ref_axis',(-1.,-5.74087398687763E-15,3.57632832502997E-33));
#91769=DIRECTION('',(0.517380359614974,0.,0.855755551243859));
#91770=DIRECTION('',(-0.855755553808469,0.,0.517380355373066));
#91771=DIRECTION('center_axis',(1.81711884491992E-14,1.,2.43630771816283E-15));
#91772=DIRECTION('ref_axis',(-1.,1.81711884491992E-14,1.11444476857717E-32));
#91773=DIRECTION('',(0.689246444718554,0.,0.724526975648825));
#91774=DIRECTION('',(-0.724526980936391,0.,0.689246439160332));
#91775=DIRECTION('center_axis',(3.0450150389411E-15,1.,-2.54486696300814E-16));
#91776=DIRECTION('ref_axis',(0.996525810855685,-3.05563087855382E-15,-0.0832845021502743));
#91777=DIRECTION('',(0.828884127273459,0.,0.559420328155955));
#91778=DIRECTION('',(-0.559420334090901,0.,0.828884123267918));
#91779=DIRECTION('center_axis',(-2.91911716366775E-15,1.,9.03125162278983E-16));
#91780=DIRECTION('ref_axis',(-1.,-2.91911716366775E-15,2.14129740204536E-33));
#91781=DIRECTION('',(0.929764111872082,0.,0.36815580434745));
#91782=DIRECTION('',(-0.36815581236092,0.,0.929764108699013));
#91783=DIRECTION('center_axis',(-7.97017386303574E-15,1.,4.52860351294214E-15));
#91784=DIRECTION('ref_axis',(-1.,-7.97017386303574E-15,-2.95419996546644E-32));
#91785=DIRECTION('',(0.987169358889856,0.,0.15967672613437));
#91786=DIRECTION('',(-0.159676734244941,0.,0.987169357577954));
#91787=DIRECTION('center_axis',(9.08042628672507E-15,1.,-8.18143872634072E-15));
#91788=DIRECTION('ref_axis',(-1.,9.08042628672507E-15,-3.70960009999131E-32));
#91789=DIRECTION('',(0.998415664035658,0.,-0.0562686574234377));
#91790=DIRECTION('',(0.0562686524743697,0.,0.998415664314577));
#91791=DIRECTION('center_axis',(0.,1.,0.));
#91792=DIRECTION('ref_axis',(0.,0.,1.));
#91793=DIRECTION('',(0.962977162506725,0.,-0.269582982568442));
#91794=DIRECTION('',(0.269582977795087,0.,0.962977163843013));
#91795=DIRECTION('center_axis',(-1.20146868912725E-15,1.,2.80951118861022E-15));
#91796=DIRECTION('ref_axis',(8.0043662084072E-33,-2.80951118861022E-15,
1.));
#91797=DIRECTION('',(0.882510919242445,0.,-0.47029190660467));
#91798=DIRECTION('',(0.470291902230154,0.,0.882510921573633));
#91799=DIRECTION('center_axis',(1.70825147914177E-15,1.,-9.00631986261566E-15));
#91800=DIRECTION('ref_axis',(7.81898694697755E-33,9.00631986261566E-15,
1.));
#91801=DIRECTION('',(0.76077944621245,0.,-0.649010503937092));
#91802=DIRECTION('',(0.649010502445546,0.,0.760779447484867));
#91803=DIRECTION('center_axis',(-8.92596786684004E-17,1.,-3.05432689493444E-15));
#91804=DIRECTION('ref_axis',(-0.0292115384811887,-3.05563087943486E-15,
-0.999573251952833));
#91805=DIRECTION('',(0.60347477344143,0.,-0.797382090230157));
#91806=DIRECTION('',(0.797382087238821,0.,0.603474777393936));
#91807=DIRECTION('center_axis',(7.43762836885792E-16,1.,2.96373024743229E-15));
#91808=DIRECTION('ref_axis',(1.6716588985035E-33,-2.96373024743229E-15,
1.));
#91809=DIRECTION('',(0.417952286130124,0.,-0.908468979392584));
#91810=DIRECTION('',(0.908468975825409,0.,0.417952293883803));
#91811=DIRECTION('center_axis',(-6.81744233180193E-15,1.,-1.36727642357042E-14));
#91812=DIRECTION('ref_axis',(2.6826757076957E-33,1.36727642357042E-14,1.));
#91813=DIRECTION('',(0.212886820908125,8.54029260079142E-16,-0.977076865698719));
#91814=DIRECTION('',(0.977076864643463,0.,0.212886825751384));
#91815=DIRECTION('center_axis',(1.9194588930583E-15,1.,2.37751080585885E-15));
#91816=DIRECTION('ref_axis',(-9.07626131178252E-33,-2.37751080585885E-15,
1.));
#91817=DIRECTION('',(-0.00213299954342001,0.,-0.999997725153886));
#91818=DIRECTION('',(0.999997725164459,0.,-0.00213299458654189));
#91819=DIRECTION('center_axis',(-7.15703269032E-15,1.,-5.72789702230434E-15));
#91820=DIRECTION('ref_axis',(-1.,-7.15703269032E-15,-3.32432154402052E-32));
#91821=DIRECTION('',(-0.217053081214603,0.,-0.976159802458208));
#91822=DIRECTION('',(0.976159802699633,0.,-0.217053080128833));
#91823=DIRECTION('center_axis',(1.09613783869135E-14,1.,5.40724200926739E-15));
#91824=DIRECTION('ref_axis',(-1.,1.09613783869135E-14,1.13030402369742E-32));
#91825=DIRECTION('',(-0.421824003608544,0.,-0.90667773215165));
#91826=DIRECTION('',(0.90667773424259,0.,-0.421823999114232));
#91827=DIRECTION('center_axis',(5.9337522978211E-15,1.,1.46222567279051E-15));
#91828=DIRECTION('ref_axis',(-1.,5.9337522978211E-15,2.62712725445791E-33));
#91829=DIRECTION('',(-0.606870906241449,0.,-0.794800417185146));
#91830=DIRECTION('',(0.794800422093049,0.,-0.606870899813718));
#91831=DIRECTION('',(-0.763541194667019,0.,-0.645759122309907));
#91832=DIRECTION('',(0.645759126094686,0.,-0.763541191466071));
#91833=DIRECTION('center_axis',(-2.99965019018643E-15,1.,5.82218923504121E-16));
#91834=DIRECTION('ref_axis',(-1.,-2.99965019018643E-15,-2.3362086080716E-33));
#91835=DIRECTION('',(-0.884509150646489,0.,-0.466522842337465));
#91836=DIRECTION('',(0.466522846721858,0.,-0.884509148333998));
#91837=DIRECTION('center_axis',(0.,1.,0.));
#91838=DIRECTION('ref_axis',(0.,0.,1.));
#91839=DIRECTION('',(-0.964118438699621,0.,-0.265472477216386));
#91840=DIRECTION('',(0.265472480987239,0.,-0.964118437661307));
#91841=DIRECTION('center_axis',(1.48676483391871E-14,1.,-1.07275680003584E-14));
#91842=DIRECTION('ref_axis',(-1.,1.48676483391871E-14,7.22009769445324E-32));
#91843=DIRECTION('',(-0.99864662067696,0.,-0.0520089127985631));
#91844=DIRECTION('',(0.0520089175439887,0.,-0.998646620429821));
#91845=DIRECTION('center_axis',(0.,1.,0.));
#91846=DIRECTION('ref_axis',(0.,0.,1.));
#91847=DIRECTION('',(-0.986479196610341,0.,0.16388652981565));
#91848=DIRECTION('',(-0.163886525562761,0.,-0.986479197316885));
#91849=DIRECTION('center_axis',(-1.49818721583241E-15,1.,2.66314009076519E-15));
#91850=DIRECTION('ref_axis',(-9.34860545733725E-33,-2.66314009076519E-15,
1.));
#91851=DIRECTION('',(-0.928185102079373,0.,0.372118820107106));
#91852=DIRECTION('',(-0.372118815506532,0.,-0.928185103923789));
#91853=DIRECTION('center_axis',(0.,1.,0.));
#91854=DIRECTION('ref_axis',(0.,0.,1.));
#91855=DIRECTION('',(-0.826490103338909,0.,0.562951249295035));
#91856=DIRECTION('',(-0.562951245198655,0.,-0.826490106129096));
#91857=DIRECTION('',(-0.686149346322776,0.,0.727460703090433));
#91858=DIRECTION('center_axis',(-0.15848403150235,-0.986495984567242,0.0413338141413225));
#91859=DIRECTION('ref_axis',(0.0350633407380601,0.0362133149627294,0.99872877096622));
#91860=DIRECTION('center_axis',(-0.938019368552222,0.33683080843185,0.0816374345018055));
#91861=DIRECTION('ref_axis',(0.111380041292018,0.0699109451028969,0.991315765110496));
#91862=DIRECTION('center_axis',(0.153961047147948,-0.986495109309872,-0.0558873444422921));
#91863=DIRECTION('ref_axis',(0.14261632231053,-0.0337827101182837,0.989201351145298));
#91864=DIRECTION('center_axis',(-0.145893126005734,-0.986495977860338,0.0744370972677616));
#91865=DIRECTION('ref_axis',(0.24894077710909,0.0362135888321499,0.967841446455058));
#91866=DIRECTION('center_axis',(0.138347359563849,-0.986495107011068,-0.087677887434251));
#91867=DIRECTION('ref_axis',(0.351931117601902,-0.0337827964682365,0.935416063111096));
#91868=DIRECTION('center_axis',(-0.126480595970886,-0.986495984693773,0.104059266891101));
#91869=DIRECTION('ref_axis',(0.451177953046194,0.0362133096746333,0.891698968759893));
#91870=DIRECTION('center_axis',(-0.817045250682722,0.336828066332674,0.467957169052254));
#91871=DIRECTION('ref_axis',(0.517325436789001,0.0698987637591658,0.852929396419194));
#91872=DIRECTION('center_axis',(0.116264722410286,-0.986495107075066,-0.115368618089205));
#91873=DIRECTION('ref_axis',(0.544789966623712,-0.0337827941729723,0.837891768120443));
#91874=DIRECTION('center_axis',(-0.101153885558881,-0.986495984771876,0.128816006246538));
#91875=DIRECTION('ref_axis',(0.632318582174376,0.0362133068361477,0.773861620087841));
#91876=DIRECTION('center_axis',(-0.697347637158444,0.336818240845437,0.63266084562214));
#91877=DIRECTION('ref_axis',(0.688594792234753,0.0699401336332757,0.721765605868371));
#91878=DIRECTION('center_axis',(0.0887457649462112,-0.986495111389322,-0.137664753692004));
#91879=DIRECTION('ref_axis',(0.712175030652464,-0.0337826696403138,0.701188602978639));
#91880=DIRECTION('center_axis',(-0.0710973252204614,-0.986495984603397,
0.147549458514326));
#91881=DIRECTION('ref_axis',(0.783892697096572,0.0362133134291354,0.619839362552222));
#91882=DIRECTION('center_axis',(-0.545039958943152,0.336830199657565,0.7677739639724));
#91883=DIRECTION('ref_axis',(0.827653466131635,0.0699408221214351,0.556864455142603));
#91884=DIRECTION('center_axis',(0.0570769811588049,-0.986495107182151,-0.15352401026378));
#91885=DIRECTION('ref_axis',(0.846259603654513,-0.0337827915677679,0.531698604677872));
#91886=DIRECTION('center_axis',(-0.0377163388188591,-0.986495984668493,
0.159383656687384));
#91887=DIRECTION('ref_axis',(0.898812861906938,0.0362133117090608,0.436834105039571));
#91888=DIRECTION('center_axis',(-0.367248269483428,0.336821700094295,0.866994723690413));
#91889=DIRECTION('ref_axis',(0.928010666644119,0.0699038870008591,0.36593667372499));
#91890=DIRECTION('center_axis',(0.0227394276772378,-0.986495107102228,-0.162204568654139));
#91891=DIRECTION('ref_axis',(0.940774007298495,-0.0337827931227811,0.337346987655669));
#91892=DIRECTION('center_axis',(-0.00257177596363353,-0.986495984633055,
0.163765253552922));
#91893=DIRECTION('ref_axis',(0.971705536836301,0.0362133124927908,0.233402968447226));
#91894=DIRECTION('center_axis',(-0.17228471282127,0.336828211432767,0.925669883765857));
#91895=DIRECTION('ref_axis',(0.984979646001483,0.0699121935542017,0.157884078219537));
#91896=DIRECTION('center_axis',(-0.012661393005518,-0.986495107143346,-0.163300620664463));
#91897=DIRECTION('ref_axis',(0.991298864141802,-0.033782791285507,0.127221401360515));
#91898=DIRECTION('center_axis',(0.0326933264329512,-0.986495977672573,0.160489353050549));
#91899=DIRECTION('ref_axis',(0.999162330746507,0.0362135961898777,0.0190581286648048));
#91900=DIRECTION('center_axis',(-0.0474700622167946,-0.986495111334321,
-0.15676092786986));
#91901=DIRECTION('ref_axis',(0.995471693573044,-0.0337826708549142,-0.0888529034118977));
#91902=DIRECTION('center_axis',(0.0664291596833768,-0.986495984759072,0.149709180740495));
#91903=DIRECTION('ref_axis',(0.979899423791816,0.0362133078390561,-0.196177765273798));
#91904=DIRECTION('center_axis',(0.232319120060856,0.33682143884262,0.912457749591803));
#91905=DIRECTION('ref_axis',(0.960238518096396,0.0699024925997113,-0.270288049851236));
#91906=DIRECTION('center_axis',(-0.0800592438663563,-0.986495109214833,
-0.142891276734311));
#91907=DIRECTION('ref_axis',(0.953097375335365,-0.0337827147074441,-0.300772540827507));
#91908=DIRECTION('center_axis',(0.0970591332333997,-0.986495984709624,0.131928756561151));
#91909=DIRECTION('ref_axis',(0.914817498304034,0.0362133096668296,-0.402240650605732));
#91910=DIRECTION('center_axis',(0.423036348843129,0.336829845929339,0.84118125421855));
#91911=DIRECTION('ref_axis',(0.879683708655244,0.0699088058937639,-0.470392741849896));
#91912=DIRECTION('center_axis',(-0.108904901561428,-0.9864951092803,-0.122340188744111));
#91913=DIRECTION('ref_axis',(0.866157283339105,-0.033782712011013,-0.498628407622152));
#91914=DIRECTION('center_axis',(0.123150730753704,-0.986495984587636,0.10797948836376));
#91915=DIRECTION('ref_axis',(0.80695972441348,0.0362133140582691,-0.589495206985975));
#91916=DIRECTION('center_axis',(0.593975878583261,0.336827700107494,0.730574948996706));
#91917=DIRECTION('ref_axis',(0.757987105710624,0.0699415758510974,-0.64850884615701));
#91918=DIRECTION('center_axis',(-0.132658256173775,-0.98649511141531,-0.096068632875815));
#91919=DIRECTION('ref_axis',(0.738716629391971,-0.0337826676212503,-0.673168977915766));
#91920=DIRECTION('center_axis',(0.14348393489496,-0.986495984508783,0.0789812191290125));
#91921=DIRECTION('ref_axis',(0.661369408704425,0.0362133163355927,-0.749185625162374));
#91922=DIRECTION('center_axis',(0.737147022152457,0.336812593121351,0.585808454058694));
#91923=DIRECTION('ref_axis',(0.600863234638785,0.0699142232257434,-0.796288499634496));
#91924=DIRECTION('center_axis',(-0.150208723144297,-0.98649510928717,-0.0653049679875403));
#91925=DIRECTION('ref_axis',(0.576734425562987,-0.033782710717192,-0.816232890067002));
#91926=DIRECTION('center_axis',(0.157108107777897,-0.9864959776017,0.0462896170443781));
#91927=DIRECTION('ref_axis',(0.484854153870186,0.0362135990806186,-0.873844966064607));
#91928=DIRECTION('center_axis',(-0.160735593006857,-0.98649510717186,-0.0314876589589351));
#91929=DIRECTION('ref_axis',(0.387784716648915,-0.0337827905276527,-0.921130683778195));
#91930=DIRECTION('center_axis',(0.163385845130553,-0.986495984561036,0.0114340743362717));
#91931=DIRECTION('ref_axis',(0.285667736486251,0.0362133139781328,-0.957644266009849));
#91932=DIRECTION('center_axis',(0.914985932287573,0.336825827252756,0.222146586314842));
#91933=DIRECTION('ref_axis',(-0.210968968536098,-0.069936861305119,0.974987656201659));
#91934=DIRECTION('center_axis',(-0.163746599808111,-0.986495107226504,0.0038019033984307));
#91935=DIRECTION('ref_axis',(0.180702658065741,-0.0337827878854193,-0.982957411392103));
#91936=DIRECTION('center_axis',(0.162023962635347,-0.986495984640472,-0.0239563732682202));
#91937=DIRECTION('ref_axis',(0.0731237773961302,0.0362133127214665,-0.996665194115385));
#91938=DIRECTION('center_axis',(0.941351387233131,0.336819278548466,0.0202568347070788));
#91939=DIRECTION('ref_axis',(0.00353863569141246,-0.0698840097142687,0.997548847547677));
#91940=DIRECTION('center_axis',(-0.159101001700983,-0.986495111312731,0.0389135787846211));
#91941=DIRECTION('ref_axis',(-0.034828839057642,-0.0337826723898334,-0.998822147840194));
#91942=DIRECTION('center_axis',(0.153085958589943,-0.986495977708609,-0.0582269288846109));
#91943=DIRECTION('ref_axis',(-0.142839410301014,0.0362135954076269,-0.989083150383481));
#91944=DIRECTION('center_axis',(-0.147016009206128,-0.986495107099126,0.0722059326273673));
#91945=DIRECTION('ref_axis',(-0.2487318162409,-0.0337827937137362,-0.967983061028652));
#91946=DIRECTION('center_axis',(0.136989946942366,-0.986495984715003,-0.0897743091196212));
#91947=DIRECTION('ref_axis',(-0.352123510109114,0.0362133099323452,-0.935252709064337));
#91948=DIRECTION('center_axis',(0.862847394774504,0.336841301078536,-0.376871743725329));
#91949=DIRECTION('ref_axis',(0.422071567400847,-0.0698917385670996,0.90386433543528));
#91950=DIRECTION('center_axis',(-0.128056773935998,-0.98649511147343,0.102121778716044));
#91951=DIRECTION('ref_axis',(-0.451004333228506,-0.0337826658124416,-0.891882179942909));
#91952=DIRECTION('center_axis',(0.114488192993927,-0.986495977375508,-0.117124464937633));
#91953=DIRECTION('ref_axis',(-0.544942774640645,0.0362136074895554,-0.837690842136613));
#91954=DIRECTION('center_axis',(-0.10310962985091,-0.986495106995456,0.127262752233448));
#91955=DIRECTION('ref_axis',(-0.632188419435967,-0.0337827973549945,-0.774077854568857));
#91956=DIRECTION('center_axis',(0.0866334501130605,-0.98649598453504,-0.138997546085356));
#91957=DIRECTION('ref_axis',(-0.712281062451427,0.0362133159577758,-0.700959545066909));
#91958=DIRECTION('center_axis',(0.624856068326553,0.336828197978433,-0.704344843753458));
#91959=DIRECTION('ref_axis',(0.762585940723454,-0.0698942588923449,0.643099895494327));
#91960=DIRECTION('center_axis',(-0.0733412580463798,-0.986495107141828,
0.146452939381247));
#91961=DIRECTION('ref_axis',(-0.783812062389502,-0.0337827924995709,-0.6200785222725));
#91962=DIRECTION('center_axis',(0.0547276501215202,-0.986495984686042,-0.154371488658016));
#91963=DIRECTION('ref_axis',(-0.846313909511036,0.0362133094747293,-0.531452126522261));
#91964=DIRECTION('center_axis',(0.458834021409677,0.336824951473368,-0.822204532255805));
#91965=DIRECTION('ref_axis',(0.88300882564239,-0.0699331565184644,0.464117191512026));
#91966=DIRECTION('center_axis',(-0.0401436056662108,-0.986495109253376,
0.158795120653264));
#91967=DIRECTION('ref_axis',(-0.898785511585147,-0.0337827124044028,-0.437085040360829));
#91968=DIRECTION('center_axis',(0.0202625544542091,-0.98649597750738,-0.162527275399387));
#91969=DIRECTION('ref_axis',(-0.940774062452267,0.0362136030624955,-0.337094554050181));
#91970=DIRECTION('center_axis',(-0.00506873401270936,-0.986495107235941,
0.163712282175342));
#91971=DIRECTION('ref_axis',(-0.971732775235418,-0.0337827882866994,-0.233653882374867));
#91972=DIRECTION('center_axis',(-0.0151497303550186,-0.986495977559997,
-0.163083328173411));
#91973=DIRECTION('ref_axis',(-0.99124465228558,0.0362136008272741,-0.126974857473291));
#91974=DIRECTION('center_axis',(0.0302430763953997,-0.986495107146461,0.160974407612619));
#91975=DIRECTION('ref_axis',(-0.999242880739712,-0.0337827931806898,-0.0192973618899598));
#91976=DIRECTION('center_axis',(-0.0498533426929182,-0.986495984676177,
-0.156013834130575));
#91977=DIRECTION('ref_axis',(-0.995365758355286,0.0362133105381907,0.0890820028606839));
#91978=DIRECTION('center_axis',(-0.132302540794811,0.3368243442411,-0.932226044919252));
#91979=DIRECTION('ref_axis',(0.983828622997496,-0.0699356922579925,-0.164894631565877));
#91980=DIRECTION('center_axis',(0.0641407497217067,-0.986495107067512,0.150709548327221));
#91981=DIRECTION('ref_axis',(-0.980029499961363,-0.0337827935857002,0.195961481069693));
#91982=DIRECTION('center_axis',(-0.0822261691028225,-0.986495984453687,
-0.141649319699833));
#91983=DIRECTION('ref_axis',(-0.952944661855718,0.0362133180488912,0.300973532119657));
#91984=DIRECTION('center_axis',(-0.329609608358645,0.336827084253146,-0.881989241085845));
#91985=DIRECTION('ref_axis',(0.925374513598419,-0.0699627075030704,-0.372541580419325));
#91986=DIRECTION('center_axis',(0.0950392721431884,-0.986495107089222,0.133397677789074));
#91987=DIRECTION('ref_axis',(-0.914991029827499,-0.0337827934393961,0.402057381728833));
#91988=DIRECTION('center_axis',(-0.110754182085875,-0.986495984521845,-0.120661442361528));
#91989=DIRECTION('ref_axis',(-0.865964932744586,0.0362133163850253,0.498791871398344));
#91990=DIRECTION('center_axis',(-0.511503841068363,0.336830860392663,-0.790511727970844));
#91991=DIRECTION('ref_axis',(0.823675742451526,-0.0698814821935577,-0.562738704678609));
#91992=DIRECTION('center_axis',(0.121493796088995,-0.986495109316191,0.109848335477251));
#91993=DIRECTION('ref_axis',(-0.807168618800916,-0.0337827102832155,0.589353501142516));
#91994=DIRECTION('center_axis',(-0.134103453923623,-0.98649598450797,-0.0940315702060031));
#91995=DIRECTION('ref_axis',(-0.73849364637247,0.0362133159122535,0.673287256687762));
#91996=DIRECTION('center_axis',(-0.669485258183011,0.336821850718734,-0.662072903805944));
#91997=DIRECTION('ref_axis',(0.683427665385484,-0.069939876813133,-0.726660195564));
#91998=DIRECTION('center_axis',(0.142267537250305,-0.986495107164757,0.0811624998674068));
#91999=DIRECTION('ref_axis',(-0.661603853930092,-0.0337827916166257,0.749092159520734));
#92000=DIRECTION('center_axis',(-0.151182194028678,-0.986495984697426,-0.0630048917508035));
#92001=DIRECTION('ref_axis',(-0.576491219554483,0.0362133092547474,0.816300477771148));
#92002=DIRECTION('center_axis',(-0.79615852923434,0.336823429075849,-0.502674421423052));
#92003=DIRECTION('ref_axis',(0.511233079746866,-0.0699576495711029,-0.856590138537108));
#92004=DIRECTION('center_axis',(0.156388938553649,-0.986495107211372,0.0486816530747087));
#92005=DIRECTION('ref_axis',(-0.485103252326991,-0.0337827889325442,0.873804072864));
#92006=DIRECTION('center_axis',(-0.161191827682753,-0.986495984704173,-0.0290321692409841));
#92007=DIRECTION('ref_axis',(-0.387532702915014,0.0362133097251902,0.921144397133333));
#92008=DIRECTION('center_axis',(-0.885603712736837,0.336826499306086,-0.319771751960576));
#92009=DIRECTION('ref_axis',(-0.315168257278309,0.069878409286689,0.946459707288015));
#92010=DIRECTION('center_axis',(0.163197749307222,-0.986495109254072,0.0139245839741768));
#92011=DIRECTION('ref_axis',(-0.285919796784119,-0.0337827117026771,0.957657871161169));
#92012=DIRECTION('center_axis',(-0.163664310470787,-0.986495984716146,0.00629806454745587));
#92013=DIRECTION('ref_axis',(-0.180453584359339,0.0362133089092276,0.982916629297578));
#92014=DIRECTION('center_axis',(-0.933640852264392,0.336824940607712,-0.121916850220263));
#92015=DIRECTION('ref_axis',(-0.10432265313841,0.0699226078440237,0.992082462779407));
#92016=DIRECTION('center_axis',(0.16237565034875,-0.986495109299984,-0.0214836566029404));
#92017=DIRECTION('ref_axis',(-0.0733670170758494,-0.0337827112753311,0.996732666879279));
#92018=DIRECTION('center_axis',(0.,-1.,0.));
#92019=DIRECTION('ref_axis',(0.,0.,-1.));
#92020=DIRECTION('',(-0.603364206226571,0.,0.797465757662723));
#92021=DIRECTION('center_axis',(0.158479767859181,0.986495111177158,-0.0413709898705178));
#92022=DIRECTION('ref_axis',(0.182060716416353,0.0119854687619504,0.983214241188827));
#92023=DIRECTION('',(0.797465759836418,0.,0.6033642033536));
#92024=DIRECTION('',(-0.417826324587941,0.,0.908526918963512));
#92025=DIRECTION('center_axis',(0.145881046725855,0.986495110670749,-0.0744722554302954));
#92026=DIRECTION('ref_axis',(0.389166237111431,0.0119855022556315,0.921089565475698));
#92027=DIRECTION('',(0.908526921826082,0.,0.417826318363533));
#92028=DIRECTION('',(-0.212751349470685,0.,0.977106372560533));
#92029=DIRECTION('center_axis',(0.126461096607096,0.986495110752455,-0.104091246060526));
#92030=DIRECTION('ref_axis',(0.578074777275499,0.0119854994431879,0.815895765205936));
#92031=DIRECTION('',(0.977106374521695,0.,0.212751340463627));
#92032=DIRECTION('',(0.00227165745136495,0.,0.999997419782883));
#92033=DIRECTION('center_axis',(0.101127974199879,0.986495110894289,-0.128843040230716));
#92034=DIRECTION('ref_axis',(0.73995317920339,0.0119854881880012,0.672551589589744));
#92035=DIRECTION('',(0.999997419791011,0.,-0.00227165387351802));
#92036=DIRECTION('',(0.217188425318953,0.,0.976129698302164));
#92037=DIRECTION('center_axis',(0.0710662092121789,0.986495110852024,-0.147570288924515));
#92038=DIRECTION('ref_axis',(0.867232196839401,0.011985492721948,0.497759645541218));
#92039=DIRECTION('',(0.976129697249629,0.,-0.217188430049455));
#92040=DIRECTION('',(0.421949715333494,0.,0.906619235252586));
#92041=DIRECTION('center_axis',(0.037681493016981,0.986495111222342,-0.159397304301016));
#92042=DIRECTION('ref_axis',(0.953960399933603,0.0119854691604863,0.299693016080662));
#92043=DIRECTION('',(0.906619236073577,0.,-0.421949713569477));
#92044=DIRECTION('',(0.606981095233153,0.,0.794716270142724));
#92045=DIRECTION('center_axis',(0.00253481763562235,0.986495111223513,-0.163771090952169));
#92046=DIRECTION('ref_axis',(0.99608247502221,0.0119854644543318,0.0876130789063035));
#92047=DIRECTION('',(0.794716264459817,0.,-0.606981102673744));
#92048=DIRECTION('',(0.763630727833486,0.,0.64565324401609));
#92049=DIRECTION('center_axis',(-0.0327304306477485,0.986495110640403,-0.160487119708069));
#92050=DIRECTION('ref_axis',(0.991628840187903,0.0119855052037018,-0.128563567827769));
#92051=DIRECTION('',(0.645653244432689,0.,-0.763630727481249));
#92052=DIRECTION('',(0.884573824525916,0.,0.466400202576708));
#92053=DIRECTION('center_axis',(-0.0664651799120975,0.986495110908589,-0.149698951274562));
#92054=DIRECTION('ref_axis',(0.940807743855523,0.0119854863573399,-0.338728707402042));
#92055=DIRECTION('',(0.466400198110657,0.,-0.884573826880685));
#92056=DIRECTION('',(0.964155238486549,0.,0.265338794937613));
#92057=DIRECTION('center_axis',(-0.0970921104723414,0.986495110838536,-0.131911024466085));
#92058=DIRECTION('ref_axis',(0.845995521661184,0.0119854859784489,-0.53305527429628));
#92059=DIRECTION('',(0.265338798459341,0.,-0.964155237517358));
#92060=DIRECTION('',(0.998653822673426,0.,0.0518704391706294));
#92061=DIRECTION('center_axis',(-0.123179135387685,0.986495110642582,-0.107955070670268));
#92062=DIRECTION('ref_axis',(0.711625490067636,0.0119855055860069,-0.702456767026872));
#92063=DIRECTION('',(0.0518704491632369,0.,-0.998653822154406));
#92064=DIRECTION('',(0.986456463072521,0.,-0.164023310728849));
#92065=DIRECTION('center_axis',(-0.143506400745292,0.98649511126427,-0.0789513039590035));
#92066=DIRECTION('ref_axis',(0.543980643219903,0.0119854622664827,-0.839012162305362));
#92067=DIRECTION('',(-0.164023304687571,0.,-0.986456464077036));
#92068=DIRECTION('',(0.928133495813481,0.,-0.372247517048868));
#92069=DIRECTION('center_axis',(-0.15712350469364,0.986495110979502,-0.0462558135408789));
#92070=DIRECTION('ref_axis',(0.350899859893009,0.0119854818250457,-0.936336283902577));
#92071=DIRECTION('',(-0.372247514176791,0.,-0.928133496965388));
#92072=DIRECTION('',(0.82641204072096,0.,-0.563065838913549));
#92073=DIRECTION('center_axis',(-0.16339367973884,0.986495110748462,-0.0113974510651309));
#92074=DIRECTION('ref_axis',(0.141411393691066,0.0119855006749099,-0.989878358945139));
#92075=DIRECTION('',(-0.563065840773055,0.,-0.826412039454008));
#92076=DIRECTION('',(0.686048466658641,0.,-0.727555840740302));
#92077=DIRECTION('center_axis',(-0.162023741836773,0.986495110751063,0.0239938230688417));
#92078=DIRECTION('ref_axis',(-0.0746893108236778,0.0119854977166643,-0.997134822726179));
#92079=DIRECTION('',(-0.727555834238047,0.,-0.686048473554296));
#92080=DIRECTION('',(0.513606044881543,0.,-0.858026124696176));
#92081=DIRECTION('center_axis',(-0.153077758419838,0.986495110978776,0.0582631606774879));
#92082=DIRECTION('ref_axis',(-0.287297624221738,0.011985482316554,-0.957766371997986));
#92083=DIRECTION('',(-0.858026124717308,0.,-0.513606044846241));
#92084=DIRECTION('',(0.317147963692256,0.,-0.948376069460768));
#92085=DIRECTION('center_axis',(-0.136974036913601,0.986495111296262,0.0898081766888047));
#92086=DIRECTION('ref_axis',(-0.486472223026737,0.0119854633644171,-0.873613830528893));
#92087=DIRECTION('',(-0.948376067456526,0.,-0.317147969685596));
#92088=DIRECTION('',(0.105860400263,0.,-0.994381001254628));
#92089=DIRECTION('center_axis',(-0.114465547034228,0.986495111103593,0.117153891573711));
#92090=DIRECTION('ref_axis',(-0.662899926125668,0.0119854775341654,-0.748612073286867));
#92091=DIRECTION('',(-0.994381001079128,0.,-0.105860401911536));
#92092=DIRECTION('',(-0.110377074078133,0.,-0.993889783385437));
#92093=DIRECTION('center_axis',(-0.086604781679156,0.986495111014318,0.139021608878454));
#92094=DIRECTION('ref_axis',(-0.808331159221251,0.0119854794471593,-0.588606052733447));
#92095=DIRECTION('',(-0.993889782988621,0.,0.110377077651255));
#92096=DIRECTION('',(-0.321453455831505,0.,-0.946925380235414));
#92097=DIRECTION('center_axis',(-0.0546944690174662,0.986495110963998,0.154388830888208));
#92098=DIRECTION('ref_axis',(-0.91596573079673,0.0119854833439481,-0.40107745909615));
#92099=DIRECTION('',(-0.946925383812815,0.,0.321453445293331));
#92100=DIRECTION('',(-0.517499007895215,0.,-0.855683806570785));
#92101=DIRECTION('center_axis',(-0.020226705941467,0.986495110930022,0.162537000335067));
#92102=DIRECTION('ref_axis',(-0.98077075817357,0.0119854859094575,-0.194794938433099));
#92103=DIRECTION('',(-0.855683806294095,0.,0.517499008352721));
#92104=DIRECTION('',(-0.689346898711863,0.,-0.724431399951946));
#92105=DIRECTION('center_axis',(0.0151868177319126,0.986495111230557,0.163085119141475));
#92106=DIRECTION('ref_axis',(-0.999716036804243,0.0119854703633428,0.0205959767087327));
#92107=DIRECTION('',(-0.724431405665859,0.,0.689346892707139));
#92108=DIRECTION('',(-0.828961683246508,0.,-0.559305397532615));
#92109=DIRECTION('center_axis',(0.049890258038083,0.986495110880213,0.156007558670503));
#92110=DIRECTION('ref_axis',(-0.971915703710593,0.0119854899509415,0.235023856047377));
#92111=DIRECTION('',(-0.559305393777797,0.,0.828961685779906));
#92112=DIRECTION('',(-0.929815150843002,0.,-0.368026881168761));
#92113=DIRECTION('center_axis',(0.0822608615150763,0.986495110907273,0.141635259800816));
#92114=DIRECTION('ref_axis',(-0.898669673512321,0.0119854860796758,0.438462274355152));
#92115=DIRECTION('',(-0.368026888901989,0.,0.92981514778214));
#92116=DIRECTION('',(-0.987191490845447,0.,-0.159539839545941));
#92117=DIRECTION('center_axis',(0.110785037875841,0.986495110984941,0.120640256074234));
#92118=DIRECTION('ref_axis',(-0.783402848266655,0.0119854803289976,0.621398684894791));
#92119=DIRECTION('',(-0.159539852444422,0.,0.987191488760925));
#92120=DIRECTION('',(-0.998407852997013,0.,0.0564070835436024));
#92121=DIRECTION('center_axis',(0.134129057425302,0.986495110447697,0.0940042180808219));
#92122=DIRECTION('ref_axis',(-0.631504974824666,0.0119855165618774,0.775279184658303));
#92123=DIRECTION('',(0.0564070922907477,0.,0.998407852502825));
#92124=DIRECTION('',(-0.962939775847857,0.,0.269716495769317));
#92125=DIRECTION('center_axis',(0.151201316773429,0.986495110675738,0.0629726799401554));
#92126=DIRECTION('ref_axis',(-0.450078631102011,0.0119855039511957,0.892908491123461));
#92127=DIRECTION('',(0.269716499111255,0.,0.96293977491179));
#92128=DIRECTION('',(-0.882445701452064,0.,0.470414268479151));
#92129=DIRECTION('center_axis',(0.161203577483734,0.986495110702338,0.0289966061260205));
#92130=DIRECTION('ref_axis',(-0.247607114474751,0.0119854981900649,0.968786387546101));
#92131=DIRECTION('',(0.47041426492384,0.,0.88244570334733));
#92132=DIRECTION('',(-0.76068944558395,0.,0.649115989155392));
#92133=DIRECTION('center_axis',(0.163668139206856,0.986495111098837,-0.00633529688789426));
#92134=DIRECTION('ref_axis',(-0.0335577583546433,0.0119854717406174,0.999364910991659));
#92135=DIRECTION('',(0.649115980606205,0.,0.760689452879193));
#92136=DIRECTION('center_axis',(0.,1.,0.));
#92137=DIRECTION('ref_axis',(1.,0.,0.));
#92138=DIRECTION('center_axis',(0.,-1.,0.));
#92139=DIRECTION('ref_axis',(0.,0.,-1.));
#92140=DIRECTION('axis',(0.,0.,1.));
#92141=DIRECTION('refdir',(1.,0.,0.));
#92142=DIRECTION('center_axis',(5.28813965849088E-17,1.,5.28813965824263E-17));
#92143=DIRECTION('ref_axis',(-1.,5.28813965849088E-17,-4.79793613002828E-34));
#92144=DIRECTION('center_axis',(5.28813965849088E-17,1.,5.28813965824263E-17));
#92145=DIRECTION('ref_axis',(-1.,5.28813965849088E-17,-4.79793613002828E-34));
#92146=DIRECTION('',(-5.28813965849088E-17,-1.,-5.28813965824263E-17));
#92147=DIRECTION('center_axis',(-5.28813965849088E-17,-1.,-5.28813965824263E-17));
#92148=DIRECTION('ref_axis',(-1.,5.28813965849088E-17,-4.79793613002828E-34));
#92149=DIRECTION('center_axis',(0.,-1.,0.));
#92150=DIRECTION('ref_axis',(0.,0.,-1.));
#92151=DIRECTION('center_axis',(0.,1.,0.));
#92152=DIRECTION('ref_axis',(0.,0.,-1.));
#92153=DIRECTION('',(0.,1.,0.));
#92154=DIRECTION('center_axis',(0.,1.,0.));
#92155=DIRECTION('ref_axis',(0.,0.,-1.));
#92156=DIRECTION('',(0.,-1.,0.));
#92157=DIRECTION('center_axis',(0.,1.,0.));
#92158=DIRECTION('ref_axis',(1.77635683940025E-15,0.,-1.));
#92159=DIRECTION('',(0.,-1.,0.));
#92160=DIRECTION('center_axis',(0.,1.,0.));
#92161=DIRECTION('ref_axis',(0.,0.,-1.));
#92162=DIRECTION('center_axis',(0.,1.,0.));
#92163=DIRECTION('ref_axis',(1.77635683940025E-15,0.,-1.));
#92164=DIRECTION('',(-2.63231840778213E-15,1.,2.63231840765855E-15));
#92165=DIRECTION('center_axis',(-2.63231840778213E-15,1.,2.63231840765855E-15));
#92166=DIRECTION('ref_axis',(1.,2.63231840778213E-15,-1.74102415060709E-31));
#92167=DIRECTION('',(2.63231840778213E-15,-1.,-2.63231840765855E-15));
#92168=DIRECTION('center_axis',(0.,1.,1.66800334228539E-17));
#92169=DIRECTION('ref_axis',(0.,-1.66800334228539E-17,1.));
#92170=DIRECTION('center_axis',(0.,1.,1.47010464065831E-16));
#92171=DIRECTION('ref_axis',(0.,1.47010464065831E-16,-1.));
#92172=DIRECTION('center_axis',(0.,1.,1.47010464065831E-16));
#92173=DIRECTION('ref_axis',(0.,1.47010464065831E-16,-1.));
#92174=DIRECTION('',(0.,-1.,-1.66800334228539E-17));
#92175=DIRECTION('center_axis',(0.,1.,1.66800334228539E-17));
#92176=DIRECTION('ref_axis',(0.,-1.66800334228539E-17,1.));
#92177=DIRECTION('center_axis',(-2.93166199061116E-26,2.06514699531572E-15,
1.));
#92178=DIRECTION('ref_axis',(-1.21086259326173E-42,-1.,2.06514699531572E-15));
#92179=DIRECTION('',(0.,0.,-1.));
#92180=DIRECTION('center_axis',(-2.93166199061116E-26,2.06514699531572E-15,
1.));
#92181=DIRECTION('ref_axis',(9.08146939547479E-43,-1.,2.06514699531572E-15));
#92182=DIRECTION('',(2.93166199061116E-26,-2.06514699531572E-15,-1.));
#92183=DIRECTION('center_axis',(0.,-1.,-1.47010464065831E-16));
#92184=DIRECTION('ref_axis',(0.,1.47010464065831E-16,-1.));
#92185=DIRECTION('',(8.65956056235493E-17,0.707106781186548,-0.707106781186547));
#92186=DIRECTION('center_axis',(0.,1.,3.67526160164578E-16));
#92187=DIRECTION('ref_axis',(0.,3.67526160164578E-16,-1.));
#92188=DIRECTION('center_axis',(-8.85182572930084E-15,-1.,-4.71957425956767E-15));
#92189=DIRECTION('ref_axis',(1.,-8.85182572930084E-15,6.75072510268539E-31));
#92190=DIRECTION('center_axis',(-1.77036514757944E-15,1.,9.43914852352751E-16));
#92191=DIRECTION('ref_axis',(1.,1.77036514757944E-15,-1.48294102778218E-31));
#92192=DIRECTION('center_axis',(0.,-1.,3.67526160164578E-16));
#92193=DIRECTION('ref_axis',(0.,-3.67526160164578E-16,-1.));
#92194=DIRECTION('center_axis',(0.,-1.,3.67526160164578E-16));
#92195=DIRECTION('ref_axis',(0.,-3.67526160164578E-16,-1.));
#92196=DIRECTION('',(0.,1.,-3.67526160164578E-16));
#92197=DIRECTION('center_axis',(-1.45977385561436E-15,1.,6.6703545231173E-26));
#92198=DIRECTION('ref_axis',(1.,1.45977385561436E-15,-6.89099987452658E-43));
#92199=DIRECTION('center_axis',(0.,-1.,0.));
#92200=DIRECTION('ref_axis',(0.,0.,-1.));
#92201=DIRECTION('center_axis',(0.,-1.,0.));
#92202=DIRECTION('ref_axis',(0.,0.,-1.));
#92203=DIRECTION('center_axis',(0.,0.,-1.));
#92204=DIRECTION('ref_axis',(0.,-1.,0.));
#92205=DIRECTION('center_axis',(0.,0.,1.));
#92206=DIRECTION('ref_axis',(1.,0.,0.));
#92207=DIRECTION('',(-1.,0.,0.));
#92208=DIRECTION('center_axis',(0.,0.,1.));
#92209=DIRECTION('ref_axis',(1.,0.,0.));
#92210=DIRECTION('',(0.,0.,1.));
#92211=DIRECTION('',(0.,0.,-1.));
#92212=DIRECTION('center_axis',(0.,1.,0.));
#92213=DIRECTION('ref_axis',(1.,0.,0.));
#92214=DIRECTION('center_axis',(-1.45977385561436E-15,1.,6.6703545231173E-26));
#92215=DIRECTION('ref_axis',(1.,1.45977385561436E-15,8.88178419700125E-16));
#92216=DIRECTION('center_axis',(0.,0.,1.));
#92217=DIRECTION('ref_axis',(1.,0.,0.));
#92218=DIRECTION('',(1.,0.,0.));
#92219=DIRECTION('center_axis',(0.,-1.,0.));
#92220=DIRECTION('ref_axis',(0.,0.,-1.));
#92221=DIRECTION('center_axis',(0.,-1.,0.));
#92222=DIRECTION('ref_axis',(0.,0.,-1.));
#92223=DIRECTION('center_axis',(0.,1.,0.));
#92224=DIRECTION('ref_axis',(1.,0.,0.));
#92225=DIRECTION('center_axis',(1.45977385561436E-15,-1.,-6.6703545231173E-26));
#92226=DIRECTION('ref_axis',(-1.,-1.45977385561436E-15,2.10124025885857E-11));
#92227=DIRECTION('center_axis',(1.0383151449662E-25,-9.0044324180798E-16,
1.));
#92228=DIRECTION('ref_axis',(-3.43490264341233E-42,-1.,-9.0044324180798E-16));
#92229=DIRECTION('center_axis',(-1.0383151449662E-25,9.0044324180798E-16,
-1.));
#92230=DIRECTION('ref_axis',(-0.564905044898505,-0.825155918750037,-7.4300607041767E-16));
#92231=DIRECTION('center_axis',(-5.53768147829691E-25,4.80236395630922E-15,
1.));
#92232=DIRECTION('ref_axis',(-1.76510259964373E-41,-1.,4.80236395630923E-15));
#92233=DIRECTION('center_axis',(-1.0383151449662E-25,9.0044324180798E-16,
1.));
#92234=DIRECTION('ref_axis',(-0.564905044898511,-0.825155918750033,7.43006070417667E-16));
#92235=DIRECTION('axis',(0.,0.,1.));
#92236=DIRECTION('refdir',(1.,0.,0.));
#92237=DIRECTION('center_axis',(0.,6.93889390390723E-16,1.));
#92238=DIRECTION('ref_axis',(0.,-1.,6.93889390390723E-16));
#92239=DIRECTION('center_axis',(0.,0.,-1.));
#92240=DIRECTION('ref_axis',(1.,0.,0.));
#92241=DIRECTION('',(0.,6.93889390390723E-16,1.));
#92242=DIRECTION('center_axis',(0.,6.93889390390723E-16,1.));
#92243=DIRECTION('ref_axis',(0.,-1.,6.93889390390723E-16));
#92244=DIRECTION('center_axis',(0.,0.,-1.));
#92245=DIRECTION('ref_axis',(1.,0.,0.));
#92246=DIRECTION('center_axis',(-3.63153646019851E-17,-6.92938439083296E-16,
1.));
#92247=DIRECTION('ref_axis',(-3.45341426252241E-35,-1.,-6.92938439083296E-16));
#92248=DIRECTION('center_axis',(-1.52446456598325E-14,7.98938021243665E-16,
-1.));
#92249=DIRECTION('ref_axis',(0.998629534767396,-0.0523359559982918,-1.52655665880975E-14));
#92250=DIRECTION('',(-1.12274446152321E-16,0.707106780692592,0.707106781680503));
#92251=DIRECTION('center_axis',(0.,0.,-1.));
#92252=DIRECTION('ref_axis',(1.,0.,0.));
#92253=DIRECTION('center_axis',(0.,-3.46944695195361E-16,1.));
#92254=DIRECTION('ref_axis',(0.,-1.,-3.46944695195361E-16));
#92255=DIRECTION('center_axis',(0.,3.46944695195361E-16,-1.));
#92256=DIRECTION('ref_axis',(0.,-1.,-3.46944695195361E-16));
#92257=DIRECTION('',(0.,-3.46944695195361E-16,1.));
#92258=DIRECTION('center_axis',(-0.743144825477131,-0.669130606359151,0.));
#92259=DIRECTION('ref_axis',(0.669130606359151,-0.743144825477131,0.));
#92260=DIRECTION('',(-0.743144825354978,-0.669130606494815,5.74180650796065E-11));
#92261=DIRECTION('',(-0.743144825338902,-0.669130606512669,-6.51837050591796E-11));
#92262=DIRECTION('center_axis',(1.68138855363801E-15,-1.86737117074379E-15,
-1.));
#92263=DIRECTION('ref_axis',(2.23032315803962E-31,1.,-1.86737117074379E-15));
#92264=DIRECTION('',(1.10232564335427E-15,-0.707106780692635,-0.70710678168046));
#92265=DIRECTION('center_axis',(0.,0.,-1.));
#92266=DIRECTION('ref_axis',(-1.,0.,0.));
#92267=DIRECTION('center_axis',(-3.79384149091044E-17,-3.92183207036316E-16,
-1.));
#92268=DIRECTION('ref_axis',(-0.765634450688746,-0.643275903418232,2.81328964270679E-16));
#92269=DIRECTION('center_axis',(3.79384149091044E-17,3.92183207036316E-16,
1.));
#92270=DIRECTION('ref_axis',(1.57435551588766E-33,1.,-3.92183207036316E-16));
#92271=DIRECTION('center_axis',(-3.79384149091044E-17,-3.92183207036316E-16,
-1.));
#92272=DIRECTION('ref_axis',(-1.16783860824811E-33,1.,-3.92183207036316E-16));
#92273=DIRECTION('',(0.,0.,1.));
#92274=DIRECTION('center_axis',(1.23118896951448E-16,-1.32862593793964E-16,
-1.));
#92275=DIRECTION('ref_axis',(-1.44020741115392E-33,1.,-1.32862593793964E-16));
#92276=DIRECTION('center_axis',(-3.79384149091044E-17,-3.92183207036316E-16,
-1.));
#92277=DIRECTION('ref_axis',(1.57435551588766E-33,1.,-3.92183207036316E-16));
#92278=DIRECTION('',(0.669130606258963,-0.74314482556734,0.));
#92279=DIRECTION('',(-0.669130606258963,0.74314482556734,0.));
#92280=DIRECTION('center_axis',(-0.743144825477572,-0.669130606358661,-5.1412188556418E-14));
#92281=DIRECTION('ref_axis',(0.669130606358661,-0.743144825477572,9.69152791773566E-30));
#92282=DIRECTION('',(-0.743144825477595,-0.669130606358635,0.));
#92283=DIRECTION('center_axis',(-0.743144825477598,-0.669130606358632,9.65978868287187E-15));
#92284=DIRECTION('ref_axis',(0.669130606358632,-0.743144825477598,-7.53421370458092E-30));
#92285=DIRECTION('',(0.743144825477595,0.669130606358636,0.));
#92286=DIRECTION('',(-0.66913060645258,0.743144825393007,0.));
#92287=DIRECTION('',(0.66913060645258,-0.743144825393007,0.));
#92288=DIRECTION('center_axis',(-0.998629535578219,0.0523359405268506,-2.25173431738112E-16));
#92289=DIRECTION('ref_axis',(0.0515611881252755,0.983846374653154,-0.171428571017072));
#92290=DIRECTION('center_axis',(-0.0348994964802897,-0.999390827026856,
0.));
#92291=DIRECTION('ref_axis',(-0.999390827026856,0.0348994964802897,0.));
#92292=DIRECTION('center_axis',(-0.0348994967020073,-0.999390827019113,
-1.98641521842394E-15));
#92293=DIRECTION('ref_axis',(-0.999390827019113,0.0348994967020073,-8.88178419700125E-16));
#92294=DIRECTION('',(0.999390827026856,-0.0348994964802897,0.));
#92295=DIRECTION('',(-0.999390827026856,0.0348994964802897,0.));
#92296=DIRECTION('center_axis',(0.,0.,1.));
#92297=DIRECTION('ref_axis',(1.,0.,0.));
#92298=DIRECTION('center_axis',(4.74434968313444E-6,-6.69147110686511E-5,
0.999999997749956));
#92299=DIRECTION('ref_axis',(0.964891936205745,-0.262647198641797,-2.21527462117478E-5));
#92300=DIRECTION('',(0.034899496686458,0.999390827019656,0.));
#92301=DIRECTION('center_axis',(0.,0.,1.));
#92302=DIRECTION('ref_axis',(1.,0.,0.));
#92303=DIRECTION('center_axis',(0.,0.,1.));
#92304=DIRECTION('ref_axis',(1.,0.,0.));
#92305=DIRECTION('center_axis',(4.74680614066393E-6,-6.69734503770472E-5,
-0.999999997746012));
#92306=DIRECTION('ref_axis',(0.964894998461477,-0.26263594851529,2.21698052188808E-5));
#92307=DIRECTION('center_axis',(0.0348994967020073,0.999390827019113,1.98641521842394E-15));
#92308=DIRECTION('ref_axis',(0.999390827019113,-0.0348994967020073,-6.11038882754296E-11));
#92309=DIRECTION('',(-0.0348994966864581,-0.999390827019656,0.));
#92310=DIRECTION('center_axis',(0.,0.,-1.));
#92311=DIRECTION('ref_axis',(0.,-1.,0.));
#92312=DIRECTION('axis',(0.,0.,1.));
#92313=DIRECTION('refdir',(1.,0.,0.));
#92314=DIRECTION('center_axis',(0.,3.46944695195361E-16,1.));
#92315=DIRECTION('ref_axis',(0.,-1.,3.46944695195361E-16));
#92316=DIRECTION('center_axis',(0.,-3.46944695195361E-16,-1.));
#92317=DIRECTION('ref_axis',(0.,-1.,3.46944695195361E-16));
#92318=DIRECTION('',(0.,3.46944695195361E-16,1.));
#92319=DIRECTION('',(0.,3.46944695195361E-16,1.));
#92320=DIRECTION('center_axis',(0.,3.46944695195361E-16,1.));
#92321=DIRECTION('ref_axis',(0.,-1.,3.46944695195361E-16));
#92322=DIRECTION('center_axis',(1.20172968798293E-14,-7.54951656745103E-15,
1.));
#92323=DIRECTION('ref_axis',(1.,0.,-1.19556786944265E-14));
#92324=DIRECTION('center_axis',(0.,-1.,0.));
#92325=DIRECTION('ref_axis',(1.,0.,-6.98296267747417E-15));
#92326=DIRECTION('center_axis',(0.,0.,1.));
#92327=DIRECTION('ref_axis',(1.,0.,0.));
#92328=DIRECTION('center_axis',(0.,-1.,0.));
#92329=DIRECTION('ref_axis',(1.,0.,-6.98296267747417E-15));
#92330=DIRECTION('center_axis',(0.,-1.,0.));
#92331=DIRECTION('ref_axis',(1.,0.,-6.98296267747417E-15));
#92332=DIRECTION('center_axis',(0.,0.,-1.));
#92333=DIRECTION('ref_axis',(-1.,0.,0.));
#92334=DIRECTION('center_axis',(0.,1.,0.));
#92335=DIRECTION('ref_axis',(1.,0.,-6.98296267717208E-15));
#92336=DIRECTION('center_axis',(-2.22101865678853E-15,-1.,2.2210186565311E-15));
#92337=DIRECTION('ref_axis',(1.,-2.22101865678853E-15,1.16857368147256E-31));
#92338=DIRECTION('center_axis',(0.,-1.,-1.23599047663347E-14));
#92339=DIRECTION('ref_axis',(0.,-1.23599047663347E-14,1.));
#92340=DIRECTION('center_axis',(0.,-1.,-1.23599047663347E-14));
#92341=DIRECTION('ref_axis',(0.,-1.23599047663347E-14,1.));
#92342=DIRECTION('',(2.22101865678853E-15,1.,-2.2210186565311E-15));
#92343=DIRECTION('',(0.,-1.,0.));
#92344=DIRECTION('center_axis',(2.22101865678853E-15,1.,-2.2210186565311E-15));
#92345=DIRECTION('ref_axis',(1.,-2.22101865678853E-15,1.16857368147256E-31));
#92346=DIRECTION('',(0.,1.,0.));
#92347=DIRECTION('',(0.,-1.,0.));
#92348=DIRECTION('center_axis',(2.22101865678853E-15,1.,-2.2210186565311E-15));
#92349=DIRECTION('ref_axis',(1.,-2.22101865678853E-15,1.16857368147256E-31));
#92350=DIRECTION('',(0.,1.,0.));
#92351=DIRECTION('center_axis',(-1.31418445149758E-16,-1.,0.));
#92352=DIRECTION('ref_axis',(1.,-1.31418445149758E-16,0.));
#92353=DIRECTION('center_axis',(0.,-1.,0.));
#92354=DIRECTION('ref_axis',(0.,0.,-1.));
#92355=DIRECTION('',(-0.707106781186547,-0.707106781186547,-8.65956056235493E-17));
#92356=DIRECTION('center_axis',(0.,-1.,0.));
#92357=DIRECTION('ref_axis',(0.,0.,-1.));
#92358=DIRECTION('center_axis',(-1.13327439325526E-16,1.,0.));
#92359=DIRECTION('ref_axis',(-1.,-1.13327439325526E-16,0.));
#92360=DIRECTION('',(-0.500000000526354,-0.866025403480548,6.12323400218274E-17));
#92361=DIRECTION('center_axis',(0.,-1.,0.));
#92362=DIRECTION('ref_axis',(0.,0.,1.));
#92363=DIRECTION('center_axis',(7.17905020235292E-15,-1.,-7.17905020184743E-15));
#92364=DIRECTION('ref_axis',(1.,7.17905020235292E-15,-1.29497664574085E-30));
#92365=DIRECTION('',(7.17905020235292E-15,-1.,-7.17905020184743E-15));
#92366=DIRECTION('center_axis',(0.,-1.,0.));
#92367=DIRECTION('ref_axis',(0.,0.,-1.));
#92368=DIRECTION('center_axis',(0.,-1.,0.));
#92369=DIRECTION('ref_axis',(0.,0.,-1.));
#92370=DIRECTION('',(1.,0.,0.));
#92371=DIRECTION('center_axis',(0.,-1.,0.));
#92372=DIRECTION('ref_axis',(0.,0.,-1.));
#92373=DIRECTION('',(-1.,0.,0.));
#92374=DIRECTION('center_axis',(1.4358100401433E-14,-1.,-1.43581004053009E-14));
#92375=DIRECTION('ref_axis',(5.17990657360398E-30,1.43581004053009E-14,
-1.));
#92376=DIRECTION('',(1.4358100401433E-14,-1.,-1.43581004053009E-14));
#92377=DIRECTION('center_axis',(0.,0.,1.));
#92378=DIRECTION('ref_axis',(1.,0.,0.));
#92379=DIRECTION('center_axis',(0.,0.,-1.));
#92380=DIRECTION('ref_axis',(0.,-1.,0.));
#92381=DIRECTION('axis',(0.,0.,1.));
#92382=DIRECTION('refdir',(1.,0.,0.));
#92383=DIRECTION('center_axis',(0.,-3.46944695195362E-16,-1.));
#92384=DIRECTION('ref_axis',(0.,1.,-3.46944695195362E-16));
#92385=DIRECTION('center_axis',(2.20309881449055E-14,0.,-1.));
#92386=DIRECTION('ref_axis',(1.,0.,2.20309881449055E-14));
#92387=DIRECTION('center_axis',(2.20309881449055E-14,0.,-1.));
#92388=DIRECTION('ref_axis',(1.,0.,2.20309881449055E-14));
#92389=DIRECTION('',(0.,3.46944695195362E-16,1.));
#92390=DIRECTION('',(0.,3.46944695195362E-16,1.));
#92391=DIRECTION('center_axis',(-2.63677968348475E-14,0.,1.));
#92392=DIRECTION('ref_axis',(-1.,0.,-2.63677968348475E-14));
#92393=DIRECTION('center_axis',(0.,-1.73472347597681E-15,-1.));
#92394=DIRECTION('ref_axis',(0.,1.,-1.73472347597681E-15));
#92395=DIRECTION('',(8.65956056235493E-17,0.707106781186548,0.707106781186547));
#92396=DIRECTION('center_axis',(0.,0.,1.));
#92397=DIRECTION('ref_axis',(-1.,0.,0.));
#92398=DIRECTION('center_axis',(0.,0.,1.));
#92399=DIRECTION('ref_axis',(1.,0.,0.));
#92400=DIRECTION('',(0.707106781186547,8.65956056235493E-17,-0.707106781186548));
#92401=DIRECTION('center_axis',(0.,0.,-1.));
#92402=DIRECTION('ref_axis',(1.,0.,0.));
#92403=DIRECTION('center_axis',(0.,0.,1.));
#92404=DIRECTION('ref_axis',(1.,0.,0.));
#92405=DIRECTION('center_axis',(0.,0.,1.));
#92406=DIRECTION('ref_axis',(1.,0.,0.));
#92407=DIRECTION('center_axis',(-2.20842887353658E-15,1.,-2.20842887397973E-15));
#92408=DIRECTION('ref_axis',(2.65393425879704E-31,2.20842887397973E-15,
1.));
#92409=DIRECTION('',(-2.20842887353658E-15,1.,-2.20842887397973E-15));
#92410=DIRECTION('axis',(0.,0.,1.));
#92411=DIRECTION('refdir',(1.,0.,0.));
#92412=DIRECTION('center_axis',(7.17905020382051E-15,1.,7.17905020446514E-15));
#92413=DIRECTION('ref_axis',(8.84265355443813E-30,-7.17905020446514E-15,
1.));
#92414=DIRECTION('center_axis',(7.17905020382051E-15,1.,7.17905020446514E-15));
#92415=DIRECTION('ref_axis',(1.09063096933567E-44,-7.17905020446514E-15,
1.));
#92416=DIRECTION('',(-7.17905020382051E-15,-1.,-7.17905020446514E-15));
#92417=DIRECTION('center_axis',(-7.17905020382051E-15,-1.,-7.17905020446514E-15));
#92418=DIRECTION('ref_axis',(8.84265355443813E-30,-7.17905020446514E-15,
1.));
#92419=DIRECTION('center_axis',(0.,1.,0.));
#92420=DIRECTION('ref_axis',(1.,0.,0.));
#92421=DIRECTION('center_axis',(0.,1.,0.));
#92422=DIRECTION('ref_axis',(1.,0.,0.));
#92423=DIRECTION('',(0.,0.,1.));
#92424=DIRECTION('',(1.,0.,0.));
#92425=DIRECTION('',(0.,0.,1.));
#92426=DIRECTION('',(1.,0.,0.));
#92427=DIRECTION('',(0.,0.,1.));
#92428=DIRECTION('',(1.,0.,0.));
#92429=DIRECTION('',(0.,0.,1.));
#92430=DIRECTION('',(1.,0.,0.));
#92431=DIRECTION('',(0.,0.,1.));
#92432=DIRECTION('',(1.,0.,0.));
#92433=DIRECTION('',(0.,0.,1.));
#92434=DIRECTION('',(1.,0.,0.));
#92435=CARTESIAN_POINT('',(0.,0.,0.));
#92436=CARTESIAN_POINT('',(0.,0.,0.));
#92437=CARTESIAN_POINT('Origin',(2.53163762382963E-15,0.,-3.4647252052902E-15));
#92438=CARTESIAN_POINT('',(-1.76317673760922E-10,0.574924266631643,-7.32492426663165));
#92439=CARTESIAN_POINT('',(1.9876441650041E-12,0.520900163746503,-7.27090016374651));
#92440=CARTESIAN_POINT('',(1.70500103440517E-15,0.,-6.75000000000001));
#92441=CARTESIAN_POINT('',(0.583996965696794,0.655900535579078,-7.3828389043069));
#92442=CARTESIAN_POINT('Ctrl Pts',(-3.52635867725153E-10,0.574924266631643,
-7.32492426663165));
#92443=CARTESIAN_POINT('Ctrl Pts',(0.0689301492338497,0.584602182770183,
-7.33460218277351));
#92444=CARTESIAN_POINT('Ctrl Pts',(0.138003016537344,0.594255597212115,
-7.3432826012457));
#92445=CARTESIAN_POINT('Ctrl Pts',(0.332487077960733,0.621315844934006,
-7.36487180976007));
#92446=CARTESIAN_POINT('Ctrl Pts',(0.458124127164828,0.63865680389821,-7.37549809589609));
#92447=CARTESIAN_POINT('Ctrl Pts',(0.583996965696794,0.655900535579078,
-7.3828389043069));
#92448=CARTESIAN_POINT('',(1.30876848074398,0.552026825468249,-7.18378179160119));
#92449=CARTESIAN_POINT('Ctrl Pts',(1.30876848039644,0.55202682497196,-7.18378179076529));
#92450=CARTESIAN_POINT('Ctrl Pts',(1.27769795963077,0.556534160327731,-7.19402386159478));
#92451=CARTESIAN_POINT('Ctrl Pts',(1.2491031004971,0.56067537123005,-7.20323933174539));
#92452=CARTESIAN_POINT('Ctrl Pts',(1.18971706977311,0.569263221052948,-7.22199063171888));
#92453=CARTESIAN_POINT('Ctrl Pts',(1.15980716658276,0.573581754023551,-7.23122799238887));
#92454=CARTESIAN_POINT('Ctrl Pts',(1.06974174972982,0.586565893247897,-7.25842391824879));
#92455=CARTESIAN_POINT('Ctrl Pts',(1.00941728088563,0.595235853584047,-7.27581144677397));
#92456=CARTESIAN_POINT('Ctrl Pts',(0.82802600490288,0.621229052863817,-7.325626142571));
#92457=CARTESIAN_POINT('Ctrl Pts',(0.706365167342942,0.638561214288606,
-7.35576585694803));
#92458=CARTESIAN_POINT('Ctrl Pts',(0.583996965783454,0.655900535821569,
-7.38283890454329));
#92459=CARTESIAN_POINT('',(1.03955650170316,0.499999998541226,-7.17508343307688));
#92460=CARTESIAN_POINT('Origin',(1.50272086180022,0.00294824858821298,-0.139203625378671));
#92461=CARTESIAN_POINT('',(1.35874712529518,0.544769999507073,-7.16711068668613));
#92462=CARTESIAN_POINT('Origin',(1.03656721497925,0.376341643908494,0.158100836374117));
#92463=CARTESIAN_POINT('',(1.66354985423409,0.499999999722904,-7.05656445327241));
#92464=CARTESIAN_POINT('Ctrl Pts',(1.66354985413997,0.499999999773013,-7.05656445301109));
#92465=CARTESIAN_POINT('Ctrl Pts',(1.61318185067642,0.507497225034372,-7.07614119873178));
#92466=CARTESIAN_POINT('Ctrl Pts',(1.56258951116536,0.514976130334334,-7.0951432142536));
#92467=CARTESIAN_POINT('Ctrl Pts',(1.46066238276572,0.529942096572695,-7.13210508637025));
#92468=CARTESIAN_POINT('Ctrl Pts',(1.40948218992217,0.537396680916625,-7.14998763782684));
#92469=CARTESIAN_POINT('Ctrl Pts',(1.35874712542329,0.544769999785901,-7.16711068694564));
#92470=CARTESIAN_POINT('',(1.4106405155084,0.552026825393108,-7.1644740979145));
#92471=CARTESIAN_POINT('Ctrl Pts',(1.41064051525833,0.552026824820363,-7.16447409806159));
#92472=CARTESIAN_POINT('Ctrl Pts',(1.43304694537867,0.54747794893926,-7.15542619891083));
#92473=CARTESIAN_POINT('Ctrl Pts',(1.45540955657652,0.542929077085632,-7.14626901081486));
#92474=CARTESIAN_POINT('Ctrl Pts',(1.4777268899251,0.538380664762857,-7.13700328942627));
#92475=CARTESIAN_POINT('Ctrl Pts',(1.50004426513297,0.533832243908898,-7.12773755065851));
#92476=CARTESIAN_POINT('Ctrl Pts',(1.52231439379302,0.529279732452209,-7.11835902210837));
#92477=CARTESIAN_POINT('Ctrl Pts',(1.54452808931809,0.524710849011714,-7.10885721603945));
#92478=CARTESIAN_POINT('Ctrl Pts',(1.58437756039739,0.516514662640066,-7.09181178810887));
#92479=CARTESIAN_POINT('Ctrl Pts',(1.62405513566634,0.508277071672323,-7.07437909996789));
#92480=CARTESIAN_POINT('Ctrl Pts',(1.66354985423409,0.499999999722904,-7.05656445327241));
#92481=CARTESIAN_POINT('',(2.15743557081923,0.655900535694669,-7.08469014864916));
#92482=CARTESIAN_POINT('Ctrl Pts',(2.15743557081923,0.655900535694667,-7.08469014864917));
#92483=CARTESIAN_POINT('Ctrl Pts',(2.03373840194332,0.638769108056856,-7.10445036682175));
#92484=CARTESIAN_POINT('Ctrl Pts',(1.90957099987732,0.621541657207324,-7.12099361629952));
#92485=CARTESIAN_POINT('Ctrl Pts',(1.66051231613118,0.586905785277197,-7.14760586946283));
#92486=CARTESIAN_POINT('Ctrl Pts',(1.53566986647824,0.569504150491215,-7.15766947092575));
#92487=CARTESIAN_POINT('Ctrl Pts',(1.41064051535414,0.552026827020548,-7.16447409926013));
#92488=CARTESIAN_POINT('',(2.82247093371176,0.552026825486419,-6.73448243022672));
#92489=CARTESIAN_POINT('Ctrl Pts',(2.82247093304854,0.552026825253083,-6.73448242917092));
#92490=CARTESIAN_POINT('Ctrl Pts',(2.79433186951501,0.556533631550359,-6.75116233153416));
#92491=CARTESIAN_POINT('Ctrl Pts',(2.76838058449236,0.560675802469198,-6.7663129162634));
#92492=CARTESIAN_POINT('Ctrl Pts',(2.71441665085727,0.569263221115838,-6.79739050203923));
#92493=CARTESIAN_POINT('Ctrl Pts',(2.68719178408473,0.573581754079392,-6.8128416433915));
#92494=CARTESIAN_POINT('Ctrl Pts',(2.60507836686489,0.586565893274957,-6.85876314585948));
#92495=CARTESIAN_POINT('Ctrl Pts',(2.54990205531152,0.595235853588861,-6.88871214120141));
#92496=CARTESIAN_POINT('Ctrl Pts',(2.38346029380532,0.621229052810113,-6.9763559594211));
#92497=CARTESIAN_POINT('Ctrl Pts',(2.27112296677513,0.638561214198741,-7.03194450776666));
#92498=CARTESIAN_POINT('Ctrl Pts',(2.1574355708213,0.655900535698362,-7.0846901486524));
#92499=CARTESIAN_POINT('',(2.55768309344323,0.499999998717349,-6.78386005050966));
#92500=CARTESIAN_POINT('Origin',(1.49751296178958,0.0029484005309216,0.187090266587314));
#92501=CARTESIAN_POINT('',(2.86769731163377,0.544769999483455,-6.70745715410932));
#92502=CARTESIAN_POINT('Origin',(0.978346013513691,0.376341857620247,0.377235070553447));
#92503=CARTESIAN_POINT('',(3.14160975116893,0.499999999552296,-6.53397185227299));
#92504=CARTESIAN_POINT('Ctrl Pts',(3.14160975112423,0.499999999567421,-6.53397185220206));
#92505=CARTESIAN_POINT('Ctrl Pts',(3.09662781122098,0.507497213775332,-6.56391849238582));
#92506=CARTESIAN_POINT('Ctrl Pts',(3.05130323285072,0.514976107913629,-6.5933520693833));
#92507=CARTESIAN_POINT('Ctrl Pts',(2.95970745311632,0.529941643027644,-6.65135944187097));
#92508=CARTESIAN_POINT('Ctrl Pts',(2.91356238951158,0.537397143986615,-6.67982962830261));
#92509=CARTESIAN_POINT('Ctrl Pts',(2.86769731188293,0.544769999867499,-6.70745715442048));
#92510=CARTESIAN_POINT('',(2.91781067495167,0.552026825837718,-6.69372666237931));
#92511=CARTESIAN_POINT('Ctrl Pts',(2.91781067507541,0.552026824628134,-6.69372666219399));
#92512=CARTESIAN_POINT('Ctrl Pts',(2.93774822535267,0.547477948549068,-6.68007357702528));
#92513=CARTESIAN_POINT('Ctrl Pts',(2.9576194865856,0.542929076717278,-6.66632317844806));
#92514=CARTESIAN_POINT('Ctrl Pts',(2.97742319707285,0.538380664394361,-6.65247651740689));
#92515=CARTESIAN_POINT('Ctrl Pts',(2.99722694470494,0.533832243540209,-6.63862983039422));
#92516=CARTESIAN_POINT('Ctrl Pts',(3.016960303858,0.529279732005685,-6.62468314711241));
#92517=CARTESIAN_POINT('Ctrl Pts',(3.03661204825892,0.524710848528471,-6.61062819995699));
#92518=CARTESIAN_POINT('Ctrl Pts',(3.07186559686841,0.516514662354408,-6.58541482690274));
#92519=CARTESIAN_POINT('Ctrl Pts',(3.10686801904124,0.508277071627687,-6.55986020013196));
#92520=CARTESIAN_POINT('Ctrl Pts',(3.14160975116893,0.499999999552296,-6.53397185227299));
#92521=CARTESIAN_POINT('',(3.62999488593847,0.655900535633648,-6.45526915564017));
#92522=CARTESIAN_POINT('Ctrl Pts',(3.62999488593847,0.655900535633648,-6.45526915564018));
#92523=CARTESIAN_POINT('Ctrl Pts',(3.51343755102735,0.638769108032714,-6.50115862572389));
#92524=CARTESIAN_POINT('Ctrl Pts',(3.39572942354314,0.621541657210048,-6.54400742428145));
#92525=CARTESIAN_POINT('Ctrl Pts',(3.15821444122951,0.586905785296612,-6.62353775264504));
#92526=CARTESIAN_POINT('Ctrl Pts',(3.03845411560859,0.569504150524582,-6.66020350902869));
#92527=CARTESIAN_POINT('Ctrl Pts',(2.91781067511717,0.552026827043759,-6.6937266636037));
#92528=CARTESIAN_POINT('',(4.20419778449755,0.552026825475761,-5.97028615389083));
#92529=CARTESIAN_POINT('Ctrl Pts',(4.20419778376074,0.552026825178374,-5.97028615316268));
#92530=CARTESIAN_POINT('Ctrl Pts',(4.18030228195419,0.556533631466163,-5.99262515546922));
#92531=CARTESIAN_POINT('Ctrl Pts',(4.15821465144795,0.560675802389299,-6.01300028710299));
#92532=CARTESIAN_POINT('Ctrl Pts',(4.11219312688654,0.569263221052653,-6.05495194678946));
#92533=CARTESIAN_POINT('Ctrl Pts',(4.08892630099689,0.57358175402933,-6.07589439067761));
#92534=CARTESIAN_POINT('Ctrl Pts',(4.01860441540169,0.586565893251218,-6.13839423144815));
#92535=CARTESIAN_POINT('Ctrl Pts',(3.97115624405401,0.595235853575711,-6.17950431192812));
#92536=CARTESIAN_POINT('Ctrl Pts',(3.82744662849934,0.621229052835717,-6.30087912525721));
#92537=CARTESIAN_POINT('Ctrl Pts',(3.72968558033533,0.638561214242502,-6.37931724897332));
#92538=CARTESIAN_POINT('Ctrl Pts',(3.62999488602545,0.655900535752202,-6.45526915572728));
#92539=CARTESIAN_POINT('',(3.95621526506587,0.499999998663635,-6.07543091191077));
#92540=CARTESIAN_POINT('Origin',(1.42228368115469,0.00294854809307285,0.50463567534438));
#92541=CARTESIAN_POINT('',(4.24255715901931,0.544769999394389,-5.93417037980192));
#92542=CARTESIAN_POINT('Origin',(0.874379082447689,0.376342413060157,0.578729547218476));
#92543=CARTESIAN_POINT('',(4.47277146634557,0.499999999622954,-5.70585799046131));
#92544=CARTESIAN_POINT('Ctrl Pts',(4.472771466155,0.499999999667942,-5.70585799041082));
#92545=CARTESIAN_POINT('Ctrl Pts',(4.43527881819098,0.507497214479082,-5.74477428551586));
#92546=CARTESIAN_POINT('Ctrl Pts',(4.39734124892664,0.514976109242423,-5.78326316956504));
#92547=CARTESIAN_POINT('Ctrl Pts',(4.32035680324058,0.529941643282175,-5.85960474175593));
#92548=CARTESIAN_POINT('Ctrl Pts',(4.28141083079792,0.53739714477637,-5.89732913864258));
#92549=CARTESIAN_POINT('Ctrl Pts',(4.24255715940239,0.544769999868629,-5.93417038011102));
#92550=CARTESIAN_POINT('',(4.28854724969871,0.552026825667153,-5.90998800741621));
#92551=CARTESIAN_POINT('Ctrl Pts',(4.28854724980574,0.552026824741665,-5.9099880073423));
#92552=CARTESIAN_POINT('Ctrl Pts',(4.3050836615186,0.547477948841813,-5.89236814036842));
#92553=CARTESIAN_POINT('Ctrl Pts',(4.32153441435246,0.542929076963385,-5.87466748472589));
#92554=CARTESIAN_POINT('Ctrl Pts',(4.33789850212508,0.53838066456022,-5.85688733857809));
#92555=CARTESIAN_POINT('Ctrl Pts',(4.35426262059039,0.533832243625994,-5.83910715908161));
#92556=CARTESIAN_POINT('Ctrl Pts',(4.37053650011405,0.529279732161267,-5.82124445270268));
#92557=CARTESIAN_POINT('Ctrl Pts',(4.3867073994258,0.524710848714242,-5.80329355833596));
#92558=CARTESIAN_POINT('Ctrl Pts',(4.41571660990344,0.516514662527723,-5.77109118894962));
#92559=CARTESIAN_POINT('Ctrl Pts',(4.44440720567689,0.508277071788115,-5.73860952892666));
#92560=CARTESIAN_POINT('Ctrl Pts',(4.47277146634557,0.499999999622954,-5.70585799046131));
#92561=CARTESIAN_POINT('',(4.93281967474729,0.655900535551958,-5.52400695138184));
#92562=CARTESIAN_POINT('Ctrl Pts',(4.93281967474729,0.655900535551957,-5.52400695138184));
#92563=CARTESIAN_POINT('Ctrl Pts',(4.82885226510583,0.638769107953755,-5.5938799327855));
#92564=CARTESIAN_POINT('Ctrl Pts',(4.72310731328421,0.621541657142716,-5.66103071826921));
#92565=CARTESIAN_POINT('Ctrl Pts',(4.50824196910535,0.586905785269717,-5.78976037198936));
#92566=CARTESIAN_POINT('Ctrl Pts',(4.39916362665628,0.569504150421789,-5.85131383354925));
#92567=CARTESIAN_POINT('Ctrl Pts',(4.28854725022243,0.55202682693946,-5.90998800878253));
#92568=CARTESIAN_POINT('',(5.38934101926066,0.552026825436104,-4.9269259328291));
#92569=CARTESIAN_POINT('Ctrl Pts',(5.38934101841487,0.552026825142794,-4.92692593229653));
#92570=CARTESIAN_POINT('Ctrl Pts',(5.37080640526157,0.556533631450834,-4.95387948778111));
#92571=CARTESIAN_POINT('Ctrl Pts',(5.35361522227531,0.560675802385154,-4.97852644785407));
#92572=CARTESIAN_POINT('Ctrl Pts',(5.31768802211116,0.569263221065196,-5.02939056849044));
#92573=CARTESIAN_POINT('Ctrl Pts',(5.29946716807536,0.573581754044685,-5.05484506947216));
#92574=CARTESIAN_POINT('Ctrl Pts',(5.24422498739726,0.586565893277644,-5.13100082538544));
#92575=CARTESIAN_POINT('Ctrl Pts',(5.20672358004069,0.595235853610458,-5.18134972930647));
#92576=CARTESIAN_POINT('Ctrl Pts',(5.09246581254656,0.621229052890819,-5.33078018623515));
#92577=CARTESIAN_POINT('Ctrl Pts',(5.01385224139044,0.638561214308336,-5.42840020573969));
#92578=CARTESIAN_POINT('Ctrl Pts',(4.93281967498493,0.655900535823712,-5.52400695153397));
#92579=CARTESIAN_POINT('',(5.16975920818102,0.499999998549721,-5.08292137660211));
#92580=CARTESIAN_POINT('Origin',(1.28054877109914,0.00294807119520506,0.798587994577735));
#92581=CARTESIAN_POINT('',(5.41903974963537,0.544769999481502,-4.8834083934489));
#92582=CARTESIAN_POINT('Origin',(0.729525470119463,0.376341730165788,0.753166654253201));
#92583=CARTESIAN_POINT('',(5.5947913592018,0.499999999550736,-4.61094454995047));
#92584=CARTESIAN_POINT('Ctrl Pts',(5.59479135904148,0.499999999587741,-4.61094454996122));
#92585=CARTESIAN_POINT('Ctrl Pts',(5.56654112187797,0.507497214329946,-4.65701081411809));
#92586=CARTESIAN_POINT('Ctrl Pts',(5.53776448467522,0.514976108986996,-4.7027553047835));
#92587=CARTESIAN_POINT('Ctrl Pts',(5.47899107359703,0.529941643074257,-4.79386143408856));
#92588=CARTESIAN_POINT('Ctrl Pts',(5.4490652670489,0.537397144438014,-4.83907608766772));
#92589=CARTESIAN_POINT('Ctrl Pts',(5.41903974987221,0.544769999736433,-4.88340839356691));
#92590=CARTESIAN_POINT('',(5.45875612184271,0.552026825349422,-4.84990488204123));
#92591=CARTESIAN_POINT('Ctrl Pts',(5.45875612172105,0.552026824787737,-4.84990488225974));
#92592=CARTESIAN_POINT('Ctrl Pts',(5.47111817039548,0.547477948904059,-4.82914211851112));
#92593=CARTESIAN_POINT('Ctrl Pts',(5.48337919604398,0.542929077052408,-4.80831886881669));
#92594=CARTESIAN_POINT('Ctrl Pts',(5.49553849473922,0.538380664711329,-4.78743661749974));
#92595=CARTESIAN_POINT('Ctrl Pts',(5.50769781624091,0.533832243839075,-4.76655432701525));
#92596=CARTESIAN_POINT('Ctrl Pts',(5.51975126758095,0.529279732320647,-4.74561083774347));
#92597=CARTESIAN_POINT('Ctrl Pts',(5.53168518856306,0.52471084886393,-4.72460335998809));
#92598=CARTESIAN_POINT('Ctrl Pts',(5.55309362269106,0.516514662491629,-4.68691774061822));
#92599=CARTESIAN_POINT('Ctrl Pts',(5.57413085193685,0.508277071597412,-4.64902785301941));
#92600=CARTESIAN_POINT('Ctrl Pts',(5.5947913592018,0.499999999550736,-4.61094454995047));
#92601=CARTESIAN_POINT('',(6.00499129856053,0.655900535637417,-4.33444832106312));
#92602=CARTESIAN_POINT('Ctrl Pts',(6.00499129856054,0.655900535637417,-4.33444832106312));
#92603=CARTESIAN_POINT('Ctrl Pts',(5.91847521462983,0.638769108018161,-4.42503763096437));
#92604=CARTESIAN_POINT('Ctrl Pts',(5.82963795480512,0.621541657186257,-4.51335050739163));
#92605=CARTESIAN_POINT('Ctrl Pts',(5.64746911313381,0.586905785286544,-4.68526023114174));
#92606=CARTESIAN_POINT('Ctrl Pts',(5.55417313630222,0.569504150412454,-4.76882322639795));
#92607=CARTESIAN_POINT('Ctrl Pts',(5.45875612252139,0.552026826918684,-4.84990488317817));
#92608=CARTESIAN_POINT('',(6.32248465789244,0.552026825409836,-3.65318813103928));
#92609=CARTESIAN_POINT('Ctrl Pts',(6.32248465691362,0.552026825139949,-3.65318813068195));
#92610=CARTESIAN_POINT('Ctrl Pts',(6.31017759038344,0.556533631445669,-3.68349592099771));
#92611=CARTESIAN_POINT('Ctrl Pts',(6.29868669552113,0.560675802386554,-3.71126224509254));
#92612=CARTESIAN_POINT('Ctrl Pts',(6.27453373572314,0.569263221059156,-3.76866047689442));
#92613=CARTESIAN_POINT('Ctrl Pts',(6.26221084042521,0.573581754029174,-3.7974368107589));
#92614=CARTESIAN_POINT('Ctrl Pts',(6.22463142764196,0.586565893240533,-3.88368752321914));
#92615=CARTESIAN_POINT('Ctrl Pts',(6.19883030841442,0.595235853563861,-3.94092099173871));
#92616=CARTESIAN_POINT('Ctrl Pts',(6.11936695523834,0.621229052814039,-4.11141988999875));
#92617=CARTESIAN_POINT('Ctrl Pts',(6.06357674434361,0.638561214214636,-4.22365720154951));
#92618=CARTESIAN_POINT('Ctrl Pts',(6.00499129862453,0.655900535703095,-4.33444832108668));
#92619=CARTESIAN_POINT('',(6.14157095730116,0.499999998704437,-3.85274008577389));
#92620=CARTESIAN_POINT('Origin',(1.07893795822326,0.00294795557416398,1.05519716394546));
#92621=CARTESIAN_POINT('',(6.34213406351935,0.544769999517614,-3.60430365899014));
#92622=CARTESIAN_POINT('Origin',(0.550561489189073,0.376341714602447,0.892384071056311));
#92623=CARTESIAN_POINT('',(6.45520502561422,0.499999999749251,-3.30042846896563));
#92624=CARTESIAN_POINT('Ctrl Pts',(6.45520502526096,0.499999999833995,-3.30042846906863));
#92625=CARTESIAN_POINT('Ctrl Pts',(6.43751814586516,0.507497215429968,-3.35149070156539));
#92626=CARTESIAN_POINT('Ctrl Pts',(6.41924800134489,0.514976110955304,-3.40235184376848));
#92627=CARTESIAN_POINT('Ctrl Pts',(6.38143380907499,0.529941643395797,-3.50396249680085));
#92628=CARTESIAN_POINT('Ctrl Pts',(6.36192746817965,0.537397143637598,-3.55455321319428));
#92629=CARTESIAN_POINT('Ctrl Pts',(6.34213406386358,0.54476999985951,-3.60430365907642));
#92630=CARTESIAN_POINT('',(6.37371962476082,0.55202682565524,-3.56304559389542));
#92631=CARTESIAN_POINT('Ctrl Pts',(6.37371962481441,0.552026824684896,-3.56304559376603));
#92632=CARTESIAN_POINT('Ctrl Pts',(6.38132927556718,0.547477948641283,-3.54011077625578));
#92633=CARTESIAN_POINT('Ctrl Pts',(6.38882726203103,0.54292907673752,-3.51713860448545));
#92634=CARTESIAN_POINT('Ctrl Pts',(6.39621321628672,0.53838066437267,-3.4941306788099));
#92635=CARTESIAN_POINT('Ctrl Pts',(6.40359918439574,0.533832243476672,-3.47112270997995));
#92636=CARTESIAN_POINT('Ctrl Pts',(6.41086860168613,0.529279732017064,-3.44807773212331));
#92637=CARTESIAN_POINT('Ctrl Pts',(6.4180075274815,0.524710848564556,-3.42499595728427));
#92638=CARTESIAN_POINT('Ctrl Pts',(6.43081414986407,0.516514662364648,-3.38358922709044));
#92639=CARTESIAN_POINT('Ctrl Pts',(6.44321433424654,0.508277071581048,-3.3420628024185));
#92640=CARTESIAN_POINT('Ctrl Pts',(6.45520502561422,0.499999999749251,-3.30042846896563));
#92641=CARTESIAN_POINT('',(6.79637620244565,0.655900535687991,-2.94221570577926));
#92642=CARTESIAN_POINT('Ctrl Pts',(6.79637620244565,0.655900535687989,-2.94221570577926));
#92643=CARTESIAN_POINT('Ctrl Pts',(6.73135684041582,0.638769108082005,-3.04928548835663));
#92644=CARTESIAN_POINT('Ctrl Pts',(6.66358120439581,0.621541657260411,-3.1546310434227));
#92645=CARTESIAN_POINT('Ctrl Pts',(6.52262687807457,0.586905785341988,-3.36168252926548));
#92646=CARTESIAN_POINT('Ctrl Pts',(6.44947568356735,0.569504150535565,-3.46334774481967));
#92647=CARTESIAN_POINT('Ctrl Pts',(6.37371962594718,0.552026827017802,-3.56304559503574));
#92648=CARTESIAN_POINT('',(6.95999594072217,0.552026825409201,-2.20863131313051));
#92649=CARTESIAN_POINT('Ctrl Pts',(6.95999593957526,0.552026825171655,-2.20863131296794));
#92650=CARTESIAN_POINT('Ctrl Pts',(6.95449188441449,0.556533631512047,-2.24087617970752));
#92651=CARTESIAN_POINT('Ctrl Pts',(6.94923857920949,0.560675802451137,-2.27046354526051));
#92652=CARTESIAN_POINT('Ctrl Pts',(6.93798922534277,0.56926322113458,-2.33171201072628));
#92653=CARTESIAN_POINT('Ctrl Pts',(6.93214049364807,0.573581754106621,-2.36246462811705));
#92654=CARTESIAN_POINT('Ctrl Pts',(6.91398102027849,0.586565893322721,-2.45477730974309));
#92655=CARTESIAN_POINT('Ctrl Pts',(6.90108662080075,0.595235853647109,-2.51621916952215));
#92656=CARTESIAN_POINT('Ctrl Pts',(6.86013329986852,0.621229052897615,-2.69981417027227));
#92657=CARTESIAN_POINT('Ctrl Pts',(6.82977513736429,0.638561214294452,-2.82142068202551));
#92658=CARTESIAN_POINT('Ctrl Pts',(6.79637620254562,0.655900535785162,-2.94221570579295));
#92659=CARTESIAN_POINT('',(6.82620967333585,0.499999998625506,-2.44240895193039));
#92660=CARTESIAN_POINT('Origin',(0.826874931113843,0.0029480911267165,1.26246803930745));
#92661=CARTESIAN_POINT('',(6.96867723761365,0.544769999414902,-2.15666569090553));
#92662=CARTESIAN_POINT('Origin',(0.34585306664821,0.37634159742266,0.989875282359732));
#92663=CARTESIAN_POINT('',(7.01378048014667,0.499999999730478,-1.83558801947582));
#92664=CARTESIAN_POINT('Ctrl Pts',(7.01378047986532,0.499999999781752,-1.83558801943565));
#92665=CARTESIAN_POINT('Ctrl Pts',(7.0074839724311,0.507497224995949,-1.88925867030701));
#92666=CARTESIAN_POINT('Ctrl Pts',(7.00057460313458,0.514976130331124,-1.94285831627193));
#92667=CARTESIAN_POINT('Ctrl Pts',(6.98548733490655,0.529942096784993,-2.0502254160513));
#92668=CARTESIAN_POINT('Ctrl Pts',(6.97731355020339,0.537396681043757,-2.10382007041908));
#92669=CARTESIAN_POINT('Ctrl Pts',(6.96867723809537,0.544769999879199,-2.15666569091947));
#92670=CARTESIAN_POINT('',(6.99065508180253,0.552026825728037,-2.10958225482661));
#92671=CARTESIAN_POINT('Ctrl Pts',(6.99065508186297,0.552026824743019,-2.10958225470308));
#92672=CARTESIAN_POINT('Ctrl Pts',(6.99315651518471,0.54747794885825,-2.08554779102925));
#92673=CARTESIAN_POINT('Ctrl Pts',(6.99554086502014,0.542929076980459,-2.06150085049816));
#92674=CARTESIAN_POINT('Ctrl Pts',(6.99780811579523,0.538380664575027,-2.03744307558802));
#92675=CARTESIAN_POINT('Ctrl Pts',(7.00007537082278,0.533832243638573,-2.01338525555501));
#92676=CARTESIAN_POINT('Ctrl Pts',(7.00222084418056,0.529279732233542,-1.98931634671837));
#92677=CARTESIAN_POINT('Ctrl Pts',(7.00423096656736,0.524710848805729,-1.9652395530089));
#92678=CARTESIAN_POINT('Ctrl Pts',(7.00783695425831,0.516514662588317,-1.92204784372608));
#92679=CARTESIAN_POINT('Ctrl Pts',(7.01102027544683,0.508277071769268,-1.8788266105124));
#92680=CARTESIAN_POINT('Ctrl Pts',(7.01378048014667,0.499999999730478,-1.83558801947582));
#92681=CARTESIAN_POINT('',(7.26997010890117,0.655900535569512,-1.41240835399411));
#92682=CARTESIAN_POINT('Ctrl Pts',(7.26997010890117,0.655900535569511,-1.41240835399411));
#92683=CARTESIAN_POINT('Ctrl Pts',(7.22948770171035,0.638769107957234,-1.53095214539221));
#92684=CARTESIAN_POINT('Ctrl Pts',(7.18594280275067,0.621541657141611,-1.64840453819461));
#92685=CARTESIAN_POINT('Ctrl Pts',(7.09279385932106,0.586905785257705,-1.88091628896775));
#92686=CARTESIAN_POINT('Ctrl Pts',(7.04320791534452,0.56950415051741,-1.99592997258257));
#92687=CARTESIAN_POINT('Ctrl Pts',(6.99065508302971,0.55202682705447,-2.10958225559804));
#92688=CARTESIAN_POINT('',(7.27206554910829,0.552026825471009,-0.660801348883197));
#92689=CARTESIAN_POINT('Ctrl Pts',(7.27206554792705,0.552026825214658,-0.660801348974819));
#92690=CARTESIAN_POINT('Ctrl Pts',(7.27362186768549,0.556533631496471,-0.693475557498244));
#92691=CARTESIAN_POINT('Ctrl Pts',(7.27485179082325,0.560675802417086,-0.723500492177397));
#92692=CARTESIAN_POINT('Ctrl Pts',(7.27703205016235,0.569263221067812,-0.785735281041659));
#92693=CARTESIAN_POINT('Ctrl Pts',(7.27793096225669,0.573581754037214,-0.817026223809206));
#92694=CARTESIAN_POINT('Ctrl Pts',(7.28004054507349,0.586565893251948,-0.911084436407912));
#92695=CARTESIAN_POINT('Ctrl Pts',(7.28065579312523,0.595235853581284,-0.973861734512161));
#92696=CARTESIAN_POINT('Ctrl Pts',(7.28012743618024,0.621229052846323,-1.16196813994222));
#92697=CARTESIAN_POINT('Ctrl Pts',(7.27662083598705,0.638561214260605,-1.28725766680698));
#92698=CARTESIAN_POINT('Ctrl Pts',(7.26997010909109,0.655900535753017,-1.41240835397878));
#92699=CARTESIAN_POINT('',(7.19166241188204,0.499999998583707,-0.917873489931604));
#92700=CARTESIAN_POINT('Origin',(0.536150814127319,0.00294833248163803,
1.41070552616189));
#92701=CARTESIAN_POINT('',(7.2693728092005,0.544769999340984,-0.608184432669663));
#92702=CARTESIAN_POINT('Origin',(0.124973750232958,0.376341620246457,1.04108062069729));
#92703=CARTESIAN_POINT('',(7.24439935455547,0.499999999619592,-0.284917513379212));
#92704=CARTESIAN_POINT('Ctrl Pts',(7.24439935438015,0.499999999673154,-0.284917513532033));
#92705=CARTESIAN_POINT('Ctrl Pts',(7.24978765199808,0.507497214783673,-0.338686864437686));
#92706=CARTESIAN_POINT('Ctrl Pts',(7.25456215704695,0.514976109782808,-0.39251861742014));
#92707=CARTESIAN_POINT('Ctrl Pts',(7.2629083902048,0.529942106270729,-0.500619067978217));
#92708=CARTESIAN_POINT('Ctrl Pts',(7.26644697143727,0.537396701243088,-0.554717907480788));
#92709=CARTESIAN_POINT('Ctrl Pts',(7.26937280977078,0.544769999900244,-0.60818443256133));
#92710=CARTESIAN_POINT('',(7.28071527694886,0.552026825363792,-0.557477194078559));
#92711=CARTESIAN_POINT('Ctrl Pts',(7.28071527697879,0.552026824732173,-0.557477194257984));
#92712=CARTESIAN_POINT('Ctrl Pts',(7.2779915286716,0.547477948852738,-0.533466909036562));
#92713=CARTESIAN_POINT('Ctrl Pts',(7.27515075242188,0.542929077057373,-0.509469607951223));
#92714=CARTESIAN_POINT('Ctrl Pts',(7.27219328578453,0.538380664766051,-0.485486898614203));
#92715=CARTESIAN_POINT('Ctrl Pts',(7.26923581360006,0.533832243943573,-0.461504144294403));
#92716=CARTESIAN_POINT('Ctrl Pts',(7.26615702303958,0.529279732525729,-0.437536739919708));
#92717=CARTESIAN_POINT('Ctrl Pts',(7.26294435094913,0.524710849108655,-0.413590731466844));
#92718=CARTESIAN_POINT('Ctrl Pts',(7.25718109175257,0.516514662684973,-0.37063363856986));
#92719=CARTESIAN_POINT('Ctrl Pts',(7.25099870095614,0.508277071644545,-0.327738572807507));
#92720=CARTESIAN_POINT('Ctrl Pts',(7.24439935455547,0.499999999619592,-0.284917513379212));
#92721=CARTESIAN_POINT('',(7.40362829346862,0.655900535690581,0.183441643835477));
#92722=CARTESIAN_POINT('Ctrl Pts',(7.40362829346862,0.655900535690581,0.183441643835477));
#92723=CARTESIAN_POINT('Ctrl Pts',(7.38957575348522,0.638769108062214,0.0589668192730024));
#92724=CARTESIAN_POINT('Ctrl Pts',(7.37229770263256,0.621541657222824,-0.0651004681833282));
#92725=CARTESIAN_POINT('Ctrl Pts',(7.33130968310938,0.586905785298123,-0.312200493074654));
#92726=CARTESIAN_POINT('Ctrl Pts',(7.30760757306436,0.569504150497685,-0.435184733230779));
#92727=CARTESIAN_POINT('Ctrl Pts',(7.28071527804253,0.552026827009743,-0.55747719455429));
#92728=CARTESIAN_POINT('',(7.24410145461844,0.552026825475149,0.917926951901574));
#92729=CARTESIAN_POINT('Ctrl Pts',(7.24410145346206,0.55202682523426,0.917926951554292));
#92730=CARTESIAN_POINT('Ctrl Pts',(7.25264537636084,0.556533631539689,0.886351210476089));
#92731=CARTESIAN_POINT('Ctrl Pts',(7.26030101799742,0.560675802457701,0.857292639234557));
#92732=CARTESIAN_POINT('Ctrl Pts',(7.27580894404161,0.569263221108155,0.796981556471936));
#92733=CARTESIAN_POINT('Ctrl Pts',(7.28341346780423,0.573581754072734,0.766615418115779));
#92734=CARTESIAN_POINT('Ctrl Pts',(7.30569346508482,0.586565893267273,0.675209732313252));
#92735=CARTESIAN_POINT('Ctrl Pts',(7.31978959236433,0.59523585357835,0.61403239277492));
#92736=CARTESIAN_POINT('Ctrl Pts',(7.35971090483336,0.621229052790785,0.430210229646323));
#92737=CARTESIAN_POINT('Ctrl Pts',(7.38321983171316,0.638561214167953,0.307096087032365));
#92738=CARTESIAN_POINT('Ctrl Pts',(7.40362829342209,0.655900535643713,0.183441643821226));
#92739=CARTESIAN_POINT('',(7.2208410099847,0.499999998929002,0.649580717715866));
#92740=CARTESIAN_POINT('Origin',(0.22035445450171,0.00294810763189539,1.4929807488716));
#92741=CARTESIAN_POINT('',(7.23016058784143,0.544769999493435,0.968734855124911));
#92742=CARTESIAN_POINT('Origin',(-0.101750885626912,0.376341834536014,1.04360639317965));
#92743=CARTESIAN_POINT('',(7.13627816756703,0.499999999904053,1.27907541649017));
#92744=CARTESIAN_POINT('Ctrl Pts',(7.13627816725196,0.500000000026025,1.27907541606446));
#92745=CARTESIAN_POINT('Ctrl Pts',(7.15309931318004,0.507497216258348,1.22772147873973));
#92746=CARTESIAN_POINT('Ctrl Pts',(7.16933443097523,0.51497611249203,1.17617465097858));
#92747=CARTESIAN_POINT('Ctrl Pts',(7.20072392982272,0.529942106403902,1.07239574048342));
#92748=CARTESIAN_POINT('Ctrl Pts',(7.21580943246971,0.53739670147069,1.02032239166843));
#92749=CARTESIAN_POINT('Ctrl Pts',(7.23016058818354,0.544769999851955,0.968734855271326));
#92750=CARTESIAN_POINT('',(7.2303373171918,0.552026825426371,1.02069488145051));
#92751=CARTESIAN_POINT('Ctrl Pts',(7.23033731739115,0.552026824912483,1.02069488110041));
#92752=CARTESIAN_POINT('Ctrl Pts',(7.2225157476636,0.547477949056865,1.04355829362695));
#92753=CARTESIAN_POINT('Ctrl Pts',(7.2145826766603,0.542929077162653,1.06638386853634));
#92754=CARTESIAN_POINT('Ctrl Pts',(7.20653878020542,0.538380664759786,1.08917010785261));
#92755=CARTESIAN_POINT('Ctrl Pts',(7.19849486866308,0.533832243825735,1.11195638990767));
#92756=CARTESIAN_POINT('Ctrl Pts',(7.19033577487136,0.529279732284339,1.13470160101827));
#92757=CARTESIAN_POINT('Ctrl Pts',(7.18205052914418,0.524710848777189,1.15739713587703));
#92758=CARTESIAN_POINT('Ctrl Pts',(7.16718750679986,0.516514662461003,1.19811098466673));
#92759=CARTESIAN_POINT('Ctrl Pts',(7.15192848598662,0.508277071585678,1.23867415561305));
#92760=CARTESIAN_POINT('Ctrl Pts',(7.13627816756703,0.499999999904053,1.27907541649017));
#92761=CARTESIAN_POINT('',(7.19110104737666,0.655900535702375,1.77071411332688));
#92762=CARTESIAN_POINT('Ctrl Pts',(7.19110104737667,0.655900535702375,1.77071411332688));
#92763=CARTESIAN_POINT('Ctrl Pts',(7.20413545578322,0.638769108080208,1.64612856036365));
#92764=CARTESIAN_POINT('Ctrl Pts',(7.2139321555394,0.621541657239082,1.52124762701307));
#92765=CARTESIAN_POINT('Ctrl Pts',(7.22702161423002,0.586905785309721,1.27111345093031));
#92766=CARTESIAN_POINT('Ctrl Pts',(7.23031162257484,0.569504150532731,1.14590926119869));
#92767=CARTESIAN_POINT('Ctrl Pts',(7.2303373187043,0.552026827039748,1.02069488122563));
#92768=CARTESIAN_POINT('',(6.87741122726476,0.552026825413561,2.45373400825514));
#92769=CARTESIAN_POINT('Ctrl Pts',(6.8774112262582,0.552026825174671,2.45373400769281));
#92770=CARTESIAN_POINT('Ctrl Pts',(6.89254324801281,0.5565336315074,2.42473318065509));
#92771=CARTESIAN_POINT('Ctrl Pts',(6.90626663890515,0.560675802448533,2.39799971923227));
#92772=CARTESIAN_POINT('Ctrl Pts',(6.93437709832155,0.569263221131459,2.34243242168606));
#92773=CARTESIAN_POINT('Ctrl Pts',(6.94833165467528,0.573581754104273,2.31441097460743));
#92774=CARTESIAN_POINT('Ctrl Pts',(6.98974027851822,0.586565893323153,2.22993184381712));
#92775=CARTESIAN_POINT('Ctrl Pts',(7.01665816578896,0.595235853649897,2.17321504719998));
#92776=CARTESIAN_POINT('Ctrl Pts',(7.09516247148734,0.621229052902576,2.00227244630821));
#92777=CARTESIAN_POINT('Ctrl Pts',(7.14458767415175,0.638561214298158,1.88709036835596));
#92778=CARTESIAN_POINT('Ctrl Pts',(7.19110104743979,0.65590053577218,1.77071411336251));
#92779=CARTESIAN_POINT('',(6.91238110673581,0.499999998645691,2.18666125139118));
#92780=CARTESIAN_POINT('Origin',(-0.105743174771213,0.00294783977492552,
1.5054455554018));
#92781=CARTESIAN_POINT('',(6.85287409290266,0.544769999392285,2.50035717665643));
#92782=CARTESIAN_POINT('Origin',(-0.323715934329361,0.376341767018527,0.997334149364529));
#92783=CARTESIAN_POINT('',(6.69447254313508,0.499999999636659,2.78326020476335));
#92784=CARTESIAN_POINT('Ctrl Pts',(6.69447254303287,0.499999999694329,2.78326020453475));
#92785=CARTESIAN_POINT('Ctrl Pts',(6.72193999413843,0.507497214796774,2.73672295029177));
#92786=CARTESIAN_POINT('Ctrl Pts',(6.74887658417363,0.514976109836711,2.68987133664889));
#92787=CARTESIAN_POINT('Ctrl Pts',(6.80184162063874,0.529942106161782,2.59526651846583));
#92788=CARTESIAN_POINT('Ctrl Pts',(6.82776866093176,0.53739670052164,2.54765355736703));
#92789=CARTESIAN_POINT('Ctrl Pts',(6.85287409329062,0.544769999851891,2.50035717693401));
#92790=CARTESIAN_POINT('',(6.84187682086182,0.552026825706407,2.55114039807484));
#92791=CARTESIAN_POINT('Ctrl Pts',(6.84187682083898,0.552026824711191,2.55114039821205));
#92792=CARTESIAN_POINT('Ctrl Pts',(6.82932315673046,0.547477948795513,2.57178787122331));
#92793=CARTESIAN_POINT('Ctrl Pts',(6.81666873272011,0.542929076939321,2.5923744209764));
#92794=CARTESIAN_POINT('Ctrl Pts',(6.80391453028886,0.538380664576819,2.61289873058665));
#92795=CARTESIAN_POINT('Ctrl Pts',(6.79116030393554,0.533832243683208,2.63342307869278));
#92796=CARTESIAN_POINT('Ctrl Pts',(6.77830241727891,0.529279732193272,2.65388255530014));
#92797=CARTESIAN_POINT('Ctrl Pts',(6.76533200698369,0.524710848747534,2.67426639813));
#92798=CARTESIAN_POINT('Ctrl Pts',(6.74206420002228,0.516514662534077,2.71083326913107));
#92799=CARTESIAN_POINT('Ctrl Pts',(6.71844204411595,0.508277071780336,2.74716785710491));
#92800=CARTESIAN_POINT('Ctrl Pts',(6.69447254313508,0.499999999636659,2.78326020476335));
#92801=CARTESIAN_POINT('',(6.64232590877187,0.655900535624813,3.27518995864757));
#92802=CARTESIAN_POINT('Ctrl Pts',(6.64232590877187,0.655900535624812,3.27518995864757));
#92803=CARTESIAN_POINT('Ctrl Pts',(6.68183779107667,0.638769108022223,3.15631915930124));
#92804=CARTESIAN_POINT('Ctrl Pts',(6.71825115862536,0.621541657210669,3.0364638737519));
#92805=CARTESIAN_POINT('Ctrl Pts',(6.78480604698142,0.586905785313935,2.79499154249107));
#92806=CARTESIAN_POINT('Ctrl Pts',(6.81493433654931,0.569504150542412,2.67342181166954));
#92807=CARTESIAN_POINT('Ctrl Pts',(6.84187682229732,0.552026827040526,2.55114039820044));
#92808=CARTESIAN_POINT('',(6.1891408947314,0.552026825513628,3.8748071900381));
#92809=CARTESIAN_POINT('Ctrl Pts',(6.18914089379959,0.552026825263855,3.8748071892122));
#92810=CARTESIAN_POINT('Ctrl Pts',(6.21015345762421,0.556533631536028,3.84973732301981));
#92811=CARTESIAN_POINT('Ctrl Pts',(6.22930290716358,0.560675802450135,3.82657899851928));
#92812=CARTESIAN_POINT('Ctrl Pts',(6.26870148598491,0.569263221090252,3.77835375142444));
#92813=CARTESIAN_POINT('Ctrl Pts',(6.28835357540481,0.573581754057455,3.75398724728214));
#92814=CARTESIAN_POINT('Ctrl Pts',(6.3469546046639,0.586565893266171,3.68038482155418));
#92815=CARTESIAN_POINT('Ctrl Pts',(6.3854356014944,0.595235853590531,3.63078058208177));
#92816=CARTESIAN_POINT('Ctrl Pts',(6.49885212650631,0.621229052846318,3.48071062903566));
#92817=CARTESIAN_POINT('Ctrl Pts',(6.5718825375239,0.638561214261876,3.37884640143506));
#92818=CARTESIAN_POINT('Ctrl Pts',(6.64232590890062,0.655900535791303,3.27518995876292));
#92819=CARTESIAN_POINT('',(6.28070594613547,0.499999998589842,3.62149593535559));
#92820=CARTESIAN_POINT('Origin',(-0.426897292137384,0.00294846562083999,
1.44751727326905));
#92821=CARTESIAN_POINT('',(6.15515482210084,0.544769999370239,3.91506557539984));
#92822=CARTESIAN_POINT('Origin',(-0.53054502599663,0.376341896131434,0.904427643646886));
#92823=CARTESIAN_POINT('',(5.93964082487683,0.499999999760686,4.15730283636664));
#92824=CARTESIAN_POINT('Ctrl Pts',(5.93964082464481,0.499999999816603,4.15730283616115));
#92825=CARTESIAN_POINT('Ctrl Pts',(5.97647028641283,0.507497225167955,4.11775823300134));
#92826=CARTESIAN_POINT('Ctrl Pts',(6.01284887255721,0.514976130663546,4.07779249736097));
#92827=CARTESIAN_POINT('Ctrl Pts',(6.08491270977972,0.529942096794905,3.9967855680827));
#92828=CARTESIAN_POINT('Ctrl Pts',(6.12046892415114,0.537396680762836,3.95585937707875));
#92829=CARTESIAN_POINT('Ctrl Pts',(6.15515482248417,0.544769999922148,3.91506557582553));
#92830=CARTESIAN_POINT('',(6.13349776832425,0.552026825402507,3.962297425611));
#92831=CARTESIAN_POINT('Ctrl Pts',(6.13349776847326,0.552026824802072,3.96229742541378));
#92832=CARTESIAN_POINT('Ctrl Pts',(6.11679900578816,0.547477948809804,3.97976350511362));
#92833=CARTESIAN_POINT('Ctrl Pts',(6.10001493530689,0.542929076865411,3.99714842583357));
#92834=CARTESIAN_POINT('Ctrl Pts',(6.08314679897251,0.538380664438636,4.01445111215885));
#92835=CARTESIAN_POINT('Ctrl Pts',(6.06627863099977,0.533832243480725,4.03175383093755));
#92836=CARTESIAN_POINT('Ctrl Pts',(6.04932317173958,0.529279731995422,4.04897091103435));
#92837=CARTESIAN_POINT('Ctrl Pts',(6.03227407857486,0.524710848504994,4.06608993632827));
#92838=CARTESIAN_POINT('Ctrl Pts',(6.00168946366319,0.516514662304296,4.09680000349837));
#92839=CARTESIAN_POINT('Ctrl Pts',(5.97080871823432,0.508277071501415,4.12720704368692));
#92840=CARTESIAN_POINT('Ctrl Pts',(5.93964082487683,0.499999999760686,4.15730283636664));
#92841=CARTESIAN_POINT('',(5.7829629925841,0.65590053576872,4.62652156291335));
#92842=CARTESIAN_POINT('Ctrl Pts',(5.7829629925841,0.65590053576872,4.62652156291335));
#92843=CARTESIAN_POINT('Ctrl Pts',(5.84710481719915,0.638769108144735,4.51892378339903));
#92844=CARTESIAN_POINT('Ctrl Pts',(5.90843220401921,0.621541657296678,4.40969844533471));
#92845=CARTESIAN_POINT('Ctrl Pts',(6.02534048954105,0.586905785338163,4.18817893639138));
#92846=CARTESIAN_POINT('Ctrl Pts',(6.08089829496035,0.569504150567409,4.07592813004998));
#92847=CARTESIAN_POINT('Ctrl Pts',(6.13349776971531,0.552026827065365,3.96229742599917));
#92848=CARTESIAN_POINT('',(5.21147321258346,0.552026825488821,5.11469869387848));
#92849=CARTESIAN_POINT('Ctrl Pts',(5.21147321185043,0.552026825253602,5.11469869287415));
#92850=CARTESIAN_POINT('Ctrl Pts',(5.23738379394425,0.556533631561209,5.09473202620163));
#92851=CARTESIAN_POINT('Ctrl Pts',(5.26106389523096,0.56067580248612,5.07623169604516));
#92852=CARTESIAN_POINT('Ctrl Pts',(5.30990835981114,0.569263221146577,5.03760345824506));
#92853=CARTESIAN_POINT('Ctrl Pts',(5.33433907239866,0.573581754115852,5.01803124777013));
#92854=CARTESIAN_POINT('Ctrl Pts',(5.40739238788304,0.58656589331835,4.95874709504346));
#92855=CARTESIAN_POINT('Ctrl Pts',(5.45563716547813,0.595235853632867,4.91857485205941));
#92856=CARTESIAN_POINT('Ctrl Pts',(5.59866267879059,0.62122905286391,4.79639465167396));
#92857=CARTESIAN_POINT('Ctrl Pts',(5.69188347709121,0.638561214252059,4.71261133285237));
#92858=CARTESIAN_POINT('Ctrl Pts',(5.78296299256075,0.655900535730205,4.62652156288089));
#92859=CARTESIAN_POINT('',(5.35535195535873,0.499999998694155,4.88699349605534));
#92860=CARTESIAN_POINT('Origin',(-0.728090752506269,0.0029480239586694,
1.32190450536879));
#92861=CARTESIAN_POINT('',(5.16962735214908,0.544769999440516,5.14670986015818));
#92862=CARTESIAN_POINT('Origin',(-0.712566664853689,0.376341596677865,0.769230974754304));
#92863=CARTESIAN_POINT('',(4.90707810144185,0.499999999671717,5.3369546096604));
#92864=CARTESIAN_POINT('Ctrl Pts',(4.90707810144553,0.499999999737817,5.33695460937341));
#92865=CARTESIAN_POINT('Ctrl Pts',(4.95154737164714,0.507497215012864,5.30625182412512));
#92866=CARTESIAN_POINT('Ctrl Pts',(4.99566684143965,0.514976110205956,5.27504083117598));
#92867=CARTESIAN_POINT('Ctrl Pts',(5.08346013591554,0.529942106054155,5.21141926724436));
#92868=CARTESIAN_POINT('Ctrl Pts',(5.12698304405488,0.537396700469416,5.17909339564586));
#92869=CARTESIAN_POINT('Ctrl Pts',(5.16962735231623,0.54476999976665,5.14670986045255));
#92870=CARTESIAN_POINT('',(5.13832317726269,0.55202682536752,5.18818182882492));
#92871=CARTESIAN_POINT('Ctrl Pts',(5.13832317758696,0.552026824841263,5.18818182871674));
#92872=CARTESIAN_POINT('Ctrl Pts',(5.11826013240217,0.547477949078305,5.20164982047142));
#92873=CARTESIAN_POINT('Ctrl Pts',(5.0981312204291,0.542929077204698,5.21502021216858));
#92874=CARTESIAN_POINT('Ctrl Pts',(5.07793788597092,0.53838066482091,5.22829222036761));
#92875=CARTESIAN_POINT('Ctrl Pts',(5.05774451363797,0.533832243906083,5.24156425345972));
#92876=CARTESIAN_POINT('Ctrl Pts',(5.0374843006292,0.529279732469265,5.25473388501665));
#92877=CARTESIAN_POINT('Ctrl Pts',(5.01715372172125,0.524710849052911,5.26778762574449));
#92878=CARTESIAN_POINT('Ctrl Pts',(4.98068240076011,0.516514662694109,5.29120492094222));
#92879=CARTESIAN_POINT('Ctrl Pts',(4.9439870145053,0.508277071784162,5.31426261449142));
#92880=CARTESIAN_POINT('Ctrl Pts',(4.90707810144185,0.499999999671717,5.3369546096604));
#92881=CARTESIAN_POINT('',(4.65319515451439,0.655900535591315,5.76152215973136));
#92882=CARTESIAN_POINT('Ctrl Pts',(4.65319515451439,0.655900535591315,5.76152215973136));
#92883=CARTESIAN_POINT('Ctrl Pts',(4.73896772095617,0.638769107997606,5.67022855280486));
#92884=CARTESIAN_POINT('Ctrl Pts',(4.82234152657392,0.621541657168761,5.57674041779526));
#92885=CARTESIAN_POINT('Ctrl Pts',(4.9841367074677,0.586905785274489,5.38553173775688));
#92886=CARTESIAN_POINT('Ctrl Pts',(5.06252620792821,0.569504150405887,5.28784857825658));
#92887=CARTESIAN_POINT('Ctrl Pts',(5.13832317842015,0.552026826925386,5.18818182943199));
#92888=CARTESIAN_POINT('',(3.99012283422776,0.552026825492826,6.11543257150016));
#92889=CARTESIAN_POINT('Ctrl Pts',(3.99012283383667,0.552026825050405,6.11543257052606));
#92890=CARTESIAN_POINT('Ctrl Pts',(4.01972335837119,0.556534160395578,6.10150108746967));
#92891=CARTESIAN_POINT('Ctrl Pts',(4.04682057104575,0.560675371296844,6.08852680808817));
#92892=CARTESIAN_POINT('Ctrl Pts',(4.10282982036569,0.569263221096838,6.06130042618763));
#92893=CARTESIAN_POINT('Ctrl Pts',(4.13089680313499,0.573581754058485,6.04743768417028));
#92894=CARTESIAN_POINT('Ctrl Pts',(4.21498651311904,0.586565893258238,6.00524386536356));
#92895=CARTESIAN_POINT('Ctrl Pts',(4.27073919943005,0.595235853580056,5.97638202814542));
#92896=CARTESIAN_POINT('Ctrl Pts',(4.43668598715217,0.621229052810602,5.88780459051503));
#92897=CARTESIAN_POINT('Ctrl Pts',(4.54573827185856,0.638561214197787,5.8260197952161));
#92898=CARTESIAN_POINT('Ctrl Pts',(4.65319515454537,0.655900535666704,5.76152215980325));
#92899=CARTESIAN_POINT('',(4.1795876597685,0.499999998696719,5.92398067050494));
#92900=CARTESIAN_POINT('Origin',(-0.99523750800882,0.00294860086620573,
1.1344822676465));
#92901=CARTESIAN_POINT('',(3.94237385367589,0.544769999466827,6.13769971104598));
#92902=CARTESIAN_POINT('Origin',(-0.861268422572583,0.376342028655932,0.598066782903451));
#92903=CARTESIAN_POINT('',(3.64506586129707,0.499999999748423,6.26705631602722));
#92904=CARTESIAN_POINT('Ctrl Pts',(3.6450658613806,0.499999999832972,6.26705631566973));
#92905=CARTESIAN_POINT('Ctrl Pts',(3.69509565834736,0.507497215478395,6.24663092213573));
#92906=CARTESIAN_POINT('Ctrl Pts',(3.74489308261439,0.514976111013341,6.22563400564159));
#92907=CARTESIAN_POINT('Ctrl Pts',(3.84431057014932,0.529942106213477,6.18237284342222));
#92908=CARTESIAN_POINT('Ctrl Pts',(3.89376504607911,0.537396700953456,6.16015887031076));
#92909=CARTESIAN_POINT('Ctrl Pts',(3.94237385379529,0.544769999856384,6.13769971143229));
#92910=CARTESIAN_POINT('',(3.90288630483179,0.552026825400315,6.17147261660978));
#92911=CARTESIAN_POINT('Ctrl Pts',(3.90288630490168,0.552026824702873,6.17147261644347));
#92912=CARTESIAN_POINT('Ctrl Pts',(3.88039710166864,0.547477948715548,6.18031277249131));
#92913=CARTESIAN_POINT('Ctrl Pts',(3.85786455338572,0.542929076879934,6.18904345089288));
#92914=CARTESIAN_POINT('Ctrl Pts',(3.83529023832017,0.538380664523847,6.19766419700609));
#92915=CARTESIAN_POINT('Ctrl Pts',(3.81271588091332,0.533832243636574,6.20628495928871));
#92916=CARTESIAN_POINT('Ctrl Pts',(3.79009825880634,0.529279732103297,6.21479134522615));
#92917=CARTESIAN_POINT('Ctrl Pts',(3.76743682902675,0.52471084863187,6.22316942325172));
#92918=CARTESIAN_POINT('Ctrl Pts',(3.72678416194743,0.516514662402908,6.23819897875861));
#92919=CARTESIAN_POINT('Ctrl Pts',(3.68598997183275,0.508277071642075,6.25282917252519));
#92920=CARTESIAN_POINT('Ctrl Pts',(3.64506586129707,0.499999999748423,6.26705631602722));
#92921=CARTESIAN_POINT('',(3.30584908284948,0.655900535589578,6.62712038403327));
#92922=CARTESIAN_POINT('Ctrl Pts',(3.30584908284948,0.655900535589577,6.62712038403327));
#92923=CARTESIAN_POINT('Ctrl Pts',(3.40924176110029,0.638769108003684,6.55639973733554));
#92924=CARTESIAN_POINT('Ctrl Pts',(3.51076351889193,0.621541657192441,6.4830202067497));
#92925=CARTESIAN_POINT('Ctrl Pts',(3.70988023275112,0.586905785290167,6.33106306050518));
#92926=CARTESIAN_POINT('Ctrl Pts',(3.80743602116347,0.569504150620629,6.25251510518218));
#92927=CARTESIAN_POINT('Ctrl Pts',(3.90288630586329,0.552026827148797,6.1714726174476));
#92928=CARTESIAN_POINT('',(2.58219874684554,0.552026825517167,6.83021561872381));
#92929=CARTESIAN_POINT('Ctrl Pts',(2.58219874670539,0.552026824982957,6.830215617774));
#92930=CARTESIAN_POINT('Ctrl Pts',(2.61410208447286,0.556534160325457,6.82297308283996));
#92931=CARTESIAN_POINT('Ctrl Pts',(2.64335486588199,0.560675371218705,6.81612723464921));
#92932=CARTESIAN_POINT('Ctrl Pts',(2.70390751748938,0.569263221030049,6.80157772338699));
#92933=CARTESIAN_POINT('Ctrl Pts',(2.73429838960121,0.573581753996881,6.79407265620546));
#92934=CARTESIAN_POINT('Ctrl Pts',(2.82549255285121,0.586565893214642,6.77094210737457));
#92935=CARTESIAN_POINT('Ctrl Pts',(2.88614621429549,0.595235853550835,6.75474022336757));
#92936=CARTESIAN_POINT('Ctrl Pts',(3.06725478939875,0.621229052830664,6.70390733094793));
#92937=CARTESIAN_POINT('Ctrl Pts',(3.18703939713228,0.638561214261602,6.66701004743552));
#92938=CARTESIAN_POINT('Ctrl Pts',(3.3058490828888,0.655900535789811,6.62712038423742));
#92939=CARTESIAN_POINT('',(2.80839049046689,0.499999998797894,6.68396909412142));
#92940=CARTESIAN_POINT('Origin',(-1.21585023743329,0.00294803147734828,
0.894011165756495));
#92941=CARTESIAN_POINT('',(2.53077933515541,0.544769999391056,6.8416975452563));
#92942=CARTESIAN_POINT('Origin',(-0.969699669491749,0.37634162951501,0.398936186856903));
#92943=CARTESIAN_POINT('',(2.21261439168749,0.499999999735722,6.90411743489196));
#92944=CARTESIAN_POINT('Ctrl Pts',(2.21261439184017,0.499999999817213,6.90411743457275));
#92945=CARTESIAN_POINT('Ctrl Pts',(2.26586537544578,0.507497215380639,6.89492450289489));
#92946=CARTESIAN_POINT('Ctrl Pts',(2.31901227965089,0.514976110859343,6.88512345692522));
#92947=CARTESIAN_POINT('Ctrl Pts',(2.42540202165424,0.529941643169758,6.86424618355541));
#92948=CARTESIAN_POINT('Ctrl Pts',(2.47848205947058,0.537397143804212,6.85318147571591));
#92949=CARTESIAN_POINT('Ctrl Pts',(2.53077933520185,0.544769999930024,6.84169754581379));
#92950=CARTESIAN_POINT('',(2.48495480706808,0.55202682538978,6.86619220319719));
#92951=CARTESIAN_POINT('Ctrl Pts',(2.48495480726074,0.552026824761649,6.86619220313449));
#92952=CARTESIAN_POINT('Ctrl Pts',(2.46109101724883,0.547477948836403,6.86999116731842));
#92953=CARTESIAN_POINT('Ctrl Pts',(2.43720842975439,0.54292907699423,6.87367389544388));
#92954=CARTESIAN_POINT('Ctrl Pts',(2.41330868415241,0.53838066468276,6.877240282869));
#92955=CARTESIAN_POINT('Ctrl Pts',(2.38940889372308,0.533832243840099,6.88080667698338));
#92956=CARTESIAN_POINT('Ctrl Pts',(2.36549143763035,0.529279732381481,6.88425206820953));
#92957=CARTESIAN_POINT('Ctrl Pts',(2.34155878047422,0.524710848937538,6.88756273388734));
#92958=CARTESIAN_POINT('Ctrl Pts',(2.29862563898931,0.516514662528013,6.89350178516055));
#92959=CARTESIAN_POINT('Ctrl Pts',(2.2556401341689,0.508277071523872,6.89902038819499));
#92960=CARTESIAN_POINT('Ctrl Pts',(2.21261439168749,0.499999999735722,6.90411743489196));
#92961=CARTESIAN_POINT('',(1.80392518236685,0.655900535538507,7.18284182470367));
#92962=CARTESIAN_POINT('Ctrl Pts',(1.80392518236684,0.655900535538507,7.18284182470367));
#92963=CARTESIAN_POINT('Ctrl Pts',(1.92010344582086,0.638769107941213,7.13600095696403));
#92964=CARTESIAN_POINT('Ctrl Pts',(2.03502611133774,0.621541657127866,7.08616117597769));
#92965=CARTESIAN_POINT('Ctrl Pts',(2.26215388153276,0.58690578524841,6.98056091106265));
#92966=CARTESIAN_POINT('Ctrl Pts',(2.37431435872934,0.56950415051877,6.92482097387188));
#92967=CARTESIAN_POINT('Ctrl Pts',(2.48495480789597,0.552026827062388,6.86619220426093));
#92968=CARTESIAN_POINT('',(1.05353391884569,0.552026825489145,7.22562537467431));
#92969=CARTESIAN_POINT('Ctrl Pts',(1.05353391887314,0.552026825234067,7.22562537350378));
#92970=CARTESIAN_POINT('Ctrl Pts',(1.08624446534929,0.556533631523835,7.22541046479856));
#92971=CARTESIAN_POINT('Ctrl Pts',(1.1162919525488,0.560675802443273,7.22501306695583));
#92972=CARTESIAN_POINT('Ctrl Pts',(1.17855350558121,0.569263221096503,7.22382080521556));
#92973=CARTESIAN_POINT('Ctrl Pts',(1.20984722359606,0.573581754066956,7.22302434149009));
#92974=CARTESIAN_POINT('Ctrl Pts',(1.30388170217393,0.586565893281114,7.22003862145737));
#92975=CARTESIAN_POINT('Ctrl Pts',(1.36660024076868,0.595235853609543,7.21725427280032));
#92976=CARTESIAN_POINT('Ctrl Pts',(1.55440216717859,0.621229052885991,7.20654281528298));
#92977=CARTESIAN_POINT('Ctrl Pts',(1.67931810259728,0.638561214319169,7.19625831961395));
#92978=CARTESIAN_POINT('Ctrl Pts',(1.80392518235829,0.655900535850668,7.18284182502767));
#92979=CARTESIAN_POINT('',(1.30587610362313,0.499999998542182,7.1314225503174));
#92980=CARTESIAN_POINT('Origin',(-1.37960997614413,0.00294866857638937,
0.611738390161336));
#92981=CARTESIAN_POINT('',(1.00084838688029,0.544769999485534,7.22578520659681));
#92982=CARTESIAN_POINT('Origin',(-1.03278788981951,0.376341816128584,0.181153191190526));
#92983=CARTESIAN_POINT('',(0.676703532269247,0.499999999748659,7.21834969580106));
#92984=CARTESIAN_POINT('Ctrl Pts',(0.676703532495311,0.499999999833265,
7.21834969551148));
#92985=CARTESIAN_POINT('Ctrl Pts',(0.730685746631788,0.50749721541619,7.22081907684223));
#92986=CARTESIAN_POINT('Ctrl Pts',(0.784697041277654,0.514976110958078,
7.22267218728766));
#92987=CARTESIAN_POINT('Ctrl Pts',(0.893087446816106,0.529941643242395,
7.22515366262821));
#92988=CARTESIAN_POINT('Ctrl Pts',(0.947305091113319,0.537397144273938,
7.22575828055198));
#92989=CARTESIAN_POINT('Ctrl Pts',(1.00084838683405,0.544769999820073,7.22578520694095));
#92990=CARTESIAN_POINT('',(0.950829584292169,0.552026825382187,7.23985627366907));
#92991=CARTESIAN_POINT('Ctrl Pts',(0.950829584616152,0.552026824852022,
7.23985627373207));
#92992=CARTESIAN_POINT('Ctrl Pts',(0.926707051733455,0.547477948948255,
7.23843641100287));
#92993=CARTESIAN_POINT('Ctrl Pts',(0.902591147829787,0.54292907703239,7.23689898861412));
#92994=CARTESIAN_POINT('Ctrl Pts',(0.878483496783891,0.538380664623052,
7.23524425699157));
#92995=CARTESIAN_POINT('Ctrl Pts',(0.854375800520945,0.533832243682573,
7.23358952226536));
#92996=CARTESIAN_POINT('Ctrl Pts',(0.830276863638705,0.529279732179528,
7.23181281608786));
#92997=CARTESIAN_POINT('Ctrl Pts',(0.80619204309476,0.524710848694838,7.22990126639148));
#92998=CARTESIAN_POINT('Ctrl Pts',(0.762985934765295,0.5165146624528,7.22647210971131));
#92999=CARTESIAN_POINT('Ctrl Pts',(0.719819071259968,0.508277071638636,
7.22262107810339));
#93000=CARTESIAN_POINT('Ctrl Pts',(0.676703532269247,0.499999999748659,
7.21834969580106));
#93001=CARTESIAN_POINT('',(0.21765174455862,0.655900535668849,7.40270156512545));
#93002=CARTESIAN_POINT('Ctrl Pts',(0.21765174455862,0.655900535668849,7.40270156512545));
#93003=CARTESIAN_POINT('Ctrl Pts',(0.341183226867587,0.638769108054916,
7.38193070326879));
#93004=CARTESIAN_POINT('Ctrl Pts',(0.464133144124308,0.621541657205909,
7.35796112462327));
#93005=CARTESIAN_POINT('Ctrl Pts',(0.708651728687176,0.586905785278378,
7.30365549191793));
#93006=CARTESIAN_POINT('Ctrl Pts',(0.83017239566547,0.569504150432432,7.27332991046189));
#93007=CARTESIAN_POINT('Ctrl Pts',(0.95082958488062,0.552026826960472,7.23985627496611));
#93008=CARTESIAN_POINT('',(-0.524392983759562,0.552026825661112,7.28317291910593));
#93009=CARTESIAN_POINT('Ctrl Pts',(-0.524392986242582,0.552026825224637,
7.28317291791701));
#93010=CARTESIAN_POINT('Ctrl Pts',(-0.492420046797248,0.556530947657473,
7.28999077169901));
#93011=CARTESIAN_POINT('Ctrl Pts',(-0.463017453584124,0.560669204314555,
7.29605638370086));
#93012=CARTESIAN_POINT('Ctrl Pts',(-0.40199584998173,0.56925092205502,7.30826883166599));
#93013=CARTESIAN_POINT('Ctrl Pts',(-0.371284572245158,0.57356636754223,
7.31421437802009));
#93014=CARTESIAN_POINT('Ctrl Pts',(-0.27887318750627,0.586541205299183,
7.33150238020033));
#93015=CARTESIAN_POINT('Ctrl Pts',(-0.217066995461581,0.595204946697494,
7.34225972045226));
#93016=CARTESIAN_POINT('Ctrl Pts',(-0.0313101433752705,0.621204274123675,
7.37218433405402));
#93017=CARTESIAN_POINT('Ctrl Pts',(0.092984705121821,0.638548819288446,
7.38900776886407));
#93018=CARTESIAN_POINT('Ctrl Pts',(0.217651744540169,0.655900535742686,
7.40270156519986));
#93019=CARTESIAN_POINT('',(-0.257699600093122,0.499999998735122,7.24541861505891));
#93020=CARTESIAN_POINT('Origin',(-1.47886105903604,0.00294835975049063,
0.30086193846136));
#93021=CARTESIAN_POINT('',(-0.575881118631359,0.544769999479607,7.2720031822402));
#93022=CARTESIAN_POINT('Origin',(-1.04758443315409,0.376341791154719,-0.0451004524651299));
#93023=CARTESIAN_POINT('',(-0.890849230764474,0.499999999848743,7.19505994779791));
#93024=CARTESIAN_POINT('Ctrl Pts',(-0.890849230400919,0.499999999957417,
7.19505994749708));
#93025=CARTESIAN_POINT('Ctrl Pts',(-0.838659931347879,0.507497215999936,
7.20907617723531));
#93026=CARTESIAN_POINT('Ctrl Pts',(-0.786309751644111,0.514976111985247,
7.22249679544923));
#93027=CARTESIAN_POINT('Ctrl Pts',(-0.680986902604104,0.529941643519156,
7.24822098717489));
#93028=CARTESIAN_POINT('Ctrl Pts',(-0.628166811783102,0.537397144461801,
7.26046666019013));
#93029=CARTESIAN_POINT('Ctrl Pts',(-0.57588111875408,0.544769999824209,
7.27200318257616));
#93030=CARTESIAN_POINT('',(-0.627755373541268,0.552026825840142,7.27499271185807));
#93031=CARTESIAN_POINT('Ctrl Pts',(-0.627755373720756,0.552026824602212,
7.27499271173872));
#93032=CARTESIAN_POINT('Ctrl Pts',(-0.651008707501433,0.547477948488361,
7.26842041243539));
#93033=CARTESIAN_POINT('Ctrl Pts',(-0.674230294564099,0.542929076630835,
7.26173472770646));
#93034=CARTESIAN_POINT('Ctrl Pts',(-0.697418603710524,0.538380664303708,
7.2549362505121));
#93035=CARTESIAN_POINT('Ctrl Pts',(-0.720606956350182,0.533832243445335,
7.24813776056616));
#93036=CARTESIAN_POINT('Ctrl Pts',(-0.743760534077517,0.529279731888512,
7.24122203367185));
#93037=CARTESIAN_POINT('Ctrl Pts',(-0.766871338143885,0.52471084838398,
7.23417765045406));
#93038=CARTESIAN_POINT('Ctrl Pts',(-0.808330143625273,0.516514662221979,
7.22154062957309));
#93039=CARTESIAN_POINT('Ctrl Pts',(-0.849659931167968,0.508277071487567,
7.20850003345545));
#93040=CARTESIAN_POINT('Ctrl Pts',(-0.890849230764474,0.499999999848743,
7.19505994779791));
#93041=CARTESIAN_POINT('',(-1.37879884614972,0.655900535669628,7.27641920769329));
#93042=CARTESIAN_POINT('Ctrl Pts',(-1.37879884614972,0.655900535669628,
7.27641920769329));
#93043=CARTESIAN_POINT('Ctrl Pts',(-1.25369034011231,0.638769108073372,
7.28268957415428));
#93044=CARTESIAN_POINT('Ctrl Pts',(-1.12846217290469,0.621541657257245,
7.28571098877648));
#93045=CARTESIAN_POINT('Ctrl Pts',(-0.87798619120963,0.586905785341198,
7.28523925936566));
#93046=CARTESIAN_POINT('Ctrl Pts',(-0.752787506813266,0.569504150568537,
7.28174602444789));
#93047=CARTESIAN_POINT('Ctrl Pts',(-0.627755373309366,0.552026827055009,
7.2749927130075));
#93048=CARTESIAN_POINT('',(-2.07779985949837,0.552026825471116,7.00016739177855));
#93049=CARTESIAN_POINT('Ctrl Pts',(-2.07779985901207,0.552026825063992,
7.00016739084456));
#93050=CARTESIAN_POINT('Ctrl Pts',(-2.0480188374859,0.556534160438074,7.01370873647915));
#93051=CARTESIAN_POINT('Ctrl Pts',(-2.02058797011571,0.560675371355804,
7.02596183329651));
#93052=CARTESIAN_POINT('Ctrl Pts',(-1.96357743496575,0.569263221179983,
7.05102397170068));
#93053=CARTESIAN_POINT('Ctrl Pts',(-1.93484159927572,0.573581754149126,
7.06344101193721));
#93054=CARTESIAN_POINT('Ctrl Pts',(-1.84824454669598,0.586565893347276,
7.10021529850817));
#93055=CARTESIAN_POINT('Ctrl Pts',(-1.79015362512635,0.595235853657326,
7.12402312288938));
#93056=CARTESIAN_POINT('Ctrl Pts',(-1.61521158880238,0.621229052879646,
7.19315764940022));
#93057=CARTESIAN_POINT('Ctrl Pts',(-1.49752260870047,0.638561214263646,
7.23627453375838));
#93058=CARTESIAN_POINT('Ctrl Pts',(-1.37879884618104,0.655900535737622,
7.27641920775656));
#93059=CARTESIAN_POINT('',(-1.80922555565879,0.499999998859462,7.02062695834227));
#93060=CARTESIAN_POINT('Origin',(-1.50896237484285,0.00294800655703135,
-0.0240861790254565));
#93061=CARTESIAN_POINT('',(-2.12568306326361,0.544769999386832,6.97819037132897));
#93062=CARTESIAN_POINT('Origin',(-1.01339705640315,0.376341645026371,-0.269247012856438));
#93063=CARTESIAN_POINT('',(-2.41674687579387,0.499999999814145,6.83533719297713));
#93064=CARTESIAN_POINT('Ctrl Pts',(-2.4167468754063,0.499999999914496,6.83533719277799));
#93065=CARTESIAN_POINT('Ctrl Pts',(-2.36879080914693,0.507497215798708,
6.86024488696298));
#93066=CARTESIAN_POINT('Ctrl Pts',(-2.32054958464766,0.514976111623878,
6.88460547932891));
#93067=CARTESIAN_POINT('Ctrl Pts',(-2.22321906508015,0.52994164330363,6.93236955346637));
#93068=CARTESIAN_POINT('Ctrl Pts',(-2.17426633735912,0.537397144146483,
6.95568368725052));
#93069=CARTESIAN_POINT('Ctrl Pts',(-2.12568306352827,0.544769999861654,
6.97819037174472));
#93070=CARTESIAN_POINT('',(-2.17698718727294,0.552026825671207,6.96995857575535));
#93071=CARTESIAN_POINT('Ctrl Pts',(-2.17698718740211,0.552026824726497,
6.96995857572821));
#93072=CARTESIAN_POINT('Ctrl Pts',(-2.19828402078696,0.547477948713226,
6.95854115432079));
#93073=CARTESIAN_POINT('Ctrl Pts',(-2.21952547527805,0.542929076826028,
6.94701982242141));
#93074=CARTESIAN_POINT('Ctrl Pts',(-2.24071018282034,0.538380664459791,
6.93539548884392));
#93075=CARTESIAN_POINT('Ctrl Pts',(-2.26189493009731,0.533832243562413,
6.92377113346348));
#93076=CARTESIAN_POINT('Ctrl Pts',(-2.28302051311801,0.529279732138545,
6.9120397577923));
#93077=CARTESIAN_POINT('Ctrl Pts',(-2.30407666515051,0.524710848698101,
6.9001919287274));
#93078=CARTESIAN_POINT('Ctrl Pts',(-2.34184960124397,0.516514662521826,
6.87893793657233));
#93079=CARTESIAN_POINT('Ctrl Pts',(-2.37940977898813,0.508277071730129,
6.85731753954631));
#93080=CARTESIAN_POINT('Ctrl Pts',(-2.41674687579387,0.499999999814145,
6.83533719297713));
#93081=CARTESIAN_POINT('',(-2.91077833515283,0.655900535563285,6.80989957534335));
#93082=CARTESIAN_POINT('Ctrl Pts',(-2.91077833515282,0.655900535563285,
6.80989957534335));
#93083=CARTESIAN_POINT('Ctrl Pts',(-2.78994273993378,0.638769107994248,
6.84291797474596));
#93084=CARTESIAN_POINT('Ctrl Pts',(-2.66829185254302,0.621541657190023,
6.87278910459999));
#93085=CARTESIAN_POINT('Ctrl Pts',(-2.42357045251948,0.586905785308089,
6.92617333592512));
#93086=CARTESIAN_POINT('Ctrl Pts',(-2.30054790110173,0.569504150458014,
6.94967578725998));
#93087=CARTESIAN_POINT('Ctrl Pts',(-2.17698718732734,0.552026826956038,
6.96995857719386));
#93088=CARTESIAN_POINT('',(-3.53405111803077,0.552026825436308,6.38984181842886));
#93089=CARTESIAN_POINT('Ctrl Pts',(-3.5340511174011,0.55202682514116,6.38984181765692));
#93090=CARTESIAN_POINT('Ctrl Pts',(-3.50788042103548,0.556533631427338,
6.40946630957861));
#93091=CARTESIAN_POINT('Ctrl Pts',(-3.48371932988497,0.56067580235628,6.42733390841975));
#93092=CARTESIAN_POINT('Ctrl Pts',(-3.43343181318378,0.569263221019227,
6.46406384362574));
#93093=CARTESIAN_POINT('Ctrl Pts',(-3.40803710195941,0.573581753992496,
6.48236793562192));
#93094=CARTESIAN_POINT('Ctrl Pts',(-3.33137002479532,0.586565893218342,
6.53689826642438));
#93095=CARTESIAN_POINT('Ctrl Pts',(-3.27975521506038,0.595235853551728,
6.57263730817139));
#93096=CARTESIAN_POINT('Ctrl Pts',(-3.12376510570602,0.621229052822137,
6.67776287459229));
#93097=CARTESIAN_POINT('Ctrl Pts',(-3.0180964840573,0.638561214233471,6.74517136209263));
#93098=CARTESIAN_POINT('Ctrl Pts',(-2.91077833526805,0.655900535740567,
6.8098995754869));
#93099=CARTESIAN_POINT('',(-3.2761541350426,0.499999998792703,6.46755858744837));
#93100=CARTESIAN_POINT('Origin',(-1.4685061574169,0.00294812732458634,-0.347904248396754));
#93101=CARTESIAN_POINT('',(-3.57609043012587,0.544769999287053,6.35808513454016));
#93102=CARTESIAN_POINT('Origin',(-0.931824239855779,0.376341640093868,-0.480802598575032));
#93103=CARTESIAN_POINT('',(-3.82964012287191,0.499999999696682,6.15600166741686));
#93104=CARTESIAN_POINT('Ctrl Pts',(-3.82964012256917,0.499999999768787,
6.15600166733699));
#93105=CARTESIAN_POINT('Ctrl Pts',(-3.78815966332415,0.507497215154986,
6.1906361677964));
#93106=CARTESIAN_POINT('Ctrl Pts',(-3.74628310205829,0.514976110458603,
6.22479765807499));
#93107=CARTESIAN_POINT('Ctrl Pts',(-3.66149335131078,0.529942106105535,
6.29237031424076));
#93108=CARTESIAN_POINT('Ctrl Pts',(-3.61870214653602,0.53739670052456,6.32565872540602));
#93109=CARTESIAN_POINT('Ctrl Pts',(-3.57609043053771,0.54476999984924,6.35808513495353));
#93110=CARTESIAN_POINT('',(-3.62442550006042,0.552026825406838,6.33901692355712));
#93111=CARTESIAN_POINT('Ctrl Pts',(-3.62442549984507,0.552026824821491,
6.33901692372192));
#93112=CARTESIAN_POINT('Ctrl Pts',(-3.64277001657995,0.547477948894753,
6.32328824595075));
#93113=CARTESIAN_POINT('Ctrl Pts',(-3.66103811189774,0.542929077026949,
6.30746999158048));
#93114=CARTESIAN_POINT('Ctrl Pts',(-3.67922864469353,0.538380664716611,
6.29156334259472));
#93115=CARTESIAN_POINT('Ctrl Pts',(-3.69741921160855,0.533832243875003,
6.27565666377351));
#93116=CARTESIAN_POINT('Ctrl Pts',(-3.71552899113642,0.529279732316413,
6.25965818517536));
#93117=CARTESIAN_POINT('Ctrl Pts',(-3.73354592897964,0.524710848840588,
6.2435609014759));
#93118=CARTESIAN_POINT('Ctrl Pts',(-3.76586677534318,0.516514662443097,
6.21468375055004));
#93119=CARTESIAN_POINT('Ctrl Pts',(-3.79790107138936,0.508277071533348,
6.18549449790963));
#93120=CARTESIAN_POINT('Ctrl Pts',(-3.82964012287191,0.499999999696682,
6.15600166741686));
#93121=CARTESIAN_POINT('',(-4.30665306547384,0.655900535733099,6.02495660721441));
#93122=CARTESIAN_POINT('Ctrl Pts',(-4.30665306547384,0.655900535733099,
6.02495660721441));
#93123=CARTESIAN_POINT('Ctrl Pts',(-4.19574051901911,0.638769108122376,
6.08317913596235));
#93124=CARTESIAN_POINT('Ctrl Pts',(-4.08335517155792,0.621541657284017,
6.13850324028558));
#93125=CARTESIAN_POINT('Ctrl Pts',(-3.85583125313783,0.586905785338359,
6.24324724526053));
#93126=CARTESIAN_POINT('Ctrl Pts',(-3.74073723333524,0.569504150566424,
6.29264643421973));
#93127=CARTESIAN_POINT('Ctrl Pts',(-3.62442550038272,0.552026827061318,
6.33901692498913));
#93128=CARTESIAN_POINT('',(-4.82505407630461,0.552026825514354,5.48073434215193));
#93129=CARTESIAN_POINT('Ctrl Pts',(-4.82505407547324,0.552026825038895,
5.48073434152274));
#93130=CARTESIAN_POINT('Ctrl Pts',(-4.80371141587077,0.55653416040321,5.50552886028028));
#93131=CARTESIAN_POINT('Ctrl Pts',(-4.78396077681986,0.560675371301183,
5.5281673919086));
#93132=CARTESIAN_POINT('Ctrl Pts',(-4.74274273530616,0.569263221112224,
5.5748512749948));
#93133=CARTESIAN_POINT('Ctrl Pts',(-4.72187657706136,0.573581754077447,
5.59818653970657));
#93134=CARTESIAN_POINT('Ctrl Pts',(-4.65872434286268,0.586565893279194,
5.66792313689829));
#93135=CARTESIAN_POINT('Ctrl Pts',(-4.61599909629449,0.595235853596475,
5.71392227800979));
#93136=CARTESIAN_POINT('Ctrl Pts',(-4.48625483849351,0.621229052817995,
5.85012332937484));
#93137=CARTESIAN_POINT('Ctrl Pts',(-4.39754752286322,0.638561214196987,
5.93867147387761));
#93138=CARTESIAN_POINT('Ctrl Pts',(-4.30665306542352,0.655900535670885,
6.02495660717391));
#93139=CARTESIAN_POINT('',(-4.58989338932486,0.499999998946337,5.61207436485739));
#93140=CARTESIAN_POINT('Origin',(-1.35938332557116,0.00294833923909749,
-0.655457300451683));
#93141=CARTESIAN_POINT('',(-4.85928378406155,0.544769999439475,5.44068290297079));
#93142=CARTESIAN_POINT('Origin',(-0.806680331093372,0.376341480826078,-0.669876452008213));
#93143=CARTESIAN_POINT('',(-5.06346365273142,0.499999999752261,5.18881834708339));
#93144=CARTESIAN_POINT('Ctrl Pts',(-5.06346365249666,0.499999999806884,
5.18881834689219));
#93145=CARTESIAN_POINT('Ctrl Pts',(-5.03039833335715,0.507497225171508,
5.2315602412285));
#93146=CARTESIAN_POINT('Ctrl Pts',(-4.99684448589563,0.514976130594258,
5.27392533114672));
#93147=CARTESIAN_POINT('Ctrl Pts',(-4.92856544338408,0.529941633734565,
5.35814269436226));
#93148=CARTESIAN_POINT('Ctrl Pts',(-4.89392655660566,0.537397123185718,
5.39985668623828));
#93149=CARTESIAN_POINT('Ctrl Pts',(-4.85928378438838,0.544769999813635,
5.44068290318055));
#93150=CARTESIAN_POINT('',(-4.90238970435406,0.552026825426173,5.41166988547225));
#93151=CARTESIAN_POINT('Ctrl Pts',(-4.90238970419515,0.552026824885702,
5.41166988580858));
#93152=CARTESIAN_POINT('Ctrl Pts',(-4.91692413516503,0.547477949104674,
5.39236540742167));
#93153=CARTESIAN_POINT('Ctrl Pts',(-4.93136467531652,0.542929077274359,
5.37298987474318));
#93154=CARTESIAN_POINT('Ctrl Pts',(-4.94571046402211,0.538380664934047,
5.35354468768559));
#93155=CARTESIAN_POINT('Ctrl Pts',(-4.96005627963508,0.533832244062601,
5.33409946415606));
#93156=CARTESIAN_POINT('Ctrl Pts',(-4.97430346254159,0.529279732633635,
5.31458195405456));
#93157=CARTESIAN_POINT('Ctrl Pts',(-4.98843873411042,0.524710849218788,
5.29498790704647));
#93158=CARTESIAN_POINT('Ctrl Pts',(-5.01379620343765,0.516514662786328,
5.25983786103679));
#93159=CARTESIAN_POINT('Ctrl Pts',(-5.03880672912297,0.508277071774748,
5.22444460988968));
#93160=CARTESIAN_POINT('Ctrl Pts',(-5.06346365273142,0.499999999752261,
5.18881834708339));
#93161=CARTESIAN_POINT('',(-5.50115348400725,0.655900535618631,4.95829336454301));
#93162=CARTESIAN_POINT('Ctrl Pts',(-5.50115348400725,0.655900535618631,
4.95829336454301));
#93163=CARTESIAN_POINT('Ctrl Pts',(-5.40535013388253,0.638769108037422,
5.03899760190824));
#93164=CARTESIAN_POINT('Ctrl Pts',(-5.30748534043842,0.621541657225329,
5.11718778708195));
#93165=CARTESIAN_POINT('Ctrl Pts',(-5.10779766963579,0.586905785321977,
5.26839385239524));
#93166=CARTESIAN_POINT('Ctrl Pts',(-5.00601384944893,0.569504150565706,
5.34137992789109));
#93167=CARTESIAN_POINT('Ctrl Pts',(-4.90238970497714,0.552026827062365,
5.41166988679766));
#93168=CARTESIAN_POINT('',(-5.89044286688532,0.552026825461704,4.31535382151131));
#93169=CARTESIAN_POINT('Ctrl Pts',(-5.89044286585037,0.552026825217669,
4.31535382099207));
#93170=CARTESIAN_POINT('Ctrl Pts',(-5.87493109527073,0.556533631547463,
4.34415331790915));
#93171=CARTESIAN_POINT('Ctrl Pts',(-5.86050549286374,0.560675802479242,
4.37051449026906));
#93172=CARTESIAN_POINT('Ctrl Pts',(-5.83028827827681,0.56926322115515,4.4249648568579));
#93173=CARTESIAN_POINT('Ctrl Pts',(-5.81492635134257,0.573581754127954,
4.45224016328351));
#93174=CARTESIAN_POINT('Ctrl Pts',(-5.76824188832753,0.586565893336634,
4.53392222111768));
#93175=CARTESIAN_POINT('Ctrl Pts',(-5.73640398994225,0.59523585365148,4.5880305928689));
#93176=CARTESIAN_POINT('Ctrl Pts',(-5.63897228081956,0.621229052877164,
4.7489385194819));
#93177=CARTESIAN_POINT('Ctrl Pts',(-5.5713741265464,0.638561214252923,4.85448590824627));
#93178=CARTESIAN_POINT('Ctrl Pts',(-5.50115348409217,0.655900535709962,
4.9582933645852));
#93179=CARTESIAN_POINT('',(-5.68901432855912,0.499999998629038,4.49417578248358));
#93180=CARTESIAN_POINT('Origin',(-1.18669842542073,0.00294833247686969,
-0.932359553028809));
#93181=CARTESIAN_POINT('',(-5.91526242791687,0.544769999463201,4.26888038646475));
#93182=CARTESIAN_POINT('Origin',(-0.643817013602778,0.376341765642476,-0.827627435534536));
#93183=CARTESIAN_POINT('',(-6.06052525045423,0.499999999933984,3.97901164806514));
#93184=CARTESIAN_POINT('Ctrl Pts',(-6.06052525004562,0.500000000016535,
3.97901164785921));
#93185=CARTESIAN_POINT('Ctrl Pts',(-6.03742122062618,0.507497226262149,
4.02786233269189));
#93186=CARTESIAN_POINT('Ctrl Pts',(-6.0137590823351,0.514976132581203,4.07645004161787));
#93187=CARTESIAN_POINT('Ctrl Pts',(-5.96518059621994,0.529941639804371,
4.17337645202689));
#93188=CARTESIAN_POINT('Ctrl Pts',(-5.9403188393161,0.53739712403384,4.22156149693423));
#93189=CARTESIAN_POINT('Ctrl Pts',(-5.91526242830641,0.544769999863304,
4.26888038660868));
#93190=CARTESIAN_POINT('',(-5.95112361506895,0.552026825675856,4.23127917814192));
#93191=CARTESIAN_POINT('Ctrl Pts',(-5.95112361521097,0.552026824647466,
4.23127917807872));
#93192=CARTESIAN_POINT('Ctrl Pts',(-5.96116834730158,0.547477948689876,
4.2093015533715));
#93193=CARTESIAN_POINT('Ctrl Pts',(-5.97110610902993,0.54292907688231,4.18727472039419));
#93194=CARTESIAN_POINT('Ctrl Pts',(-5.98093636090419,0.538380664555678,
4.16520023027504));
#93195=CARTESIAN_POINT('Ctrl Pts',(-5.99076663121642,0.533832243697881,
4.14312569875219));
#93196=CARTESIAN_POINT('Ctrl Pts',(-6.0004850352215,0.529279732186206,4.12100177376764));
#93197=CARTESIAN_POINT('Ctrl Pts',(-6.01007769116381,0.524710848712617,
4.09882715890195));
#93198=CARTESIAN_POINT('Ctrl Pts',(-6.02728609557759,0.516514662483712,
4.05904779616615));
#93199=CARTESIAN_POINT('Ctrl Pts',(-6.04410338579749,0.508277071670928,
4.01910549692898));
#93200=CARTESIAN_POINT('Ctrl Pts',(-6.06052525045423,0.499999999933984,
3.97901164806514));
#93201=CARTESIAN_POINT('',(-6.43842607969659,0.655900535543649,3.65978583507949));
#93202=CARTESIAN_POINT('Ctrl Pts',(-6.43842607969659,0.655900535543648,
3.65978583507949));
#93203=CARTESIAN_POINT('Ctrl Pts',(-6.36221158414701,0.63876910796355,3.75919814047178));
#93204=CARTESIAN_POINT('Ctrl Pts',(-6.28344339378497,0.621541657163328,
3.85659832020235));
#93205=CARTESIAN_POINT('Ctrl Pts',(-6.12092914436792,0.586905785291491,
4.04719621800423));
#93206=CARTESIAN_POINT('Ctrl Pts',(-6.03721482183592,0.569504150472652,
4.14035643254888));
#93207=CARTESIAN_POINT('Ctrl Pts',(-5.95112361580156,0.552026826978804,
4.23127917908606));
#93208=CARTESIAN_POINT('',(-6.68040109666531,0.552026825412667,2.94819215069797));
#93209=CARTESIAN_POINT('Ctrl Pts',(-6.68040109566058,0.552026825128316,
2.94819215045262));
#93210=CARTESIAN_POINT('Ctrl Pts',(-6.67144302222964,0.556533631437695,
2.97965290314322));
#93211=CARTESIAN_POINT('Ctrl Pts',(-6.66302155520908,0.560675802374939,
3.00849884408019));
#93212=CARTESIAN_POINT('Ctrl Pts',(-6.64521602158031,0.569263221053295,
3.06817199929897));
#93213=CARTESIAN_POINT('Ctrl Pts',(-6.63607663258483,0.573581754029128,
3.09811198443641));
#93214=CARTESIAN_POINT('Ctrl Pts',(-6.60804285427525,0.58656589325219,3.18792014081814));
#93215=CARTESIAN_POINT('Ctrl Pts',(-6.58858100873347,0.595235853578946,
3.24760769601679));
#93216=CARTESIAN_POINT('Ctrl Pts',(-6.52801764659181,0.621229052843535,
3.42569862232371));
#93217=CARTESIAN_POINT('Ctrl Pts',(-6.48468946820172,0.638561214255091,
3.54330997689522));
#93218=CARTESIAN_POINT('Ctrl Pts',(-6.43842607993088,0.655900535776209,
3.65978583513793));
#93219=CARTESIAN_POINT('',(-6.52212328092484,0.499999998610809,3.16613453548233));
#93220=CARTESIAN_POINT('Origin',(-0.958526833969954,0.00294802284599618,
-1.16566486688198));
#93221=CARTESIAN_POINT('',(-6.69464997525716,0.544769999368522,2.89746976731015));
#93222=CARTESIAN_POINT('Origin',(-0.450850612214941,0.3763418800084,-0.946678874814712));
#93223=CARTESIAN_POINT('',(-6.77420342353812,0.499999999786671,2.58315078520083));
#93224=CARTESIAN_POINT('Ctrl Pts',(-6.77420342316194,0.499999999880416,
2.58315078535635));
#93225=CARTESIAN_POINT('Ctrl Pts',(-6.76214102323053,0.507497215697533,
2.63582597812924));
#93226=CARTESIAN_POINT('Ctrl Pts',(-6.74947703553349,0.514976111417823,
2.68836432144651));
#93227=CARTESIAN_POINT('Ctrl Pts',(-6.72286973356319,0.529942106249854,
2.79347100949626));
#93228=CARTESIAN_POINT('Ctrl Pts',(-6.70894923891358,0.53739670136936,2.84586782142646));
#93229=CARTESIAN_POINT('Ctrl Pts',(-6.69464997581791,0.54476999991391,2.89746976738761));
#93230=CARTESIAN_POINT('',(-6.72158959959758,0.552026825343707,2.85303855926069));
#93231=CARTESIAN_POINT('Ctrl Pts',(-6.72158959957876,0.552026824717549,
2.85303855943171));
#93232=CARTESIAN_POINT('Ctrl Pts',(-6.72667495173065,0.547477948832495,
2.82941543926053));
#93233=CARTESIAN_POINT('Ctrl Pts',(-6.73164525610249,0.542929077003787,
2.80576725640421));
#93234=CARTESIAN_POINT('Ctrl Pts',(-6.73650031926673,0.538380664658224,
2.78209564204453));
#93235=CARTESIAN_POINT('Ctrl Pts',(-6.74135539153724,0.533832243781545,
2.75842398328578));
#93236=CARTESIAN_POINT('Ctrl Pts',(-6.74609059481198,0.529279732319472,
2.73472813380816));
#93237=CARTESIAN_POINT('Ctrl Pts',(-6.7506920930816,0.524710848861558,2.71100981166606));
#93238=CARTESIAN_POINT('Ctrl Pts',(-6.75894678762545,0.516514662501874,
2.66846116926658));
#93239=CARTESIAN_POINT('Ctrl Pts',(-6.76678448543499,0.508277071532466,
2.62583747771786));
#93240=CARTESIAN_POINT('Ctrl Pts',(-6.77420342353812,0.499999999786671,
2.58315078520083));
#93241=CARTESIAN_POINT('',(-7.07464502826342,0.655900535710891,2.19015078679768));
#93242=CARTESIAN_POINT('Ctrl Pts',(-7.07464502826342,0.655900535710891,
2.19015078679768));
#93243=CARTESIAN_POINT('Ctrl Pts',(-7.02158309222455,0.638769108081322,
2.30362275157115));
#93244=CARTESIAN_POINT('Ctrl Pts',(-6.96559461778364,0.621541657221281,
2.41567860194491));
#93245=CARTESIAN_POINT('Ctrl Pts',(-6.84785277504007,0.586905785274964,
2.63675618678576));
#93246=CARTESIAN_POINT('Ctrl Pts',(-6.78612233907849,0.569504150426287,
2.7457344722221));
#93247=CARTESIAN_POINT('Ctrl Pts',(-6.7215896004347,0.5520268269623,2.85303856002776));
#93248=CARTESIAN_POINT('',(-7.15799119607484,0.552026825446138,1.44317629208911));
#93249=CARTESIAN_POINT('Ctrl Pts',(-7.15799119488379,0.55202682520204,1.44317629205038));
#93250=CARTESIAN_POINT('Ctrl Pts',(-7.15600568807706,0.556533631500037,
1.47582723080508));
#93251=CARTESIAN_POINT('Ctrl Pts',(-7.15398213489251,0.560675802423479,
1.5058091360986));
#93252=CARTESIAN_POINT('Ctrl Pts',(-7.14942084918708,0.569263221076987,
1.56791482941623));
#93253=CARTESIAN_POINT('Ctrl Pts',(-7.14693134581205,0.573581754042761,
1.59911953277205));
#93254=CARTESIAN_POINT('Ctrl Pts',(-7.13885908057076,0.586565893249146,
1.6928544579728));
#93255=CARTESIAN_POINT('Ctrl Pts',(-7.13268330218066,0.595235853572959,
1.75533027279036));
#93256=CARTESIAN_POINT('Ctrl Pts',(-7.11182016263718,0.621229052815269,
1.94227686467748));
#93257=CARTESIAN_POINT('Ctrl Pts',(-7.09478793767363,0.638561214209733,
2.06645280858534));
#93258=CARTESIAN_POINT('Ctrl Pts',(-7.07464502823531,0.655900535683804,
2.19015078679689));
#93259=CARTESIAN_POINT('',(-7.05026499842311,0.499999998724005,1.69004835618955));
#93260=CARTESIAN_POINT('Origin',(-0.685531569485398,0.00294801892202427,
-1.34446804942707));
#93261=CARTESIAN_POINT('',(-7.16100313078815,0.544769999536036,1.39057668144311));
#93262=CARTESIAN_POINT('Origin',(-0.236801120050296,0.376341888117048,-1.02146591795983));
#93263=CARTESIAN_POINT('',(-7.17112737311027,0.499999999517536,1.0665046612835));
#93264=CARTESIAN_POINT('Ctrl Pts',(-7.17112737305704,0.499999999527143,
1.06650466128172));
#93265=CARTESIAN_POINT('Ctrl Pts',(-7.17067059482892,0.507497213567971,
1.12054138398888));
#93266=CARTESIAN_POINT('Ctrl Pts',(-7.16959687566357,0.514976107571692,
1.17457378031923));
#93267=CARTESIAN_POINT('Ctrl Pts',(-7.16620657274698,0.529941643310162,
1.28293959095106));
#93268=CARTESIAN_POINT('Ctrl Pts',(-7.16387501996956,0.53739714398625,1.33711045128718));
#93269=CARTESIAN_POINT('Ctrl Pts',(-7.16100313111276,0.544769999849767,
1.39057668141728));
#93270=CARTESIAN_POINT('',(-7.17776152484637,0.55202682540428,1.34139302791087));
#93271=CARTESIAN_POINT('Ctrl Pts',(-7.17776152490766,0.552026824855066,
1.34139302824004));
#93272=CARTESIAN_POINT('Ctrl Pts',(-7.17764971205927,0.547477949014844,
1.31722900355443));
#93273=CARTESIAN_POINT('Ctrl Pts',(-7.17742015316916,0.542929077144782,
1.29306523348913));
#93274=CARTESIAN_POINT('Ctrl Pts',(-7.17707301030228,0.53838066479279,1.26890335318175));
#93275=CARTESIAN_POINT('Ctrl Pts',(-7.1767258667843,0.53383224390963,1.24474142755546));
#93276=CARTESIAN_POINT('Ctrl Pts',(-7.17625645642031,0.529279732411963,
1.22058164507269));
#93277=CARTESIAN_POINT('Ctrl Pts',(-7.17565163607013,0.524710848946523,
1.19642865794178));
#93278=CARTESIAN_POINT('Ctrl Pts',(-7.17456664006963,0.516514662615714,
1.15310026393304));
#93279=CARTESIAN_POINT('Ctrl Pts',(-7.1730582631878,0.508277071721035,1.10978821734395));
#93280=CARTESIAN_POINT('Ctrl Pts',(-7.17112737311027,0.499999999517536,
1.0665046612835));
#93281=CARTESIAN_POINT('',(-7.38006143764124,0.655900535683362,0.618106723046989));
#93282=CARTESIAN_POINT('Ctrl Pts',(-7.38006143764124,0.655900535683362,
0.618106723046988));
#93283=CARTESIAN_POINT('Ctrl Pts',(-7.3526331783707,0.63876910802647,0.740332523974201));
#93284=CARTESIAN_POINT('Ctrl Pts',(-7.32204237884272,0.621541657175023,
0.861804437744292));
#93285=CARTESIAN_POINT('Ctrl Pts',(-7.25457842071691,0.586905785258295,
1.10302436718471));
#93286=CARTESIAN_POINT('Ctrl Pts',(-7.21771831817857,0.569504150488276,
1.22272501946576));
#93287=CARTESIAN_POINT('Ctrl Pts',(-7.17776152609422,0.552026827023669,
1.34139302856953));
#93288=CARTESIAN_POINT('',(-7.30088158247247,0.552026825456915,-0.129320885806511));
#93289=CARTESIAN_POINT('Ctrl Pts',(-7.3008815813318,0.552026825209583,-0.1293208855927));
#93290=CARTESIAN_POINT('Ctrl Pts',(-7.30596148125041,0.556533631510786,
-0.0970064823605118));
#93291=CARTESIAN_POINT('Ctrl Pts',(-7.31043046100619,0.560675802446503,
-0.0672905331523253));
#93292=CARTESIAN_POINT('Ctrl Pts',(-7.31932670386724,0.569263221112411,
-0.00565629475601271));
#93293=CARTESIAN_POINT('Ctrl Pts',(-7.32360349251664,0.573581754082038,
0.0253540296392704));
#93294=CARTESIAN_POINT('Ctrl Pts',(-7.33587019047837,0.586565893288676,
0.118632782797426));
#93295=CARTESIAN_POINT('Ctrl Pts',(-7.34326925176093,0.595235853607951,
0.180975557563082));
#93296=CARTESIAN_POINT('Ctrl Pts',(-7.36308187196685,0.621229052849239,
0.368036400349092));
#93297=CARTESIAN_POINT('Ctrl Pts',(-7.37314200827478,0.638561214247294,
0.492970604652602));
#93298=CARTESIAN_POINT('Ctrl Pts',(-7.38006143769083,0.655900535731995,
0.618106723037508));
#93299=CARTESIAN_POINT('',(-7.24874416021239,0.499999998894538,0.134937395088208));
#93300=CARTESIAN_POINT('Origin',(-0.380481977827258,0.00294817441139524,
-1.46040437774116));
#93301=CARTESIAN_POINT('',(-7.2925157382699,0.544769999418317,-0.181338224043539));
#93302=CARTESIAN_POINT('Origin',(-0.0116792896362683,0.376341641496503,
-1.04848995475632));
#93303=CARTESIAN_POINT('',(-7.23273737687419,0.49999999957512,-0.500010032745376));
#93304=CARTESIAN_POINT('Ctrl Pts',(-7.23273737677256,0.499999999597735,
-0.50001003270372));
#93305=CARTESIAN_POINT('Ctrl Pts',(-7.24390757625351,0.507497213911131,
-0.447138462547856));
#93306=CARTESIAN_POINT('Ctrl Pts',(-7.25447432840697,0.514976108202603,
-0.394138493533089));
#93307=CARTESIAN_POINT('Ctrl Pts',(-7.27445873396409,0.529941643242863,
-0.287577405483172));
#93308=CARTESIAN_POINT('Ctrl Pts',(-7.28382682503527,0.537397143705099,
-0.234171816569637));
#93309=CARTESIAN_POINT('Ctrl Pts',(-7.29251573872258,0.544769999874284,
-0.181338224181616));
#93310=CARTESIAN_POINT('',(-7.29830929881042,0.552026825658063,-0.232974550490544));
#93311=CARTESIAN_POINT('Ctrl Pts',(-7.2983092988398,0.552026824668521,-0.232974550626286));
#93312=CARTESIAN_POINT('Ctrl Pts',(-7.29300554884515,0.547477948674746,
-0.256549598283125));
#93313=CARTESIAN_POINT('Ctrl Pts',(-7.2875868606527,0.542929076835482,-0.280099084445121));
#93314=CARTESIAN_POINT('Ctrl Pts',(-7.28205374376109,0.538380664501388,
-0.303621447946045));
#93315=CARTESIAN_POINT('Ctrl Pts',(-7.27652061649133,0.533832243636109,
-0.327143855566465));
#93316=CARTESIAN_POINT('Ctrl Pts',(-7.27086854156995,0.52927973210616,-0.350637886369769));
#93317=CARTESIAN_POINT('Ctrl Pts',(-7.26508568330685,0.524710848643296,
-0.37409617156336));
#93318=CARTESIAN_POINT('Ctrl Pts',(-7.25471173014415,0.516514662450736,
-0.416178329002402));
#93319=CARTESIAN_POINT('Ctrl Pts',(-7.24392780876621,0.508277071726877,
-0.458153506858803));
#93320=CARTESIAN_POINT('Ctrl Pts',(-7.23273737687419,0.49999999957512,-0.500010032745376));
#93321=CARTESIAN_POINT('',(-7.34039437668371,0.655900535573722,-0.98283932438691));
#93322=CARTESIAN_POINT('Ctrl Pts',(-7.34039437668371,0.655900535573721,
-0.98283932438691));
#93323=CARTESIAN_POINT('Ctrl Pts',(-7.3398823091396,0.638769107974336,-0.857574829919374));
#93324=CARTESIAN_POINT('Ctrl Pts',(-7.3361195763012,0.621541657159446,-0.732366744488661));
#93325=CARTESIAN_POINT('Ctrl Pts',(-7.32208804245887,0.586905785274177,
-0.482283646433133));
#93326=CARTESIAN_POINT('Ctrl Pts',(-7.31182181051129,0.569504150452724,
-0.35745769620365));
#93327=CARTESIAN_POINT('Ctrl Pts',(-7.29830930016154,0.552026826973882,
-0.232974550159142));
#93328=CARTESIAN_POINT('',(-7.10239085947497,0.552026825477796,-1.69577116499436));
#93329=CARTESIAN_POINT('Ctrl Pts',(-7.10239085868817,0.552026824950452,
-1.69577116460884));
#93330=CARTESIAN_POINT('Ctrl Pts',(-7.11430003273687,0.556534160312844,
-1.66530070594601));
#93331=CARTESIAN_POINT('Ctrl Pts',(-7.12505008206614,0.560675371213913,
-1.63724669915386));
#93332=CARTESIAN_POINT('Ctrl Pts',(-7.14698897655328,0.569263221046235,
-1.57896293803046));
#93333=CARTESIAN_POINT('Ctrl Pts',(-7.15783207936236,0.573581754020886,
-1.54959700089359));
#93334=CARTESIAN_POINT('Ctrl Pts',(-7.1898641634356,0.586565893249612,-1.46113603045405));
#93335=CARTESIAN_POINT('Ctrl Pts',(-7.21049209255752,0.595235853584485,
-1.4018413744536));
#93336=CARTESIAN_POINT('Ctrl Pts',(-7.27005405652529,0.621229052855129,
-1.22341303761221));
#93337=CARTESIAN_POINT('Ctrl Pts',(-7.30673615337281,0.638561214263141,
-1.10356235732804));
#93338=CARTESIAN_POINT('Ctrl Pts',(-7.3403943768537,0.655900535751893,-0.982839324459895));
#93339=CARTESIAN_POINT('',(-7.10828010110168,0.499999998819424,-1.4264830890482));
#93340=CARTESIAN_POINT('Origin',(-0.0576434912618817,0.00294819472885649,
-1.50805332165096));
#93341=CARTESIAN_POINT('',(-7.08303841516615,0.544769999432261,-1.74477395495737));
#93342=CARTESIAN_POINT('Origin',(0.213987977808648,0.376341652662118,-1.02648755829279));
#93343=CARTESIAN_POINT('',(-6.95615261946262,0.499999999579506,-2.04314481407824));
#93344=CARTESIAN_POINT('Ctrl Pts',(-6.9561526193664,0.499999999623434,-2.04314481391355));
#93345=CARTESIAN_POINT('Ctrl Pts',(-6.97842749214027,0.507497214509123,
-1.99391061084159));
#93346=CARTESIAN_POINT('Ctrl Pts',(-7.00014062758234,0.514976109292713,
-1.94442128735484));
#93347=CARTESIAN_POINT('Ctrl Pts',(-7.04256660156483,0.529942105956751,
-1.8446445168329));
#93348=CARTESIAN_POINT('Ctrl Pts',(-7.06319378908159,0.537396700077726,
-1.79450746095607));
#93349=CARTESIAN_POINT('Ctrl Pts',(-7.08303841565686,0.544769999974806,
-1.74477395523361));
#93350=CARTESIAN_POINT('',(-7.07759624149658,0.55202682539532,-1.79644849796954));
#93351=CARTESIAN_POINT('Ctrl Pts',(-7.07759624155095,0.552026824779479,
-1.79644849775501));
#93352=CARTESIAN_POINT('Ctrl Pts',(-7.06734855208673,0.547477948772125,
-1.81833222393605));
#93353=CARTESIAN_POINT('Ctrl Pts',(-7.05699410635578,0.542929076886224,
-1.84016627842884));
#93354=CARTESIAN_POINT('Ctrl Pts',(-7.04653373779578,0.53838066452945,-1.8619492456006));
#93355=CARTESIAN_POINT('Ctrl Pts',(-7.03607334961583,0.533832243641466,
-1.88373225362949));
#93356=CARTESIAN_POINT('Ctrl Pts',(-7.02550289495077,0.529279732158083,
-1.90546197808978));
#93357=CARTESIAN_POINT('Ctrl Pts',(-7.01481239879411,0.524710848694791,
-1.92712867807061));
#93358=CARTESIAN_POINT('Ctrl Pts',(-6.99563456268909,0.516514662385204,
-1.96599688540912));
#93359=CARTESIAN_POINT('Ctrl Pts',(-6.97607934059764,0.508277071500689,
-2.00467248320679));
#93360=CARTESIAN_POINT('Ctrl Pts',(-6.95615261946262,0.499999999579506,
-2.04314481407824));
#93361=CARTESIAN_POINT('',(-6.95749863316843,0.655900535537742,-2.53782889725405));
#93362=CARTESIAN_POINT('Ctrl Pts',(-6.95749863316843,0.655900535537741,
-2.53782889725405));
#93363=CARTESIAN_POINT('Ctrl Pts',(-6.98392670096081,0.638769107926578,
-2.4153829377179));
#93364=CARTESIAN_POINT('Ctrl Pts',(-7.00716797595779,0.621541657119776,
-2.29229327145058));
#93365=CARTESIAN_POINT('Ctrl Pts',(-7.0472249652761,0.586905785256709,-2.04504061223377));
#93366=CARTESIAN_POINT('Ctrl Pts',(-7.06403264154237,0.56950415053602,-1.92092608751711));
#93367=CARTESIAN_POINT('Ctrl Pts',(-7.07759624290549,0.55202682706362,-1.79644849788882));
#93368=CARTESIAN_POINT('',(-6.57180023450511,0.552026825547467,-3.18292906702191));
#93369=CARTESIAN_POINT('Ctrl Pts',(-6.57180023370417,0.552026825029646,
-3.18292906640069));
#93370=CARTESIAN_POINT('Ctrl Pts',(-6.58998122584121,0.556534160399563,
-3.1557311104335));
#93371=CARTESIAN_POINT('Ctrl Pts',(-6.60651072723157,0.560675371309851,
-3.13064393347764));
#93372=CARTESIAN_POINT('Ctrl Pts',(-6.64046598836063,0.569263221140471,
-3.07843902805526));
#93373=CARTESIAN_POINT('Ctrl Pts',(-6.65736839388578,0.573581754112593,
-3.05209059678148));
#93374=CARTESIAN_POINT('Ctrl Pts',(-6.70766807935086,0.586565893323852,
-2.97258374591643));
#93375=CARTESIAN_POINT('Ctrl Pts',(-6.74056033721591,0.595235853644447,
-2.91910976107274));
#93376=CARTESIAN_POINT('Ctrl Pts',(-6.83708659364138,0.62122905289433,-2.75765704122748));
#93377=CARTESIAN_POINT('Ctrl Pts',(-6.89868023266326,0.638562584594348,
-2.64848530079444));
#93378=CARTESIAN_POINT('Ctrl Pts',(-6.95750328265113,0.655901906252846,
-2.53782015062894));
#93379=CARTESIAN_POINT('',(-6.6354407643065,0.499999998577759,-2.92120280882441));
#93380=CARTESIAN_POINT('Origin',(0.267888816907871,0.002948723900741,-1.48518799392768));
#93381=CARTESIAN_POINT('',(-6.54236608768061,0.544769999554987,-3.2266259964821));
#93382=CARTESIAN_POINT('Origin',(0.429648088530983,0.376341930995795,-0.956488181367567));
#93383=CARTESIAN_POINT('',(-6.35430589758883,0.499999999782203,-3.49074441377444));
#93384=CARTESIAN_POINT('Ctrl Pts',(-6.35430589746526,0.499999999874871,
-3.4907444133915));
#93385=CARTESIAN_POINT('Ctrl Pts',(-6.38664389820455,0.507497215608088,
-3.44744971264936));
#93386=CARTESIAN_POINT('Ctrl Pts',(-6.41848813786028,0.514976111277326,
-3.40378509899666));
#93387=CARTESIAN_POINT('Ctrl Pts',(-6.48136931942955,0.529941643107535,
-3.31546412729002));
#93388=CARTESIAN_POINT('Ctrl Pts',(-6.51229599592233,0.537397144213602,
-3.27092808317226));
#93389=CARTESIAN_POINT('Ctrl Pts',(-6.54236608792216,0.544769999867112,
-3.226625996698));
#93390=CARTESIAN_POINT('',(-6.52594265037054,0.552026825343033,-3.27592250968595));
#93391=CARTESIAN_POINT('Ctrl Pts',(-6.52594265060015,0.552026824772377,
-3.27592250954095));
#93392=CARTESIAN_POINT('Ctrl Pts',(-6.51123019227503,0.547477948958686,
-3.29509165566118));
#93393=CARTESIAN_POINT('Ctrl Pts',(-6.49642415158775,0.542929077147482,
-3.31418934218825));
#93394=CARTESIAN_POINT('Ctrl Pts',(-6.48152564671875,0.538380664815547,
-3.33321436547128));
#93395=CARTESIAN_POINT('Ctrl Pts',(-6.46662711390579,0.533832243952507,
-3.35223942443808));
#93396=CARTESIAN_POINT('Ctrl Pts',(-6.45163254231022,0.529279732515485,
-3.37118878455419));
#93397=CARTESIAN_POINT('Ctrl Pts',(-6.43653428412055,0.524710849087795,
-3.39005078828863));
#93398=CARTESIAN_POINT('Ctrl Pts',(-6.4094492992381,0.516514662679131,-3.42388761102558));
#93399=CARTESIAN_POINT('Ctrl Pts',(-6.38203715678421,0.508277071679413,
-3.45745520047593));
#93400=CARTESIAN_POINT('Ctrl Pts',(-6.35430589758883,0.499999999782203,
-3.49074441377444));
#93401=CARTESIAN_POINT('',(-6.24927798598832,0.655900535655765,-3.97415241251114));
#93402=CARTESIAN_POINT('Ctrl Pts',(-6.24927798598832,0.655900535655764,
-3.97415241251114));
#93403=CARTESIAN_POINT('Ctrl Pts',(-6.30141044213484,0.638769107998681,
-3.86025042465859));
#93404=CARTESIAN_POINT('Ctrl Pts',(-6.35056898884682,0.621541657147841,
-3.74503471332135));
#93405=CARTESIAN_POINT('Ctrl Pts',(-6.44284148098601,0.586905785248514,
-3.51217375248129));
#93406=CARTESIAN_POINT('Ctrl Pts',(-6.48593715743418,0.569504150382786,
-3.39457410907575));
#93407=CARTESIAN_POINT('Ctrl Pts',(-6.52594265148857,0.552026826911856,
-3.27592250983182));
#93408=CARTESIAN_POINT('',(-5.73391953562396,0.55202682544913,-4.52125674256205));
#93409=CARTESIAN_POINT('Ctrl Pts',(-5.73391953482653,0.552026825209883,
-4.52125674168361));
#93410=CARTESIAN_POINT('Ctrl Pts',(-5.75751945158617,0.556533631513851,
-4.49860569374452));
#93411=CARTESIAN_POINT('Ctrl Pts',(-5.77906050160631,0.560675802441731,
-4.47765354396293));
#93412=CARTESIAN_POINT('Ctrl Pts',(-5.82344219070902,0.569263221097661,
-4.43397073094407));
#93413=CARTESIAN_POINT('Ctrl Pts',(-5.84561356122113,0.573581754061752,
-4.41187182893966));
#93414=CARTESIAN_POINT('Ctrl Pts',(-5.91182889066216,0.586565893258212,
-4.34503674964823));
#93415=CARTESIAN_POINT('Ctrl Pts',(-5.95544747185424,0.595235853573338,
-4.29988382003214));
#93416=CARTESIAN_POINT('Ctrl Pts',(-6.08442456016951,0.621229052798543,
-4.16295606704363));
#93417=CARTESIAN_POINT('Ctrl Pts',(-6.16804687114597,0.638562584486272,
-4.06957751305599));
#93418=CARTESIAN_POINT('Ctrl Pts',(-6.24928440687142,0.655901906135767,
-3.97414486969703));
#93419=CARTESIAN_POINT('',(-5.8523355926758,0.499999998656627,-4.27933033369558));
#93420=CARTESIAN_POINT('Origin',(0.580899441097913,0.00294817653332898,
-1.39287596826395));
#93421=CARTESIAN_POINT('',(-5.6957799933929,0.544769999409456,-4.55760459135602));
#93422=CARTESIAN_POINT('Origin',(0.625220773956524,0.376341599776432,-0.841763888523078));
#93423=CARTESIAN_POINT('',(-5.45533889445124,0.499999999895941,-4.7751206845917));
#93424=CARTESIAN_POINT('Ctrl Pts',(-5.45533889440156,0.500000000015963,
-4.77512068407292));
#93425=CARTESIAN_POINT('Ctrl Pts',(-5.49622793426929,0.507497216227668,
-4.73978990121483));
#93426=CARTESIAN_POINT('Ctrl Pts',(-5.53671427714317,0.514976112406574,
-4.70399170969356));
#93427=CARTESIAN_POINT('Ctrl Pts',(-5.61711421180195,0.529942106266039,
-4.63125098296299));
#93428=CARTESIAN_POINT('Ctrl Pts',(-5.65688694612934,0.537396700836268,
-4.59440895204351));
#93429=CARTESIAN_POINT('Ctrl Pts',(-5.69577999365009,0.5447699998331,-4.55760459171267));
#93430=CARTESIAN_POINT('',(-5.6691432330339,0.552026825689722,-4.60221802656881));
#93431=CARTESIAN_POINT('Ctrl Pts',(-5.66914323294736,0.552026824715417,
-4.60221802667545));
#93432=CARTESIAN_POINT('Ctrl Pts',(-5.65065394335861,0.54747794861729,-4.61777626606602));
#93433=CARTESIAN_POINT('Ctrl Pts',(-5.63208862125364,0.542929076718581,
-4.63324459847705));
#93434=CARTESIAN_POINT('Ctrl Pts',(-5.61344861718722,0.53838066432356,-4.6486220894244));
#93435=CARTESIAN_POINT('Ctrl Pts',(-5.59480857815863,0.533832243397299,
-4.66399960921458));
#93436=CARTESIAN_POINT('Ctrl Pts',(-5.57609101865346,0.529279731820936,
-4.6792825543774));
#93437=CARTESIAN_POINT('Ctrl Pts',(-5.55729097574615,0.524710848291274,
-4.69445789598088));
#93438=CARTESIAN_POINT('Ctrl Pts',(-5.52356530743021,0.516514662183872,
-4.72168116031188));
#93439=CARTESIAN_POINT('Ctrl Pts',(-5.48957800753799,0.508277071515041,
-4.74857115672597));
#93440=CARTESIAN_POINT('Ctrl Pts',(-5.45533889445124,0.499999999895941,
-4.7751206845917));
#93441=CARTESIAN_POINT('',(-5.24884804614103,0.655900535635267,-5.2246489769404));
#93442=CARTESIAN_POINT('Ctrl Pts',(-5.24884804614103,0.655900535635267,
-5.2246489769404));
#93443=CARTESIAN_POINT('Ctrl Pts',(-5.32424723478688,0.638769108036499,
-5.12461689150441));
#93444=CARTESIAN_POINT('Ctrl Pts',(-5.39702445404335,0.621541657221802,
-5.02266249409391));
#93445=CARTESIAN_POINT('Ctrl Pts',(-5.53719788981516,0.58690578531704,-4.81508155141789));
#93446=CARTESIAN_POINT('Ctrl Pts',(-5.60456646001111,0.569504150534648,
-4.70949561946656));
#93447=CARTESIAN_POINT('Ctrl Pts',(-5.66914323445625,0.552026827033793,
-4.60221802720604));
#93448=CARTESIAN_POINT('',(-4.62792713082569,0.552026825464003,-5.64817547903717));
#93449=CARTESIAN_POINT('Ctrl Pts',(-4.62792713032582,0.552026825167876,
-5.64817547814032));
#93450=CARTESIAN_POINT('Ctrl Pts',(-4.65584459965789,0.556533631437719,
-5.63112728375854));
#93451=CARTESIAN_POINT('Ctrl Pts',(-4.68138612466351,0.560675802353204,
-5.61529567266897));
#93452=CARTESIAN_POINT('Ctrl Pts',(-4.73412070799516,0.569263221001596,
-5.58217489085802));
#93453=CARTESIAN_POINT('Ctrl Pts',(-4.76052433490904,0.573581753974147,
-5.56535883816861));
#93454=CARTESIAN_POINT('Ctrl Pts',(-4.83955915331318,0.586565893205448,
-5.51432066433269));
#93455=CARTESIAN_POINT('Ctrl Pts',(-4.89186450159291,0.595235853547021,
-5.47960009065209));
#93456=CARTESIAN_POINT('Ctrl Pts',(-5.0472615968587,0.621229052835566,-5.37359989373892));
#93457=CARTESIAN_POINT('Ctrl Pts',(-5.14899450119751,0.638561214261278,
-5.3003866574176));
#93458=CARTESIAN_POINT('Ctrl Pts',(-5.24884804621161,0.655900535773218,
-5.22464897706503));
#93459=CARTESIAN_POINT('',(-4.79558171331894,0.499999998635506,-5.43736112658256));
#93460=CARTESIAN_POINT('Origin',(0.86674356849252,0.0029485729091093,-1.23543653251669));
#93461=CARTESIAN_POINT('',(-4.58286555743328,0.544769999438325,-5.67547466095984));
#93462=CARTESIAN_POINT('Origin',(0.791557319693054,0.376341880383263,-0.687680335770907));
#93463=CARTESIAN_POINT('',(-4.30128630597295,0.499999999668149,-5.8362176204432));
#93464=CARTESIAN_POINT('Ctrl Pts',(-4.3012863060072,0.499999999733392,-5.83621762016198));
#93465=CARTESIAN_POINT('Ctrl Pts',(-4.34881445038693,0.507497215062244,
-5.81050278990619));
#93466=CARTESIAN_POINT('Ctrl Pts',(-4.39604979182165,0.514976110280007,
-5.78424491097689));
#93467=CARTESIAN_POINT('Ctrl Pts',(-4.49020422802782,0.529941643423082,
-5.73049008633081));
#93468=CARTESIAN_POINT('Ctrl Pts',(-4.53697271591002,0.537397143969364,
-5.70305604352401));
#93469=CARTESIAN_POINT('Ctrl Pts',(-4.58286555763755,0.544769999934216,
-5.67547466143228));
#93470=CARTESIAN_POINT('',(-4.54726098010409,0.552026825712293,-5.71331894285122));
#93471=CARTESIAN_POINT('Ctrl Pts',(-4.54726098003085,0.552026824734663,
-5.71331894296981));
#93472=CARTESIAN_POINT('Ctrl Pts',(-4.52585939887053,0.547477948879278,
-5.72453878810256));
#93473=CARTESIAN_POINT('Ctrl Pts',(-4.5044028899783,0.542929077117612,-5.73565448379864));
#93474=CARTESIAN_POINT('Ctrl Pts',(-4.48289297336656,0.538380664817293,
-5.74666540740134));
#93475=CARTESIAN_POINT('Ctrl Pts',(-4.4613830164101,0.533832243985818,-5.75767635165651));
#93476=CARTESIAN_POINT('Ctrl Pts',(-4.43981768212375,0.529279732533536,
-5.76857826781063));
#93477=CARTESIAN_POINT('Ctrl Pts',(-4.41819492443471,0.524710849116548,
-5.77935736461706));
#93478=CARTESIAN_POINT('Ctrl Pts',(-4.37940554536671,0.516514662796208,
-5.79869414293404));
#93479=CARTESIAN_POINT('Ctrl Pts',(-4.34043229426036,0.508277071898963,
-5.81764920186379));
#93480=CARTESIAN_POINT('Ctrl Pts',(-4.30128630597295,0.499999999668149,
-5.8362176204432));
#93481=CARTESIAN_POINT('',(-4.00298780534354,0.655900535589649,-6.23084676214381));
#93482=CARTESIAN_POINT('Ctrl Pts',(-4.00298780534354,0.655900535589649,
-6.23084676214381));
#93483=CARTESIAN_POINT('Ctrl Pts',(-4.09812814433568,0.63876910799483,-6.14936196802781));
#93484=CARTESIAN_POINT('Ctrl Pts',(-4.19112105437463,0.621541657181549,
-6.06543615860511));
#93485=CARTESIAN_POINT('Ctrl Pts',(-4.37264107972524,0.586905785291398,
-5.89284148821998));
#93486=CARTESIAN_POINT('Ctrl Pts',(-4.46113246462634,0.569504150480316,
-5.80420634770189));
#93487=CARTESIAN_POINT('Ctrl Pts',(-4.54726098115828,0.552026826991961,
-5.71331894360413));
#93488=CARTESIAN_POINT('',(-3.30553799692616,0.552026825425635,-6.51099180780492));
#93489=CARTESIAN_POINT('Ctrl Pts',(-3.30553799661828,0.552026825151617,
-6.51099180679462));
#93490=CARTESIAN_POINT('Ctrl Pts',(-3.33646762905524,0.556533631448746,
-6.50034362033982));
#93491=CARTESIAN_POINT('Ctrl Pts',(-3.36481533595166,0.560675802386594,
-6.49037281634335));
#93492=CARTESIAN_POINT('Ctrl Pts',(-3.42343700322561,0.569263221057426,
-6.46936275654394));
#93493=CARTESIAN_POINT('Ctrl Pts',(-3.4528382822726,0.573581754030701,-6.45861585311779));
#93494=CARTESIAN_POINT('Ctrl Pts',(-3.54099700923227,0.586565893258024,
-6.42576107312447));
#93495=CARTESIAN_POINT('Ctrl Pts',(-3.5995433845281,0.595235853593481,-6.40309635090712));
#93496=CARTESIAN_POINT('Ctrl Pts',(-3.7740942910582,0.621229052873939,-6.3329801616529));
#93497=CARTESIAN_POINT('Ctrl Pts',(-3.88918741828664,0.638561214300223,
-6.28334817732656));
#93498=CARTESIAN_POINT('Ctrl Pts',(-4.00298780541949,0.655900535838296,
-6.23084676239056));
#93499=CARTESIAN_POINT('',(-3.51459176321357,0.499999998556402,-6.34114695680857));
#93500=CARTESIAN_POINT('Origin',(1.11206245074807,0.0029480682560324,-1.02022796045556));
#93501=CARTESIAN_POINT('',(-3.25566142038069,0.544769999525692,-6.52796584410679));
#93502=CARTESIAN_POINT('Origin',(0.920882297147526,0.376341845396332,-0.501441043894132));
#93503=CARTESIAN_POINT('',(-2.94611035073431,0.499999999616658,-6.62441950656243));
#93504=CARTESIAN_POINT('Ctrl Pts',(-2.94611035081038,0.499999999669515,
-6.62441950634589));
#93505=CARTESIAN_POINT('Ctrl Pts',(-2.99805524028318,0.507497214728035,
-6.60952302110954));
#93506=CARTESIAN_POINT('Ctrl Pts',(-3.04983091180412,0.514976109662867,
-6.59403323946265));
#93507=CARTESIAN_POINT('Ctrl Pts',(-3.15333976933434,0.529941642974774,
-6.56177559288136));
#93508=CARTESIAN_POINT('Ctrl Pts',(-3.20491234608337,0.537397143866723,
-6.54503678468685));
#93509=CARTESIAN_POINT('Ctrl Pts',(-3.25566142044168,0.544769999834553,
-6.52796584442151));
#93510=CARTESIAN_POINT('',(-3.21275385699847,0.552026825371849,-6.55727141543876));
#93511=CARTESIAN_POINT('Ctrl Pts',(-3.21275385729611,0.552026824836102,
-6.55727141537468));
#93512=CARTESIAN_POINT('Ctrl Pts',(-3.18944069859206,0.547477949075286,
-6.56362823961408));
#93513=CARTESIAN_POINT('Ctrl Pts',(-3.16609628497767,0.542929077270821,
-6.56987154130488));
#93514=CARTESIAN_POINT('Ctrl Pts',(-3.1427222351911,0.538380664940049,-6.57600103934811));
#93515=CARTESIAN_POINT('Ctrl Pts',(-3.11934814156362,0.533832244078171,
-6.58213054888797));
#93516=CARTESIAN_POINT('Ctrl Pts',(-3.09594340312024,0.529279732637972,
-6.5881416748998));
#93517=CARTESIAN_POINT('Ctrl Pts',(-3.0725089863305,0.524710849234664,-6.59402050867988));
#93518=CARTESIAN_POINT('Ctrl Pts',(-3.03046964479739,0.516514662764997,
-6.60456663420605));
#93519=CARTESIAN_POINT('Ctrl Pts',(-2.98833278843496,0.508277071749586,
-6.6147004376975));
#93520=CARTESIAN_POINT('Ctrl Pts',(-2.94611035073431,0.499999999616658,
-6.62441950656243));
#93521=CARTESIAN_POINT('',(-2.56995230272842,0.655900535691932,-6.94569707849852));
#93522=CARTESIAN_POINT('Ctrl Pts',(-2.56994356813194,0.65590189068777,-6.94570175512237));
#93523=CARTESIAN_POINT('Ctrl Pts',(-2.68037640112295,0.638770463049698,
-6.88657439066599));
#93524=CARTESIAN_POINT('Ctrl Pts',(-2.78924549159031,0.621541657200288,
-6.82459677010367));
#93525=CARTESIAN_POINT('Ctrl Pts',(-3.00362443206904,0.586905785275581,
-6.69505870685461));
#93526=CARTESIAN_POINT('Ctrl Pts',(-3.10910087303173,0.569504150420659,
-6.62751883845557));
#93527=CARTESIAN_POINT('Ctrl Pts',(-3.21275385797399,0.552026826943697,
-6.5572714164871));
#93528=CARTESIAN_POINT('',(-1.8285855811266,0.552026825425414,-7.06936139573953));
#93529=CARTESIAN_POINT('Ctrl Pts',(-1.82858558103768,0.552026825163243,
-7.06936139465403));
#93530=CARTESIAN_POINT('Ctrl Pts',(-1.86108114124179,0.556533631476899,
-7.06561111358071));
#93531=CARTESIAN_POINT('Ctrl Pts',(-1.8909095225058,0.560675802405676,-7.06196734049061));
#93532=CARTESIAN_POINT('Ctrl Pts',(-1.9526771894402,0.569263221073273,-7.05405040986236));
#93533=CARTESIAN_POINT('Ctrl Pts',(-1.98370134940776,0.573581754044103,
-7.04987516898144));
#93534=CARTESIAN_POINT('Ctrl Pts',(-2.07686178061951,0.586565893263386,
-7.03674003587851));
#93535=CARTESIAN_POINT('Ctrl Pts',(-2.13891161936245,0.595235853592223,
-7.02719094237657));
#93536=CARTESIAN_POINT('Ctrl Pts',(-2.32445453032465,0.621229052843979,
-6.996237315988));
#93537=CARTESIAN_POINT('Ctrl Pts',(-2.4475262534217,0.638561214240612,-6.97250732017752));
#93538=CARTESIAN_POINT('Ctrl Pts',(-2.56995230273162,0.655900535729553,
-6.94569707853746));
#93539=CARTESIAN_POINT('',(-2.06926340708605,0.499999998689052,-6.94842780378674));
#93540=CARTESIAN_POINT('Origin',(1.30538195718773,0.00294813417282574,-0.757314928844572));
#93541=CARTESIAN_POINT('',(-1.77622617508296,0.544769999508108,-7.0752165988522));
#93542=CARTESIAN_POINT('Origin',(1.00714758409605,0.376341924620739,-0.291755136603755));
#93543=CARTESIAN_POINT('',(-1.45317754992019,0.499999999562998,-7.10287089873148));
#93544=CARTESIAN_POINT('Ctrl Pts',(-1.453177549962,0.499999999591156,-7.10287089861264));
#93545=CARTESIAN_POINT('Ctrl Pts',(-1.50711029708834,0.50749721411147,-7.09948930088892));
#93546=CARTESIAN_POINT('Ctrl Pts',(-1.56100532369139,0.514976108586445,
-7.09549190108463));
#93547=CARTESIAN_POINT('Ctrl Pts',(-1.66903199485859,0.529942106372944,
-7.08623947785291));
#93548=CARTESIAN_POINT('Ctrl Pts',(-1.722990644337,0.537396701470885,-7.0809792252342));
#93549=CARTESIAN_POINT('Ctrl Pts',(-1.7762261750738,0.544769999857778,-7.07521659921502));
#93550=CARTESIAN_POINT('',(-1.72802193438852,0.552026825864411,-7.09461316486523));
#93551=CARTESIAN_POINT('Ctrl Pts',(-1.72802193417285,0.552026824670133,
-7.0946131647742));
#93552=CARTESIAN_POINT('Ctrl Pts',(-1.7038872937459,0.547477948670733,-7.09580972983484));
#93553=CARTESIAN_POINT('Ctrl Pts',(-1.67974653386692,0.542929076807001,
-7.09688870775154));
#93554=CARTESIAN_POINT('Ctrl Pts',(-1.65560129511354,0.538380664413428,
-7.09785017177835));
#93555=CARTESIAN_POINT('Ctrl Pts',(-1.63145601107289,0.533832243488767,
-7.09881163760849));
#93556=CARTESIAN_POINT('Ctrl Pts',(-1.60730624762677,0.529279732034816,
-7.0996508999705));
#93557=CARTESIAN_POINT('Ctrl Pts',(-1.58315593862026,0.524710848592855,
-7.10035458302231));
#93558=CARTESIAN_POINT('Ctrl Pts',(-1.53983234963671,0.516514662436402,
-7.10161693023715));
#93559=CARTESIAN_POINT('Ctrl Pts',(-1.49650216271934,0.508277071708823,
-7.10245563246828));
#93560=CARTESIAN_POINT('Ctrl Pts',(-1.45317754992019,0.499999999562998,
-7.10287089873148));
#93561=CARTESIAN_POINT('',(-1.01674868797125,0.655900535661223,-7.33577431833995));
#93562=CARTESIAN_POINT('Ctrl Pts',(-1.01674868797125,0.655900535661222,
-7.33577431833995));
#93563=CARTESIAN_POINT('Ctrl Pts',(-1.1373102980958,0.638769108040252,-7.30176911356082));
#93564=CARTESIAN_POINT('Ctrl Pts',(-1.25694791022009,0.621541657216736,
-7.26464682128884));
#93565=CARTESIAN_POINT('Ctrl Pts',(-1.49416164478959,0.586905785305847,
-7.18422242117417));
#93566=CARTESIAN_POINT('Ctrl Pts',(-1.61169117978909,0.569504150566262,
-7.14093591456739));
#93567=CARTESIAN_POINT('Ctrl Pts',(-1.72802193502821,0.55202682707541,-7.09461316601479));
#93568=CARTESIAN_POINT('',(-0.266130534258616,0.552026825448126,-7.29717550202562));
#93569=CARTESIAN_POINT('Ctrl Pts',(-0.266130534397895,0.552026825135067,
-7.29717550108625));
#93570=CARTESIAN_POINT('Ctrl Pts',(-0.298672565884604,0.556533631418656,
-7.30049848436175));
#93571=CARTESIAN_POINT('Ctrl Pts',(-0.328586879728604,0.560675802348281,
-7.30335212091617));
#93572=CARTESIAN_POINT('Ctrl Pts',(-0.390612359103792,0.569263221019371,
-7.30889850628478));
#93573=CARTESIAN_POINT('Ctrl Pts',(-0.421808744919157,0.57358175399926,
-7.31149015754806));
#93574=CARTESIAN_POINT('Ctrl Pts',(-0.515614802533565,0.586565893231015,
-7.31868885547649));
#93575=CARTESIAN_POINT('Ctrl Pts',(-0.578266723431897,0.59523585356534,
-7.32270189562898));
#93576=CARTESIAN_POINT('Ctrl Pts',(-0.766125859322722,0.621229052856937,
-7.33235818909006));
#93577=CARTESIAN_POINT('Ctrl Pts',(-0.891421481876299,0.638561214284284,
-7.33563976988323));
#93578=CARTESIAN_POINT('Ctrl Pts',(-1.01674868795464,0.655900535780308,
-7.33577431846248));
#93579=CARTESIAN_POINT('',(-0.527178595390885,0.499999998624239,-7.23080788849307));
#93580=CARTESIAN_POINT('Origin',(1.43766293562731,0.00294815640760344,-0.458991651664984));
#93581=CARTESIAN_POINT('',(-0.213736567552909,0.544769999381455,-7.29163808917903));
#93582=CARTESIAN_POINT('Origin',(1.04631978522547,0.376341808593957,-0.0684270503981665));
#93583=CARTESIAN_POINT('',(-1.6931015459671E-12,0.515079044621721,-7.26507904462173));
#93584=CARTESIAN_POINT('Ctrl Pts',(-0.21373656742832,0.544769999882563,
-7.29163808968401));
#93585=CARTESIAN_POINT('Ctrl Pts',(-0.1531484544219,0.536377426449655,-7.2850179040679));
#93586=CARTESIAN_POINT('Ctrl Pts',(-0.0921392149746007,0.527925589541755,
-7.27759928397786));
#93587=CARTESIAN_POINT('Ctrl Pts',(-0.0206282398277339,0.517957822703902,
-7.26793586550817));
#93588=CARTESIAN_POINT('Ctrl Pts',(-0.0103124763152848,0.516518781586931,
-7.26651878158693));
#93589=CARTESIAN_POINT('Ctrl Pts',(-3.38786891177452E-12,0.515079044621721,
-7.26507904462173));
#93590=CARTESIAN_POINT('',(1.70500103440517E-15,-3.33066907387547E-15,-6.75));
#93591=CARTESIAN_POINT('',(1.70500103440517E-15,0.,-6.75000000000001));
#93592=CARTESIAN_POINT('Origin',(0.,0.,0.));
#93593=CARTESIAN_POINT('',(0.107704216070514,0.499999999886364,-7.24919994256545));
#93594=CARTESIAN_POINT('Ctrl Pts',(-3.38786891177452E-12,0.515079044621721,
-7.26507904462173));
#93595=CARTESIAN_POINT('Ctrl Pts',(0.0359424207011893,0.510061080929743,
-7.26006108092977));
#93596=CARTESIAN_POINT('Ctrl Pts',(0.0718449099581247,0.505034664458654,
-7.25476793811845));
#93597=CARTESIAN_POINT('Ctrl Pts',(0.107704215711866,0.500000000004417,
-7.24919994219928));
#93598=CARTESIAN_POINT('Ctrl Pts',(0.107704215939162,0.499999999815039,
-7.2491999420065));
#93599=CARTESIAN_POINT('Ctrl Pts',(0.089612700297626,0.503531634900662,
-7.25300075962746));
#93600=CARTESIAN_POINT('Ctrl Pts',(0.0715042823655147,0.507055955084127,
-7.25672637957618));
#93601=CARTESIAN_POINT('Ctrl Pts',(0.0356018297225805,0.514022459397225,
-7.2639570313917));
#93602=CARTESIAN_POINT('Ctrl Pts',(0.0178086383737658,0.517464881394668,
-7.26746488139467));
#93603=CARTESIAN_POINT('Ctrl Pts',(3.97374700519909E-12,0.520900163746503,
-7.27090016374651));
#93604=CARTESIAN_POINT('Origin',(-1.99005104861445E-16,1.2,0.));
#93605=CARTESIAN_POINT('',(-3.25,1.2,-3.9801020972289E-16));
#93606=CARTESIAN_POINT('Origin',(-1.99005104861445E-16,1.2,0.));
#93607=CARTESIAN_POINT('',(-3.25,-2.77555756156289E-16,-3.9801020972289E-16));
#93608=CARTESIAN_POINT('',(-3.25,1.2,-3.9801020972289E-16));
#93609=CARTESIAN_POINT('Origin',(-7.89088642168964E-17,0.,0.));
#93610=CARTESIAN_POINT('Origin',(2.53163762382963E-15,0.,-3.4647252052902E-15));
#93611=CARTESIAN_POINT('',(-0.162489628597199,0.552026825816562,-7.30021868724729));
#93612=CARTESIAN_POINT('Ctrl Pts',(3.97374700519909E-12,0.520900163746503,
-7.27090016374651));
#93613=CARTESIAN_POINT('Ctrl Pts',(-0.00482179263778413,0.521830286466864,
-7.27183028646687));
#93614=CARTESIAN_POINT('Ctrl Pts',(-0.00964471767961773,0.522759885796396,
-7.27275508934469));
#93615=CARTESIAN_POINT('Ctrl Pts',(-0.0642175574728398,0.53327019661184,
-7.28315686485796));
#93616=CARTESIAN_POINT('Ctrl Pts',(-0.114535467221313,0.54287200381573,
-7.29212897072435));
#93617=CARTESIAN_POINT('Ctrl Pts',(-0.162489634298702,0.552026826,-7.30021868757157));
#93618=CARTESIAN_POINT('Ctrl Pts',(-0.162489633664295,0.552026826,-7.30021868758569));
#93619=CARTESIAN_POINT('Ctrl Pts',(-0.108422033090161,0.559674024978565,
-7.30907122741516));
#93620=CARTESIAN_POINT('Ctrl Pts',(-0.0542552256312394,0.567306736081167,
-7.31730673607856));
#93621=CARTESIAN_POINT('Ctrl Pts',(-3.52635867725153E-10,0.574924266631643,
-7.32492426663165));
#93622=CARTESIAN_POINT('Origin',(-4.28626379701574E-16,3.7,0.));
#93623=CARTESIAN_POINT('',(-1.28587913910472E-15,3.7,7.));
#93624=CARTESIAN_POINT('Origin',(-4.28626379701574E-16,3.7,0.));
#93625=CARTESIAN_POINT('',(-1.28587913910472E-15,1.2,7.));
#93626=CARTESIAN_POINT('',(-1.28587913910472E-15,3.7,7.));
#93627=CARTESIAN_POINT('Origin',(-4.28626379701574E-16,1.2,0.));
#93628=CARTESIAN_POINT('Origin',(-3.75048082238878E-16,5.2,0.));
#93629=CARTESIAN_POINT('',(6.125,5.2,7.68465866464964E-16));
#93630=CARTESIAN_POINT('',(-6.125,5.2,-7.50096164477754E-16));
#93631=CARTESIAN_POINT('Origin',(0.,5.2,0.));
#93632=CARTESIAN_POINT('',(-6.125,3.7,-7.50096164477754E-16));
#93633=CARTESIAN_POINT('',(-6.125,5.2,-7.50096164477754E-16));
#93634=CARTESIAN_POINT('Origin',(-5.87463201746242E-16,3.7,0.));
#93635=CARTESIAN_POINT('Origin',(0.,5.2,0.));
#93636=CARTESIAN_POINT('Origin',(-3.75048082238878E-16,5.2,0.));
#93637=CARTESIAN_POINT('',(6.425,5.5,-7.86835568452174E-16));
#93638=CARTESIAN_POINT('',(6.125,5.2,-7.50096164477754E-16));
#93639=CARTESIAN_POINT('Origin',(0.,5.5,0.));
#93640=CARTESIAN_POINT('Origin',(-9.54665999398665E-15,5.5,-2.76142397078324E-15));
#93641=CARTESIAN_POINT('',(-0.213736565703542,4.95523000035635,-7.29163808949555));
#93642=CARTESIAN_POINT('',(0.107704216070517,5.00000000011364,-7.24919994256545));
#93643=CARTESIAN_POINT('Ctrl Pts',(-0.213736565699183,4.95523000035695,
-7.29163808949507));
#93644=CARTESIAN_POINT('Ctrl Pts',(-0.152772191073571,4.9636746929782,-7.28497679148068));
#93645=CARTESIAN_POINT('Ctrl Pts',(-0.0913875379650499,4.97217869295328,
-7.27750760769982));
#93646=CARTESIAN_POINT('Ctrl Pts',(0.016083985202725,4.98715979332583,-7.26296732930841));
#93647=CARTESIAN_POINT('Ctrl Pts',(0.0619292881126885,4.99357317727733,
-7.256307570323));
#93648=CARTESIAN_POINT('Ctrl Pts',(0.107704215711865,4.99999999999558,-7.24919994219928));
#93649=CARTESIAN_POINT('',(-0.5271785952156,5.00000000119539,-7.23080788868627));
#93650=CARTESIAN_POINT('Origin',(1.04631978098754,5.12365820970434,-0.0684270868039383));
#93651=CARTESIAN_POINT('',(-0.266130538254917,4.94797317376359,-7.29717550201765));
#93652=CARTESIAN_POINT('Origin',(1.43766416616257,5.4970519860903,-0.458987126402098));
#93653=CARTESIAN_POINT('',(-1.01674868753842,4.84409946427727,-7.33577431846203));
#93654=CARTESIAN_POINT('Ctrl Pts',(-1.01674868753842,4.84409946427728,-7.33577431846203));
#93655=CARTESIAN_POINT('Ctrl Pts',(-0.891421482506232,4.86143878562856,
-7.33563976987693));
#93656=CARTESIAN_POINT('Ctrl Pts',(-0.76612586099832,4.87877094691128,-7.33235818913045));
#93657=CARTESIAN_POINT('Ctrl Pts',(-0.578266726672991,4.90476414598618,
-7.32270189581848));
#93658=CARTESIAN_POINT('Ctrl Pts',(-0.515614806296964,4.91343410624817,
-7.31868885572902));
#93659=CARTESIAN_POINT('Ctrl Pts',(-0.421808749462441,4.92641824537184,
-7.31149015791479));
#93660=CARTESIAN_POINT('Ctrl Pts',(-0.39061236390569,4.93073677831587,-7.30889850669274));
#93661=CARTESIAN_POINT('Ctrl Pts',(-0.328583770897313,4.9393246280689,-7.3033518429423));
#93662=CARTESIAN_POINT('Ctrl Pts',(-0.2986763903816,4.94346583891753,-7.30049887487933));
#93663=CARTESIAN_POINT('Ctrl Pts',(-0.266130538384521,4.94797317431282,
-7.29717550149333));
#93664=CARTESIAN_POINT('',(-1.7280219382183,4.94797317381307,-7.09461316422209));
#93665=CARTESIAN_POINT('Ctrl Pts',(-1.72802193844647,4.94797317343814,-7.09461316465364));
#93666=CARTESIAN_POINT('Ctrl Pts',(-1.61169118369406,4.9304958500154,-7.14093591308127));
#93667=CARTESIAN_POINT('Ctrl Pts',(-1.4941616457248,4.91309421483262,-7.18422242082973));
#93668=CARTESIAN_POINT('Ctrl Pts',(-1.25694791103012,4.87845834289962,-7.26464682104157));
#93669=CARTESIAN_POINT('Ctrl Pts',(-1.1373102982891,4.86123089198667,-7.30176911351439));
#93670=CARTESIAN_POINT('Ctrl Pts',(-1.01674868753842,4.84409946427728,-7.33577431846203));
#93671=CARTESIAN_POINT('',(-1.45317754970485,5.00000000046694,-7.10287089874499));
#93672=CARTESIAN_POINT('Ctrl Pts',(-1.45317754970711,5.00000000048678,-7.10287089858523));
#93673=CARTESIAN_POINT('Ctrl Pts',(-1.49899199588298,4.99124725113094,-7.10243176744319));
#93674=CARTESIAN_POINT('Ctrl Pts',(-1.54480889124354,4.98253937036453,-7.10151921695448));
#93675=CARTESIAN_POINT('Ctrl Pts',(-1.63675210786151,4.96515485125473,-7.09873687841323));
#93676=CARTESIAN_POINT('Ctrl Pts',(-1.68349106311083,4.95636631499385,-7.09682095024594));
#93677=CARTESIAN_POINT('Ctrl Pts',(-1.72802193834098,4.94797317467986,-7.09461316340132));
#93678=CARTESIAN_POINT('',(-1.77622617387013,4.95523000030894,-7.07521659934531));
#93679=CARTESIAN_POINT('Ctrl Pts',(-1.77622617387013,4.95523000030894,-7.07521659934532));
#93680=CARTESIAN_POINT('Ctrl Pts',(-1.72299384371354,4.96260285540458,-7.08097887890016));
#93681=CARTESIAN_POINT('Ctrl Pts',(-1.66902865274438,4.97005835664292,-7.08623976410856));
#93682=CARTESIAN_POINT('Ctrl Pts',(-1.56100532539457,4.9850238911777,-7.09549190093333));
#93683=CARTESIAN_POINT('Ctrl Pts',(-1.50711029785297,4.99250278578221,-7.09948930084237));
#93684=CARTESIAN_POINT('Ctrl Pts',(-1.45317754977974,5.00000000043418,-7.10287089862406));
#93685=CARTESIAN_POINT('',(-2.06926340799607,5.00000000131937,-6.94842780350358));
#93686=CARTESIAN_POINT('Origin',(1.00714768739185,5.12365815569165,-0.291754918966577));
#93687=CARTESIAN_POINT('',(-1.82858558437265,4.94797317379205,-7.06936139493043));
#93688=CARTESIAN_POINT('Origin',(1.3053840183489,5.49705199769362,-0.757310959927074));
#93689=CARTESIAN_POINT('',(-2.56995230260316,4.84409946428864,-6.94569707856559));
#93690=CARTESIAN_POINT('Ctrl Pts',(-2.56995230260316,4.84409946428864,-6.94569707856559));
#93691=CARTESIAN_POINT('Ctrl Pts',(-2.44752625408122,4.86143878566591,-6.97250732003083));
#93692=CARTESIAN_POINT('Ctrl Pts',(-2.32445453178037,4.87877094695098,-6.99623731570619));
#93693=CARTESIAN_POINT('Ctrl Pts',(-2.13891162202374,4.90476414603551,-7.0271909419521));
#93694=CARTESIAN_POINT('Ctrl Pts',(-2.07686178368571,4.91343410630846,-7.03674003541638));
#93695=CARTESIAN_POINT('Ctrl Pts',(-1.98370135308225,4.92641824544418,-7.04987516847821));
#93696=CARTESIAN_POINT('Ctrl Pts',(-1.9526771933166,4.93073677838734,-7.0540504093481));
#93697=CARTESIAN_POINT('Ctrl Pts',(-1.89090642570761,4.93932462813562,-7.06196773743291));
#93698=CARTESIAN_POINT('Ctrl Pts',(-1.86108495939093,4.9434658389819,-7.06561067291908));
#93699=CARTESIAN_POINT('Ctrl Pts',(-1.82858558437693,4.94797317437364,-7.06936139426864));
#93700=CARTESIAN_POINT('',(-3.21275385990511,4.9479731738326,-6.55727141456418));
#93701=CARTESIAN_POINT('Ctrl Pts',(-3.21275386023597,4.9479731734377,-6.55727141495412));
#93702=CARTESIAN_POINT('Ctrl Pts',(-3.10910087559271,4.93049585000559,-6.62751883677731));
#93703=CARTESIAN_POINT('Ctrl Pts',(-3.00362443262307,4.91309421481583,-6.69505870649984));
#93704=CARTESIAN_POINT('Ctrl Pts',(-2.78924549212175,4.87845834288368,-6.82459676980254));
#93705=CARTESIAN_POINT('Ctrl Pts',(-2.68038513592731,4.86123089197814,-6.88656971393363));
#93706=CARTESIAN_POINT('Ctrl Pts',(-2.56995230260316,4.84409946428864,-6.94569707856559));
#93707=CARTESIAN_POINT('',(-2.94611035073431,5.00000000038334,-6.62441950656244));
#93708=CARTESIAN_POINT('Ctrl Pts',(-2.94611035068246,5.00000000041537,-6.62441950630989));
#93709=CARTESIAN_POINT('Ctrl Pts',(-2.99075928957681,4.99124724929563,-6.61414188797));
#93710=CARTESIAN_POINT('Ctrl Pts',(-3.03530883451336,4.9825393695754,-6.60340139544388));
#93711=CARTESIAN_POINT('Ctrl Pts',(-3.12450434638238,4.96515485090219,-6.5809190335638));
#93712=CARTESIAN_POINT('Ctrl Pts',(-3.16973870290945,4.95636631460213,-6.56900040494851));
#93713=CARTESIAN_POINT('Ctrl Pts',(-3.21275385984555,4.94797317473687,-6.55727141369868));
#93714=CARTESIAN_POINT('',(-3.25566141942808,4.95523000031271,-6.52796584476247));
#93715=CARTESIAN_POINT('Ctrl Pts',(-3.25566141942808,4.95523000031271,-6.52796584476247));
#93716=CARTESIAN_POINT('Ctrl Pts',(-3.20491234522498,4.96260285625755,-6.54503678496748));
#93717=CARTESIAN_POINT('Ctrl Pts',(-3.15333976865463,4.97005835712355,-6.56177559309746));
#93718=CARTESIAN_POINT('Ctrl Pts',(-3.04983091146342,4.98502389038635,-6.59403323956458));
#93719=CARTESIAN_POINT('Ctrl Pts',(-2.99805524011227,4.99250278529663,-6.60952302115855));
#93720=CARTESIAN_POINT('Ctrl Pts',(-2.94611035081039,5.00000000033048,-6.62441950634589));
#93721=CARTESIAN_POINT('',(-3.51459176313735,5.00000000126224,-6.34114695705619));
#93722=CARTESIAN_POINT('Origin',(0.920882278249773,5.12365817302287,-0.50144107485158));
#93723=CARTESIAN_POINT('',(-3.30553800089752,4.94797317379562,-6.51099180615017));
#93724=CARTESIAN_POINT('Origin',(1.11206539330992,5.49705207100037,-1.02022445880335));
#93725=CARTESIAN_POINT('',(-4.00298780463037,4.84409946428194,-6.23084676275461));
#93726=CARTESIAN_POINT('Ctrl Pts',(-4.00298780463038,4.84409946428194,-6.23084676275462));
#93727=CARTESIAN_POINT('Ctrl Pts',(-3.88918741840099,4.86143878568141,-6.28334817725779));
#93728=CARTESIAN_POINT('Ctrl Pts',(-3.77409429209713,4.87877094696915,-6.33298016119694));
#93729=CARTESIAN_POINT('Ctrl Pts',(-3.59954338698338,4.90476414604199,-6.40309634994019));
#93730=CARTESIAN_POINT('Ctrl Pts',(-3.54099701216533,4.91343410630816,-6.42576107199865));
#93731=CARTESIAN_POINT('Ctrl Pts',(-3.45283828592698,4.92641824543199,-6.4586158517722));
#93732=CARTESIAN_POINT('Ctrl Pts',(-3.42343700712078,4.93073677837089,-6.4693627551283));
#93733=CARTESIAN_POINT('Ctrl Pts',(-3.36481534024033,4.93932419698624,-6.49037281482567));
#93734=CARTESIAN_POINT('Ctrl Pts',(-3.33646763361339,4.94346636788396,-6.50034361875279));
#93735=CARTESIAN_POINT('Ctrl Pts',(-3.30553800070206,4.94797317425333,-6.51099180538869));
#93736=CARTESIAN_POINT('',(-4.54726098251639,4.94797317384177,-5.71331894151198));
#93737=CARTESIAN_POINT('Ctrl Pts',(-4.54726098289168,4.94797317335979,-5.71331894177495));
#93738=CARTESIAN_POINT('Ctrl Pts',(-4.46113246652684,4.93049584989789,-5.80420634576006));
#93739=CARTESIAN_POINT('Ctrl Pts',(-4.37264108000304,4.91309421476323,-5.89284148794172));
#93740=CARTESIAN_POINT('Ctrl Pts',(-4.19112105443983,4.87845834282927,-6.06543615855723));
#93741=CARTESIAN_POINT('Ctrl Pts',(-4.09812814402033,4.86123089194598,-6.14936196831929));
#93742=CARTESIAN_POINT('Ctrl Pts',(-4.00298780463038,4.84409946428194,-6.23084676275461));
#93743=CARTESIAN_POINT('',(-4.30128630597296,5.00000000033185,-5.83621762044319));
#93744=CARTESIAN_POINT('Ctrl Pts',(-4.30128630584344,5.00000000037138,-5.83621762015252));
#93745=CARTESIAN_POINT('Ctrl Pts',(-4.34268199875195,4.99124724802707,-5.81658208220761));
#93746=CARTESIAN_POINT('Ctrl Pts',(-4.38388110883993,4.98253936886008,-5.79651586247342));
#93747=CARTESIAN_POINT('Ctrl Pts',(-4.46615823557318,4.9651548502495,-5.75538472749207));
#93748=CARTESIAN_POINT('Ctrl Pts',(-4.5077728825359,4.95636631460042,-5.73402070142715));
#93749=CARTESIAN_POINT('Ctrl Pts',(-4.54726098217293,4.94797317484349,-5.71331894045073));
#93750=CARTESIAN_POINT('',(-4.58286555616587,4.95523000030221,-5.67547466231674));
#93751=CARTESIAN_POINT('Ctrl Pts',(-4.58286555616587,4.95523000030221,-5.67547466231674));
#93752=CARTESIAN_POINT('Ctrl Pts',(-4.53696995549485,4.96260329950046,-5.70305770250615));
#93753=CARTESIAN_POINT('Ctrl Pts',(-4.4902071393007,4.97005789384013,-5.73048842422905));
#93754=CARTESIAN_POINT('Ctrl Pts',(-4.39604979132316,4.98502388979892,-5.78424491125399));
#93755=CARTESIAN_POINT('Ctrl Pts',(-4.34881445013615,4.99250278497732,-5.81050279004188));
#93756=CARTESIAN_POINT('Ctrl Pts',(-4.30128630600721,5.00000000026661,-5.83621762016198));
#93757=CARTESIAN_POINT('',(-4.79558171325023,5.00000000122353,-5.43736112682667));
#93758=CARTESIAN_POINT('Origin',(0.791557283173849,5.12365813463513,-0.687680371718459));
#93759=CARTESIAN_POINT('',(-4.62792713406617,4.94797317374629,-5.64817547655208));
#93760=CARTESIAN_POINT('Origin',(0.86674739196922,5.49705157326691,-1.23543359314626));
#93761=CARTESIAN_POINT('',(-5.24884804582745,4.84409946429349,-5.22464897735641));
#93762=CARTESIAN_POINT('Ctrl Pts',(-5.24884804582745,4.84409946429349,-5.22464897735642));
#93763=CARTESIAN_POINT('Ctrl Pts',(-5.14899450165896,4.86143878565774,-5.30038665705747));
#93764=CARTESIAN_POINT('Ctrl Pts',(-5.04726159819795,4.87877094693586,-5.37359989277013));
#93765=CARTESIAN_POINT('Ctrl Pts',(-4.8918645042952,4.90476414600326,-5.47960008883646));
#93766=CARTESIAN_POINT('Ctrl Pts',(-4.83955915647839,4.91343410627102,-5.51432066224534));
#93767=CARTESIAN_POINT('Ctrl Pts',(-4.76052433877805,4.92641824539201,-5.56535883569174));
#93768=CARTESIAN_POINT('Ctrl Pts',(-4.73412071209948,4.93073677832799,-5.58217488825481));
#93769=CARTESIAN_POINT('Ctrl Pts',(-4.68138348157109,4.93932462805598,-5.61529733272974));
#93770=CARTESIAN_POINT('Ctrl Pts',(-4.65584788071166,4.94346583888768,-5.63112528011843));
#93771=CARTESIAN_POINT('Ctrl Pts',(-4.62792713381804,4.94797317426837,-5.64817547600773));
#93772=CARTESIAN_POINT('',(-5.66914323582772,4.94797317380338,-4.60221802398246));
#93773=CARTESIAN_POINT('Ctrl Pts',(-5.6691432362703,4.94797317345716,-4.60221802419248));
#93774=CARTESIAN_POINT('Ctrl Pts',(-5.60456646211845,4.93049585002012,-4.70949561608431));
#93775=CARTESIAN_POINT('Ctrl Pts',(-5.53719789031756,4.91309421481273,-4.81508155063048));
#93776=CARTESIAN_POINT('Ctrl Pts',(-5.39702445448899,4.87845834288268,-5.02266249347739));
#93777=CARTESIAN_POINT('Ctrl Pts',(-5.32424723486628,4.86123089197962,-5.12461689141406));
#93778=CARTESIAN_POINT('Ctrl Pts',(-5.24884804582746,4.84409946429349,-5.22464897735641));
#93779=CARTESIAN_POINT('',(-5.45533889445123,5.00000000010406,-4.77512068459171));
#93780=CARTESIAN_POINT('Ctrl Pts',(-5.45533889410359,5.00000000017678,-4.77512068412071));
#93781=CARTESIAN_POINT('Ctrl Pts',(-5.49154573973822,4.99124724267219,-4.74704534735226));
#93782=CARTESIAN_POINT('Ctrl Pts',(-5.52746798253027,4.98253936613918,-4.71859168193082));
#93783=CARTESIAN_POINT('Ctrl Pts',(-5.59897952991459,4.96515484938229,-4.66073502606677));
#93784=CARTESIAN_POINT('Ctrl Pts',(-5.63502861628044,4.95636631359973,-4.63092455917339));
#93785=CARTESIAN_POINT('Ctrl Pts',(-5.66914323546902,4.9479731746332,-4.60221802331358));
#93786=CARTESIAN_POINT('',(-5.69577999258466,4.95523000036888,-4.55760459272089));
#93787=CARTESIAN_POINT('Ctrl Pts',(-5.69577999258466,4.95523000036888,-4.55760459272089));
#93788=CARTESIAN_POINT('Ctrl Pts',(-5.65688928340724,4.9626028560638,-4.59440674027076));
#93789=CARTESIAN_POINT('Ctrl Pts',(-5.6171117243295,4.97005835676343,-4.63125323347676));
#93790=CARTESIAN_POINT('Ctrl Pts',(-5.53671427677798,4.98502388766089,-4.70399171001648));
#93791=CARTESIAN_POINT('Ctrl Pts',(-5.49622793408486,4.99250278380615,-4.73978990137419));
#93792=CARTESIAN_POINT('Ctrl Pts',(-5.45533889440155,4.99999999998404,-4.77512068407294));
#93793=CARTESIAN_POINT('',(-5.85233559273308,5.00000000113546,-4.27933033396379));
#93794=CARTESIAN_POINT('Origin',(0.625220748686339,5.12365841984548,-0.841763906061353));
#93795=CARTESIAN_POINT('',(-5.73391953761776,4.94797317377359,-4.52125673988802));
#93796=CARTESIAN_POINT('Origin',(0.58090261596229,5.49705193280982,-1.39287448079707));
#93797=CARTESIAN_POINT('',(-6.24927798597133,4.84409946433865,-3.97415241254827));
#93798=CARTESIAN_POINT('Ctrl Pts',(-6.24927798597134,4.84409946433865,-3.97415241254827));
#93799=CARTESIAN_POINT('Ctrl Pts',(-6.16804032445152,4.86143878571084,-4.06958494783095));
#93800=CARTESIAN_POINT('Ctrl Pts',(-6.08442456118427,4.87877094699107,-4.16295606591001));
#93801=CARTESIAN_POINT('Ctrl Pts',(-5.95544747371417,4.90476414605477,-4.29988381808576));
#93802=CARTESIAN_POINT('Ctrl Pts',(-5.911828892812,4.91343410631592,-4.3450367474367));
#93803=CARTESIAN_POINT('Ctrl Pts',(-5.84561356381545,4.92641824543168,-4.41187182634179));
#93804=CARTESIAN_POINT('Ctrl Pts',(-5.82344219345241,4.93073677836905,-4.43397072821995));
#93805=CARTESIAN_POINT('Ctrl Pts',(-5.77905827644861,4.93932462810677,-4.47765573410487));
#93806=CARTESIAN_POINT('Ctrl Pts',(-5.75752222447624,4.94346583895174,-4.498603032325));
#93807=CARTESIAN_POINT('Ctrl Pts',(-5.73391953723181,4.9479731743308,-4.52125673937504));
#93808=CARTESIAN_POINT('',(-6.52594265175988,4.94797317388831,-3.27592250727311));
#93809=CARTESIAN_POINT('Ctrl Pts',(-6.52594265231059,4.94797317344726,-3.27592250739383));
#93810=CARTESIAN_POINT('Ctrl Pts',(-6.48593715840192,4.93049585002046,-3.39457410634552));
#93811=CARTESIAN_POINT('Ctrl Pts',(-6.44284148120856,4.91309421484135,-3.512173751874));
#93812=CARTESIAN_POINT('Ctrl Pts',(-6.35056898909567,4.87845834293924,-3.74503471273904));
#93813=CARTESIAN_POINT('Ctrl Pts',(-6.30141044225873,4.8612308920418,-3.8602504243896));
#93814=CARTESIAN_POINT('Ctrl Pts',(-6.24927798597133,4.84409946433865,-3.97415241254827));
#93815=CARTESIAN_POINT('',(-6.35430589758882,5.0000000002178,-3.49074441377445));
#93816=CARTESIAN_POINT('Ctrl Pts',(-6.35430589724851,5.00000000027394,-3.49074441347699));
#93817=CARTESIAN_POINT('Ctrl Pts',(-6.38363087081989,4.99124724542744,-3.45554207113647));
#93818=CARTESIAN_POINT('Ctrl Pts',(-6.41259657898731,4.9825393675923,-3.42003141116201));
#93819=CARTESIAN_POINT('Ctrl Pts',(-6.4699987557459,4.96515485077748,-3.34815454233767));
#93820=CARTESIAN_POINT('Ctrl Pts',(-6.49879666789651,4.95636631412613,-3.31129153669143));
#93821=CARTESIAN_POINT('Ctrl Pts',(-6.52594265111574,4.94797317489863,-3.27592250653897));
#93822=CARTESIAN_POINT('',(-6.54236608731522,4.9552300002817,-3.22662599759221));
#93823=CARTESIAN_POINT('Ctrl Pts',(-6.54236608731522,4.9552300002817,-3.22662599759221));
#93824=CARTESIAN_POINT('Ctrl Pts',(-6.5122959954036,4.96260285591192,-3.27092808392267));
#93825=CARTESIAN_POINT('Ctrl Pts',(-6.48136931901497,4.9700583569918,-3.31546412787944));
#93826=CARTESIAN_POINT('Ctrl Pts',(-6.41848813764831,4.98502388877246,-3.40378509928733));
#93827=CARTESIAN_POINT('Ctrl Pts',(-6.38664389809692,4.99250278441687,-3.44744971279347));
#93828=CARTESIAN_POINT('Ctrl Pts',(-6.35430589746526,5.00000000012513,-3.49074441339151));
#93829=CARTESIAN_POINT('',(-6.63544076432503,5.00000000130698,-2.92120280906809));
#93830=CARTESIAN_POINT('Origin',(0.429648035935632,5.12365808305802,-0.956488199897906));
#93831=CARTESIAN_POINT('',(-6.5718002370655,4.94797317371172,-3.1829290620009));
#93832=CARTESIAN_POINT('Origin',(0.267892146939279,5.49705138256567,-1.48518724332511));
#93833=CARTESIAN_POINT('',(-6.9574986329725,4.84409946433526,-2.5378288981618));
#93834=CARTESIAN_POINT('Ctrl Pts',(-6.95749863297251,4.84409946433526,-2.5378288981618));
#93835=CARTESIAN_POINT('Ctrl Pts',(-6.89867543702368,4.86143878567583,-2.64849396955423));
#93836=CARTESIAN_POINT('Ctrl Pts',(-6.83708659426749,4.87877094692769,-2.75765704010306));
#93837=CARTESIAN_POINT('Ctrl Pts',(-6.74056033871976,4.90476414595529,-2.91910975859602));
#93838=CARTESIAN_POINT('Ctrl Pts',(-6.70766808115882,4.91343410620189,-2.97258374299614));
#93839=CARTESIAN_POINT('Ctrl Pts',(-6.65736839616571,4.92641824530265,-3.05209059320888));
#93840=CARTESIAN_POINT('Ctrl Pts',(-6.64046599080045,4.93073677823803,-3.07843902426737));
#93841=CARTESIAN_POINT('Ctrl Pts',(-6.60651073008813,4.93932462797207,-3.13064392912216));
#93842=CARTESIAN_POINT('Ctrl Pts',(-6.58998122902561,4.94346583880374,-3.15573110563001));
#93843=CARTESIAN_POINT('Ctrl Pts',(-6.57180023681244,4.94797317419977,-3.18292906175086));
#93844=CARTESIAN_POINT('',(-7.0775962428047,4.94797317380733,-1.79644849492893));
#93845=CARTESIAN_POINT('Ctrl Pts',(-7.0775962432299,4.94797317335439,-1.79644849491167));
#93846=CARTESIAN_POINT('Ctrl Pts',(-7.06403264194361,4.93049584991313,-1.92092608431536));
#93847=CARTESIAN_POINT('Ctrl Pts',(-7.04722496533824,4.91309421480762,-2.04504061177499));
#93848=CARTESIAN_POINT('Ctrl Pts',(-7.0071679759942,4.8784583429011,-2.29229327130114));
#93849=CARTESIAN_POINT('Ctrl Pts',(-6.98392670089476,4.86123089201992,-2.4153829381001));
#93850=CARTESIAN_POINT('Ctrl Pts',(-6.95749863297251,4.84409946433526,-2.5378288981618));
#93851=CARTESIAN_POINT('',(-6.95615261953385,5.0000000003909,-2.0431448139407));
#93852=CARTESIAN_POINT('Ctrl Pts',(-6.95615261934601,5.00000000041751,-2.04314481383768));
#93853=CARTESIAN_POINT('Ctrl Pts',(-6.97722451588073,4.99124725073596,-2.00246150420444));
#93854=CARTESIAN_POINT('Ctrl Pts',(-6.9978792864587,4.98253937018195,-1.9615542801404));
#93855=CARTESIAN_POINT('Ctrl Pts',(-7.03848803841168,4.96515484981917,-1.8790180643763));
#93856=CARTESIAN_POINT('Ctrl Pts',(-7.05868821461483,4.95636631330385,-1.8368261953792));
#93857=CARTESIAN_POINT('Ctrl Pts',(-7.07759624194427,4.94797317474325,-1.79644849433146));
#93858=CARTESIAN_POINT('',(-7.08303841496067,4.95523000028387,-1.74477395697836));
#93859=CARTESIAN_POINT('Ctrl Pts',(-7.08303841496068,4.95523000028387,-1.74477395697837));
#93860=CARTESIAN_POINT('Ctrl Pts',(-7.06319378849081,4.96260330013697,-1.79450746240022));
#93861=CARTESIAN_POINT('Ctrl Pts',(-7.04256660110086,4.97005789420884,-1.84464451794085));
#93862=CARTESIAN_POINT('Ctrl Pts',(-7.00014062676657,4.98502389099315,-1.94442128925669));
#93863=CARTESIAN_POINT('Ctrl Pts',(-6.97842749173757,4.99250278562616,-1.99391061172942));
#93864=CARTESIAN_POINT('Ctrl Pts',(-6.95615261941778,5.00000000035927,-2.0431448138));
#93865=CARTESIAN_POINT('',(-7.10828010096112,5.00000000118293,-1.4264830892052));
#93866=CARTESIAN_POINT('Origin',(0.213987963839789,5.12365837061161,-1.02648756263497));
#93867=CARTESIAN_POINT('',(-7.10239086153082,4.94797317376557,-1.69577115923219));
#93868=CARTESIAN_POINT('Origin',(-0.0576388480719026,5.4970519466876,-1.50805329764877));
#93869=CARTESIAN_POINT('',(-7.34039437668646,4.84409946433426,-0.982839325059756));
#93870=CARTESIAN_POINT('Ctrl Pts',(-7.34039437668647,4.84409946433426,-0.982839325059758));
#93871=CARTESIAN_POINT('Ctrl Pts',(-7.30673615347733,4.86143878567784,-1.10356235691438));
#93872=CARTESIAN_POINT('Ctrl Pts',(-7.27005405695223,4.87877094694078,-1.22341303619949));
#93873=CARTESIAN_POINT('Ctrl Pts',(-7.21049209354376,4.90476414599402,-1.40184137156618));
#93874=CARTESIAN_POINT('Ctrl Pts',(-7.1898641646212,4.91343410625637,-1.46113602707844));
#93875=CARTESIAN_POINT('Ctrl Pts',(-7.15783208086489,4.92641824537678,-1.54959699679477));
#93876=CARTESIAN_POINT('Ctrl Pts',(-7.14698897816429,4.93073677831544,-1.57896293369232));
#93877=CARTESIAN_POINT('Ctrl Pts',(-7.12505118531909,4.93932419693192,-1.63724376826478));
#93878=CARTESIAN_POINT('Ctrl Pts',(-7.11429863727107,4.94346636782592,-1.665304276277));
#93879=CARTESIAN_POINT('Ctrl Pts',(-7.10239086091004,4.94797317420863,-1.69577115892403));
#93880=CARTESIAN_POINT('',(-7.29830929924953,4.94797317385515,-0.232974546960617));
#93881=CARTESIAN_POINT('Ctrl Pts',(-7.29830929980229,4.9479731734908,-0.232974546849461));
#93882=CARTESIAN_POINT('Ctrl Pts',(-7.31182181016524,4.93049585006795,-0.357457692479486));
#93883=CARTESIAN_POINT('Ctrl Pts',(-7.32208804239158,4.9130942148399,-0.48228364561484));
#93884=CARTESIAN_POINT('Ctrl Pts',(-7.3361195762891,4.87845834292249,-0.73236674389168));
#93885=CARTESIAN_POINT('Ctrl Pts',(-7.3398823091514,4.86123089202013,-0.857574829957159));
#93886=CARTESIAN_POINT('Ctrl Pts',(-7.34039437668647,4.84409946433426,-0.982839325059756));
#93887=CARTESIAN_POINT('',(-7.23273737682457,5.00000000045635,-0.500010033007036));
#93888=CARTESIAN_POINT('Ctrl Pts',(-7.23273737668175,5.00000000047483,-0.5000100329652));
#93889=CARTESIAN_POINT('Ctrl Pts',(-7.24457091367181,4.99124725176391,-0.455748046850563));
#93890=CARTESIAN_POINT('Ctrl Pts',(-7.25594894401456,4.98253937067083,-0.411357042952466));
#93891=CARTESIAN_POINT('Ctrl Pts',(-7.27786544000373,4.96515484972087,-0.322020793969775));
#93892=CARTESIAN_POINT('Ctrl Pts',(-7.2885233424811,4.95636631334907,-0.276472907790325));
#93893=CARTESIAN_POINT('Ctrl Pts',(-7.2983092985434,4.94797317475611,-0.232974546627913));
#93894=CARTESIAN_POINT('',(-7.29251573846638,4.95523000034311,-0.18133822573945));
#93895=CARTESIAN_POINT('Ctrl Pts',(-7.29251573846639,4.95523000034311,-0.181338225739452));
#93896=CARTESIAN_POINT('Ctrl Pts',(-7.28382682480052,4.96260285648447,-0.23417181792712));
#93897=CARTESIAN_POINT('Ctrl Pts',(-7.27445873376066,4.97005835691444,-0.287577406606114));
#93898=CARTESIAN_POINT('Ctrl Pts',(-7.25447432879073,4.98502389150509,-0.394138491448891));
#93899=CARTESIAN_POINT('Ctrl Pts',(-7.24390757645083,4.99250278595753,-0.447138461622359));
#93900=CARTESIAN_POINT('Ctrl Pts',(-7.23273737672512,5.00000000043411,-0.500010032928329));
#93901=CARTESIAN_POINT('',(-7.24874416011981,5.00000000111792,0.13493739489825));
#93902=CARTESIAN_POINT('Origin',(-0.0116793057854747,5.12365838142277,-1.04848995574475));
#93903=CARTESIAN_POINT('',(-7.30088158231934,4.94797317377374,-0.129320882509947));
#93904=CARTESIAN_POINT('Origin',(-0.380478934841684,5.49705192399641,-1.4604050333425));
#93905=CARTESIAN_POINT('',(-7.38006143768145,4.84409946429152,0.618106722867779));
#93906=CARTESIAN_POINT('Ctrl Pts',(-7.38006143768146,4.84409946429152,0.618106722867779));
#93907=CARTESIAN_POINT('Ctrl Pts',(-7.37314200830705,4.86143878566475,0.492970605287479));
#93908=CARTESIAN_POINT('Ctrl Pts',(-7.36308187208114,4.87877094695141,0.36803640178613));
#93909=CARTESIAN_POINT('Ctrl Pts',(-7.34326925205903,4.90476414602571,0.180975560198201));
#93910=CARTESIAN_POINT('Ctrl Pts',(-7.33587019084798,4.91343410628931,0.118632785831322));
#93911=CARTESIAN_POINT('Ctrl Pts',(-7.32360349300845,4.92641824541276,0.0253540332676023));
#93912=CARTESIAN_POINT('Ctrl Pts',(-7.31932670440219,4.93073677835475,-0.00565629093040938));
#93913=CARTESIAN_POINT('Ctrl Pts',(-7.31043001499084,4.93932462810217,-0.0672936233185138));
#93914=CARTESIAN_POINT('Ctrl Pts',(-7.30596207811234,4.94346583894984,-0.0970026855058121));
#93915=CARTESIAN_POINT('Ctrl Pts',(-7.30088158184065,4.94797317433898,-0.129320882355863));
#93916=CARTESIAN_POINT('',(-7.17776152475488,4.94797317380236,1.34139303118644));
#93917=CARTESIAN_POINT('Ctrl Pts',(-7.17776152514807,4.94797317339019,1.34139303137954));
#93918=CARTESIAN_POINT('Ctrl Pts',(-7.21771831716903,4.93049584997349,1.2227250226255));
#93919=CARTESIAN_POINT('Ctrl Pts',(-7.25457842050998,4.9130942148394,1.10302436785673));
#93920=CARTESIAN_POINT('Ctrl Pts',(-7.32204237868749,4.87845834291323,0.861804438367264));
#93921=CARTESIAN_POINT('Ctrl Pts',(-7.35263317832365,4.86123089200476,0.740332524198434));
#93922=CARTESIAN_POINT('Ctrl Pts',(-7.38006143768146,4.84409946429152,0.618106722867782));
#93923=CARTESIAN_POINT('',(-7.17112737312078,5.00000000051076,1.06650466102044));
#93924=CARTESIAN_POINT('Ctrl Pts',(-7.17112737304764,5.00000000051987,1.06650466102544));
#93925=CARTESIAN_POINT('Ctrl Pts',(-7.17316922946218,4.99124725346394,1.11227567873281));
#93926=CARTESIAN_POINT('Ctrl Pts',(-7.17473849443647,4.98253937156206,1.15807478980744));
#93927=CARTESIAN_POINT('Ctrl Pts',(-7.17693794222823,4.96515485006557,1.25003380867691));
#93928=CARTESIAN_POINT('Ctrl Pts',(-7.17755521977201,4.95636631307048,1.29680794788393));
#93929=CARTESIAN_POINT('Ctrl Pts',(-7.17776152382245,4.94797317469699,1.34139303135917));
#93930=CARTESIAN_POINT('',(-7.16100313117102,4.95523000029981,1.39057668033257));
#93931=CARTESIAN_POINT('Ctrl Pts',(-7.16100313117103,4.95523000029981,1.39057668033257));
#93932=CARTESIAN_POINT('Ctrl Pts',(-7.16387519267682,4.96260329941632,1.33710723583422));
#93933=CARTESIAN_POINT('Ctrl Pts',(-7.16620646791303,4.97005789390706,1.2829429419715));
#93934=CARTESIAN_POINT('Ctrl Pts',(-7.16959687559227,4.98502389213623,1.17457378243522));
#93935=CARTESIAN_POINT('Ctrl Pts',(-7.17067059482315,4.99250278630537,1.12054138490138));
#93936=CARTESIAN_POINT('Ctrl Pts',(-7.1711273730592,5.00000000050815,1.06650466102737));
#93937=CARTESIAN_POINT('',(-7.05026499821003,5.00000000126723,1.69004835712118));
#93938=CARTESIAN_POINT('Origin',(-0.236800892431308,5.12365819333402,-1.02146601117213));
#93939=CARTESIAN_POINT('',(-7.15799119542332,4.94797317376926,1.44317629552494));
#93940=CARTESIAN_POINT('Origin',(-0.685527333282975,5.49705211802892,-1.34446996642009));
#93941=CARTESIAN_POINT('',(-7.0746450282201,4.8440994643031,2.19015078689032));
#93942=CARTESIAN_POINT('Ctrl Pts',(-7.07464502822011,4.8440994643031,2.19015078689033));
#93943=CARTESIAN_POINT('Ctrl Pts',(-7.09478793753128,4.86143878566637,2.06645280946945));
#93944=CARTESIAN_POINT('Ctrl Pts',(-7.11182016240746,4.87877094695015,1.94227686635824));
#93945=CARTESIAN_POINT('Ctrl Pts',(-7.13268330187995,4.90476414602651,1.75533027567424));
#93946=CARTESIAN_POINT('Ctrl Pts',(-7.13885908025635,4.91343410629485,1.69285446126028));
#93947=CARTESIAN_POINT('Ctrl Pts',(-7.14693134549244,4.92641824541834,1.59911953666473));
#93948=CARTESIAN_POINT('Ctrl Pts',(-7.1494208488683,4.93073677835663,1.56791483350988));
#93949=CARTESIAN_POINT('Ctrl Pts',(-7.15398236358274,4.93932462809247,1.50580602253555));
#93950=CARTESIAN_POINT('Ctrl Pts',(-7.15600545475998,4.94346583893296,1.47583106739905));
#93951=CARTESIAN_POINT('Ctrl Pts',(-7.15799119467072,4.94797317431431,1.4431762955544));
#93952=CARTESIAN_POINT('',(-6.72158959858316,4.94797317388402,2.85303856204128));
#93953=CARTESIAN_POINT('Ctrl Pts',(-6.72158959902029,4.94797317342077,2.85303856237963));
#93954=CARTESIAN_POINT('Ctrl Pts',(-6.78612233751133,4.93049585000813,2.7457344749205));
#93955=CARTESIAN_POINT('Ctrl Pts',(-6.84785277466984,4.91309421482941,2.63675618743939));
#93956=CARTESIAN_POINT('Ctrl Pts',(-6.96559461743177,4.87845834288678,2.41567860264718));
#93957=CARTESIAN_POINT('Ctrl Pts',(-7.02158309203489,4.86123089197945,2.30362275197257));
#93958=CARTESIAN_POINT('Ctrl Pts',(-7.07464502822011,4.8440994643031,2.19015078689033));
#93959=CARTESIAN_POINT('',(-6.77420342353812,5.00000000021333,2.58315078520084));
#93960=CARTESIAN_POINT('Ctrl Pts',(-6.7742034230859,5.00000000027013,2.58315078513325));
#93961=CARTESIAN_POINT('Ctrl Pts',(-6.7663581191946,4.99124724528312,2.62829068126326));
#93962=CARTESIAN_POINT('Ctrl Pts',(-6.75804524388186,4.98253936748107,2.67335635884948));
#93963=CARTESIAN_POINT('Ctrl Pts',(-6.74042480375319,4.96515485062198,2.76363821908636));
#93964=CARTESIAN_POINT('Ctrl Pts',(-6.73097259275404,4.95636631384195,2.80945150006911));
#93965=CARTESIAN_POINT('Ctrl Pts',(-6.72158959756006,4.94797317490626,2.85303856201789));
#93966=CARTESIAN_POINT('',(-6.69464997632219,4.95523000034612,2.89746976556783));
#93967=CARTESIAN_POINT('Ctrl Pts',(-6.6946499763222,4.95523000034612,2.89746976556783));
#93968=CARTESIAN_POINT('Ctrl Pts',(-6.70894923932624,4.96260329885002,2.84586781988646));
#93969=CARTESIAN_POINT('Ctrl Pts',(-6.72286973387921,4.97005789392374,2.79347100827728));
#93970=CARTESIAN_POINT('Ctrl Pts',(-6.74947703568066,4.98502388866908,2.68836432083602));
#93971=CARTESIAN_POINT('Ctrl Pts',(-6.76214102330062,4.99250278434603,2.6358259778232));
#93972=CARTESIAN_POINT('Ctrl Pts',(-6.77420342316194,5.00000000011959,2.58315078535635));
#93973=CARTESIAN_POINT('',(-6.52212328112776,5.00000000126512,3.16613453534081));
#93974=CARTESIAN_POINT('Origin',(-0.450850659841332,5.12365813414324,-0.946678847083811));
#93975=CARTESIAN_POINT('',(-6.68040109545753,4.94797317379139,2.94819215415093));
#93976=CARTESIAN_POINT('Origin',(-0.958523019359824,5.49705207103514,-1.16566772092202));
#93977=CARTESIAN_POINT('',(-6.43842608023093,4.84409946433625,3.65978583438252));
#93978=CARTESIAN_POINT('Ctrl Pts',(-6.43842608023094,4.84409946433625,3.65978583438252));
#93979=CARTESIAN_POINT('Ctrl Pts',(-6.48468946811766,4.86143878571813,3.54330997707003));
#93980=CARTESIAN_POINT('Ctrl Pts',(-6.52801764617062,4.87877094699052,3.42569862344729));
#93981=CARTESIAN_POINT('Ctrl Pts',(-6.58858100787816,4.90476414604654,3.2476076985895));
#93982=CARTESIAN_POINT('Ctrl Pts',(-6.608042853287,4.91343410630369,3.18792014387897));
#93983=CARTESIAN_POINT('Ctrl Pts',(-6.63607663141585,4.92641824542267,3.09811198823373));
#93984=CARTESIAN_POINT('Ctrl Pts',(-6.6452160203545,4.93073677836402,3.06817200334143));
#93985=CARTESIAN_POINT('Ctrl Pts',(-6.66302244782254,4.93932462811458,3.00849585265603));
#93986=CARTESIAN_POINT('Ctrl Pts',(-6.67144196955517,4.94346583896624,2.97965660008473));
#93987=CARTESIAN_POINT('Ctrl Pts',(-6.68040109464971,4.94797317436312,2.94819215400281));
#93988=CARTESIAN_POINT('',(-5.9511236137351,4.94797317388934,4.23127918051304));
#93989=CARTESIAN_POINT('Ctrl Pts',(-5.95112361406283,4.94797317337418,4.23127918092237));
#93990=CARTESIAN_POINT('Ctrl Pts',(-6.03721481998975,4.93049584990762,4.14035643456259));
#93991=CARTESIAN_POINT('Ctrl Pts',(-6.12092914409712,4.91309421476481,4.04719621830559));
#93992=CARTESIAN_POINT('Ctrl Pts',(-6.28344339371998,4.87845834285195,3.85659832029483));
#93993=CARTESIAN_POINT('Ctrl Pts',(-6.36221158439183,4.86123089198366,3.75919814017742));
#93994=CARTESIAN_POINT('Ctrl Pts',(-6.43842608023093,4.84409946433625,3.65978583438252));
#93995=CARTESIAN_POINT('',(-6.06052525045423,5.00000000006602,3.97901164806513));
#93996=CARTESIAN_POINT('Ctrl Pts',(-6.06052524986571,5.00000000014428,3.97901164784023));
#93997=CARTESIAN_POINT('Ctrl Pts',(-6.04315961497363,4.99124724184196,4.02140970579152));
#93998=CARTESIAN_POINT('Ctrl Pts',(-6.02535330478515,4.98253936579715,4.0636347419452));
#93999=CARTESIAN_POINT('Ctrl Pts',(-5.98873689183328,4.96515484996222,4.1480179834896));
#94000=CARTESIAN_POINT('Ctrl Pts',(-5.96965716811944,4.95636631373681,4.19072822695835));
#94001=CARTESIAN_POINT('Ctrl Pts',(-5.95112361260635,4.94797317496797,4.2312791802204));
#94002=CARTESIAN_POINT('',(-5.9152624289547,4.95523000032746,4.26888038538439));
#94003=CARTESIAN_POINT('Ctrl Pts',(-5.9152624289547,4.95523000032746,4.26888038538439));
#94004=CARTESIAN_POINT('Ctrl Pts',(-5.94031885595169,4.96260288086368,4.22156146549675));
#94005=CARTESIAN_POINT('Ctrl Pts',(-5.96518060385663,4.9700583625512,4.17337643669248));
#94006=CARTESIAN_POINT('Ctrl Pts',(-6.01375908058615,4.98502386688622,4.07645004498659));
#94007=CARTESIAN_POINT('Ctrl Pts',(-6.03742121981557,4.99250277347481,4.02786233440585));
#94008=CARTESIAN_POINT('Ctrl Pts',(-6.06052525004563,4.99999999998347,3.97901164785921));
#94009=CARTESIAN_POINT('',(-5.68901432884376,5.00000000114322,4.49417578249345));
#94010=CARTESIAN_POINT('Origin',(-0.643817031139517,5.12365825596667,-0.827627422281949));
#94011=CARTESIAN_POINT('',(-5.89044286473166,4.94797317375056,4.31535382449974));
#94012=CARTESIAN_POINT('Origin',(-1.18669562488869,5.49705179923779,-0.932362816200588));
#94013=CARTESIAN_POINT('',(-5.50115348427103,4.8440994643342,4.9582933643208));
#94014=CARTESIAN_POINT('Ctrl Pts',(-5.50115348427104,4.8440994643342,4.95829336432081));
#94015=CARTESIAN_POINT('Ctrl Pts',(-5.57137412622155,4.86143878566795,4.85448590871698));
#94016=CARTESIAN_POINT('Ctrl Pts',(-5.63897228002819,4.8787709469205,4.74893852071259));
#94017=CARTESIAN_POINT('Ctrl Pts',(-5.73640398850807,4.9047641459615,4.58803059527565));
#94018=CARTESIAN_POINT('Ctrl Pts',(-5.76824188668813,4.91343410621467,4.53392222392337));
#94019=CARTESIAN_POINT('Ctrl Pts',(-5.81492634941089,4.92641824533118,4.45224016669456));
#94020=CARTESIAN_POINT('Ctrl Pts',(-5.83028827625063,4.93073677827342,4.42496486047126));
#94021=CARTESIAN_POINT('Ctrl Pts',(-5.86050700772111,4.93932462802316,4.3705117605863));
#94022=CARTESIAN_POINT('Ctrl Pts',(-5.87492927249967,4.94346583886421,4.3441567020763));
#94023=CARTESIAN_POINT('Ctrl Pts',(-5.89044286410019,4.94797317427384,4.31535382424151));
#94024=CARTESIAN_POINT('',(-4.90238970219432,4.94797317377648,5.41166988820258));
#94025=CARTESIAN_POINT('Ctrl Pts',(-4.90238970237242,4.94797317337695,5.41166988856449));
#94026=CARTESIAN_POINT('Ctrl Pts',(-5.00601384658402,4.93049584992143,5.34137992990052));
#94027=CARTESIAN_POINT('Ctrl Pts',(-5.10779766906465,4.91309421477567,5.2683938528048));
#94028=CARTESIAN_POINT('Ctrl Pts',(-5.30748533998087,4.87845834285546,5.11718778745134));
#94029=CARTESIAN_POINT('Ctrl Pts',(-5.405357821173,4.86122953170664,5.03899135032968));
#94030=CARTESIAN_POINT('Ctrl Pts',(-5.50116106175314,4.84409810933837,4.95828698108094));
#94031=CARTESIAN_POINT('',(-5.06346365273142,5.00000000024774,5.18881834708339));
#94032=CARTESIAN_POINT('Ctrl Pts',(-5.0634636523831,5.00000000029952,5.18881834685435));
#94033=CARTESIAN_POINT('Ctrl Pts',(-5.03738969924476,4.99124724607008,5.22649204615994));
#94034=CARTESIAN_POINT('Ctrl Pts',(-5.01092254989299,4.98253936790085,5.26390206337639));
#94035=CARTESIAN_POINT('Ctrl Pts',(-4.95702230137582,4.96515485070685,5.33844103118426));
#94036=CARTESIAN_POINT('Ctrl Pts',(-4.92920721075983,4.95636631423499,5.37605115707747));
#94037=CARTESIAN_POINT('Ctrl Pts',(-4.90238970136707,4.94797317463228,5.4116698877814));
#94038=CARTESIAN_POINT('',(-4.8592837852266,4.95523000036476,5.44068290219272));
#94039=CARTESIAN_POINT('Ctrl Pts',(-4.8592837852266,4.95523000036476,5.44068290219272));
#94040=CARTESIAN_POINT('Ctrl Pts',(-4.89392864298546,4.9626033208512,5.39985422744277));
#94041=CARTESIAN_POINT('Ctrl Pts',(-4.92856333329916,4.97005790377228,5.3581452969328));
#94042=CARTESIAN_POINT('Ctrl Pts',(-4.99684448344413,4.98502386886887,5.273925334085));
#94043=CARTESIAN_POINT('Ctrl Pts',(-5.03039833218755,4.9925027745633,5.23156024274039));
#94044=CARTESIAN_POINT('Ctrl Pts',(-5.06346365249666,5.00000000019312,5.1888183468922));
#94045=CARTESIAN_POINT('',(-4.58989338860951,5.00000000112623,5.61207436548009));
#94046=CARTESIAN_POINT('Origin',(-0.806680192645151,5.12365860650201,-0.669876686411711));
#94047=CARTESIAN_POINT('',(-4.82505407222897,4.94797317374014,5.48073434620426));
#94048=CARTESIAN_POINT('Origin',(-1.35938120842026,5.49705179230414,-0.655461214805863));
#94049=CARTESIAN_POINT('',(-4.30665306526583,4.84409946429903,6.0249566073236));
#94050=CARTESIAN_POINT('Ctrl Pts',(-4.30665306526583,4.84409946429903,6.02495660732361));
#94051=CARTESIAN_POINT('Ctrl Pts',(-4.39754752209537,4.86143878565606,5.93867147461155));
#94052=CARTESIAN_POINT('Ctrl Pts',(-4.48625483714493,4.87877094691826,5.85012333072359));
#94053=CARTESIAN_POINT('Ctrl Pts',(-4.61599909412046,4.90476414596476,5.71392228032555));
#94054=CARTESIAN_POINT('Ctrl Pts',(-4.65872434042047,4.91343410622358,5.66792313954466));
#94055=CARTESIAN_POINT('Ctrl Pts',(-4.72187657422963,4.92641824533791,5.59818654285872));
#94056=CARTESIAN_POINT('Ctrl Pts',(-4.74274273234744,4.9307367782742,5.57485127831631));
#94057=CARTESIAN_POINT('Ctrl Pts',(-4.78395870432753,4.93932419688864,5.52816973925923));
#94058=CARTESIAN_POINT('Ctrl Pts',(-4.80371391686449,4.94346636778017,5.50552595475308));
#94059=CARTESIAN_POINT('Ctrl Pts',(-4.82505407173893,4.94797317417246,5.48073434586103));
#94060=CARTESIAN_POINT('',(-3.62442549739344,4.94797317379252,6.3390169257249));
#94061=CARTESIAN_POINT('Ctrl Pts',(-3.62442549749584,4.94797317337247,6.33901692614006));
#94062=CARTESIAN_POINT('Ctrl Pts',(-3.74073723005479,4.93049584992828,6.29264643558571));
#94063=CARTESIAN_POINT('Ctrl Pts',(-3.85583125231974,4.91309421478534,6.24324724561167));
#94064=CARTESIAN_POINT('Ctrl Pts',(-4.08335517068789,4.87845834284928,6.1385032407116));
#94065=CARTESIAN_POINT('Ctrl Pts',(-4.19574051848432,4.86123089196007,6.0831791362385));
#94066=CARTESIAN_POINT('Ctrl Pts',(-4.30665306526583,4.84409946429903,6.02495660732361));
#94067=CARTESIAN_POINT('',(-3.82964012287192,5.00000000030332,6.15600166741685));
#94068=CARTESIAN_POINT('Ctrl Pts',(-3.82964012262647,5.00000000034701,6.15600166716498));
#94069=CARTESIAN_POINT('Ctrl Pts',(-3.79607703682092,4.99124724741758,6.18718944279529));
#94070=CARTESIAN_POINT('Ctrl Pts',(-3.76218662411001,4.98253936856204,6.21803518242874));
#94071=CARTESIAN_POINT('Ctrl Pts',(-3.6935228484439,4.96515484867379,6.27924451971109));
#94072=CARTESIAN_POINT('Ctrl Pts',(-3.65827299131585,4.95636631176606,6.30999592123176));
#94073=CARTESIAN_POINT('Ctrl Pts',(-3.62442549665219,4.94797317467946,6.33901692511689));
#94074=CARTESIAN_POINT('',(-3.57609043208675,4.9552300004188,6.35808513377476));
#94075=CARTESIAN_POINT('Ctrl Pts',(-3.57609043208675,4.9552300004188,6.35808513377476));
#94076=CARTESIAN_POINT('Ctrl Pts',(-3.61869958609048,4.9626028564312,6.32566067382102));
#94077=CARTESIAN_POINT('Ctrl Pts',(-3.66149597485689,4.97005835696801,6.29236822343175));
#94078=CARTESIAN_POINT('Ctrl Pts',(-3.74628310255969,4.98502388963094,6.22479765766597));
#94079=CARTESIAN_POINT('Ctrl Pts',(-3.7881596635725,4.9925027848899,6.19063616758905));
#94080=CARTESIAN_POINT('Ctrl Pts',(-3.82964012256919,5.00000000023122,6.15600166733698));
#94081=CARTESIAN_POINT('',(-3.27615413515278,5.00000000120582,6.46755858726378));
#94082=CARTESIAN_POINT('Origin',(-0.931824247626192,5.12365838328379,-0.480802586718734));
#94083=CARTESIAN_POINT('',(-3.53405111422536,4.94797317377853,6.3898418209816));
#94084=CARTESIAN_POINT('Origin',(-1.46850476501289,5.49705202712533,-0.347909162332483));
#94085=CARTESIAN_POINT('',(-2.91077833579864,4.84409946434516,6.80989957516688));
#94086=CARTESIAN_POINT('Ctrl Pts',(-2.91077833579864,4.84409946434516,6.80989957516688));
#94087=CARTESIAN_POINT('Ctrl Pts',(-3.01809648368299,4.8614387857069,6.74517136230629));
#94088=CARTESIAN_POINT('Ctrl Pts',(-3.12376510445404,4.87877094697295,6.6777628753848));
#94089=CARTESIAN_POINT('Ctrl Pts',(-3.27975521253511,4.90476414602561,6.5726373098989));
#94090=CARTESIAN_POINT('Ctrl Pts',(-3.33137002185206,4.91343410628631,6.53689826847531));
#94091=CARTESIAN_POINT('Ctrl Pts',(-3.40803709840257,4.92641824540357,6.48236793817296));
#94092=CARTESIAN_POINT('Ctrl Pts',(-3.43343180942504,4.93073677834079,6.46406384634563));
#94093=CARTESIAN_POINT('Ctrl Pts',(-3.48371932585261,4.93932419695326,6.42733391139021));
#94094=CARTESIAN_POINT('Ctrl Pts',(-3.5078804168098,4.94346636784446,6.4094663127248));
#94095=CARTESIAN_POINT('Ctrl Pts',(-3.53405111372333,4.9479731742255,6.38984182041476));
#94096=CARTESIAN_POINT('',(-2.17698718490753,4.94797317384646,6.96995857709649));
#94097=CARTESIAN_POINT('Ctrl Pts',(-2.1769871849229,4.94797317338406,6.96995857758856));
#94098=CARTESIAN_POINT('Ctrl Pts',(-2.30054789847439,4.93049584991362,6.94967578773418));
#94099=CARTESIAN_POINT('Ctrl Pts',(-2.42357045206225,4.91309421475659,6.92617333601248));
#94100=CARTESIAN_POINT('Ctrl Pts',(-2.66829185230895,4.87845834284315,6.87278910466344));
#94101=CARTESIAN_POINT('Ctrl Pts',(-2.78994274014277,4.8612308919762,6.84291797470086));
#94102=CARTESIAN_POINT('Ctrl Pts',(-2.91077833579864,4.84409946434516,6.80989957516688));
#94103=CARTESIAN_POINT('',(-2.41674687579388,5.00000000018585,6.83533719297713));
#94104=CARTESIAN_POINT('Ctrl Pts',(-2.41674687553562,5.00000000024666,6.83533719256134));
#94105=CARTESIAN_POINT('Ctrl Pts',(-2.37726401472209,4.99124724464907,6.85858075086912));
#94106=CARTESIAN_POINT('Ctrl Pts',(-2.33753502535484,4.98253936723008,6.8814198933422));
#94107=CARTESIAN_POINT('Ctrl Pts',(-2.25731838756175,4.96515485080288,6.92643749957918));
#94108=CARTESIAN_POINT('Ctrl Pts',(-2.21628201016599,4.95636631379398,6.94889227342396));
#94109=CARTESIAN_POINT('Ctrl Pts',(-2.17698718426122,4.94797317482836,6.96995857628212));
#94110=CARTESIAN_POINT('',(-2.12568306502001,4.95523000036473,6.97819037105365));
#94111=CARTESIAN_POINT('Ctrl Pts',(-2.12568306502001,4.95523000036473,6.97819037105365));
#94112=CARTESIAN_POINT('Ctrl Pts',(-2.17426925953366,4.96260329931481,6.95568233351109));
#94113=CARTESIAN_POINT('Ctrl Pts',(-2.22321605556432,4.97005789395287,6.9323710303661));
#94114=CARTESIAN_POINT('Ctrl Pts',(-2.32054958513549,4.98502388845175,6.88460547908258));
#94115=CARTESIAN_POINT('Ctrl Pts',(-2.3687908093894,4.9925027842392,6.86024488683704));
#94116=CARTESIAN_POINT('Ctrl Pts',(-2.4167468754063,5.0000000000855,6.83533719277799));
#94117=CARTESIAN_POINT('',(-1.80922555581647,5.00000000114933,7.02062695820467));
#94118=CARTESIAN_POINT('Origin',(-1.01339706190693,5.12365837744257,-0.269246995538954));
#94119=CARTESIAN_POINT('',(-2.07779985458226,4.94797317377022,7.0001673937011));
#94120=CARTESIAN_POINT('Origin',(-1.50896214363388,5.49705211430466,-0.024090086241163));
#94121=CARTESIAN_POINT('',(-1.37879884640616,4.84409946429526,7.27641920768044));
#94122=CARTESIAN_POINT('Ctrl Pts',(-1.37879884640616,4.84409946429526,7.27641920768044));
#94123=CARTESIAN_POINT('Ctrl Pts',(-1.49752260815187,4.86143878565642,7.23627453393968));
#94124=CARTESIAN_POINT('Ctrl Pts',(-1.61521158749359,4.87877094692771,7.1931576498776));
#94125=CARTESIAN_POINT('Ctrl Pts',(-1.79015362269918,4.90476414598114,7.12402312386852));
#94126=CARTESIAN_POINT('Ctrl Pts',(-1.84824454389819,4.9134341062347,7.10021529966484));
#94127=CARTESIAN_POINT('Ctrl Pts',(-1.93484159592898,4.92641824534835,7.0634410133741));
#94128=CARTESIAN_POINT('Ctrl Pts',(-1.96357743143852,4.93073677828957,7.0510239732327));
#94129=CARTESIAN_POINT('Ctrl Pts',(-2.02058510409539,4.93932419691696,7.02596309323285));
#94130=CARTESIAN_POINT('Ctrl Pts',(-2.04802232781495,4.94346636781934,7.01370714941363));
#94131=CARTESIAN_POINT('Ctrl Pts',(-2.07779985420982,4.9479731742092,7.00016739302812));
#94132=CARTESIAN_POINT('',(-0.627755369881773,4.94797317385797,7.27499271230061));
#94133=CARTESIAN_POINT('Ctrl Pts',(-0.627755369794896,4.94797317343625,
7.27499271281768));
#94134=CARTESIAN_POINT('Ctrl Pts',(-0.752787502800013,4.93049584999059,
7.28174602429238));
#94135=CARTESIAN_POINT('Ctrl Pts',(-0.877986190217805,4.91309421479666,
7.28523925933799));
#94136=CARTESIAN_POINT('Ctrl Pts',(-1.12846217199833,4.87845834286738,7.28571098880058));
#94137=CARTESIAN_POINT('Ctrl Pts',(-1.2536903397881,4.86123089197091,7.28268957417498));
#94138=CARTESIAN_POINT('Ctrl Pts',(-1.37879884640616,4.84409946429526,7.27641920768044));
#94139=CARTESIAN_POINT('',(-0.890849230764476,5.00000000015126,7.19505994779791));
#94140=CARTESIAN_POINT('Ctrl Pts',(-0.890849230588139,5.0000000002171,7.19505994729805));
#94141=CARTESIAN_POINT('Ctrl Pts',(-0.847292775126946,4.99124724379543,
7.20927243748423));
#94142=CARTESIAN_POINT('Ctrl Pts',(-0.803582888665312,4.98253936671115,
7.22303705456792));
#94143=CARTESIAN_POINT('Ctrl Pts',(-0.715564210890097,4.96515484899948,
7.24975797013115));
#94144=CARTESIAN_POINT('Ctrl Pts',(-0.670660129606432,4.95636631231393,
7.26286615515939));
#94145=CARTESIAN_POINT('Ctrl Pts',(-0.627755369455795,4.94797317481926,
7.2749927114588));
#94146=CARTESIAN_POINT('',(-0.575881119919221,4.95523000034009,7.27200318231908));
#94147=CARTESIAN_POINT('Ctrl Pts',(-0.575881119919222,4.95523000034009,
7.27200318231908));
#94148=CARTESIAN_POINT('Ctrl Pts',(-0.628166812764969,4.96260285567682,
7.2604666599647));
#94149=CARTESIAN_POINT('Ctrl Pts',(-0.680986903378122,4.97005835659053,
7.24822098699053));
#94150=CARTESIAN_POINT('Ctrl Pts',(-0.786309752028458,4.98502388806966,
7.2224967953507));
#94151=CARTESIAN_POINT('Ctrl Pts',(-0.838659931539472,4.99250278402759,
7.20907617718386));
#94152=CARTESIAN_POINT('Ctrl Pts',(-0.890849230400931,5.00000000004258,
7.19505994749707));
#94153=CARTESIAN_POINT('',(-0.257699599156794,5.00000000131521,7.24541861504245));
#94154=CARTESIAN_POINT('Origin',(-1.04758446035831,5.12365828658895,-0.0451006802085374));
#94155=CARTESIAN_POINT('',(-0.524392983891646,4.94797317434015,7.28317291923316));
#94156=CARTESIAN_POINT('Origin',(-1.47886142963726,5.4970517149711,0.300859522968813));
#94157=CARTESIAN_POINT('',(-2.18488949210674E-10,4.87444016471971,7.37555983528029));
#94158=CARTESIAN_POINT('Ctrl Pts',(-0.524392986567054,4.94797317482107,
7.28317291784782));
#94159=CARTESIAN_POINT('Ctrl Pts',(-0.492420047419541,4.94346905243022,
7.28999077156774));
#94160=CARTESIAN_POINT('Ctrl Pts',(-0.463017454517293,4.93933079581677,
7.29605638350877));
#94161=CARTESIAN_POINT('Ctrl Pts',(-0.40199585152166,4.93074907816145,7.30826883136319));
#94162=CARTESIAN_POINT('Ctrl Pts',(-0.371284574090945,4.92643363271708,
7.31421437766545));
#94163=CARTESIAN_POINT('Ctrl Pts',(-0.278873190275588,4.91345879508931,
7.33150237970099));
#94164=CARTESIAN_POINT('Ctrl Pts',(-0.217066998849999,4.90479505377733,
7.34225971987183));
#94165=CARTESIAN_POINT('Ctrl Pts',(-0.103503078100512,4.88890015931504,
7.36055436914659));
#94166=CARTESIAN_POINT('Ctrl Pts',(-0.0517890764005938,4.88167113576107,
7.36832886423586));
#94167=CARTESIAN_POINT('Ctrl Pts',(-4.36966868262861E-10,4.87444016471971,
7.37555983528029));
#94168=CARTESIAN_POINT('',(-1.03732965834111E-14,5.50000000000001,6.74999999999999));
#94169=CARTESIAN_POINT('',(-1.03732965834111E-14,5.5,6.75));
#94170=CARTESIAN_POINT('Origin',(0.,5.5,0.));
#94171=CARTESIAN_POINT('',(0.21765174428364,4.84409946429302,7.40270156517168));
#94172=CARTESIAN_POINT('Ctrl Pts',(-4.36966868262861E-10,4.87444016471971,
7.37555983528029));
#94173=CARTESIAN_POINT('Ctrl Pts',(0.07241494809842,4.86432933756015,7.38567066244414));
#94174=CARTESIAN_POINT('Ctrl Pts',(0.144966842395702,4.85421607421616,7.39471764056659));
#94175=CARTESIAN_POINT('Ctrl Pts',(0.217651744283678,4.84409946429301,7.40270156517169));
#94176=CARTESIAN_POINT('',(0.950829587222573,4.94797317382581,7.23985627382323));
#94177=CARTESIAN_POINT('Ctrl Pts',(0.950829587406162,4.94797317340535,7.23985627426545));
#94178=CARTESIAN_POINT('Ctrl Pts',(0.830172398471133,4.93049584997117,7.27332990973079));
#94179=CARTESIAN_POINT('Ctrl Pts',(0.708651729226591,4.91309421479886,7.30365549178332));
#94180=CARTESIAN_POINT('Ctrl Pts',(0.46413314457925,4.8784583428577,7.35796112453704));
#94181=CARTESIAN_POINT('Ctrl Pts',(0.341183226959201,4.86123089195753,7.38193070325828));
#94182=CARTESIAN_POINT('Ctrl Pts',(0.217651744283639,4.84409946429302,7.40270156517168));
#94183=CARTESIAN_POINT('',(0.676703532269286,5.00000000025134,7.21834969580106));
#94184=CARTESIAN_POINT('Ctrl Pts',(0.676703532319703,5.0000000003026,7.21834969539148));
#94185=CARTESIAN_POINT('Ctrl Pts',(0.722296915759018,4.99124724609782,7.22286655391651));
#94186=CARTESIAN_POINT('Ctrl Pts',(0.767943881459432,4.9825393678581,7.22691302904827));
#94187=CARTESIAN_POINT('Ctrl Pts',(0.8596489367427,4.96515485059302,7.23408781029232));
#94188=CARTESIAN_POINT('Ctrl Pts',(0.906321056460437,4.95636631402168,7.23723648333365));
#94189=CARTESIAN_POINT('Ctrl Pts',(0.950829587450824,4.94797317474932,7.23985627290408));
#94190=CARTESIAN_POINT('',(1.00084838567572,4.95523000033943,7.22578520694037));
#94191=CARTESIAN_POINT('Ctrl Pts',(1.00084838567572,4.95523000033943,7.22578520694036));
#94192=CARTESIAN_POINT('Ctrl Pts',(0.947301871009143,4.96260329913093,7.22575827892429));
#94193=CARTESIAN_POINT('Ctrl Pts',(0.89309079863658,4.97005789396946,7.22515373936875));
#94194=CARTESIAN_POINT('Ctrl Pts',(0.78469704089313,4.98502388909517,7.22267218727446));
#94195=CARTESIAN_POINT('Ctrl Pts',(0.730685746439649,4.9925027846105,7.22081907683343));
#94196=CARTESIAN_POINT('Ctrl Pts',(0.676703532495354,5.00000000016673,7.21834969551148));
#94197=CARTESIAN_POINT('',(1.30587610327248,5.00000000125165,7.13142255059264));
#94198=CARTESIAN_POINT('Origin',(-1.03278734186302,5.12365720261328,0.181154547137244));
#94199=CARTESIAN_POINT('',(1.05353392264426,4.94797317373232,7.22562537403499));
#94200=CARTESIAN_POINT('Origin',(-1.37961143582091,5.49705145501706,0.611734678451162));
#94201=CARTESIAN_POINT('',(1.80392518127354,4.84409946430028,7.18284182514446));
#94202=CARTESIAN_POINT('Ctrl Pts',(1.80392518127354,4.84409946430028,7.18284182514446));
#94203=CARTESIAN_POINT('Ctrl Pts',(1.67931810259866,4.86143878568035,7.19625831959543));
#94204=CARTESIAN_POINT('Ctrl Pts',(1.55440216827193,4.87877094696219,7.20654281518377));
#94205=CARTESIAN_POINT('Ctrl Pts',(1.36660024350474,4.90476414601202,7.21725427266271));
#94206=CARTESIAN_POINT('Ctrl Pts',(1.30388170545924,4.91343410626486,7.22003862132074));
#94207=CARTESIAN_POINT('Ctrl Pts',(1.20984722770454,4.92641824536596,7.22302434137574));
#94208=CARTESIAN_POINT('Ctrl Pts',(1.17855350996234,4.930736778299,7.22382080511211));
#94209=CARTESIAN_POINT('Ctrl Pts',(1.11628883152147,4.93932462802435,7.22501312674049));
#94210=CARTESIAN_POINT('Ctrl Pts',(1.08624830934207,4.94346583885495,7.22541043952854));
#94211=CARTESIAN_POINT('Ctrl Pts',(1.05353392271017,4.94797317423728,7.22562537347857));
#94212=CARTESIAN_POINT('',(2.48495480999609,4.94797317381999,6.86619220270977));
#94213=CARTESIAN_POINT('Ctrl Pts',(2.48495481024058,4.94797317330798,6.86619220301851));
#94214=CARTESIAN_POINT('Ctrl Pts',(2.37431436120362,4.93049584986762,6.92482097261293));
#94215=CARTESIAN_POINT('Ctrl Pts',(2.26215388175163,4.91309421478555,6.98056091095388));
#94216=CARTESIAN_POINT('Ctrl Pts',(2.03502611120553,4.8784583428514,7.08616117604617));
#94217=CARTESIAN_POINT('Ctrl Pts',(1.92010344521286,4.86123089196737,7.13600095723115));
#94218=CARTESIAN_POINT('Ctrl Pts',(1.80392518127354,4.84409946430028,7.18284182514446));
#94219=CARTESIAN_POINT('',(2.21261439168749,5.00000000026428,6.90411743489196));
#94220=CARTESIAN_POINT('Ctrl Pts',(2.21261439165011,5.00000000031365,6.90411743449623));
#94221=CARTESIAN_POINT('Ctrl Pts',(2.25811281635062,4.99124724655127,6.8987274617925));
#94222=CARTESIAN_POINT('Ctrl Pts',(2.3035624540921,4.98253936819152,6.89286658436005));
#94223=CARTESIAN_POINT('Ctrl Pts',(2.39466586712529,4.96515484985945,6.88015974650244));
#94224=CARTESIAN_POINT('Ctrl Pts',(2.44092369359696,4.95636631272802,6.87320167850187));
#94225=CARTESIAN_POINT('Ctrl Pts',(2.48495480999432,4.94797317483196,6.86619220148691));
#94226=CARTESIAN_POINT('',(2.53077933337913,4.95523000032694,6.84169754621404));
#94227=CARTESIAN_POINT('Ctrl Pts',(2.53077933337913,4.95523000032694,6.84169754621403));
#94228=CARTESIAN_POINT('Ctrl Pts',(2.47848205792871,4.96260285641261,6.85318147604075));
#94229=CARTESIAN_POINT('Ctrl Pts',(2.42540202043434,4.97005835700181,6.86424618380204));
#94230=CARTESIAN_POINT('Ctrl Pts',(2.31901227904161,4.98502388922639,6.88512345703757));
#94231=CARTESIAN_POINT('Ctrl Pts',(2.26586537514055,4.99250278466233,6.89492450294757));
#94232=CARTESIAN_POINT('Ctrl Pts',(2.21261439184018,5.00000000018279,6.90411743457274));
#94233=CARTESIAN_POINT('',(2.80839049007527,5.00000000117302,6.68396909420632));
#94234=CARTESIAN_POINT('Origin',(-0.969699637310454,5.12365838153926,0.398936247790705));
#94235=CARTESIAN_POINT('',(2.58219875254243,4.94797317374736,6.83021561692927));
#94236=CARTESIAN_POINT('Origin',(-1.2158521634837,5.4970520772469,0.894008300633824));
#94237=CARTESIAN_POINT('',(3.30584908222536,4.84409946430701,6.62712038446017));
#94238=CARTESIAN_POINT('Ctrl Pts',(3.30584908222536,4.84409946430701,6.62712038446016));
#94239=CARTESIAN_POINT('Ctrl Pts',(3.18703939746008,4.86143878569,6.6670100473131));
#94240=CARTESIAN_POINT('Ctrl Pts',(3.06725479073445,4.8787709469758,6.70390733053034));
#94241=CARTESIAN_POINT('Ctrl Pts',(2.88614621716508,4.90476414603823,6.75474022258351));
#94242=CARTESIAN_POINT('Ctrl Pts',(2.82549255623583,4.913434106302,6.77094210648112));
#94243=CARTESIAN_POINT('Ctrl Pts',(2.73429839376083,4.92641824541161,6.79407265516783));
#94244=CARTESIAN_POINT('Ctrl Pts',(2.70390752190762,4.93073677834248,6.80157772230459));
#94245=CARTESIAN_POINT('Ctrl Pts',(2.6433579107688,4.93932419694258,6.81612650304836));
#94246=CARTESIAN_POINT('Ctrl Pts',(2.61409834609453,4.94346636783281,6.82297393148364));
#94247=CARTESIAN_POINT('Ctrl Pts',(2.58219875249933,4.94797317419847,6.83021561645868));
#94248=CARTESIAN_POINT('',(3.90288630848711,4.94797317379406,6.17147261466615));
#94249=CARTESIAN_POINT('Ctrl Pts',(3.90288630880333,4.94797317338954,6.17147261495134));
#94250=CARTESIAN_POINT('Ctrl Pts',(3.80743602447103,4.93049584997553,6.2525151024618));
#94251=CARTESIAN_POINT('Ctrl Pts',(3.70988023341334,4.91309421482796,6.33106305997198));
#94252=CARTESIAN_POINT('Ctrl Pts',(3.51076351938066,4.87845834288964,6.48302020640452));
#94253=CARTESIAN_POINT('Ctrl Pts',(3.40924176104253,4.86123089198511,6.55639973739089));
#94254=CARTESIAN_POINT('Ctrl Pts',(3.30584908222535,4.84409946430701,6.62712038446016));
#94255=CARTESIAN_POINT('',(3.64506586129705,5.00000000025158,6.26705631602723));
#94256=CARTESIAN_POINT('Ctrl Pts',(3.64506586117092,5.00000000030281,6.2670563156346));
#94257=CARTESIAN_POINT('Ctrl Pts',(3.68834187479224,4.99124724618209,6.25201154058592));
#94258=CARTESIAN_POINT('Ctrl Pts',(3.73146900939394,4.98253936797242,6.23651735865113));
#94259=CARTESIAN_POINT('Ctrl Pts',(3.81771087915457,4.96515484992084,6.20452305941057));
#94260=CARTESIAN_POINT('Ctrl Pts',(3.86139143710234,4.95636631419786,6.18778360482291));
#94261=CARTESIAN_POINT('Ctrl Pts',(3.90288630830385,4.94797317467443,6.17147261374693));
#94262=CARTESIAN_POINT('',(3.94237385257086,4.95523000032935,6.13769971199802));
#94263=CARTESIAN_POINT('Ctrl Pts',(3.94237385257086,4.95523000032935,6.13769971199802));
#94264=CARTESIAN_POINT('Ctrl Pts',(3.89376504504097,4.96260329920329,6.16015887077973));
#94265=CARTESIAN_POINT('Ctrl Pts',(3.84431056932647,4.97005789391054,6.18237284378588));
#94266=CARTESIAN_POINT('Ctrl Pts',(3.74489308220244,4.98502388904853,6.22563400581526));
#94267=CARTESIAN_POINT('Ctrl Pts',(3.69509565814041,4.99250278455262,6.24663092222021));
#94268=CARTESIAN_POINT('Ctrl Pts',(3.64506586138057,5.00000000016703,6.26705631566973));
#94269=CARTESIAN_POINT('',(4.17958766035098,5.00000000132489,5.92398067006497));
#94270=CARTESIAN_POINT('Origin',(-0.861267622003431,5.12365714954158,0.598067515194973));
#94271=CARTESIAN_POINT('',(3.99012283826856,4.94797317375666,6.11543256900459));
#94272=CARTESIAN_POINT('Origin',(-0.995240108880086,5.49705150748935,1.1344797623526));
#94273=CARTESIAN_POINT('',(4.65319515431945,4.84409946436975,5.76152215993885));
#94274=CARTESIAN_POINT('Ctrl Pts',(4.65319515431945,4.84409946436975,5.76152215993884));
#94275=CARTESIAN_POINT('Ctrl Pts',(4.54573827233818,4.86143878572445,5.82601979492307));
#94276=CARTESIAN_POINT('Ctrl Pts',(4.43668598835844,4.8787709469975,5.88780458982905));
#94277=CARTESIAN_POINT('Ctrl Pts',(4.27073920175616,4.90476414605707,5.97638202692489));
#94278=CARTESIAN_POINT('Ctrl Pts',(4.21498651582412,4.91343410632183,6.00524386397367));
#94279=CARTESIAN_POINT('Ctrl Pts',(4.13089680641441,4.92641824543627,6.04743768254098));
#94280=CARTESIAN_POINT('Ctrl Pts',(4.10282982383664,4.93073677836966,6.06130042448136));
#94281=CARTESIAN_POINT('Ctrl Pts',(4.0468205750289,4.93932462809372,6.08852680617075));
#94282=CARTESIAN_POINT('Ctrl Pts',(4.01972336279107,4.94346583892761,6.10150108536912));
#94283=CARTESIAN_POINT('Ctrl Pts',(3.99012283811852,4.94797317429759,6.11543256851079));
#94284=CARTESIAN_POINT('',(5.13832317951413,4.94797317385176,5.18818182713878));
#94285=CARTESIAN_POINT('Ctrl Pts',(5.13832317996159,4.94797317343003,5.18818182740512));
#94286=CARTESIAN_POINT('Ctrl Pts',(5.06252620966765,4.93049584998606,5.28784857604244));
#94287=CARTESIAN_POINT('Ctrl Pts',(4.9841367078042,4.91309421480021,5.38553173733754));
#94288=CARTESIAN_POINT('Ctrl Pts',(4.82234152687057,4.87845834289208,5.5767404174663));
#94289=CARTESIAN_POINT('Ctrl Pts',(4.73896772101397,4.86123089201307,5.67022855275052));
#94290=CARTESIAN_POINT('Ctrl Pts',(4.65319515431944,4.84409946436975,5.76152215993884));
#94291=CARTESIAN_POINT('',(4.90707810144186,5.00000000032828,5.3369546096604));
#94292=CARTESIAN_POINT('Ctrl Pts',(4.90707810127956,5.00000000036833,5.3369546093818));
#94293=CARTESIAN_POINT('Ctrl Pts',(4.94610815640319,4.99124724787197,5.31295851374921));
#94294=CARTESIAN_POINT('Ctrl Pts',(4.98489621575647,4.98253936874299,5.28855551546913));
#94295=CARTESIAN_POINT('Ctrl Pts',(5.06224396652565,4.96515485157286,5.2387697744877));
#94296=CARTESIAN_POINT('Ctrl Pts',(5.10130481486224,4.95636631445717,5.21303164702084));
#94297=CARTESIAN_POINT('Ctrl Pts',(5.13832317915037,4.94797317480355,5.18818182627541));
#94298=CARTESIAN_POINT('',(5.1696273514169,4.95523000038885,5.14670986113548));
#94299=CARTESIAN_POINT('Ctrl Pts',(5.1696273514169,4.95523000038884,5.14670986113548));
#94300=CARTESIAN_POINT('Ctrl Pts',(5.12698560699481,4.96260285639141,5.17909144937227));
#94301=CARTESIAN_POINT('Ctrl Pts',(5.083457419883,4.97005835694427,5.21142123548925));
#94302=CARTESIAN_POINT('Ctrl Pts',(4.99566684113432,4.9850238898458,5.27504083139195));
#94303=CARTESIAN_POINT('Ctrl Pts',(4.95154737149327,4.99250278501308,5.30625182423134));
#94304=CARTESIAN_POINT('Ctrl Pts',(4.90707810144554,5.00000000026218,5.33695460937339));
#94305=CARTESIAN_POINT('',(5.3553519559481,5.00000000121457,4.88699349554604));
#94306=CARTESIAN_POINT('Origin',(-0.712566840944546,5.12365847699368,0.769230858395806));
#94307=CARTESIAN_POINT('',(5.21147321561416,4.94797317373827,5.11469869085934));
#94308=CARTESIAN_POINT('Origin',(-0.728094867478207,5.49705211887932,1.3219019862453));
#94309=CARTESIAN_POINT('',(5.78296299265857,4.84409946425117,4.62652156278843));
#94310=CARTESIAN_POINT('Ctrl Pts',(5.78296299265856,4.84409946425117,4.62652156278842));
#94311=CARTESIAN_POINT('Ctrl Pts',(5.69188347782073,4.86143878560935,4.71261133216591));
#94312=CARTESIAN_POINT('Ctrl Pts',(5.59866268018144,4.87877094687763,4.79639465042542));
#94313=CARTESIAN_POINT('Ctrl Pts',(5.45563716790461,4.90476414592899,4.9185748500168));
#94314=CARTESIAN_POINT('Ctrl Pts',(5.40739239066292,4.91343410618348,4.95874709274369));
#94315=CARTESIAN_POINT('Ctrl Pts',(5.33433907571752,4.92641824529631,5.01803124509864));
#94316=CARTESIAN_POINT('Ctrl Pts',(5.30990836331075,4.93073677823582,5.03760345545227));
#94317=CARTESIAN_POINT('Ctrl Pts',(5.26106389895748,4.93932419686102,5.07623169312291));
#94318=CARTESIAN_POINT('Ctrl Pts',(5.23738379781279,4.94346636776206,5.09473202319924));
#94319=CARTESIAN_POINT('Ctrl Pts',(5.21147321523184,4.94797317415825,5.11469869026842));
#94320=CARTESIAN_POINT('',(6.13349777051141,4.9479731738001,3.96229742335492));
#94321=CARTESIAN_POINT('Ctrl Pts',(6.13349777089164,4.9479731733255,3.96229742345793));
#94322=CARTESIAN_POINT('Ctrl Pts',(6.08089829633568,4.93049584987379,4.07592812719467));
#94323=CARTESIAN_POINT('Ctrl Pts',(6.025340489868,4.91309421476424,4.18817893573079));
#94324=CARTESIAN_POINT('Ctrl Pts',(5.90843220440268,4.87845834281139,4.40969844464914));
#94325=CARTESIAN_POINT('Ctrl Pts',(5.84710481743528,4.86123089191899,4.51892378299799));
#94326=CARTESIAN_POINT('Ctrl Pts',(5.78296299265856,4.84409946425117,4.62652156278842));
#94327=CARTESIAN_POINT('',(5.93964082487683,5.00000000023931,4.15730283636664));
#94328=CARTESIAN_POINT('Ctrl Pts',(5.93964082458775,5.00000000029233,4.15730283605268));
#94329=CARTESIAN_POINT('Ctrl Pts',(5.97259993462298,4.99124724583479,4.12547744086007));
#94330=CARTESIAN_POINT('Ctrl Pts',(6.00523522309373,4.9825393678026,4.09330668903726));
#94331=CARTESIAN_POINT('Ctrl Pts',(6.07007216271111,4.9651548509353,4.02805743204809));
#94332=CARTESIAN_POINT('Ctrl Pts',(6.10268685331395,4.95636631401737,3.99452411977945));
#94333=CARTESIAN_POINT('Ctrl Pts',(6.13349776983711,4.94797317475143,3.96229742246247));
#94334=CARTESIAN_POINT('',(6.15515482124631,4.95523000034099,3.91506557728136));
#94335=CARTESIAN_POINT('Ctrl Pts',(6.15515482124631,4.95523000034099,3.91506557728135));
#94336=CARTESIAN_POINT('Ctrl Pts',(6.12047100548719,4.96260287679691,3.95585692921522));
#94337=CARTESIAN_POINT('Ctrl Pts',(6.08491047859624,4.97005836655391,3.99678807609253));
#94338=CARTESIAN_POINT('Ctrl Pts',(6.01284887492248,4.98502386882789,4.07779249461766));
#94339=CARTESIAN_POINT('Ctrl Pts',(5.97647028764588,4.99250277458103,4.11775823167738));
#94340=CARTESIAN_POINT('Ctrl Pts',(5.9396408246448,5.00000000018339,4.15730283616115));
#94341=CARTESIAN_POINT('',(6.28070594613454,5.00000000118451,3.62149593580336));
#94342=CARTESIAN_POINT('Origin',(-0.53054494989452,5.12365811164979,0.904427678178179));
#94343=CARTESIAN_POINT('',(6.18914089681808,4.94797317372704,3.87480718636556));
#94344=CARTESIAN_POINT('Origin',(-0.426900607566502,5.4970516443896,1.44751614087276));
#94345=CARTESIAN_POINT('',(6.64232590857355,4.8440994642892,3.2751899592442));
#94346=CARTESIAN_POINT('Ctrl Pts',(6.64232590857354,4.8440994642892,3.27518995924419));
#94347=CARTESIAN_POINT('Ctrl Pts',(6.57188253777224,4.861438785675,3.37884640105228));
#94348=CARTESIAN_POINT('Ctrl Pts',(6.49885212737317,4.87877094694699,3.48071062781813));
#94349=CARTESIAN_POINT('Ctrl Pts',(6.38543560335193,4.90476414598776,3.63078057965921));
#94350=CARTESIAN_POINT('Ctrl Pts',(6.34695460686237,4.91343410624046,3.6803848187376));
#94351=CARTESIAN_POINT('Ctrl Pts',(6.28835357812894,4.92641824534208,3.75398724388821));
#94352=CARTESIAN_POINT('Ctrl Pts',(6.26870148888606,4.93073677827376,3.778353747841));
#94353=CARTESIAN_POINT('Ctrl Pts',(6.22930291024878,4.939324196881,3.82657899477485));
#94354=CARTESIAN_POINT('Ctrl Pts',(6.21015346081782,4.94346636777425,3.84973731918386));
#94355=CARTESIAN_POINT('Ctrl Pts',(6.18914089648487,4.9479731741602,3.87480718600841));
#94356=CARTESIAN_POINT('',(6.84187682255284,4.94797317381414,2.55114039475589));
#94357=CARTESIAN_POINT('Ctrl Pts',(6.84187682304406,4.94797317344389,2.5511403948112));
#94358=CARTESIAN_POINT('Ctrl Pts',(6.8149343374485,4.93049585000131,2.6734218078687));
#94359=CARTESIAN_POINT('Ctrl Pts',(6.78480604719052,4.91309421480685,2.79499154164727));
#94360=CARTESIAN_POINT('Ctrl Pts',(6.71825115882247,4.87845834287996,3.03646387312177));
#94361=CARTESIAN_POINT('Ctrl Pts',(6.68183779109199,4.86123089197961,3.15631915928958));
#94362=CARTESIAN_POINT('Ctrl Pts',(6.64232590857354,4.8440994642892,3.27518995924419));
#94363=CARTESIAN_POINT('',(6.69447254313508,5.00000000036334,2.78326020476335));
#94364=CARTESIAN_POINT('Ctrl Pts',(6.69447254290451,5.00000000039828,2.78326020460221));
#94365=CARTESIAN_POINT('Ctrl Pts',(6.71981956014049,4.99124724875399,2.74509364678722));
#94366=CARTESIAN_POINT('Ctrl Pts',(6.74477609751374,4.98253936923545,2.70665940034705));
#94367=CARTESIAN_POINT('Ctrl Pts',(6.79407052861097,4.96515485071796,2.62899760210498));
#94368=CARTESIAN_POINT('Ctrl Pts',(6.81871403470949,4.95636631384115,2.58923708620832));
#94369=CARTESIAN_POINT('Ctrl Pts',(6.8418768219553,4.94797317467669,2.55114039420255));
#94370=CARTESIAN_POINT('',(6.85287409254451,4.95523000036724,2.50035717833961));
#94371=CARTESIAN_POINT('Ctrl Pts',(6.8528740925445,4.95523000036724,2.50035717833961));
#94372=CARTESIAN_POINT('Ctrl Pts',(6.82776866029154,4.96260329966329,2.54765355854871));
#94373=CARTESIAN_POINT('Ctrl Pts',(6.80184162012553,4.97005789398453,2.5952665193949));
#94374=CARTESIAN_POINT('Ctrl Pts',(6.74887658391066,4.98502389023629,2.68987133710622));
#94375=CARTESIAN_POINT('Ctrl Pts',(6.72193999400436,4.99250278523982,2.7367229505189));
#94376=CARTESIAN_POINT('Ctrl Pts',(6.69447254303287,5.00000000030567,2.78326020453474));
#94377=CARTESIAN_POINT('',(6.91238110702276,5.00000000129598,2.18666125068283));
#94378=CARTESIAN_POINT('Origin',(-0.323716134246077,5.12365830463126,0.997334119173099));
#94379=CARTESIAN_POINT('',(6.87741122879209,4.94797317381514,2.45373400464787));
#94380=CARTESIAN_POINT('Origin',(-0.10574754861476,5.49705229109587,1.50544504490825));
#94381=CARTESIAN_POINT('',(7.19110104734923,4.84409946426157,1.77071411358907));
#94382=CARTESIAN_POINT('Ctrl Pts',(7.19110104734922,4.84409946426157,1.77071411358906));
#94383=CARTESIAN_POINT('Ctrl Pts',(7.14458767434116,4.86143878562981,1.88709036787101));
#94384=CARTESIAN_POINT('Ctrl Pts',(7.09516247199227,4.87877094691969,2.00227244512627));
#94385=CARTESIAN_POINT('Ctrl Pts',(7.01665816682038,4.90476414601387,2.17321504499532));
#94386=CARTESIAN_POINT('Ctrl Pts',(6.98974027973458,4.91343410628763,2.22993184127428));
#94387=CARTESIAN_POINT('Ctrl Pts',(6.94833165618154,4.92641824542731,2.31441097156495));
#94388=CARTESIAN_POINT('Ctrl Pts',(6.93437709992616,4.93073677837388,2.34243241847897));
#94389=CARTESIAN_POINT('Ctrl Pts',(6.90626664071228,4.93932419700383,2.39799971569474));
#94390=CARTESIAN_POINT('Ctrl Pts',(6.89254324996912,4.94346636790369,2.4247331768729));
#94391=CARTESIAN_POINT('Ctrl Pts',(6.87741122807904,4.94797317428302,2.4537340042031));
#94392=CARTESIAN_POINT('',(7.23033731830119,4.94797317377381,1.02069487829441));
#94393=CARTESIAN_POINT('Ctrl Pts',(7.23033731870489,4.94797317337711,1.02069487823912));
#94394=CARTESIAN_POINT('Ctrl Pts',(7.23031162262742,4.93049584992953,1.14590925787838));
#94395=CARTESIAN_POINT('Ctrl Pts',(7.22702161424753,4.91309421478301,1.27111345026311));
#94396=CARTESIAN_POINT('Ctrl Pts',(7.21393215558699,4.87845834284057,1.52124762643535));
#94397=CARTESIAN_POINT('Ctrl Pts',(7.20413545580418,4.86123089194126,1.64612856020698));
#94398=CARTESIAN_POINT('Ctrl Pts',(7.19110104734922,4.84409946426157,1.77071411358906));
#94399=CARTESIAN_POINT('',(7.13627816756702,5.00000000009595,1.27907541649019));
#94400=CARTESIAN_POINT('Ctrl Pts',(7.1362781670175,5.00000000016985,1.27907541626218));
#94401=CARTESIAN_POINT('Ctrl Pts',(7.15282791462048,4.99124724255673,1.23635228273902));
#94402=CARTESIAN_POINT('Ctrl Pts',(7.16893874895024,4.98253936613945,1.19345170510829));
#94403=CARTESIAN_POINT('Ctrl Pts',(7.20038570823038,4.96515485002847,1.10700876358092));
#94404=CARTESIAN_POINT('Ctrl Pts',(7.21590572580901,4.9563663139889,1.06288020482779));
#94405=CARTESIAN_POINT('Ctrl Pts',(7.23033731750308,4.94797317462113,1.02069487785279));
#94406=CARTESIAN_POINT('',(7.23016058785084,4.95523000031898,0.968734856467267));
#94407=CARTESIAN_POINT('Ctrl Pts',(7.23016058785083,4.95523000031898,0.968734856467265));
#94408=CARTESIAN_POINT('Ctrl Pts',(7.21581029494733,4.96260285540334,1.02031929132061));
#94409=CARTESIAN_POINT('Ctrl Pts',(7.20072295871774,4.97005835660489,1.07239895113449));
#94410=CARTESIAN_POINT('Ctrl Pts',(7.16933443085165,4.98502388756489,1.17617465137087));
#94411=CARTESIAN_POINT('Ctrl Pts',(7.15309931311601,4.99250278377018,1.22772147893514));
#94412=CARTESIAN_POINT('Ctrl Pts',(7.13627816725194,4.99999999997397,1.27907541606446));
#94413=CARTESIAN_POINT('',(7.22084100984491,5.00000000122638,0.649580716950613));
#94414=CARTESIAN_POINT('Origin',(-0.101751095987447,5.12365823908661,1.04360640710232));
#94415=CARTESIAN_POINT('',(7.24410145512007,4.94797317373785,0.917926948134186));
#94416=CARTESIAN_POINT('Origin',(0.220349566562635,5.49705203762993,1.49298124256275));
#94417=CARTESIAN_POINT('',(7.40362829344876,4.84409946433362,0.183441643659611));
#94418=CARTESIAN_POINT('Ctrl Pts',(7.40362829344875,4.84409946433362,0.183441643659609));
#94419=CARTESIAN_POINT('Ctrl Pts',(7.38321983188076,4.86143878569194,0.307096086033609));
#94420=CARTESIAN_POINT('Ctrl Pts',(7.35971090518389,4.87877094695177,0.430210227817895));
#94421=CARTESIAN_POINT('Ctrl Pts',(7.31978959305236,4.90476414598828,0.614032389714094));
#94422=CARTESIAN_POINT('Ctrl Pts',(7.3056934658962,4.91343410624058,0.675209728842564));
#94423=CARTESIAN_POINT('Ctrl Pts',(7.28341346881588,4.92641824534731,0.766615414036037));
#94424=CARTESIAN_POINT('Ctrl Pts',(7.27580894512243,4.93073677828274,0.796981552190475));
#94425=CARTESIAN_POINT('Ctrl Pts',(7.26030024063061,4.93932462801487,0.857295662529265));
#94426=CARTESIAN_POINT('Ctrl Pts',(7.25264638036975,4.94346583884927,0.886347499907857));
#94427=CARTESIAN_POINT('Ctrl Pts',(7.24410145445558,4.94797317424166,0.917926947882475));
#94428=CARTESIAN_POINT('',(7.28071527711384,4.94797317386005,-0.557477196754691));
#94429=CARTESIAN_POINT('Ctrl Pts',(7.28071527752219,4.94797317332841,-0.557477196920467));
#94430=CARTESIAN_POINT('Ctrl Pts',(7.30760757251772,4.93049584988333,-0.435184735912635));
#94431=CARTESIAN_POINT('Ctrl Pts',(7.33130968299057,4.9130942147891,-0.3122004936911));
#94432=CARTESIAN_POINT('Ctrl Pts',(7.37229770253631,4.87845834287167,-0.0651004688633301));
#94433=CARTESIAN_POINT('Ctrl Pts',(7.38957575343373,4.86123089199693,0.0589668188442981));
#94434=CARTESIAN_POINT('Ctrl Pts',(7.40362829344875,4.84409946433362,0.183441643659612));
#94435=CARTESIAN_POINT('',(7.24439935455547,5.00000000038041,-0.28491751337921));
#94436=CARTESIAN_POINT('Ctrl Pts',(7.24439935429826,5.00000000041286,-0.284917513425124));
#94437=CARTESIAN_POINT('Ctrl Pts',(7.25137796208485,4.99124724919002,-0.330199477540848));
#94438=CARTESIAN_POINT('Ctrl Pts',(7.25788978100876,4.98253936940856,-0.375560433736857));
#94439=CARTESIAN_POINT('Ctrl Pts',(7.27001885281739,4.96515485016347,-0.466742571032449));
#94440=CARTESIAN_POINT('Ctrl Pts',(7.27568968574208,4.95636631336266,-0.513175778026053));
#94441=CARTESIAN_POINT('Ctrl Pts',(7.28071527589721,4.94797317493522,-0.557477197096403));
#94442=CARTESIAN_POINT('',(7.26937280966497,4.9552300003664,-0.60818443062782));
#94443=CARTESIAN_POINT('Ctrl Pts',(7.26937280966496,4.95523000036639,-0.60818443062782));
#94444=CARTESIAN_POINT('Ctrl Pts',(7.26644714723044,4.96260285571173,-0.554721120165454));
#94445=CARTESIAN_POINT('Ctrl Pts',(7.26290813196574,4.97005835680198,-0.500615723169021));
#94446=CARTESIAN_POINT('Ctrl Pts',(7.25456215699018,4.98502389030606,-0.39251861678044));
#94447=CARTESIAN_POINT('Ctrl Pts',(7.24978765196605,4.99250278526087,-0.338686864118216));
#94448=CARTESIAN_POINT('Ctrl Pts',(7.24439935438014,5.00000000032684,-0.284917513532059));
#94449=CARTESIAN_POINT('',(7.19166241212645,5.00000000121785,-0.917873489557443));
#94450=CARTESIAN_POINT('Origin',(0.124975105914598,5.12365739689806,1.04108015340628));
#94451=CARTESIAN_POINT('',(7.27206554876221,4.94797317374701,-0.660801352633178));
#94452=CARTESIAN_POINT('Origin',(0.536147021643578,5.49705179128573,1.41070678503679));
#94453=CARTESIAN_POINT('',(7.26997010912512,4.84409946433572,-1.41240835333832));
#94454=CARTESIAN_POINT('Ctrl Pts',(7.26997010912511,4.84409946433571,-1.41240835333831));
#94455=CARTESIAN_POINT('Ctrl Pts',(7.27662083595686,4.86143878568868,-1.28725766717237));
#94456=CARTESIAN_POINT('Ctrl Pts',(7.2801274361364,4.87877094696363,-1.16196814131573));
#94457=CARTESIAN_POINT('Ctrl Pts',(7.28065579313712,4.90476414601994,-0.973861737398919));
#94458=CARTESIAN_POINT('Ctrl Pts',(7.28004054511674,4.91343410627963,-0.9110844398));
#94459=CARTESIAN_POINT('Ctrl Pts',(7.27793096236606,4.92641824539027,-0.817026227957172));
#94460=CARTESIAN_POINT('Ctrl Pts',(7.27703205029688,4.93073677832517,-0.785735285440253));
#94461=CARTESIAN_POINT('Ctrl Pts',(7.27485168155049,4.93932462805329,-0.723497372470726));
#94462=CARTESIAN_POINT('Ctrl Pts',(7.27362205056032,4.9434658388885,-0.693479397176331));
#94463=CARTESIAN_POINT('Ctrl Pts',(7.27206554810619,4.94797317426655,-0.660801352736085));
#94464=CARTESIAN_POINT('',(6.99065508110836,4.94797317379603,-2.10958225861235));
#94465=CARTESIAN_POINT('Ctrl Pts',(6.9906550815225,4.94797317344677,-2.10958225885756));
#94466=CARTESIAN_POINT('Ctrl Pts',(7.04320791370601,4.93049585004491,-1.99592997627474));
#94467=CARTESIAN_POINT('Ctrl Pts',(7.09279385896656,4.91309421486669,-1.88091628978998));
#94468=CARTESIAN_POINT('Ctrl Pts',(7.18594280252527,4.8784583429496,-1.6484045388198));
#94469=CARTESIAN_POINT('Ctrl Pts',(7.22948770172626,4.86123089204045,-1.53095214538267));
#94470=CARTESIAN_POINT('Ctrl Pts',(7.26997010912511,4.84409946433571,-1.41240835333831));
#94471=CARTESIAN_POINT('',(7.01378048014667,5.00000000026952,-1.83558801947581));
#94472=CARTESIAN_POINT('Ctrl Pts',(7.01378047975564,5.00000000031813,-1.83558801946016));
#94473=CARTESIAN_POINT('Ctrl Pts',(7.01086164706033,4.99124724655311,-1.88131152369201));
#94474=CARTESIAN_POINT('Ctrl Pts',(7.00746995880966,4.98253936810556,-1.92701180779298));
#94475=CARTESIAN_POINT('Ctrl Pts',(6.99971399681033,4.96515485196445,-2.01866953306197));
#94476=CARTESIAN_POINT('Ctrl Pts',(6.99527048224866,4.95636631483061,-2.06523621940693));
#94477=CARTESIAN_POINT('Ctrl Pts',(6.99065508034933,4.9479731746186,-2.10958225868904));
#94478=CARTESIAN_POINT('',(6.96867723835465,4.95523000034217,-2.15666568933291));
#94479=CARTESIAN_POINT('Ctrl Pts',(6.96867723835464,4.95523000034216,-2.1566656893329));
#94480=CARTESIAN_POINT('Ctrl Pts',(6.97731355112746,4.9626033197548,-2.10382006469291));
#94481=CARTESIAN_POINT('Ctrl Pts',(6.98548733530497,4.97005790364313,-2.05022541290881));
#94482=CARTESIAN_POINT('Ctrl Pts',(7.00057460256239,4.98502386914664,-1.94285831994863));
#94483=CARTESIAN_POINT('Ctrl Pts',(7.00748397221452,4.99250277474619,-1.88925867215296));
#94484=CARTESIAN_POINT('Ctrl Pts',(7.01378047986531,5.00000000021824,-1.83558801943564));
#94485=CARTESIAN_POINT('',(6.82620967368096,5.00000000114615,-2.44240895163504));
#94486=CARTESIAN_POINT('Origin',(0.345853143282498,5.12365841010391,0.989875246164395));
#94487=CARTESIAN_POINT('',(6.95999593981941,4.94797317380956,-2.20863131600617));
#94488=CARTESIAN_POINT('Origin',(0.826872135186473,5.497052011915,1.26246970665074));
#94489=CARTESIAN_POINT('',(6.79637620263612,4.84409946426182,-2.9422157054656));
#94490=CARTESIAN_POINT('Ctrl Pts',(6.79637620263611,4.84409946426182,-2.94221570546559));
#94491=CARTESIAN_POINT('Ctrl Pts',(6.82977513725051,4.86143878564932,-2.82142068241563));
#94492=CARTESIAN_POINT('Ctrl Pts',(6.86013329958665,4.87877094694303,-2.69981417138956));
#94493=CARTESIAN_POINT('Ctrl Pts',(6.9010866203215,4.90476414603892,-2.51621917174387));
#94494=CARTESIAN_POINT('Ctrl Pts',(6.91398101974245,4.91343410631165,-2.45477731233615));
#94495=CARTESIAN_POINT('Ctrl Pts',(6.93214049304112,4.92641824545061,-2.36246463126814));
#94496=CARTESIAN_POINT('Ctrl Pts',(6.93798922471456,4.93073677839702,-2.33171201406331));
#94497=CARTESIAN_POINT('Ctrl Pts',(6.94923914330869,4.93932462815421,-2.27046047403663));
#94498=CARTESIAN_POINT('Ctrl Pts',(6.95449123775758,4.94346583900203,-2.24087996800498));
#94499=CARTESIAN_POINT('Ctrl Pts',(6.95999593906431,4.94797317440998,-2.2086313159612));
#94500=CARTESIAN_POINT('',(6.37371962360107,4.94797317381679,-3.56304559730339));
#94501=CARTESIAN_POINT('Ctrl Pts',(6.37371962396418,4.94797317343968,-3.56304559764541));
#94502=CARTESIAN_POINT('Ctrl Pts',(6.44947568136037,4.93049584998276,-3.46334774781826));
#94503=CARTESIAN_POINT('Ctrl Pts',(6.52262687755466,4.91309421478169,-3.36168252998804));
#94504=CARTESIAN_POINT('Ctrl Pts',(6.66358120398301,4.87845834284509,-3.15463104407018));
#94505=CARTESIAN_POINT('Ctrl Pts',(6.7313568403172,4.8612308919452,-3.04928548853122));
#94506=CARTESIAN_POINT('Ctrl Pts',(6.79637620263611,4.84409946426182,-2.94221570546559));
#94507=CARTESIAN_POINT('',(6.45520502561423,5.00000000025075,-3.30042846896563));
#94508=CARTESIAN_POINT('Ctrl Pts',(6.45520502521441,5.0000000003021,-3.30042846886068));
#94509=CARTESIAN_POINT('Ctrl Pts',(6.44252523076982,4.99124724615799,-3.34445552223589));
#94510=CARTESIAN_POINT('Ctrl Pts',(6.42938862844364,4.98253936795439,-3.38835824515637));
#94511=CARTESIAN_POINT('Ctrl Pts',(6.4021102929694,4.96515485046747,-3.47620576779447));
#94512=CARTESIAN_POINT('Ctrl Pts',(6.38776020295519,4.95636631289811,-3.5207285295106));
#94513=CARTESIAN_POINT('Ctrl Pts',(6.37371962278214,4.94797317468673,-3.56304559720421));
#94514=CARTESIAN_POINT('',(6.34213406430118,4.9552300003035,-3.6043036579765));
#94515=CARTESIAN_POINT('Ctrl Pts',(6.34213406430117,4.95523000030349,-3.60430365797649));
#94516=CARTESIAN_POINT('Ctrl Pts',(6.36192865855916,4.96260329977038,-3.55455022116892));
#94517=CARTESIAN_POINT('Ctrl Pts',(6.38143263973457,4.97005789381842,-3.50396563895263));
#94518=CARTESIAN_POINT('Ctrl Pts',(6.41924800147741,4.98502388909895,-3.4023518433995));
#94519=CARTESIAN_POINT('Ctrl Pts',(6.4375181459293,4.99250278459722,-3.35149070138016));
#94520=CARTESIAN_POINT('Ctrl Pts',(6.45520502526095,5.000000000166,-3.30042846906862));
#94521=CARTESIAN_POINT('',(6.14157095691406,5.00000000128657,-3.85274008640452));
#94522=CARTESIAN_POINT('Origin',(0.550561349058368,5.12365835348864,0.892384193535622));
#94523=CARTESIAN_POINT('',(6.32248465610192,4.94797317381261,-3.65318813480831));
#94524=CARTESIAN_POINT('Origin',(1.07893432263829,5.49705219109465,1.05520055428565));
#94525=CARTESIAN_POINT('',(6.00499129873184,4.84409946432866,-4.33444832088375));
#94526=CARTESIAN_POINT('Ctrl Pts',(6.00499129873183,4.84409946432866,-4.33444832088374));
#94527=CARTESIAN_POINT('Ctrl Pts',(6.0635767440552,4.86143878570101,-4.22365720208668));
#94528=CARTESIAN_POINT('Ctrl Pts',(6.11936695459161,4.87877094698558,-4.11141989129545));
#94529=CARTESIAN_POINT('Ctrl Pts',(6.19883030728706,4.90476414606178,-3.94092099420311));
#94530=CARTESIAN_POINT('Ctrl Pts',(6.22463142636344,4.91343410632696,-3.88368752607863));
#94531=CARTESIAN_POINT('Ctrl Pts',(6.26221083893537,4.92641824545147,-3.79743681421562));
#94532=CARTESIAN_POINT('Ctrl Pts',(6.27453373416553,4.93073677839264,-3.76866048055067));
#94533=CARTESIAN_POINT('Ctrl Pts',(6.29868669384673,4.93932419701259,-3.71126224911645));
#94534=CARTESIAN_POINT('Ctrl Pts',(6.31017758861645,4.94346636791043,-3.68349592530596));
#94535=CARTESIAN_POINT('Ctrl Pts',(6.32248465533595,4.94797317428232,-3.65318813456712));
#94536=CARTESIAN_POINT('',(5.45875612031797,4.94797317386576,-4.84990488434038));
#94537=CARTESIAN_POINT('Ctrl Pts',(5.45875612062196,4.94797317342923,-4.84990488479222));
#94538=CARTESIAN_POINT('Ctrl Pts',(5.55417313422535,4.93049584997211,-4.76882322821963));
#94539=CARTESIAN_POINT('Ctrl Pts',(5.64746911273217,4.91309421478837,-4.68526023150146));
#94540=CARTESIAN_POINT('Ctrl Pts',(5.82963795448276,4.87845834287648,-4.51335050771509));
#94541=CARTESIAN_POINT('Ctrl Pts',(5.91847521456085,4.86123089199598,-4.42503763104279));
#94542=CARTESIAN_POINT('Ctrl Pts',(6.00499129873183,4.84409946432866,-4.33444832088374));
#94543=CARTESIAN_POINT('',(5.59479135903471,5.00000000038232,-4.61094455025847));
#94544=CARTESIAN_POINT('Ctrl Pts',(5.59479135887404,5.00000000040474,-4.61094455017618));
#94545=CARTESIAN_POINT('Ctrl Pts',(5.57294351023375,4.99124725213808,-4.65121646793442));
#94546=CARTESIAN_POINT('Ctrl Pts',(5.55067623930233,4.9825393709129,-4.69126880256542));
#94547=CARTESIAN_POINT('Ctrl Pts',(5.50515102629905,4.96515484986163,-4.77119847942965));
#94548=CARTESIAN_POINT('Ctrl Pts',(5.48156535851485,4.95636631335134,-4.81159547373595));
#94549=CARTESIAN_POINT('Ctrl Pts',(5.45875611941956,4.9479731748415,-4.84990488401924));
#94550=CARTESIAN_POINT('',(5.4190397503672,4.95523000038511,-4.88340839283606));
#94551=CARTESIAN_POINT('Ctrl Pts',(5.41903975036719,4.95523000038511,-4.88340839283605));
#94552=CARTESIAN_POINT('Ctrl Pts',(5.44906526742851,4.96260285565642,-4.83907608709589));
#94553=CARTESIAN_POINT('Ctrl Pts',(5.47899107385436,4.97005835699077,-4.79386143369335));
#94554=CARTESIAN_POINT('Ctrl Pts',(5.53776448660362,4.98502389150453,-4.70275530179052));
#94555=CARTESIAN_POINT('Ctrl Pts',(5.56654112273603,4.99250278589832,-4.65701081271476));
#94556=CARTESIAN_POINT('Ctrl Pts',(5.59479135889404,5.00000000037313,-4.61094455020163));
#94557=CARTESIAN_POINT('',(5.16975920861961,5.00000000120979,-5.08292137649758));
#94558=CARTESIAN_POINT('Origin',(0.729525520746253,5.12365827876601,0.753166594087148));
#94559=CARTESIAN_POINT('',(5.38934101651039,4.94797317378957,-4.92692593619431));
#94560=CARTESIAN_POINT('Origin',(1.28054633176727,5.49705206174571,0.798591557250787));
#94561=CARTESIAN_POINT('',(4.93281967559905,4.84409946430769,-5.52400695080939));
#94562=CARTESIAN_POINT('Ctrl Pts',(4.93281967559905,4.84409946430769,-5.52400695080939));
#94563=CARTESIAN_POINT('Ctrl Pts',(5.01385224130635,4.86143878567624,-5.42840020581429));
#94564=CARTESIAN_POINT('Ctrl Pts',(5.0924658118048,4.87877094694699,-5.33078018714352));
#94565=CARTESIAN_POINT('Ctrl Pts',(5.20672357837545,4.90476414600742,-5.18134973151522));
#94566=CARTESIAN_POINT('Ctrl Pts',(5.24422498543453,4.91343410626691,-5.13100082803629));
#94567=CARTESIAN_POINT('Ctrl Pts',(5.2994671656839,4.9264182453903,-5.05484507279633));
#94568=CARTESIAN_POINT('Ctrl Pts',(5.31768801958001,4.93073677833341,-5.02939057204024));
#94569=CARTESIAN_POINT('Ctrl Pts',(5.3536152195635,4.93932419696309,-4.97852645172661));
#94570=CARTESIAN_POINT('Ctrl Pts',(5.37080640243511,4.94346636786295,-4.95387949186148));
#94571=CARTESIAN_POINT('Ctrl Pts',(5.38934101594713,4.94797317425716,-4.92692593588516));
#94572=CARTESIAN_POINT('',(4.28854724725375,4.94797317383398,-5.90998800973694));
#94573=CARTESIAN_POINT('Ctrl Pts',(4.28854724746879,4.94797317349561,-5.90998801024313));
#94574=CARTESIAN_POINT('Ctrl Pts',(4.39916362364428,4.93049585005688,-5.85131383520822));
#94575=CARTESIAN_POINT('Ctrl Pts',(4.50824196854606,4.91309421481951,-5.78976037230495));
#94576=CARTESIAN_POINT('Ctrl Pts',(4.72310731303538,4.87845834289832,-5.66103071843775));
#94577=CARTESIAN_POINT('Ctrl Pts',(4.82885226541687,4.86123089199607,-5.59387993259784));
#94578=CARTESIAN_POINT('Ctrl Pts',(4.93281967559905,4.84409946430769,-5.52400695080939));
#94579=CARTESIAN_POINT('',(4.47277146646462,5.00000000040085,-5.70585799033773));
#94580=CARTESIAN_POINT('Ctrl Pts',(4.47277146628161,5.00000000043033,-5.70585799018668));
#94581=CARTESIAN_POINT('Ctrl Pts',(4.4427771279562,4.99124724963524,-5.74049174101125));
#94582=CARTESIAN_POINT('Ctrl Pts',(4.41242038951624,4.9825393696399,-5.77482086437295));
#94583=CARTESIAN_POINT('Ctrl Pts',(4.35077702246364,4.96515485137633,-5.84309524400365));
#94584=CARTESIAN_POINT('Ctrl Pts',(4.31905861476746,4.95636631464917,-5.87747755814629));
#94585=CARTESIAN_POINT('Ctrl Pts',(4.28854724663545,4.94797317468629,-5.9099880093767));
#94586=CARTESIAN_POINT('',(4.24255716059391,4.95523000035748,-5.9341703789812));
#94587=CARTESIAN_POINT('Ctrl Pts',(4.24255716059391,4.95523000035748,-5.93417037898119));
#94588=CARTESIAN_POINT('Ctrl Pts',(4.28141083181686,4.9626028554184,-5.89732913766012));
#94589=CARTESIAN_POINT('Ctrl Pts',(4.32035680406356,4.97005835687664,-5.85960474094954));
#94590=CARTESIAN_POINT('Ctrl Pts',(4.39734124811627,4.9850238906012,-5.78326317035894));
#94591=CARTESIAN_POINT('Ctrl Pts',(4.43527881784727,4.99250278545199,-5.7447742858742));
#94592=CARTESIAN_POINT('Ctrl Pts',(4.47277146625573,5.0000000003522,-5.70585799030624));
#94593=CARTESIAN_POINT('',(3.9562152655006,5.00000000119967,-6.07543091178372));
#94594=CARTESIAN_POINT('Origin',(0.874379005841,5.12365747043237,0.578729661810663));
#94595=CARTESIAN_POINT('',(4.20419778110858,4.94797317373202,-5.97028615646991));
#94596=CARTESIAN_POINT('Origin',(1.42228181186611,5.49705160338535,0.504640299297654));
#94597=CARTESIAN_POINT('',(3.62999488635505,4.84409946430512,-6.45526915547616));
#94598=CARTESIAN_POINT('Ctrl Pts',(3.62999488635505,4.84409946430512,-6.45526915547615));
#94599=CARTESIAN_POINT('Ctrl Pts',(3.7296855797877,4.86143878566297,-6.37931724938182));
#94600=CARTESIAN_POINT('Ctrl Pts',(3.82744662710813,4.87877094691801,-6.30087912636897));
#94601=CARTESIAN_POINT('Ctrl Pts',(3.97115624145015,4.90476414595063,-6.17950431415894));
#94602=CARTESIAN_POINT('Ctrl Pts',(4.01860441240173,4.91343410619924,-6.13839423406338));
#94603=CARTESIAN_POINT('Ctrl Pts',(4.08892629741799,4.92641824530769,-6.07589439388384));
#94604=CARTESIAN_POINT('Ctrl Pts',(4.11219312311801,4.93073677824677,-6.0549519501943));
#94605=CARTESIAN_POINT('Ctrl Pts',(4.15821695793549,4.93932462798877,-6.01299818461731));
#94606=CARTESIAN_POINT('Ctrl Pts',(4.18029947338156,4.94346583882346,-5.99262778107491));
#94607=CARTESIAN_POINT('Ctrl Pts',(4.20419778064507,4.94797317423399,-5.97028615607538));
#94608=CARTESIAN_POINT('',(2.91781067191024,4.94797317384864,-6.69372666398598));
#94609=CARTESIAN_POINT('Ctrl Pts',(2.91781067198254,4.94797317341034,-6.69372666447471));
#94610=CARTESIAN_POINT('Ctrl Pts',(3.03845411208919,4.93049584998617,-6.6602035100653));
#94611=CARTESIAN_POINT('Ctrl Pts',(3.15821444043594,4.9130942148187,-6.62353775288799));
#94612=CARTESIAN_POINT('Ctrl Pts',(3.39572942290471,4.87845834288346,-6.54400742451796));
#94613=CARTESIAN_POINT('Ctrl Pts',(3.51343755092169,4.86123089198299,-6.5011586257738));
#94614=CARTESIAN_POINT('Ctrl Pts',(3.62999488635505,4.84409946430512,-6.45526915547615));
#94615=CARTESIAN_POINT('',(3.14160975151107,5.00000000050473,-6.53397185204522));
#94616=CARTESIAN_POINT('Ctrl Pts',(3.1416097514399,5.00000000051907,-6.5339718519543));
#94617=CARTESIAN_POINT('Ctrl Pts',(3.10487144135448,4.99124725210346,-6.56134798140165));
#94618=CARTESIAN_POINT('Ctrl Pts',(3.06784467500926,4.98253937089912,-6.58834871129871));
#94619=CARTESIAN_POINT('Ctrl Pts',(2.99296550810226,4.96515484931178,-6.6417753822365));
#94620=CARTESIAN_POINT('Ctrl Pts',(2.95459747928808,4.9563663132354,-6.66853533540674));
#94621=CARTESIAN_POINT('Ctrl Pts',(2.9178106712046,4.9479731748178,-6.69372666327845));
#94622=CARTESIAN_POINT('',(2.86769731302197,4.9552300003156,-6.70745715373435));
#94623=CARTESIAN_POINT('Ctrl Pts',(2.86769731302196,4.9552300003156,-6.70745715373435));
#94624=CARTESIAN_POINT('Ctrl Pts',(2.91356514802405,4.96260329944764,-6.67982796665955));
#94625=CARTESIAN_POINT('Ctrl Pts',(2.95970462086193,4.97005789421878,-6.65136123553827));
#94626=CARTESIAN_POINT('Ctrl Pts',(3.05130322991824,4.98502389160803,-6.5933520712326));
#94627=CARTESIAN_POINT('Ctrl Pts',(3.0966278099219,4.99250278600782,-6.56391849325386));
#94628=CARTESIAN_POINT('Ctrl Pts',(3.1416097514151,5.00000000048106,-6.53397185200841));
#94629=CARTESIAN_POINT('',(2.55768309275547,5.00000000129321,-6.78386005075774));
#94630=CARTESIAN_POINT('Origin',(0.978345977284807,5.12365820924026,0.377235247498451));
#94631=CARTESIAN_POINT('',(2.82247093033594,4.94797317374067,-6.73448243143106));
#94632=CARTESIAN_POINT('Origin',(1.49751226228398,5.49705172217515,0.187094326967195));
#94633=CARTESIAN_POINT('',(2.15743557083302,4.84409946430342,-7.08469014864696));
#94634=CARTESIAN_POINT('Ctrl Pts',(2.15743557083301,4.84409946430342,-7.08469014864696));
#94635=CARTESIAN_POINT('Ctrl Pts',(2.27112296602449,4.86143878568678,-7.03194450811468));
#94636=CARTESIAN_POINT('Ctrl Pts',(2.3834602923105,4.87877094695926,-6.97635596016067));
#94637=CARTESIAN_POINT('Ctrl Pts',(2.54990205272904,4.90476414600642,-6.88871214258509));
#94638=CARTESIAN_POINT('Ctrl Pts',(2.60507836392412,4.91343410626223,-6.85876314746769));
#94639=CARTESIAN_POINT('Ctrl Pts',(2.68719178061627,4.92641824537106,-6.81284164534936));
#94640=CARTESIAN_POINT('Ctrl Pts',(2.71441664721448,4.93073677830577,-6.79739050411575));
#94641=CARTESIAN_POINT('Ctrl Pts',(2.76838328981831,4.93932462803495,-6.7663113582995));
#94642=CARTESIAN_POINT('Ctrl Pts',(2.79432856296978,4.94346583886611,-6.75116429152838));
#94643=CARTESIAN_POINT('Ctrl Pts',(2.82247092998867,4.94797317425684,-6.73448243098469));
#94644=CARTESIAN_POINT('',(1.4106405125511,4.94797317381983,-7.1644740989605));
#94645=CARTESIAN_POINT('Ctrl Pts',(1.41064051251384,4.94797317337648,-7.16447409941471));
#94646=CARTESIAN_POINT('Ctrl Pts',(1.53566986328428,4.9304958499545,-7.15766947114909));
#94647=CARTESIAN_POINT('Ctrl Pts',(1.6605123154199,4.91309421482194,-7.14760586952016));
#94648=CARTESIAN_POINT('Ctrl Pts',(1.90957099917454,4.87845834289018,-7.12099361639327));
#94649=CARTESIAN_POINT('Ctrl Pts',(2.03373840160017,4.86123089199066,-7.1044503668768));
#94650=CARTESIAN_POINT('Ctrl Pts',(2.15743557083302,4.84409946430342,-7.08469014864696));
#94651=CARTESIAN_POINT('',(1.66354985423409,5.0000000002771,-7.05656445327241));
#94652=CARTESIAN_POINT('Ctrl Pts',(1.66354985406861,5.0000000003246,-7.05656445292761));
#94653=CARTESIAN_POINT('Ctrl Pts',(1.62178538240259,4.99124724672022,-7.07540290402672));
#94654=CARTESIAN_POINT('Ctrl Pts',(1.57981993525488,4.98253936818981,-7.09381270558874));
#94655=CARTESIAN_POINT('Ctrl Pts',(1.49520626317404,4.96515484998644,-7.12989347614351));
#94656=CARTESIAN_POINT('Ctrl Pts',(1.45198265424955,4.95636631292779,-7.14777980636546));
#94657=CARTESIAN_POINT('Ctrl Pts',(1.41064051201504,4.94797317475814,-7.16447409810473));
#94658=CARTESIAN_POINT('',(1.35874712633804,4.95523000034704,-7.16711068663691));
#94659=CARTESIAN_POINT('Ctrl Pts',(1.35874712633804,4.95523000034704,-7.16711068663691));
#94660=CARTESIAN_POINT('Ctrl Pts',(1.40947914477903,4.96260287653345,-7.14998866555321));
#94661=CARTESIAN_POINT('Ctrl Pts',(1.46066553790084,4.97005836668923,-7.13210394217435));
#94662=CARTESIAN_POINT('Ctrl Pts',(1.5625895074464,4.98502386911349,-7.09514321554628));
#94663=CARTESIAN_POINT('Ctrl Pts',(1.61318184884325,4.99250277469276,-7.07614119944428));
#94664=CARTESIAN_POINT('Ctrl Pts',(1.66354985413998,5.00000000022698,-7.05656445301108));
#94665=CARTESIAN_POINT('',(1.03955650211012,5.00000000120338,-7.17508343327527));
#94666=CARTESIAN_POINT('Origin',(1.036567218847,5.12365836611404,0.158100762754939));
#94667=CARTESIAN_POINT('',(1.30876847510296,4.94797317377319,-7.18378179327604));
#94668=CARTESIAN_POINT('Origin',(1.50272107965398,5.49705188654033,-0.139199236961874));
#94669=CARTESIAN_POINT('',(0.583996966610964,4.84409946429569,-7.38283890436021));
#94670=CARTESIAN_POINT('Ctrl Pts',(0.583996966610964,4.84409946429569,-7.38283890436021));
#94671=CARTESIAN_POINT('Ctrl Pts',(0.706365167153948,4.86143878568503,-7.35576585697531));
#94672=CARTESIAN_POINT('Ctrl Pts',(0.828026003708649,4.87877094696627,-7.32562614285952));
#94673=CARTESIAN_POINT('Ctrl Pts',(1.00941727820285,4.9047641460309,-7.27581144753047));
#94674=CARTESIAN_POINT('Ctrl Pts',(1.06974174655383,4.91343410629532,-7.25842391917415));
#94675=CARTESIAN_POINT('Ctrl Pts',(1.15980716267515,4.92641824541257,-7.23122799358558));
#94676=CARTESIAN_POINT('Ctrl Pts',(1.18971706562288,4.93073677834755,-7.22199063300904));
#94677=CARTESIAN_POINT('Ctrl Pts',(1.24910011444237,4.93932419695411,-7.20324027462032));
#94678=CARTESIAN_POINT('Ctrl Pts',(1.27770160048699,4.94346636784186,-7.19402266140034));
#94679=CARTESIAN_POINT('Ctrl Pts',(1.30876847481697,4.94797317421864,-7.1837817926045));
#94680=CARTESIAN_POINT('',(-0.162489631407365,4.94797317382355,-7.30021868713222));
#94681=CARTESIAN_POINT('Ctrl Pts',(0.583996966611005,4.84409946429568,-7.38283890436021));
#94682=CARTESIAN_POINT('Ctrl Pts',(0.458124049300158,4.8613432067681,-7.37549809137105));
#94683=CARTESIAN_POINT('Ctrl Pts',(0.332486921697074,4.87868417663361,-7.36487179654896));
#94684=CARTESIAN_POINT('Ctrl Pts',(0.0835403843745239,4.91332225950562,
-7.33723683118231));
#94685=CARTESIAN_POINT('Ctrl Pts',(-0.039730334296242,4.93061037670979,
-7.32031818479942));
#94686=CARTESIAN_POINT('Ctrl Pts',(-0.162489633664296,4.947973174,-7.30021868758569));
#94687=CARTESIAN_POINT('Ctrl Pts',(-0.16248963429871,4.947973174,-7.30021868757157));
#94688=CARTESIAN_POINT('Ctrl Pts',(-0.108561113272334,4.95826854665991,
-7.29112111604271));
#94689=CARTESIAN_POINT('Ctrl Pts',(-0.0521079532441121,4.96904363931287,
-7.280985998079));
#94690=CARTESIAN_POINT('Ctrl Pts',(0.0386164317799012,4.98655204091907,
-7.26342789469982));
#94691=CARTESIAN_POINT('Ctrl Pts',(0.0731912356494929,4.99326273977431,
-7.25645071890302));
#94692=CARTESIAN_POINT('Ctrl Pts',(0.107704215939166,5.00000000018496,-7.2491999420065));
#94693=CARTESIAN_POINT('Origin',(1.80433264358217E-13,0.560925700000069,
-1.78199469069718E-12));
#94694=CARTESIAN_POINT('',(0.0337098038873345,0.680081834075993,7.43224893803594));
#94695=CARTESIAN_POINT('',(-0.576449088722096,0.562053379604022,7.28929565008102));
#94696=CARTESIAN_POINT('Origin',(1.46195216787403,0.516179043705186,-0.0906469046179226));
#94697=CARTESIAN_POINT('',(-0.598338399571803,0.767975418683164,7.49397642673713));
#94698=CARTESIAN_POINT('Origin',(-1.04077295590179,0.781987935583024,-0.237140562616648));
#94699=CARTESIAN_POINT('',(-1.20895591280749,0.680609080401461,7.33160125317681));
#94700=CARTESIAN_POINT('Ctrl Pts',(-1.20895590604886,0.680609079137261,
7.33160125103559));
#94701=CARTESIAN_POINT('Ctrl Pts',(-1.10870785777768,0.695136945009207,
7.36285586434991));
#94702=CARTESIAN_POINT('Ctrl Pts',(-1.00781302078567,0.709660812774055,
7.39200030989459));
#94703=CARTESIAN_POINT('Ctrl Pts',(-0.804232337447924,0.738780776769552,
7.44620706154414));
#94704=CARTESIAN_POINT('Ctrl Pts',(-0.701560825553855,0.753373671689897,
7.47123699479757));
#94705=CARTESIAN_POINT('Ctrl Pts',(-0.598394674877222,0.76794900780124,
7.49409641631185));
#94706=CARTESIAN_POINT('Ctrl Pts',(-0.576449088806045,0.562053379332408,
7.28929564980192));
#94707=CARTESIAN_POINT('Ctrl Pts',(-0.681392523124575,0.582224590096564,
7.30123074297468));
#94708=CARTESIAN_POINT('Ctrl Pts',(-0.786632152876032,0.602198953290415,
7.31073322818269));
#94709=CARTESIAN_POINT('Ctrl Pts',(-0.944626918335057,0.63181112165897,
7.32130389112597));
#94710=CARTESIAN_POINT('Ctrl Pts',(-0.997209431170085,0.64160443307101,
7.32421114415442));
#94711=CARTESIAN_POINT('Ctrl Pts',(-1.10694538657959,0.661914308861971,
7.3290041747411));
#94712=CARTESIAN_POINT('Ctrl Pts',(-1.1598156619626,0.671620855129919,7.33059470553222));
#94713=CARTESIAN_POINT('Ctrl Pts',(-1.20895591292573,0.680609080021414,
7.33160125079771));
#94714=CARTESIAN_POINT('Origin',(-1.91686944095437E-13,0.560925699999978,
-1.84856470408779E-14));
#94715=CARTESIAN_POINT('',(-7.41752113576009,0.680609079284826,0.440830472641154));
#94716=CARTESIAN_POINT('',(-7.30981359453413,0.562053379737014,-0.180969162848937));
#94717=CARTESIAN_POINT('Ctrl Pts',(-7.30981359577408,0.562053380753659,
-0.180969163194634));
#94718=CARTESIAN_POINT('Ctrl Pts',(-7.33220244279024,0.581887251281355,
-0.0780125161171526));
#94719=CARTESIAN_POINT('Ctrl Pts',(-7.35239722361586,0.601712674307791,
0.0253974978158168));
#94720=CARTESIAN_POINT('Ctrl Pts',(-7.37931284034215,0.631348476780122,
0.180808155407383));
#94721=CARTESIAN_POINT('Ctrl Pts',(-7.38769933974359,0.641177712391296,
0.232489641937349));
#94722=CARTESIAN_POINT('Ctrl Pts',(-7.40413083467024,0.661766419240893,
0.341043172649691));
#94723=CARTESIAN_POINT('Ctrl Pts',(-7.411386466036,0.67167472079557,0.393456954212761));
#94724=CARTESIAN_POINT('Ctrl Pts',(-7.41752113534007,0.680609080456112,
0.440830481409885));
#94725=CARTESIAN_POINT('',(-7.51537925264731,0.767975418698991,-0.191745179874597));
#94726=CARTESIAN_POINT('Origin',(0.180300736303671,0.781863706247153,-1.05208177488254));
#94727=CARTESIAN_POINT('',(-7.38630038189549,0.680609080418115,-0.810257984958939));
#94728=CARTESIAN_POINT('Ctrl Pts',(-7.38630037943127,0.680609079122411,
-0.810257978393205));
#94729=CARTESIAN_POINT('Ctrl Pts',(-7.41208183476458,0.695136944724126,
-0.708464863768294));
#94730=CARTESIAN_POINT('Ctrl Pts',(-7.43572120077453,0.70966081220104,-0.606140151255856));
#94731=CARTESIAN_POINT('Ctrl Pts',(-7.47882681837764,0.738780776746267,
-0.399923338135681));
#94732=CARTESIAN_POINT('Ctrl Pts',(-7.49826151950297,0.753373671681126,
-0.29604730943592));
#94733=CARTESIAN_POINT('Ctrl Pts',(-7.51550211293464,0.767949007820357,
-0.19179487652695));
#94734=CARTESIAN_POINT('Ctrl Pts',(-7.3098135938762,0.562053378853381,-0.180969163074211));
#94735=CARTESIAN_POINT('Ctrl Pts',(-7.32741270633406,0.582224589722421,
-0.285112536374756));
#94736=CARTESIAN_POINT('Ctrl Pts',(-7.34259881413271,0.602198953022129,
-0.38968336948138));
#94737=CARTESIAN_POINT('Ctrl Pts',(-7.36170779620114,0.631811365835249,
-0.546875435673787));
#94738=CARTESIAN_POINT('Ctrl Pts',(-7.36745767304757,0.641604918980557,
-0.599224737511866));
#94739=CARTESIAN_POINT('Ctrl Pts',(-7.37818459623173,0.661914788918559,
-0.708540272763156));
#94740=CARTESIAN_POINT('Ctrl Pts',(-7.38263500616264,0.671621089600935,
-0.761245578256281));
#94741=CARTESIAN_POINT('Ctrl Pts',(-7.38630037964414,0.680609080075174,
-0.810257985190196));
#94742=CARTESIAN_POINT('Origin',(-1.90342533401555E-12,0.901573518000139,
8.56519716263549E-14));
#94743=CARTESIAN_POINT('',(7.4975175754087,0.900669500589968,0.19295130544917));
#94744=CARTESIAN_POINT('',(7.49067431208828,0.809946052894305,-0.373896494420664));
#94745=CARTESIAN_POINT('Ctrl Pts',(7.49067429618873,0.809946054097563,-0.373896494256488));
#94746=CARTESIAN_POINT('Ctrl Pts',(7.49125842929932,0.811814511300298,-0.362193921634754));
#94747=CARTESIAN_POINT('Ctrl Pts',(7.49181928421141,0.813696729840433,-0.350406919339319));
#94748=CARTESIAN_POINT('Ctrl Pts',(7.49288856452571,0.817476260956881,-0.326742025674024));
#94749=CARTESIAN_POINT('Ctrl Pts',(7.49339363131842,0.819360421133853,-0.31494646269074));
#94750=CARTESIAN_POINT('Ctrl Pts',(7.49482562592852,0.825015714746983,-0.279547522709436));
#94751=CARTESIAN_POINT('Ctrl Pts',(7.49566888951138,0.828788189479575,-0.255941112703458));
#94752=CARTESIAN_POINT('Ctrl Pts',(7.49786506079125,0.840115815423992,-0.185079488469201));
#94753=CARTESIAN_POINT('Ctrl Pts',(7.49888268519632,0.847675760663585,-0.137815748088289));
#94754=CARTESIAN_POINT('Ctrl Pts',(7.50059447826849,0.870367208581086,0.00396235750429899));
#94755=CARTESIAN_POINT('Ctrl Pts',(7.49994903612033,0.885511641104869,0.0984719273944452));
#94756=CARTESIAN_POINT('Ctrl Pts',(7.49751757541842,0.900669500313366,0.192951305493795));
#94757=CARTESIAN_POINT('',(7.46163841178383,0.80994605200789,0.757596327810578));
#94758=CARTESIAN_POINT('Origin',(-0.191501740625454,0.803573279257418,-0.0204809236956735));
#94759=CARTESIAN_POINT('',(7.49028775646232,0.750000000660804,0.381561705761236));
#94760=CARTESIAN_POINT('Origin',(-0.18323094549859,0.946349170784347,-0.0404830745463346));
#94761=CARTESIAN_POINT('',(7.49999996733933,0.750000000076743,-0.000442032240240194));
#94762=CARTESIAN_POINT('Origin',(0.,0.750000001098927,0.));
#94763=CARTESIAN_POINT('Origin',(-0.192837956609714,0.803569462561183,0.00860069228931772));
#94764=CARTESIAN_POINT('Origin',(-1.8385328792773E-14,1.03148891300036,
2.49279763497867E-12));
#94765=CARTESIAN_POINT('',(0.352520299374595,0.940053947031003,-7.49171071504816));
#94766=CARTESIAN_POINT('',(-0.21691191335407,1.03040248142683,-7.49686262514646));
#94767=CARTESIAN_POINT('Ctrl Pts',(-0.216911913327511,1.03040248160653,
-7.49686262520794));
#94768=CARTESIAN_POINT('Ctrl Pts',(-0.122018200336322,1.01543877096837,
-7.49960825066177));
#94769=CARTESIAN_POINT('Ctrl Pts',(-0.0270884842090412,1.00042308922614,
-7.50055169267878));
#94770=CARTESIAN_POINT('Ctrl Pts',(0.162771944844896,0.970299044466182,
-7.49883462807081));
#94771=CARTESIAN_POINT('Ctrl Pts',(0.257687167935843,0.955193108293956,
-7.49617306068821));
#94772=CARTESIAN_POINT('Ctrl Pts',(0.352520283380967,0.940053949645103,
-7.4917107158382));
#94773=CARTESIAN_POINT('',(-0.21323909129465,0.849330497163622,-7.49696798168821));
#94774=CARTESIAN_POINT('Ctrl Pts',(0.352520299950128,0.940053947,-7.49171071505854));
#94775=CARTESIAN_POINT('Ctrl Pts',(0.258300413424799,0.924915272696728,
-7.49614420480774));
#94776=CARTESIAN_POINT('Ctrl Pts',(0.164004206490097,0.909779286371552,
-7.49879990837626));
#94777=CARTESIAN_POINT('Ctrl Pts',(-0.0246342017421915,0.8795298092342,
-7.50055261076486));
#94778=CARTESIAN_POINT('Ctrl Pts',(-0.118951432514705,0.864420318633172,
-7.49964985260826));
#94779=CARTESIAN_POINT('Ctrl Pts',(-0.213239091592113,0.849330499322643,
-7.49696799311674));
#94780=CARTESIAN_POINT('',(-0.778885090560337,0.940053948012018,-7.45944622867757));
#94781=CARTESIAN_POINT('Origin',(-0.0019124445238064,0.80358396694885,0.191459074564228));
#94782=CARTESIAN_POINT('Origin',(0.0190137625473567,0.946429295162185,0.191888929096342));
#94783=CARTESIAN_POINT('Origin',(5.63351448823468E-13,4.93907429999929,
-1.01706634108613E-13));
#94784=CARTESIAN_POINT('',(7.43060586817456,4.81939092007921,0.00690867062542753));
#94785=CARTESIAN_POINT('',(7.28652936255512,4.93794662021698,-0.61042155713763));
#94786=CARTESIAN_POINT('Ctrl Pts',(7.28652936159588,4.93794662121202,-0.610421556668722));
#94787=CARTESIAN_POINT('Ctrl Pts',(7.31511188023545,4.91789697871817,-0.509403982041436));
#94788=CARTESIAN_POINT('Ctrl Pts',(7.34136770815382,4.89804362330483,-0.407718113515646));
#94789=CARTESIAN_POINT('Ctrl Pts',(7.37733075383442,4.86848704273741,-0.253835059088018));
#94790=CARTESIAN_POINT('Ctrl Pts',(7.38878640668564,4.85863343285326,-0.202106738273538));
#94791=CARTESIAN_POINT('Ctrl Pts',(7.4114199687586,4.83820008061128,-0.0939490028819038));
#94792=CARTESIAN_POINT('Ctrl Pts',(7.42160776861126,4.82843422647897,-0.0417175607597513));
#94793=CARTESIAN_POINT('Ctrl Pts',(7.43060586925475,4.81939091904273,0.00690867580317548));
#94794=CARTESIAN_POINT('',(7.49205823556675,4.73201982385041,-0.621930980993225));
#94795=CARTESIAN_POINT('Origin',(-0.147247077923713,4.81289609762555,-1.05774438459138));
#94796=CARTESIAN_POINT('',(7.3263771516294,4.8193909197014,-1.2402214161419));
#94797=CARTESIAN_POINT('Ctrl Pts',(7.32637714974651,4.81939092084888,-1.24022141040838));
#94798=CARTESIAN_POINT('Ctrl Pts',(7.35824914062546,4.80491309543195,-1.13868537527286));
#94799=CARTESIAN_POINT('Ctrl Pts',(7.3879807452778,4.79041128730459,-1.03649293430841));
#94800=CARTESIAN_POINT('Ctrl Pts',(7.44329381503338,4.76128647694134,-0.830331917669992));
#94801=CARTESIAN_POINT('Ctrl Pts',(7.46884404609903,4.74666639456629,-0.72637863675835));
#94802=CARTESIAN_POINT('Ctrl Pts',(7.49219469844694,4.73203683302836,-0.621923452288041));
#94803=CARTESIAN_POINT('Ctrl Pts',(7.28652936366133,4.93794661914144,-0.61042155681656));
#94804=CARTESIAN_POINT('Ctrl Pts',(7.29763906183347,4.91814186442495,-0.715041521521126));
#94805=CARTESIAN_POINT('Ctrl Pts',(7.30652508358286,4.89834552791114,-0.819874369499637));
#94806=CARTESIAN_POINT('Ctrl Pts',(7.31648502147922,4.86872423031979,-0.977205672761118));
#94807=CARTESIAN_POINT('Ctrl Pts',(7.31924110656159,4.85888055797719,-1.02956737186234));
#94808=CARTESIAN_POINT('Ctrl Pts',(7.32384982960819,4.83826147069255,-1.13942245512654));
#94809=CARTESIAN_POINT('Ctrl Pts',(7.32539897638504,4.82833849612749,-1.1923916710017));
#94810=CARTESIAN_POINT('Ctrl Pts',(7.32637714961331,4.81939092000682,-1.24022141624027));
#94811=CARTESIAN_POINT('Origin',(-5.17787725715513E-14,4.89709473199831,
9.39656338849737E-12));
#94812=CARTESIAN_POINT('',(0.40918343007075,4.81939092003514,-7.41933421681296));
#94813=CARTESIAN_POINT('',(-0.215041573947508,4.93794662006386,-7.30889059675964));
#94814=CARTESIAN_POINT('Ctrl Pts',(-0.215041573499948,4.93794662117583,
-7.30889059546253));
#94815=CARTESIAN_POINT('Ctrl Pts',(-0.111912073431109,4.91775746672574,
-7.33212275399106));
#94816=CARTESIAN_POINT('Ctrl Pts',(-0.00823378782372437,4.89776736698642,
-7.35296247351665));
#94817=CARTESIAN_POINT('Ctrl Pts',(0.147742625517286,4.86814634061535,-7.38055596638373));
#94818=CARTESIAN_POINT('Ctrl Pts',(0.199659714009096,4.85836129974299,-7.38912265896429));
#94819=CARTESIAN_POINT('Ctrl Pts',(0.308142139983319,4.83806891418287,-7.40573574428087));
#94820=CARTESIAN_POINT('Ctrl Pts',(0.360483919976071,4.82837106019443,-7.41302625476642));
#94821=CARTESIAN_POINT('Ctrl Pts',(0.409183435372163,4.81939091904092,-7.41933421745164));
#94822=CARTESIAN_POINT('',(-0.215407009827946,4.73201982383798,-7.5147411512686));
#94823=CARTESIAN_POINT('Origin',(-1.06416490854892,4.8128960435549,0.0897660560821278));
#94824=CARTESIAN_POINT('',(-0.841760461628196,4.81939091968843,-7.38277662222671));
#94825=CARTESIAN_POINT('Ctrl Pts',(-0.841760456065915,4.81939092085314,
-7.38277662005998));
#94826=CARTESIAN_POINT('Ctrl Pts',(-0.73864781800586,4.8049130955081,-7.40910481766066));
#94827=CARTESIAN_POINT('Ctrl Pts',(-0.634995615012,4.79041128745961,-7.43326023103532));
#94828=CARTESIAN_POINT('Ctrl Pts',(-0.42614236103085,4.76128647694644,-7.47733084719864));
#94829=CARTESIAN_POINT('Ctrl Pts',(-0.320958274967625,4.74666639456744,
-7.49721568948058));
#94830=CARTESIAN_POINT('Ctrl Pts',(-0.215392104223649,4.73203683301729,
-7.51487700641513));
#94831=CARTESIAN_POINT('Ctrl Pts',(-0.215041573798538,4.93794661921194,
-7.30889059741849));
#94832=CARTESIAN_POINT('Ctrl Pts',(-0.31890663738018,4.91814186444707,-7.32564801301616));
#94833=CARTESIAN_POINT('Ctrl Pts',(-0.423104659537805,4.89834552786635,
-7.34019653868519));
#94834=CARTESIAN_POINT('Ctrl Pts',(-0.5796660027,4.86872423024089,-7.35865961455493));
#94835=CARTESIAN_POINT('Ctrl Pts',(-0.631801697389271,4.85888055789695,
-7.36424646284628));
#94836=CARTESIAN_POINT('Ctrl Pts',(-0.741246156930806,4.83826147071718,
-7.37479586106029));
#94837=CARTESIAN_POINT('Ctrl Pts',(-0.794053819745922,4.82833849616759,
-7.37921043141456));
#94838=CARTESIAN_POINT('Ctrl Pts',(-0.841760461825666,4.81939091997017,
-7.38277662029196));
#94839=CARTESIAN_POINT('Origin',(1.04430353253804E-12,1.16011713400017,
4.97377746627725E-14));
#94840=CARTESIAN_POINT('',(7.49772190572655,1.15903910528887,0.184841071447948));
#94841=CARTESIAN_POINT('',(7.49040836445842,1.06939092095439,-0.379186648426675));
#94842=CARTESIAN_POINT('Ctrl Pts',(7.49040836574509,1.0693909221528,-0.379186648467453));
#94843=CARTESIAN_POINT('Ctrl Pts',(7.49516278556348,1.0844050142568,-0.285268399695008));
#94844=CARTESIAN_POINT('Ctrl Pts',(7.49815066787259,1.09938963374112,-0.191263707148619));
#94845=CARTESIAN_POINT('Ctrl Pts',(7.50058866531781,1.12928008044628,-0.00320582877183695));
#94846=CARTESIAN_POINT('Ctrl Pts',(7.5000395265062,1.14418337209935,0.0908312575294414));
#94847=CARTESIAN_POINT('Ctrl Pts',(7.49772190590341,1.15903910529533,0.184841071561819));
#94848=CARTESIAN_POINT('',(7.46217159729501,1.06939091911158,0.752326401888058));
#94849=CARTESIAN_POINT('Origin',(-0.181513436785086,1.33838400563824,0.0240420059235262));
#94850=CARTESIAN_POINT('',(7.49755829997,0.979367659104793,0.191362310599562));
#94851=CARTESIAN_POINT('Origin',(-0.19191440622657,0.946436322382179,0.000401916073186764));
#94852=CARTESIAN_POINT('Ctrl Pts',(7.4975583002797,0.979367658874596,0.191362310570904));
#94853=CARTESIAN_POINT('Ctrl Pts',(7.49998541853642,0.994471430918934,0.0962680332434526));
#94854=CARTESIAN_POINT('Ctrl Pts',(7.5006033321718,1.00953259012931,0.00112879444476032));
#94855=CARTESIAN_POINT('Ctrl Pts',(7.4982187960069,1.03954821707066,-0.189104195261569));
#94856=CARTESIAN_POINT('Ctrl Pts',(7.4952177633165,1.05450026189394,-0.284182377452428));
#94857=CARTESIAN_POINT('Ctrl Pts',(7.49040836538004,1.069390921,-0.379186655678594));
#94858=CARTESIAN_POINT('Origin',(-4.50160742015981E-13,4.74999999999911,
-7.45388993583784E-14));
#94859=CARTESIAN_POINT('',(7.49028775568068,4.75000000000442,0.381561704655806));
#94860=CARTESIAN_POINT('',(7.4999999819041,4.75000000415214,-0.00044203176353017));
#94861=CARTESIAN_POINT('Origin',(0.,4.75000000067138,0.));
#94862=CARTESIAN_POINT('',(7.46163840082974,4.69005394803158,0.757596337309733));
#94863=CARTESIAN_POINT('Origin',(-0.183233979794819,4.55370521392812,-0.0404746383756041));
#94864=CARTESIAN_POINT('',(7.4975175754792,4.5993304994336,0.192951308991991));
#94865=CARTESIAN_POINT('Origin',(-0.19149502490191,4.69642568282372,-0.0204805842445447));
#94866=CARTESIAN_POINT('',(7.49067431020226,4.69005394712068,-0.373896499429461));
#94867=CARTESIAN_POINT('Ctrl Pts',(7.49751757532976,4.59933049913374,0.192951308940038));
#94868=CARTESIAN_POINT('Ctrl Pts',(7.49994903597294,4.61448835770566,0.0984719348112532));
#94869=CARTESIAN_POINT('Ctrl Pts',(7.50059447821245,4.62963278959406,0.00396236889379918));
#94870=CARTESIAN_POINT('Ctrl Pts',(7.49888268543748,4.65232423742436,-0.137815736135372));
#94871=CARTESIAN_POINT('Ctrl Pts',(7.49786506102374,4.65988418320927,-0.185079479921373));
#94872=CARTESIAN_POINT('Ctrl Pts',(7.49566888963438,4.67121180996999,-0.255941109259036));
#94873=CARTESIAN_POINT('Ctrl Pts',(7.49482562599899,4.67498428497423,-0.279547520964337));
#94874=CARTESIAN_POINT('Ctrl Pts',(7.49339363128608,4.68063957899424,-0.314946463492495));
#94875=CARTESIAN_POINT('Ctrl Pts',(7.4928885644551,4.68252373930679,-0.326742027324636));
#94876=CARTESIAN_POINT('Ctrl Pts',(7.49181928405843,4.68630327068637,-0.350406922637988));
#94877=CARTESIAN_POINT('Ctrl Pts',(7.49125842910013,4.68818548936229,-0.36219392578413));
#94878=CARTESIAN_POINT('Ctrl Pts',(7.49067429593706,4.69005394670754,-0.373896499298968));
#94879=CARTESIAN_POINT('Origin',(-0.192835064026876,4.69643091592117,0.00860058943978748));
#94880=CARTESIAN_POINT('Origin',(4.05578348683377E-12,4.78597145200587,
3.00810833964919E-13));
#94881=CARTESIAN_POINT('',(7.46187241733356,4.78575691081507,0.188108803306894));
#94882=CARTESIAN_POINT('Ctrl Pts',(7.49999998560045,4.75000000137362,-0.000442028262827379));
#94883=CARTESIAN_POINT('Ctrl Pts',(7.49405312262923,4.75594872264478,0.0310883694741082));
#94884=CARTESIAN_POINT('Ctrl Pts',(7.48790160624312,4.76190334823606,0.0625682707651447));
#94885=CARTESIAN_POINT('Ctrl Pts',(7.47519008163412,4.77382403272204,0.125426831226749));
#94886=CARTESIAN_POINT('Ctrl Pts',(7.46863459627975,4.77978626801372,0.156785509594588));
#94887=CARTESIAN_POINT('Ctrl Pts',(7.46187241698066,4.78575691117149,0.188108803162771));
#94888=CARTESIAN_POINT('Origin',(-0.261599883382976,4.80792711944447,1.42878715025716));
#94889=CARTESIAN_POINT('Origin',(-9.65329266569198E-14,1.28891220999942,
-2.21003770839445E-12));
#94890=CARTESIAN_POINT('',(0.346190408762415,1.19797317426376,-7.49200588672075));
#94891=CARTESIAN_POINT('',(-0.215486077596536,1.28783500377754,-7.49690374767466));
#94892=CARTESIAN_POINT('Ctrl Pts',(-0.215486074181298,1.28783500620183,
-7.49690374433565));
#94893=CARTESIAN_POINT('Ctrl Pts',(-0.121879038955992,1.27281874405466,
-7.49959432343662));
#94894=CARTESIAN_POINT('Ctrl Pts',(-0.0282369965533449,1.25781697911053,
-7.50053152780386));
#94895=CARTESIAN_POINT('Ctrl Pts',(0.112248484511282,1.23534090680584,-7.49930625044361));
#94896=CARTESIAN_POINT('Ctrl Pts',(0.15908255975695,1.22785302041325,-7.49845896723859));
#94897=CARTESIAN_POINT('Ctrl Pts',(0.229301947591752,1.21663380888301,-7.4965304222764));
#94898=CARTESIAN_POINT('Ctrl Pts',(0.252694445968612,1.21289755923839,-7.49577836510434));
#94899=CARTESIAN_POINT('Ctrl Pts',(0.287773141688719,1.2072966749925,-7.49448620361555));
#94900=CARTESIAN_POINT('Ctrl Pts',(0.299462014246144,1.20543067036107,-7.49402824540192));
#94901=CARTESIAN_POINT('Ctrl Pts',(0.322912484277998,1.20168768135239,-7.49305452574449));
#94902=CARTESIAN_POINT('Ctrl Pts',(0.334592979913718,1.19982364587847,-7.49254178002325));
#94903=CARTESIAN_POINT('Ctrl Pts',(0.346190411497856,1.19797317338938,-7.49200588620877));
#94904=CARTESIAN_POINT('',(-0.220938354192998,1.1083007626432,-7.49674504312255));
#94905=CARTESIAN_POINT('Ctrl Pts',(0.346190409540422,1.19797317429373,-7.49200588629922));
#94906=CARTESIAN_POINT('Ctrl Pts',(0.334478336782823,1.19613294342686,-7.49254707744697));
#94907=CARTESIAN_POINT('Ctrl Pts',(0.322694364732621,1.19428069285451,-7.49306406841878));
#94908=CARTESIAN_POINT('Ctrl Pts',(0.299045101682687,1.19056192455289,-7.49404506041721));
#94909=CARTESIAN_POINT('Ctrl Pts',(0.28724999051619,1.18870644997233,-7.49450643984025));
#94910=CARTESIAN_POINT('Ctrl Pts',(0.251844369753666,1.18313463689047,-7.49580766695149));
#94911=CARTESIAN_POINT('Ctrl Pts',(0.228231329885431,1.17941569911441,-7.49656378454989));
#94912=CARTESIAN_POINT('Ctrl Pts',(0.157317570547834,1.16823832462178,-7.49849918027799));
#94913=CARTESIAN_POINT('Ctrl Pts',(0.11001033880432,1.16077003178017,-7.49934237919276));
#94914=CARTESIAN_POINT('Ctrl Pts',(-0.031866414243553,1.13833699173946,
-7.50052851618956));
#94915=CARTESIAN_POINT('Ctrl Pts',(-0.12642295644833,1.1233390886692,-7.49953052900198));
#94916=CARTESIAN_POINT('Ctrl Pts',(-0.220938354235387,1.10830076288434,
-7.49674504325897));
#94917=CARTESIAN_POINT('',(-0.785187302803007,1.19797317358555,-7.45878548488081));
#94918=CARTESIAN_POINT('Origin',(0.0417752178770776,1.33917527074983,0.181485827824975));
#94919=CARTESIAN_POINT('Ctrl Pts',(-0.215486081067869,1.28783500479116,
-7.49690374413771));
#94920=CARTESIAN_POINT('Ctrl Pts',(-0.371541670048592,1.26310656824362,
-7.492418184706));
#94921=CARTESIAN_POINT('Ctrl Pts',(-0.52705976664116,1.23856749893779,-7.4830668161156));
#94922=CARTESIAN_POINT('Ctrl Pts',(-0.68159806042696,1.21428571428671,-7.46896405695075));
#94923=CARTESIAN_POINT('Ctrl Pts',(-0.716124358854676,1.20886077964635,
-7.46581327755717));
#94924=CARTESIAN_POINT('Ctrl Pts',(-0.750655784688141,1.20342302038954,
-7.46242062154302));
#94925=CARTESIAN_POINT('Ctrl Pts',(-0.785187302078986,1.1979731744789,-7.45878548428992));
#94926=CARTESIAN_POINT('Origin',(4.64569195380408E-14,4.651755933,1.34441069388203E-13));
#94927=CARTESIAN_POINT('',(0.352520299435009,4.55994605297308,-7.49171071504532));
#94928=CARTESIAN_POINT('',(-0.213239091294667,4.65066950283638,-7.49696798168821));
#94929=CARTESIAN_POINT('Ctrl Pts',(-0.21323909159213,4.65066950067736,-7.49696799311675));
#94930=CARTESIAN_POINT('Ctrl Pts',(-0.118951423809548,4.63557967997365,
-7.49964985285588));
#94931=CARTESIAN_POINT('Ctrl Pts',(-0.0246341842936763,4.62047018797078,
-7.50055261092768));
#94932=CARTESIAN_POINT('Ctrl Pts',(0.164004223867748,4.59022071083884,-7.49879990788983));
#94933=CARTESIAN_POINT('Ctrl Pts',(0.258300407446502,4.57508472826227,-7.49614420490339));
#94934=CARTESIAN_POINT('Ctrl Pts',(0.352520285220108,4.55994605536672,-7.49171071575167));
#94935=CARTESIAN_POINT('',(-0.216911910735758,4.46959751859283,-7.49686262533737));
#94936=CARTESIAN_POINT('Ctrl Pts',(0.352520299950129,4.559946053,-7.49171071505855));
#94937=CARTESIAN_POINT('Ctrl Pts',(0.257687188908902,4.54480689504879,-7.49617305991154));
#94938=CARTESIAN_POINT('Ctrl Pts',(0.162771970224917,4.5297009595704,-7.4988346274642));
#94939=CARTESIAN_POINT('Ctrl Pts',(-0.0270884634955866,4.49957691405067,
-7.50055169286844));
#94940=CARTESIAN_POINT('Ctrl Pts',(-0.122018188701805,4.48456123086711,
-7.49960825096596));
#94941=CARTESIAN_POINT('Ctrl Pts',(-0.216911910766392,4.46959751879733,
-7.49686262528204));
#94942=CARTESIAN_POINT('',(-0.778885090560973,4.55994605198798,-7.45944622867665));
#94943=CARTESIAN_POINT('Origin',(0.019013766933039,4.55357071037472,0.191888962985897));
#94944=CARTESIAN_POINT('Origin',(-0.00191244455506986,4.69641603310801,
0.191459074053018));
#94945=CARTESIAN_POINT('Origin',(-1.0698907038087E-12,1.41887506700011,
-6.74102700742862E-14));
#94946=CARTESIAN_POINT('',(7.4975151551836,1.41778968867681,0.193045310352991));
#94947=CARTESIAN_POINT('',(7.49065292194418,1.32710049349124,-0.374324466840203));
#94948=CARTESIAN_POINT('Ctrl Pts',(7.4906529218194,1.32710049291663,-0.374324464653929));
#94949=CARTESIAN_POINT('Ctrl Pts',(7.49537415365484,1.34215639817109,-0.279847313460021));
#94950=CARTESIAN_POINT('Ctrl Pts',(7.49830730405831,1.3572471693734,-0.185294207848121));
#94951=CARTESIAN_POINT('Ctrl Pts',(7.50059562915091,1.38748517979131,0.00388086647019446));
#94952=CARTESIAN_POINT('Ctrl Pts',(7.49995002764233,1.40262869206186,0.0984794794256389));
#94953=CARTESIAN_POINT('Ctrl Pts',(7.49751515557731,1.41778968810576,0.1930453104547));
#94954=CARTESIAN_POINT('',(7.46168168499786,1.32710049307755,0.757170029230453));
#94955=CARTESIAN_POINT('Origin',(-0.192110746278644,1.33928593621152,-0.0175336555807591));
#94956=CARTESIAN_POINT('',(7.49763545617134,1.23689319392375,0.188315065789256));
#94957=CARTESIAN_POINT('Origin',(-0.180076328767131,1.48200507450974,-0.0430982005950535));
#94958=CARTESIAN_POINT('Ctrl Pts',(7.49763520838133,1.23689161580505,0.188324937383956));
#94959=CARTESIAN_POINT('Ctrl Pts',(7.49999062502235,1.25189323496832,0.0945456360206955));
#94960=CARTESIAN_POINT('Ctrl Pts',(7.50058654174518,1.26691709131601,0.000733325220453728));
#94961=CARTESIAN_POINT('Ctrl Pts',(7.49884066957372,1.28947386856058,-0.139957457048645));
#94962=CARTESIAN_POINT('Ctrl Pts',(7.49781889281453,1.29699561098365,-0.186845521176366));
#94963=CARTESIAN_POINT('Ctrl Pts',(7.49562653093622,1.30828230113851,-0.257163397504894));
#94964=CARTESIAN_POINT('Ctrl Pts',(7.49478566948927,1.31204559065348,-0.280602684308469));
#94965=CARTESIAN_POINT('Ctrl Pts',(7.49335944336427,1.31769120063995,-0.315755915413143));
#94966=CARTESIAN_POINT('Ctrl Pts',(7.49285652500688,1.31957324836617,-0.327473114439529));
#94967=CARTESIAN_POINT('Ctrl Pts',(7.49179152371613,1.32335238839832,-0.350997861002957));
#94968=CARTESIAN_POINT('Ctrl Pts',(7.49123331922751,1.32523416776575,-0.362710060842525));
#94969=CARTESIAN_POINT('Ctrl Pts',(7.49065292159669,1.32710049380022,-0.374324469110649));
#94970=CARTESIAN_POINT('Origin',(2.16840434497101E-15,4.52171036999889,
-3.69170839731314E-14));
#94971=CARTESIAN_POINT('',(7.49755829997,4.52063234089521,0.191362310599587));
#94972=CARTESIAN_POINT('',(7.49040836444859,4.43060907904567,-0.379186648479543));
#94973=CARTESIAN_POINT('Ctrl Pts',(7.49040836538005,4.430609079,-0.379186655678578));
#94974=CARTESIAN_POINT('Ctrl Pts',(7.49521776331607,4.44549973810469,-0.28418237746117));
#94975=CARTESIAN_POINT('Ctrl Pts',(7.49821879600634,4.46045178292658,-0.189104195279084));
#94976=CARTESIAN_POINT('Ctrl Pts',(7.50060333217191,4.49046740986781,0.00112879442655575));
#94977=CARTESIAN_POINT('Ctrl Pts',(7.49998541853666,4.50552856907956,0.096268033234006));
#94978=CARTESIAN_POINT('Ctrl Pts',(7.49755830027969,4.52063234112541,0.191362310570927));
#94979=CARTESIAN_POINT('',(7.4621715972985,4.43060908088843,0.752326401885845));
#94980=CARTESIAN_POINT('Origin',(-0.191914406238891,4.55356367763345,0.000401916168807082));
#94981=CARTESIAN_POINT('',(7.49772190590322,4.34096089502546,0.184841070538928));
#94982=CARTESIAN_POINT('Origin',(-0.181513473722006,4.1616169543297,0.0240418511233536));
#94983=CARTESIAN_POINT('Ctrl Pts',(7.49772190592924,4.3409608948701,0.184841070515018));
#94984=CARTESIAN_POINT('Ctrl Pts',(7.50003951773272,4.35581657174786,0.0908316128767517));
#94985=CARTESIAN_POINT('Ctrl Pts',(7.50058866069735,4.37071997613226,-0.00320618473889875));
#94986=CARTESIAN_POINT('Ctrl Pts',(7.49815066788195,4.4006103662136,-0.191263706864571));
#94987=CARTESIAN_POINT('Ctrl Pts',(7.49516278557001,4.41559498572476,-0.285268399579692));
#94988=CARTESIAN_POINT('Ctrl Pts',(7.4904083657424,4.43060907785576,-0.379186648520938));
#94989=CARTESIAN_POINT('Origin',(1.95927331601629E-14,1.54874775200071,
4.17200995972422E-13));
#94990=CARTESIAN_POINT('',(0.352840825559124,1.45719264094421,-7.49169562594985));
#94991=CARTESIAN_POINT('',(-0.216060229695852,1.5476605353396,-7.49688720083611));
#94992=CARTESIAN_POINT('Ctrl Pts',(-0.21606023090219,1.54766053042136,-7.49688721914786));
#94993=CARTESIAN_POINT('Ctrl Pts',(-0.121254461794605,1.5326678365177,-7.49961952067055));
#94994=CARTESIAN_POINT('Ctrl Pts',(-0.0264122851482628,1.51762759595714,
-7.5005530047104));
#94995=CARTESIAN_POINT('Ctrl Pts',(0.163270940331239,1.48746377141007,-7.49882263926133));
#94996=CARTESIAN_POINT('Ctrl Pts',(0.258096561970816,1.47234261566213,-7.49615785262344));
#94997=CARTESIAN_POINT('Ctrl Pts',(0.352840824503127,1.45719264779623,-7.49169562599575));
#94998=CARTESIAN_POINT('',(-0.213439952126814,1.36645689698012,-7.49696226262636));
#94999=CARTESIAN_POINT('Ctrl Pts',(0.35284082530523,1.45719263430125,-7.49169562595797));
#95000=CARTESIAN_POINT('Ctrl Pts',(0.258534072859532,1.44204301532236,-7.49613724692419));
#95001=CARTESIAN_POINT('Ctrl Pts',(0.164150094801047,1.4269003938282,-7.49879783063957));
#95002=CARTESIAN_POINT('Ctrl Pts',(-0.0246589716878631,1.39664733164099,
-7.50055356277755));
#95003=CARTESIAN_POINT('Ctrl Pts',(-0.119068897208256,1.3815393153964,-7.49964903915524));
#95004=CARTESIAN_POINT('Ctrl Pts',(-0.213439952646206,1.36645690010564,
-7.49696227712133));
#95005=CARTESIAN_POINT('',(-0.778565868050108,1.45719264185526,-7.4594796221293));
#95006=CARTESIAN_POINT('Origin',(0.00109374381087227,1.33929191273629,0.192073141094562));
#95007=CARTESIAN_POINT('Origin',(0.0160466501341866,1.48214300449102,0.192311369972427));
#95008=CARTESIAN_POINT('Origin',(8.81553556769983E-15,4.39277644299907,
-3.33934269125535E-13));
#95009=CARTESIAN_POINT('',(0.346190408897311,4.30202682581797,-7.49200588608201));
#95010=CARTESIAN_POINT('',(-0.22093835419311,4.39169923735679,-7.49674504312255));
#95011=CARTESIAN_POINT('Ctrl Pts',(-0.220938354235514,4.39169923711568,
-7.49674504325896));
#95012=CARTESIAN_POINT('Ctrl Pts',(-0.126423456390729,4.37666099087654,
-7.49953051426805));
#95013=CARTESIAN_POINT('Ctrl Pts',(-0.0318659149821987,4.36166292932587,
-7.50052851196345));
#95014=CARTESIAN_POINT('Ctrl Pts',(0.157228920363726,4.33176393656074,-7.4989476160608));
#95015=CARTESIAN_POINT('Ctrl Pts',(0.251742511016298,4.31686672140778,-7.49637013230712));
#95016=CARTESIAN_POINT('Ctrl Pts',(0.346190410702883,4.30202682552361,-7.49200588624552));
#95017=CARTESIAN_POINT('',(-0.215486073506791,4.21216499623305,-7.49690374429604));
#95018=CARTESIAN_POINT('Ctrl Pts',(0.346190408849771,4.30202682618809,-7.49200588633115));
#95019=CARTESIAN_POINT('Ctrl Pts',(0.252649129683146,4.2871014901393,-7.49632823927246));
#95020=CARTESIAN_POINT('Ctrl Pts',(0.15903942881174,4.27214510978957,-7.49889815186353));
#95021=CARTESIAN_POINT('Ctrl Pts',(-0.0282336964774338,4.24218354883077,
-7.5005314988649));
#95022=CARTESIAN_POINT('Ctrl Pts',(-0.121882317798758,4.22718072995957,
-7.49959422918663));
#95023=CARTESIAN_POINT('Ctrl Pts',(-0.215486073772638,4.21216499386373,
-7.49690374434742));
#95024=CARTESIAN_POINT('',(-0.785187302803463,4.30202682641444,-7.45878548488046));
#95025=CARTESIAN_POINT('Ctrl Pts',(-0.785187302079502,4.30202682552109,
-7.45878548428987));
#95026=CARTESIAN_POINT('Ctrl Pts',(-0.750655784688943,4.29657697961046,
-7.46242062154294));
#95027=CARTESIAN_POINT('Ctrl Pts',(-0.716124358855617,4.29113922035365,
-7.46581327755709));
#95028=CARTESIAN_POINT('Ctrl Pts',(-0.681598060427919,4.28571428571329,
-7.46896405695068));
#95029=CARTESIAN_POINT('Ctrl Pts',(-0.527059766177999,4.26143250098929,
-7.4830668161579));
#95030=CARTESIAN_POINT('Ctrl Pts',(-0.37154166922301,4.23689343090281,-7.49241818475199));
#95031=CARTESIAN_POINT('Ctrl Pts',(-0.215486079999965,4.21216499285671,
-7.49690374416843));
#95032=CARTESIAN_POINT('Origin',(0.0417752178670641,4.16082472928313,0.181485827653811));
#95033=CARTESIAN_POINT('Origin',(-1.196959198424E-13,1.67745375799978,8.90672084696842E-14));
#95034=CARTESIAN_POINT('',(7.49772469075855,1.67637477915458,0.184728058371449));
#95035=CARTESIAN_POINT('',(7.49046336885653,1.58673401543383,-0.378098557106388));
#95036=CARTESIAN_POINT('Ctrl Pts',(7.49046336880353,1.58673401412648,-0.378098559389485));
#95037=CARTESIAN_POINT('Ctrl Pts',(7.49104984295418,1.58859408979895,-0.36647999318996));
#95038=CARTESIAN_POINT('Ctrl Pts',(7.49161452488343,1.59047040833691,-0.354756247142257));
#95039=CARTESIAN_POINT('Ctrl Pts',(7.49269257930982,1.59423866938533,-0.331203385564833));
#95040=CARTESIAN_POINT('Ctrl Pts',(7.49320174293478,1.59611422170125,-0.319476780521802));
#95041=CARTESIAN_POINT('Ctrl Pts',(7.49464630148781,1.60173828677872,-0.284301798040097));
#95042=CARTESIAN_POINT('Ctrl Pts',(7.49549918410855,1.60548553472768,-0.260849964297874));
#95043=CARTESIAN_POINT('Ctrl Pts',(7.49772641398529,1.61671588159084,-0.19052031221021));
#95044=CARTESIAN_POINT('Ctrl Pts',(7.49877119174833,1.6241933649187,-0.143632234283588));
#95045=CARTESIAN_POINT('Ctrl Pts',(7.50058632742757,1.64660512917628,-0.0029156602441874));
#95046=CARTESIAN_POINT('Ctrl Pts',(7.50003602916833,1.66151082526603,0.0909156932702936));
#95047=CARTESIAN_POINT('Ctrl Pts',(7.4977246911644,1.67637478000353,0.18472805824694));
#95048=CARTESIAN_POINT('',(7.46206223280785,1.5867340145509,0.753410392836019));
#95049=CARTESIAN_POINT('Ctrl Pts',(7.46206223337568,1.58673401558742,0.753410394279069));
#95050=CARTESIAN_POINT('Ctrl Pts',(7.46642527039844,1.59355605166272,0.710197223313913));
#95051=CARTESIAN_POINT('Ctrl Pts',(7.47040896742014,1.60035948085492,0.666985156712096));
#95052=CARTESIAN_POINT('Ctrl Pts',(7.47401454883397,1.60714285706879,0.62378403772218));
#95053=CARTESIAN_POINT('Ctrl Pts',(7.48616963301732,1.63001087959054,0.47814503827788));
#95054=CARTESIAN_POINT('Ctrl Pts',(7.494104357436,1.65310706300625,0.331669800426859));
#95055=CARTESIAN_POINT('Ctrl Pts',(7.49772469043156,1.67637477800781,0.18472806265998));
#95056=CARTESIAN_POINT('',(7.49754425839464,1.49654505839769,0.191911677629216));
#95057=CARTESIAN_POINT('Origin',(-0.192404287439453,1.48214578128891,-0.00260234602763698));
#95058=CARTESIAN_POINT('Ctrl Pts',(7.49754425848888,1.4965450582203,0.191911677603393));
#95059=CARTESIAN_POINT('Ctrl Pts',(7.49997612730393,1.51166788439511,0.0969042017717349));
#95060=CARTESIAN_POINT('Ctrl Pts',(7.50060207017734,1.52675096771425,0.00186225802549974));
#95061=CARTESIAN_POINT('Ctrl Pts',(7.49883027565662,1.54931297209943,-0.140733683683761));
#95062=CARTESIAN_POINT('Ctrl Pts',(7.49778716674769,1.55682462514503,-0.188280250890954));
#95063=CARTESIAN_POINT('Ctrl Pts',(7.49554517915627,1.5680672540857,-0.259550299424227));
#95064=CARTESIAN_POINT('Ctrl Pts',(7.49468580826546,1.57180799972993,-0.283281797632825));
#95065=CARTESIAN_POINT('Ctrl Pts',(7.49322802771744,1.57741257213675,-0.318864395530059));
#95066=CARTESIAN_POINT('Ctrl Pts',(7.49271420215881,1.57927897900857,-0.330718414082093));
#95067=CARTESIAN_POINT('Ctrl Pts',(7.4916274518607,1.58301976664233,-0.354486080543136));
#95068=CARTESIAN_POINT('Ctrl Pts',(7.49105747772631,1.58488296741043,-0.366328741600808));
#95069=CARTESIAN_POINT('Ctrl Pts',(7.49046336891913,1.58673401549796,-0.37809855709943));
#95070=CARTESIAN_POINT('Origin',(-1.32718118079324E-13,1.80614392399977,
-8.28330459778925E-13));
#95071=CARTESIAN_POINT('',(0.345447470364996,1.71532338704984,-7.49204017902143));
#95072=CARTESIAN_POINT('',(-0.216253748659272,1.80506741735209,-7.49688163939095));
#95073=CARTESIAN_POINT('Ctrl Pts',(-0.21625374864293,1.80506741777536,-7.49688163946837));
#95074=CARTESIAN_POINT('Ctrl Pts',(-0.122646000119446,1.79006264722948,
-7.49958183236105));
#95075=CARTESIAN_POINT('Ctrl Pts',(-0.0289925193184668,1.7750750069347,
-7.50052867438228));
#95076=CARTESIAN_POINT('Ctrl Pts',(0.15828886644386,1.7451527227798,-7.49891406340871));
#95077=CARTESIAN_POINT('Ctrl Pts',(0.251901963680161,1.73022043511571,-7.49635343127732));
#95078=CARTESIAN_POINT('Ctrl Pts',(0.345447470172254,1.71532338695633,-7.49204017910686));
#95079=CARTESIAN_POINT('',(-0.220230577166923,1.62564958718448,-7.49676586836886));
#95080=CARTESIAN_POINT('Ctrl Pts',(0.345447470364785,1.71532338707357,-7.49204017909798));
#95081=CARTESIAN_POINT('Ctrl Pts',(0.251240613271182,1.70047396625177,-7.49638392522001));
#95082=CARTESIAN_POINT('Ctrl Pts',(0.156967907525142,1.68557177708759,-7.49895005759635));
#95083=CARTESIAN_POINT('Ctrl Pts',(-0.0316419039501056,1.65567252678535,
-7.50052637935151));
#95084=CARTESIAN_POINT('Ctrl Pts',(-0.125958586906449,1.64067867637695,
-7.49953527307687));
#95085=CARTESIAN_POINT('Ctrl Pts',(-0.220230577126277,1.62564958683412,
-7.49676586888631));
#95086=CARTESIAN_POINT('',(-0.785926947266129,1.7153233873478,-7.45870758578964));
#95087=CARTESIAN_POINT('Origin',(0.0444645659943935,1.87485304789864,0.179386017271571));
#95088=CARTESIAN_POINT('Ctrl Pts',(-0.21625375099681,1.80506741660064,-7.49688163879576));
#95089=CARTESIAN_POINT('Ctrl Pts',(-0.333198817477333,1.78658581162692,
-7.4935082618823));
#95090=CARTESIAN_POINT('Ctrl Pts',(-0.44982066598863,1.76822051520783,-7.48740412737111));
#95091=CARTESIAN_POINT('Ctrl Pts',(-0.5659326671137,1.75000000002106,-7.47861753370175));
#95092=CARTESIAN_POINT('Ctrl Pts',(-0.639240188522535,1.73849644467944,
-7.47307010195039));
#95093=CARTESIAN_POINT('Ctrl Pts',(-0.712587645320282,1.72693520694186,
-7.46643537569407));
#95094=CARTESIAN_POINT('Ctrl Pts',(-0.785926945488551,1.71532338729505,
-7.45870758473092));
#95095=CARTESIAN_POINT('Origin',(7.4013735416371E-14,4.134630322,-2.08166817117217E-14));
#95096=CARTESIAN_POINT('',(0.352840846703245,4.04280735915174,-7.49169562495402));
#95097=CARTESIAN_POINT('',(-0.213439952122633,4.13354310263043,-7.49696226262648));
#95098=CARTESIAN_POINT('Ctrl Pts',(-0.213439952646204,4.13354309989436,
-7.49696227712133));
#95099=CARTESIAN_POINT('Ctrl Pts',(-0.119068801382565,4.11846066928871,
-7.49964904188342));
#95100=CARTESIAN_POINT('Ctrl Pts',(-0.0246587799652441,4.10335263767846,
-7.50055356461426));
#95101=CARTESIAN_POINT('Ctrl Pts',(0.164150289677141,4.07309957490726,-7.49879782520741));
#95102=CARTESIAN_POINT('Ctrl Pts',(0.258534175068266,4.05795696825996,-7.4961372422326));
#95103=CARTESIAN_POINT('Ctrl Pts',(0.352840834990003,4.04280736414296,-7.49169562550186));
#95104=CARTESIAN_POINT('',(-0.216060229702239,3.95233946533212,-7.4968872008231));
#95105=CARTESIAN_POINT('Ctrl Pts',(0.352840846647665,4.04280735574477,-7.49169562495281));
#95106=CARTESIAN_POINT('Ctrl Pts',(0.25809657502234,4.02765738641835,-7.49615785228942));
#95107=CARTESIAN_POINT('Ctrl Pts',(0.163270944270159,4.01253622921479,-7.49882263929091));
#95108=CARTESIAN_POINT('Ctrl Pts',(-0.0264122886211297,3.98237240349212,
-7.5005530046766));
#95109=CARTESIAN_POINT('Ctrl Pts',(-0.121254463560225,3.96733216320307,
-7.49961952062042));
#95110=CARTESIAN_POINT('Ctrl Pts',(-0.21606023096172,3.95233946956923,-7.49688721914614));
#95111=CARTESIAN_POINT('',(-0.778565868050654,4.04280735814475,-7.45947962212857));
#95112=CARTESIAN_POINT('Origin',(0.0160466022232138,4.01785667422611,0.192311407730464));
#95113=CARTESIAN_POINT('Origin',(0.00109374380103399,4.16070808729083,0.192073140869918));
#95114=CARTESIAN_POINT('Origin',(1.0321604682062E-12,1.93599222699994,7.12320827322976E-14));
#95115=CARTESIAN_POINT('',(7.49751546373246,1.93490816812523,0.193032549393738));
#95116=CARTESIAN_POINT('',(7.49062612097592,1.84427517280653,-0.374860382219912));
#95117=CARTESIAN_POINT('Ctrl Pts',(7.4906261216132,1.84427517300727,-0.374860382283726));
#95118=CARTESIAN_POINT('Ctrl Pts',(7.49121303530402,1.84614015233912,-0.363132413068011));
#95119=CARTESIAN_POINT('Ctrl Pts',(7.49177591444379,1.84801682086589,-0.351333568492057));
#95120=CARTESIAN_POINT('Ctrl Pts',(7.49284976660165,1.85178766568973,-0.327631235139327));
#95121=CARTESIAN_POINT('Ctrl Pts',(7.49335705074457,1.85366774354606,-0.315816333714424));
#95122=CARTESIAN_POINT('Ctrl Pts',(7.49479553393039,1.85931163604412,-0.280356648675277));
#95123=CARTESIAN_POINT('Ctrl Pts',(7.49564276527711,1.86307720271901,-0.256708875702626));
#95124=CARTESIAN_POINT('Ctrl Pts',(7.4978500074469,1.87438749651835,-0.185712247460573));
#95125=CARTESIAN_POINT('Ctrl Pts',(7.49887334226035,1.8819386651109,-0.138355057832773));
#95126=CARTESIAN_POINT('Ctrl Pts',(7.50059683829672,1.90460873985635,0.0036923073310301));
#95127=CARTESIAN_POINT('Ctrl Pts',(7.49995243135686,1.91974763415408,0.0983798626929981));
#95128=CARTESIAN_POINT('Ctrl Pts',(7.49751548411153,1.93490816308888,0.193032550384539));
#95129=CARTESIAN_POINT('',(7.4617358852843,1.8442751723037,0.75663616261998));
#95130=CARTESIAN_POINT('Origin',(-0.192468731460285,1.87499927803,-0.0145618870896762));
#95131=CARTESIAN_POINT('',(7.49766239512274,1.75423095970248,0.187239441586169));
#95132=CARTESIAN_POINT('Origin',(-0.177845399432686,2.01767772337631,-0.0457629068187224));
#95133=CARTESIAN_POINT('Ctrl Pts',(7.49766239501538,1.75423096138946,0.187239441623221));
#95134=CARTESIAN_POINT('Ctrl Pts',(7.50000203158565,1.76919630156981,0.0935529566687501));
#95135=CARTESIAN_POINT('Ctrl Pts',(7.50058539451906,1.78418803845602,-0.000165562178714458));
#95136=CARTESIAN_POINT('Ctrl Pts',(7.49823961397369,1.814210421049,-0.187579914718305));
#95137=CARTESIAN_POINT('Ctrl Pts',(7.49531020708347,1.82923869541257,-0.281260911311939));
#95138=CARTESIAN_POINT('Ctrl Pts',(7.49062612155154,1.84427517297352,-0.374860382221891));
#95139=CARTESIAN_POINT('Origin',(-2.35922392732846E-13,4.00453392000067,
-1.61275073157219E-14));
#95140=CARTESIAN_POINT('',(7.49754425839464,4.00345494160231,0.191911677629249));
#95141=CARTESIAN_POINT('',(7.49046336898085,3.91326598495459,-0.378098554637036));
#95142=CARTESIAN_POINT('Ctrl Pts',(7.49046336879689,3.91326598412122,-0.378098559520896));
#95143=CARTESIAN_POINT('Ctrl Pts',(7.49105747761129,3.91511703221824,-0.366328743954911));
#95144=CARTESIAN_POINT('Ctrl Pts',(7.49162745175183,3.91698023299548,-0.354486082844943));
#95145=CARTESIAN_POINT('Ctrl Pts',(7.49271420206082,3.92072102064167,-0.330718416303762));
#95146=CARTESIAN_POINT('Ctrl Pts',(7.49322802762509,3.92258742752121,-0.318864397702178));
#95147=CARTESIAN_POINT('Ctrl Pts',(7.49468580818944,3.92819199995176,-0.283281799652642));
#95148=CARTESIAN_POINT('Ctrl Pts',(7.49554517909013,3.93193274561174,-0.259550301343109));
#95149=CARTESIAN_POINT('Ctrl Pts',(7.49778716670837,3.94317537459964,-0.188280252507716));
#95150=CARTESIAN_POINT('Ctrl Pts',(7.49883027563135,3.95068702767696,-0.140733685098229));
#95151=CARTESIAN_POINT('Ctrl Pts',(7.50060207018266,3.97324903215747,0.00186225721714485));
#95152=CARTESIAN_POINT('Ctrl Pts',(7.49997612731427,3.98833211554058,0.0969042013677435));
#95153=CARTESIAN_POINT('Ctrl Pts',(7.49754425848887,4.0034549417797,0.191911677603424));
#95154=CARTESIAN_POINT('',(7.46206223280808,3.91326598544903,0.753410392836296));
#95155=CARTESIAN_POINT('Origin',(-0.192404287971952,4.01785421864167,-0.0026023460724639));
#95156=CARTESIAN_POINT('',(7.49772469113674,3.82362522066483,0.18472805242102));
#95157=CARTESIAN_POINT('Ctrl Pts',(7.49772469126306,3.82362522012807,0.184728050404971));
#95158=CARTESIAN_POINT('Ctrl Pts',(7.49410435803577,3.84689293573233,0.331669792293636));
#95159=CARTESIAN_POINT('Ctrl Pts',(7.48616963408108,3.86998912007418,0.478145035441857));
#95160=CARTESIAN_POINT('Ctrl Pts',(7.47401454883743,3.89285714293126,0.623784037719768));
#95161=CARTESIAN_POINT('Ctrl Pts',(7.47040896720935,3.89964051905595,0.666985156348763));
#95162=CARTESIAN_POINT('Ctrl Pts',(7.46642527039842,3.90644394833732,0.710197223314147));
#95163=CARTESIAN_POINT('Ctrl Pts',(7.46206223337563,3.91326598441267,0.753410394279661));
#95164=CARTESIAN_POINT('Ctrl Pts',(7.49772469130685,3.82362522091266,0.184728052464479));
#95165=CARTESIAN_POINT('Ctrl Pts',(7.50003602919478,3.83848917537128,0.090915689258002));
#95166=CARTESIAN_POINT('Ctrl Pts',(7.50058632740452,3.85339487118032,-0.0029156624840335));
#95167=CARTESIAN_POINT('Ctrl Pts',(7.49877119175063,3.87580663501669,-0.143632233877501));
#95168=CARTESIAN_POINT('Ctrl Pts',(7.49772641401234,3.88328411820511,-0.190520310930482));
#95169=CARTESIAN_POINT('Ctrl Pts',(7.4954991841973,3.89451446485863,-0.260849961708079));
#95170=CARTESIAN_POINT('Ctrl Pts',(7.49464630160125,3.89826171273757,-0.284301795013283));
#95171=CARTESIAN_POINT('Ctrl Pts',(7.49320174309141,3.90388577770994,-0.319476776839918));
#95172=CARTESIAN_POINT('Ctrl Pts',(7.49269257948187,3.9057613299908,-0.331203381664559));
#95173=CARTESIAN_POINT('Ctrl Pts',(7.49161452508621,3.9095295909769,-0.354756242854235));
#95174=CARTESIAN_POINT('Ctrl Pts',(7.491049843174,3.9114059094791,-0.366479988688053));
#95175=CARTESIAN_POINT('Ctrl Pts',(7.49046336904451,3.91326598510923,-0.37809855461549));
#95176=CARTESIAN_POINT('Origin',(4.14511924508249E-14,2.06597317200048,
1.50400525367189E-12));
#95177=CARTESIAN_POINT('',(0.353054365832619,1.97432008473567,-7.49168556575891));
#95178=CARTESIAN_POINT('',(-0.215318823985962,2.06488542583352,-7.49690853987847));
#95179=CARTESIAN_POINT('Ctrl Pts',(-0.21531882455298,2.06488542424203,-7.49690854978191));
#95180=CARTESIAN_POINT('Ctrl Pts',(-0.120597229775604,2.04986689835188,
-7.49962905014707));
#95181=CARTESIAN_POINT('Ctrl Pts',(-0.0258486669508494,2.03480680756073,
-7.5005539179205));
#95182=CARTESIAN_POINT('Ctrl Pts',(0.116255388562765,2.01216376703626,-7.49924848405551));
#95183=CARTESIAN_POINT('Ctrl Pts',(0.163608775699612,2.00460910542996,-7.49836482670986));
#95184=CARTESIAN_POINT('Ctrl Pts',(0.234638059001823,1.9932632677006,-7.49636622501913));
#95185=CARTESIAN_POINT('Ctrl Pts',(0.258323187161593,1.9894775996329,-7.49558741551992));
#95186=CARTESIAN_POINT('Ctrl Pts',(0.29384846706808,1.9837959838051,-7.49425070100337));
#95187=CARTESIAN_POINT('Ctrl Pts',(0.305691842860589,1.98190126977851,-7.49377695059779));
#95188=CARTESIAN_POINT('Ctrl Pts',(0.329478959924526,1.9780946126958,-7.49276895103959));
#95189=CARTESIAN_POINT('Ctrl Pts',(0.341319546987744,1.97619916724463,-7.49223858260928));
#95190=CARTESIAN_POINT('Ctrl Pts',(0.353054369828204,1.97432008410232,-7.49168556547491));
#95191=CARTESIAN_POINT('',(-0.213747920400373,1.88359400911337,-7.49695348562358));
#95192=CARTESIAN_POINT('Ctrl Pts',(0.353054367065202,1.9743200854565,-7.49168556560512));
#95193=CARTESIAN_POINT('Ctrl Pts',(0.341349315939044,1.9724405873732,-7.4922371797086));
#95194=CARTESIAN_POINT('Ctrl Pts',(0.329552974666823,1.97054679727599,-7.49276563402704));
#95195=CARTESIAN_POINT('Ctrl Pts',(0.305841049153146,1.96674083570353,-7.49377080520936));
#95196=CARTESIAN_POINT('Ctrl Pts',(0.294034012727743,1.96484608111116,-7.49424336601566));
#95197=CARTESIAN_POINT('Ctrl Pts',(0.258613729773365,1.95916306904533,-7.49557718010503));
#95198=CARTESIAN_POINT('Ctrl Pts',(0.234997369840539,1.95537543065149,-7.49635475238689));
#95199=CARTESIAN_POINT('Ctrl Pts',(0.164158264868712,1.94401858829907,-7.49835205236256));
#95200=CARTESIAN_POINT('Ctrl Pts',(0.116926694462175,1.93645243803566,-7.49923727598405));
#95201=CARTESIAN_POINT('Ctrl Pts',(-0.0247977080462619,1.91376710880402,
-7.50055422089684));
#95202=CARTESIAN_POINT('Ctrl Pts',(-0.119287039118363,1.89866636706812,
-7.49964670593636));
#95203=CARTESIAN_POINT('Ctrl Pts',(-0.213747921084859,1.88359401243752,
-7.49695350300585));
#95204=CARTESIAN_POINT('',(-0.778353303331698,1.97432008362658,-7.45950173389065));
#95205=CARTESIAN_POINT('Origin',(0.00409925169774547,1.87500219272972,0.192502951085732));
#95206=CARTESIAN_POINT('Origin',(0.0130774175759701,2.01785756222504,0.192617386214208));
#95207=CARTESIAN_POINT('Origin',(-1.68728737038287E-13,3.87542691999814,
-2.61249355482107E-12));
#95208=CARTESIAN_POINT('',(0.345447470705384,3.78467661285328,-7.49204017900575));
#95209=CARTESIAN_POINT('',(-0.22023057716692,3.87435041281552,-7.49676586836886));
#95210=CARTESIAN_POINT('Ctrl Pts',(-0.220230577126272,3.87435041316588,
-7.49676586888631));
#95211=CARTESIAN_POINT('Ctrl Pts',(-0.125958586550348,3.85932132356628,
-7.49953527308733));
#95212=CARTESIAN_POINT('Ctrl Pts',(-0.0316419034223253,3.84432747313072,
-7.5005263793582));
#95213=CARTESIAN_POINT('Ctrl Pts',(0.156967908702848,3.81442822272598,-7.49895005757541));
#95214=CARTESIAN_POINT('Ctrl Pts',(0.251240614743078,3.79952603351569,-7.49638392517439));
#95215=CARTESIAN_POINT('Ctrl Pts',(0.345447472130071,3.78467661264817,-7.4920401790166));
#95216=CARTESIAN_POINT('',(-0.216253753419816,3.69493258269211,-7.49688163925365));
#95217=CARTESIAN_POINT('Ctrl Pts',(0.345447470002635,3.78467661301666,-7.49204017911469));
#95218=CARTESIAN_POINT('Ctrl Pts',(0.251901960340126,3.76977956435237,-7.49635343142922));
#95219=CARTESIAN_POINT('Ctrl Pts',(0.158288859355404,3.75484727608745,-7.49891406345454));
#95220=CARTESIAN_POINT('Ctrl Pts',(-0.0289925200732418,3.72492499294492,
-7.50052867440407));
#95221=CARTESIAN_POINT('Ctrl Pts',(-0.122646002852608,3.70993735233324,
-7.49958183234109));
#95222=CARTESIAN_POINT('Ctrl Pts',(-0.216253753350609,3.69493258147004,
-7.49688163933261));
#95223=CARTESIAN_POINT('',(-0.785926947266576,3.7846766126522,-7.45870758578904));
#95224=CARTESIAN_POINT('Ctrl Pts',(-0.785926945489019,3.78467661270495,
-7.4587075847303));
#95225=CARTESIAN_POINT('Ctrl Pts',(-0.712587645321075,3.77306479305815,
-7.46643537569305));
#95226=CARTESIAN_POINT('Ctrl Pts',(-0.639240188779733,3.76150355535492,
-7.4730701018862));
#95227=CARTESIAN_POINT('Ctrl Pts',(-0.565932667114682,3.74999999997894,
-7.47861753370054));
#95228=CARTESIAN_POINT('Ctrl Pts',(-0.449820668513435,3.73177948519748,
-7.48740412724795));
#95229=CARTESIAN_POINT('Ctrl Pts',(-0.333198823358805,3.71341418928976,
-7.49350826150332));
#95230=CARTESIAN_POINT('Ctrl Pts',(-0.216253759848471,3.69493258476514,
-7.49688163830947));
#95231=CARTESIAN_POINT('Origin',(0.0444645660021557,3.62514695210178,0.179386017273158));
#95232=CARTESIAN_POINT('Origin',(-6.24500451351651E-14,2.19479107900067,
9.90418684565508E-14));
#95233=CARTESIAN_POINT('',(7.4977201549805,2.19371102280125,0.184912079215527));
#95234=CARTESIAN_POINT('',(7.49051254924921,2.10403448601065,-0.37712299467934));
#95235=CARTESIAN_POINT('Ctrl Pts',(7.490512548626,2.104034486,-0.37712300231648));
#95236=CARTESIAN_POINT('Ctrl Pts',(7.49522437558569,2.11903557744126,-0.283535502345184));
#95237=CARTESIAN_POINT('Ctrl Pts',(7.49818204534608,2.13401580726065,-0.18986395636617));
#95238=CARTESIAN_POINT('Ctrl Pts',(7.50058481057828,2.16391559853964,-0.00247117275680855));
#95239=CARTESIAN_POINT('Ctrl Pts',(7.50003045536675,2.17883280263076,0.091235199694861));
#95240=CARTESIAN_POINT('Ctrl Pts',(7.49772015487359,2.19371102268306,0.184912079231655));
#95241=CARTESIAN_POINT('',(7.46196404695618,2.10403448645287,0.754382247112074));
#95242=CARTESIAN_POINT('Ctrl Pts',(7.46196404603328,2.10403448479514,0.7543822497587));
#95243=CARTESIAN_POINT('Ctrl Pts',(7.47026686575195,2.11704095516578,0.672254992309608));
#95244=CARTESIAN_POINT('Ctrl Pts',(7.47720030543364,2.12998516342589,0.590120924256145));
#95245=CARTESIAN_POINT('Ctrl Pts',(7.48277273680961,2.14285714326542,0.508047408556932));
#95246=CARTESIAN_POINT('Ctrl Pts',(7.49006088260498,2.15969232114795,0.400703994567648));
#95247=CARTESIAN_POINT('Ctrl Pts',(7.49505584610473,2.17665108712233,0.292943108994319));
#95248=CARTESIAN_POINT('Ctrl Pts',(7.49772015503783,2.19371102301421,0.184912078878391));
#95249=CARTESIAN_POINT('',(7.49753295098489,2.01370168038256,0.192352916919592));
#95250=CARTESIAN_POINT('Origin',(-0.192711908600478,2.01785800812459,-0.00560467461627225));
#95251=CARTESIAN_POINT('Ctrl Pts',(7.49753295126449,2.0137016812419,0.192352917063813));
#95252=CARTESIAN_POINT('Ctrl Pts',(7.49996803906273,2.02883889136636,0.0974380528380879));
#95253=CARTESIAN_POINT('Ctrl Pts',(7.50060070245807,2.04394235290159,0.00247949131625866));
#95254=CARTESIAN_POINT('Ctrl Pts',(7.49825945640149,2.07406116001761,-0.187395514074732));
#95255=CARTESIAN_POINT('Ctrl Pts',(7.49528675591947,2.08907407473323,-0.282296488362628));
#95256=CARTESIAN_POINT('Ctrl Pts',(7.490512548626,2.104034486,-0.377123002316484));
#95257=CARTESIAN_POINT('Origin',(5.81566045321225E-13,3.74685310400011,
6.96328845278815E-14));
#95258=CARTESIAN_POINT('',(7.49766239511298,3.74576903988833,0.18723944161622));
#95259=CARTESIAN_POINT('',(7.49062612097616,3.65572482719341,-0.374860382220325));
#95260=CARTESIAN_POINT('Ctrl Pts',(7.49062612155167,3.65572482702639,-0.374860382222295));
#95261=CARTESIAN_POINT('Ctrl Pts',(7.49531020708282,3.67076130458482,-0.281260911328065));
#95262=CARTESIAN_POINT('Ctrl Pts',(7.49823961397226,3.68578957894398,-0.187579914762058));
#95263=CARTESIAN_POINT('Ctrl Pts',(7.50058539451876,3.71581196152875,-0.000165562273871897));
#95264=CARTESIAN_POINT('Ctrl Pts',(7.50000203158683,3.73080369841115,0.0935529565497265));
#95265=CARTESIAN_POINT('Ctrl Pts',(7.49766239501894,3.74576903858778,0.187239441480738));
#95266=CARTESIAN_POINT('',(7.4617358794251,3.65572482796968,0.756636166346095));
#95267=CARTESIAN_POINT('Origin',(-0.177843206429112,3.48232181763573,-0.0457629117666998));
#95268=CARTESIAN_POINT('',(7.49751546373715,3.56509183186907,0.19303254812848));
#95269=CARTESIAN_POINT('Origin',(-0.192466710504741,3.62500080527713,-0.0145618519171436));
#95270=CARTESIAN_POINT('Ctrl Pts',(7.49751548414534,3.56509183712149,0.193032549071094));
#95271=CARTESIAN_POINT('Ctrl Pts',(7.49995243849788,3.58025241037405,0.0983795846860867));
#95272=CARTESIAN_POINT('Ctrl Pts',(7.50059684165538,3.59539121607547,0.00369258345655861));
#95273=CARTESIAN_POINT('Ctrl Pts',(7.49887334224948,3.61806133497713,-0.138355058384732));
#95274=CARTESIAN_POINT('Ctrl Pts',(7.49785000743527,3.62561250355198,-0.185712247901861));
#95275=CARTESIAN_POINT('Ctrl Pts',(7.49564276526749,3.63692279732492,-0.25670887597848));
#95276=CARTESIAN_POINT('Ctrl Pts',(7.49479553392196,3.640688363991,-0.280356648895874));
#95277=CARTESIAN_POINT('Ctrl Pts',(7.49335705073873,3.64633225647582,-0.315816333851884));
#95278=CARTESIAN_POINT('Ctrl Pts',(7.49284976659679,3.64821233432779,-0.327631235249468));
#95279=CARTESIAN_POINT('Ctrl Pts',(7.49177591444114,3.65198317914295,-0.351333568547655));
#95280=CARTESIAN_POINT('Ctrl Pts',(7.49121303530262,3.65385984766531,-0.36313241309592));
#95281=CARTESIAN_POINT('Ctrl Pts',(7.49062612161318,3.65572482699279,-0.374860382284109));
#95282=CARTESIAN_POINT('Origin',(7.01313526684356E-14,2.32340998499977,
1.50834206236183E-12));
#95283=CARTESIAN_POINT('',(0.345002061015038,2.23266407489608,-7.49206070239071));
#95284=CARTESIAN_POINT('',(-0.217131941212996,2.32233405333693,-7.4968562557694));
#95285=CARTESIAN_POINT('Ctrl Pts',(-0.217131941025569,2.32233405396696,
-7.49685625580393));
#95286=CARTESIAN_POINT('Ctrl Pts',(-0.123452179549237,2.30733288148859,
-7.49956950889964));
#95287=CARTESIAN_POINT('Ctrl Pts',(-0.0297257413240806,2.29235307873659,
-7.50052672529768));
#95288=CARTESIAN_POINT('Ctrl Pts',(0.110879654202442,2.2699241212905,-7.49932688666955));
#95289=CARTESIAN_POINT('Ctrl Pts',(0.157757857214269,2.26245346441813,-7.4984872311799));
#95290=CARTESIAN_POINT('Ctrl Pts',(0.228038659103193,2.25126411895454,-7.49656900932632));
#95291=CARTESIAN_POINT('Ctrl Pts',(0.251448152483116,2.24753891515717,-7.49582032886621));
#95292=CARTESIAN_POINT('Ctrl Pts',(0.286551146394412,2.24195560118718,-7.49453303715063));
#95293=CARTESIAN_POINT('Ctrl Pts',(0.298247249301271,2.24009572515162,-7.49407670011623));
#95294=CARTESIAN_POINT('Ctrl Pts',(0.321707635570041,2.23636603413695,-7.49310635560389));
#95295=CARTESIAN_POINT('Ctrl Pts',(0.333394495071327,2.23450853328971,-7.49259522007918));
#95296=CARTESIAN_POINT('Ctrl Pts',(0.345002061078998,2.23266407597544,-7.49206070302766));
#95297=CARTESIAN_POINT('',(-0.219224277906958,2.14301213152219,-7.49679536286557));
#95298=CARTESIAN_POINT('Ctrl Pts',(0.345002067217683,2.232664075,-7.49206070274498));
#95299=CARTESIAN_POINT('Ctrl Pts',(0.251036504641597,2.2178090840518,-7.4963877249919));
#95300=CARTESIAN_POINT('Ctrl Pts',(0.15700486422329,2.20290583169153,-7.49894626488442));
#95301=CARTESIAN_POINT('Ctrl Pts',(-0.0311189115788482,2.17301418427561,
-7.50052548339322));
#95302=CARTESIAN_POINT('Ctrl Pts',(-0.125196010903262,2.15802815571166,
-7.49954497514307));
#95303=CARTESIAN_POINT('Ctrl Pts',(-0.219224277787359,2.14301213155917,
-7.49679536308873));
#95304=CARTESIAN_POINT('',(-0.786370364711829,2.23266407449122,-7.45866084596208));
#95305=CARTESIAN_POINT('Origin',(0.0471099633924378,2.41052394526463,0.177110167734925));
#95306=CARTESIAN_POINT('Ctrl Pts',(-0.217131942481557,2.32233405325538,
-7.49685625574591));
#95307=CARTESIAN_POINT('Ctrl Pts',(-0.29496967936998,2.31006874163771,-7.49460183611176));
#95308=CARTESIAN_POINT('Ctrl Pts',(-0.372654673125393,2.2978593648052,-7.49113829054721));
#95309=CARTESIAN_POINT('Ctrl Pts',(-0.450131733931299,2.28571428607735,
-7.4864799085177));
#95310=CARTESIAN_POINT('Ctrl Pts',(-0.562135980734646,2.26815682575238,
-7.47974554609165));
#95311=CARTESIAN_POINT('Ctrl Pts',(-0.674272603922395,2.25046493734972,
-7.47047937137698));
#95312=CARTESIAN_POINT('Ctrl Pts',(-0.786370369442445,2.23266407446841,
-7.45866084752161));
#95313=CARTESIAN_POINT('Origin',(-4.70537863882532E-15,3.61749373599881,
4.70110061989715E-13));
#95314=CARTESIAN_POINT('',(0.353054364847621,3.52567991485733,-7.49168556587659));
#95315=CARTESIAN_POINT('',(-0.213747920400581,3.61640599088661,-7.49695348562358));
#95316=CARTESIAN_POINT('Ctrl Pts',(-0.213747920849145,3.61640598752487,
-7.49695350301259));
#95317=CARTESIAN_POINT('Ctrl Pts',(-0.119290334839949,3.60133415880332,
-7.49964661196808));
#95318=CARTESIAN_POINT('Ctrl Pts',(-0.0247944268889988,3.58623236600729,
-7.50055419025866));
#95319=CARTESIAN_POINT('Ctrl Pts',(0.116926685865832,3.56354756335538,-7.49923727598735));
#95320=CARTESIAN_POINT('Ctrl Pts',(0.164158251379456,3.55598141386297,-7.49835205273171));
#95321=CARTESIAN_POINT('Ctrl Pts',(0.234997367947894,3.54462456965167,-7.49635475244958));
#95322=CARTESIAN_POINT('Ctrl Pts',(0.258613728155951,3.54083693121376,-7.49557718016419));
#95323=CARTESIAN_POINT('Ctrl Pts',(0.294034012069731,3.53515391899408,-7.49424336604505));
#95324=CARTESIAN_POINT('Ctrl Pts',(0.305841049178711,3.53325916429236,-7.49377080520672));
#95325=CARTESIAN_POINT('Ctrl Pts',(0.329549629766121,3.52945373960847,-7.49276577582196));
#95326=CARTESIAN_POINT('Ctrl Pts',(0.341352546817462,3.52755889383967,-7.49223702744892));
#95327=CARTESIAN_POINT('Ctrl Pts',(0.353054366551428,3.52567991462599,-7.49168556562935));
#95328=CARTESIAN_POINT('',(-0.215318825491527,3.43511457396892,-7.49690853966387));
#95329=CARTESIAN_POINT('Ctrl Pts',(0.353054364802041,3.52567991509285,-7.4916855657118));
#95330=CARTESIAN_POINT('Ctrl Pts',(0.341319541914271,3.52380083194171,-7.4922385828405));
#95331=CARTESIAN_POINT('Ctrl Pts',(0.329478954738908,3.52190538647417,-7.49276895126789));
#95332=CARTESIAN_POINT('Ctrl Pts',(0.305691837408766,3.51809872934921,-7.49377695082036));
#95333=CARTESIAN_POINT('Ctrl Pts',(0.293848461509,3.51620401530564,-7.49425070122153));
#95334=CARTESIAN_POINT('Ctrl Pts',(0.258323181276033,3.51052239942619,-7.49558741572346));
#95335=CARTESIAN_POINT('Ctrl Pts',(0.234638052906211,3.50673673132531,-7.49636622521058));
#95336=CARTESIAN_POINT('Ctrl Pts',(0.163608768968816,3.49539089349572,-7.49836482685939));
#95337=CARTESIAN_POINT('Ctrl Pts',(0.11625538140688,3.48783623182252,-7.49924848416912));
#95338=CARTESIAN_POINT('Ctrl Pts',(-0.0258453825439643,3.46519371578282,
-7.50055388765264));
#95339=CARTESIAN_POINT('Ctrl Pts',(-0.120600525541143,3.45013257908954,
-7.49962895551085));
#95340=CARTESIAN_POINT('Ctrl Pts',(-0.215318826251877,3.43511457548861,
-7.49690854973315));
#95341=CARTESIAN_POINT('',(-0.778353303338544,3.52567991637271,-7.45950173388933));
#95342=CARTESIAN_POINT('Origin',(0.0130772088859088,3.48214112196594,0.192617420003678));
#95343=CARTESIAN_POINT('Origin',(0.00409925167992709,3.6249978073121,0.192502950758071));
#95344=CARTESIAN_POINT('Origin',(-1.14925430283463E-13,2.45311202899922,
5.55653613398821E-14));
#95345=CARTESIAN_POINT('',(7.49751856063912,2.45202942596296,0.192913016089072));
#95346=CARTESIAN_POINT('',(7.49059383870815,2.36147458181351,-0.375504899176539));
#95347=CARTESIAN_POINT('Ctrl Pts',(7.49059383965004,2.36147458233101,-0.375504899298271));
#95348=CARTESIAN_POINT('Ctrl Pts',(7.4911823243483,2.36333688481693,-0.363765771889329));
#95349=CARTESIAN_POINT('Ctrl Pts',(7.49174663150587,2.36521061426394,-0.351957688190679));
#95350=CARTESIAN_POINT('Ctrl Pts',(7.49282321345917,2.36897545960216,-0.328238288443623));
#95351=CARTESIAN_POINT('Ctrl Pts',(7.49333186630279,2.37085280695196,-0.316413682529276));
#95352=CARTESIAN_POINT('Ctrl Pts',(7.49477437393667,2.37648893076456,-0.280923509903681));
#95353=CARTESIAN_POINT('Ctrl Pts',(7.49562410848287,2.38024966579896,-0.257254971800962));
#95354=CARTESIAN_POINT('Ctrl Pts',(7.49783844368032,2.39154716307407,-0.186190543045395));
#95355=CARTESIAN_POINT('Ctrl Pts',(7.49886566756327,2.39909119483712,-0.138786406196185));
#95356=CARTESIAN_POINT('Ctrl Pts',(7.50059811512875,2.42174259853615,0.00339777825096544));
#95357=CARTESIAN_POINT('Ctrl Pts',(7.49995628033341,2.43687275373891,0.0981716218080551));
#95358=CARTESIAN_POINT('Ctrl Pts',(7.49751856071574,2.45202942632333,0.192913015950082));
#95359=CARTESIAN_POINT('',(7.46180089043427,2.36147458096339,0.755994147437323));
#95360=CARTESIAN_POINT('Origin',(-0.192710522543249,2.41071411382912,-0.0115878204131166));
#95361=CARTESIAN_POINT('',(7.49768896324805,2.27159573047444,0.186172524012441));
#95362=CARTESIAN_POINT('Ctrl Pts',(7.49768896256665,2.27159573309532,0.186172532960065));
#95363=CARTESIAN_POINT('Ctrl Pts',(7.49694289493809,2.27631121117708,0.216218782605194));
#95364=CARTESIAN_POINT('Ctrl Pts',(7.49601668785442,2.28101755500063,0.246241293301155));
#95365=CARTESIAN_POINT('Ctrl Pts',(7.49491115290311,2.28571428596856,0.276236875889871));
#95366=CARTESIAN_POINT('Ctrl Pts',(7.48932977407838,2.30942609312731,0.42767188314124));
#95367=CARTESIAN_POINT('Ctrl Pts',(7.47913550857591,2.33338323202062,0.579455883520034));
#95368=CARTESIAN_POINT('Ctrl Pts',(7.46427457798021,2.3575225017414,0.731166892692783));
#95369=CARTESIAN_POINT('Ctrl Pts',(7.46346389862386,2.35883932423202,0.739442887421059));
#95370=CARTESIAN_POINT('Ctrl Pts',(7.46263934471632,2.36015668777524,0.747718662273833));
#95371=CARTESIAN_POINT('Ctrl Pts',(7.46180091190877,2.36147458179854,0.755994147902303));
#95372=CARTESIAN_POINT('Ctrl Pts',(7.4976889633641,2.27159572893773,0.186172523881806));
#95373=CARTESIAN_POINT('Ctrl Pts',(7.50001352343751,2.28652496523362,0.0925559791646668));
#95374=CARTESIAN_POINT('Ctrl Pts',(7.5005844224481,2.30148474771429,-0.00109164279741452));
#95375=CARTESIAN_POINT('Ctrl Pts',(7.49821906806474,2.33145198408239,-0.188365088745824));
#95376=CARTESIAN_POINT('Ctrl Pts',(7.49528245577757,2.34645707710048,-0.281976109257676));
#95377=CARTESIAN_POINT('Ctrl Pts',(7.49059383954544,2.361474582,-0.375504901384827));
#95378=CARTESIAN_POINT('Origin',(1.68431523742753E-13,2.58316965299976,
1.28022592527088E-12));
#95379=CARTESIAN_POINT('',(0.353161059393618,2.49144077909165,-7.49168053681783));
#95380=CARTESIAN_POINT('',(-0.214686790752558,2.58208164289175,-7.49692666440967));
#95381=CARTESIAN_POINT('Ctrl Pts',(-0.214686791009888,2.58208164104049,
-7.49692667576293));
#95382=CARTESIAN_POINT('Ctrl Pts',(-0.120052354351971,2.56704149196775,
-7.49963668806582));
#95383=CARTESIAN_POINT('Ctrl Pts',(-0.0253904843322359,2.55196418346729,
-7.50055439644757));
#95384=CARTESIAN_POINT('Ctrl Pts',(0.116586597891132,2.5293015607346,-7.4992430842681));
#95385=CARTESIAN_POINT('Ctrl Pts',(0.16389926048191,2.52174124069315,-7.49835822710871));
#95386=CARTESIAN_POINT('Ctrl Pts',(0.234864949024222,2.51038899728159,-7.4963590470893));
#95387=CARTESIAN_POINT('Ctrl Pts',(0.258527076426483,2.50660176131153,-7.49558031352006));
#95388=CARTESIAN_POINT('Ctrl Pts',(0.294017234894503,2.50091831508106,-7.49424406250517));
#95389=CARTESIAN_POINT('Ctrl Pts',(0.305848454025024,2.49902313294419,-7.49377054115703));
#95390=CARTESIAN_POINT('Ctrl Pts',(0.329609345416721,2.4952159669497,-7.49276319401097));
#95391=CARTESIAN_POINT('Ctrl Pts',(0.341437329052012,2.49332026768562,-7.49223319856089));
#95392=CARTESIAN_POINT('Ctrl Pts',(0.353161059381371,2.49144077728819,-7.49168053684465));
#95393=CARTESIAN_POINT('',(-0.214163364586765,2.40074633135423,-7.49694162681415));
#95394=CARTESIAN_POINT('Ctrl Pts',(0.353161059342393,2.49144078070713,-7.49168053684648));
#95395=CARTESIAN_POINT('Ctrl Pts',(0.341445095676823,2.48956080663179,-7.49223283243877));
#95396=CARTESIAN_POINT('Ctrl Pts',(0.329636241314836,2.4876663623943,-7.49276199369556));
#95397=CARTESIAN_POINT('Ctrl Pts',(0.305898177313054,2.48385907115041,-7.49376849248492));
#95398=CARTESIAN_POINT('Ctrl Pts',(0.294079068303966,2.4819638757106,-7.49424161722381));
#95399=CARTESIAN_POINT('Ctrl Pts',(0.258623899996873,2.47627996468824,-7.49557690117514));
#95400=CARTESIAN_POINT('Ctrl Pts',(0.23498468888381,2.47249207223284,-7.49635522214074));
#95401=CARTESIAN_POINT('Ctrl Pts',(0.164082374314062,2.46113616130948,-7.49835396752701));
#95402=CARTESIAN_POINT('Ctrl Pts',(0.1168103051957,2.45357201211615,-7.49923934606941));
#95403=CARTESIAN_POINT('Ctrl Pts',(-0.0250402834869289,2.43089529097404,
-7.50055449258178));
#95404=CARTESIAN_POINT('Ctrl Pts',(-0.119615788079795,2.41580442945549,
-7.49964256498655));
#95405=CARTESIAN_POINT('Ctrl Pts',(-0.214163365287468,2.40074633459546,
-7.49694164662957));
#95406=CARTESIAN_POINT('',(-0.77824708168631,2.49144077881243,-7.45951282263306));
#95407=CARTESIAN_POINT('Origin',(0.00710118688723879,2.41071461179977,0.192748080607653));
#95408=CARTESIAN_POINT('Origin',(0.0100862188857957,2.55357129378393,0.192647581726705));
#95409=CARTESIAN_POINT('Origin',(-5.2989451611378E-14,3.35806380000116,
-3.57353036051222E-13));
#95410=CARTESIAN_POINT('',(0.345002067680305,3.26733592524982,-7.49206070116328));
#95411=CARTESIAN_POINT('',(-0.219224277907411,3.3569878684778,-7.49679536286556));
#95412=CARTESIAN_POINT('Ctrl Pts',(-0.219224277787808,3.3569878684409,-7.49679536308871));
#95413=CARTESIAN_POINT('Ctrl Pts',(-0.125196017082453,3.34197184527514,
-7.49954497496237));
#95414=CARTESIAN_POINT('Ctrl Pts',(-0.0311189239394535,3.32698581769337,
-7.50052548326445));
#95415=CARTESIAN_POINT('Ctrl Pts',(0.157004851868707,3.29709417026657,-7.49894626522065));
#95416=CARTESIAN_POINT('Ctrl Pts',(0.251036498468413,3.28219091692411,-7.49638772527614));
#95417=CARTESIAN_POINT('Ctrl Pts',(0.345002067217704,3.267335925,-7.49206070274495));
#95418=CARTESIAN_POINT('',(-0.21713193487299,3.17766594634372,-7.49685625595301));
#95419=CARTESIAN_POINT('Ctrl Pts',(0.345002067007358,3.26733592496657,-7.49206070275464));
#95420=CARTESIAN_POINT('Ctrl Pts',(0.333394500515828,3.26549146757557,-7.49259521983764));
#95421=CARTESIAN_POINT('Ctrl Pts',(0.321707640575037,3.26363396665861,-7.49310635538957));
#95422=CARTESIAN_POINT('Ctrl Pts',(0.298247253481625,3.25990427551308,-7.49407669995052));
#95423=CARTESIAN_POINT('Ctrl Pts',(0.286551150129963,3.25804439940689,-7.49453303700846));
#95424=CARTESIAN_POINT('Ctrl Pts',(0.251448154881864,3.25246108522453,-7.4958203287885));
#95425=CARTESIAN_POINT('Ctrl Pts',(0.228038660609242,3.24873588128519,-7.49656900928323));
#95426=CARTESIAN_POINT('Ctrl Pts',(0.157757856048062,3.23754653539625,-7.49848723121556));
#95427=CARTESIAN_POINT('Ctrl Pts',(0.110879651250187,3.23007587823904,-7.49932688672432));
#95428=CARTESIAN_POINT('Ctrl Pts',(-0.0297257424336825,3.20764692108542,
-7.50052672524788));
#95429=CARTESIAN_POINT('Ctrl Pts',(-0.123452177029398,3.19266711891365,
-7.4995695088958));
#95430=CARTESIAN_POINT('Ctrl Pts',(-0.217131934884892,3.17766594701636,
-7.49685625598175));
#95431=CARTESIAN_POINT('',(-0.786370364711874,3.26733592550877,-7.45866084596202));
#95432=CARTESIAN_POINT('Ctrl Pts',(-0.786370365032877,3.26733592483135,
-7.45866084798646));
#95433=CARTESIAN_POINT('Ctrl Pts',(-0.674272603922472,3.24953506265028,
-7.47047937137689));
#95434=CARTESIAN_POINT('Ctrl Pts',(-0.562135980523448,3.23184317427154,
-7.47974554652098));
#95435=CARTESIAN_POINT('Ctrl Pts',(-0.4501317339314,3.21428571392265,-7.48647990851758));
#95436=CARTESIAN_POINT('Ctrl Pts',(-0.372654670650082,3.20214063476731,
-7.49113829040766));
#95437=CARTESIAN_POINT('Ctrl Pts',(-0.294969674111711,3.189931257554,-7.49460183646999));
#95438=CARTESIAN_POINT('Ctrl Pts',(-0.217131934940514,3.17766594555634,
-7.49685625596432));
#95439=CARTESIAN_POINT('Origin',(0.0471099633931913,3.08947605473442,0.177110167732994));
#95440=CARTESIAN_POINT('Origin',(-2.51534904016637E-14,2.71213386199933,
1.21701693861498E-13));
#95441=CARTESIAN_POINT('',(7.49770826960434,2.71105259871213,0.185393371624325));
#95442=CARTESIAN_POINT('',(7.49055600853578,2.6212967969219,-0.376258793102556));
#95443=CARTESIAN_POINT('Ctrl Pts',(7.49055600834388,2.621296797,-0.376258801708933));
#95444=CARTESIAN_POINT('Ctrl Pts',(7.49525383105908,2.63630241371388,-0.282734599734975));
#95445=CARTESIAN_POINT('Ctrl Pts',(7.49819984507317,2.65129140216,-0.18912734946931));
#95446=CARTESIAN_POINT('Ctrl Pts',(7.50058420320881,2.68121760799003,-0.00186233163152409));
#95447=CARTESIAN_POINT('Ctrl Pts',(7.50002300113011,2.69615247103889,0.0917806350178888));
#95448=CARTESIAN_POINT('Ctrl Pts',(7.49770826971422,2.71105259844403,0.185393371669702));
#95449=CARTESIAN_POINT('',(7.4618769614406,2.62129679727526,0.755243144934415));
#95450=CARTESIAN_POINT('Ctrl Pts',(7.4618769610079,2.6212967956465,0.755243148620498));
#95451=CARTESIAN_POINT('Ctrl Pts',(7.47412902591129,2.64052352569905,0.634191540197154));
#95452=CARTESIAN_POINT('Ctrl Pts',(7.48340741224169,2.65962575012096,0.513101823956039));
#95453=CARTESIAN_POINT('Ctrl Pts',(7.48973882790869,2.67857142921234,0.392189105781614));
#95454=CARTESIAN_POINT('Ctrl Pts',(7.49334082608902,2.68934979372956,0.323400789414678));
#95455=CARTESIAN_POINT('Ctrl Pts',(7.49600058062456,2.70017879535254,0.254456008468695));
#95456=CARTESIAN_POINT('Ctrl Pts',(7.4977082697183,2.71105259958609,0.185393367698602));
#95457=CARTESIAN_POINT('',(7.49752438375778,2.53084202102195,0.192686562343836));
#95458=CARTESIAN_POINT('Origin',(-0.192836928120053,2.55357153483116,-0.00860198345926738));
#95459=CARTESIAN_POINT('Ctrl Pts',(7.49752438400009,2.53084202125182,0.192686562386803));
#95460=CARTESIAN_POINT('Ctrl Pts',(7.49996148555515,2.54599092181985,0.0978577995033554));
#95461=CARTESIAN_POINT('Ctrl Pts',(7.50059940836,2.56110926407678,0.0029936701125065));
#95462=CARTESIAN_POINT('Ctrl Pts',(7.49827553106324,2.59126912608015,-0.186706858669859));
#95463=CARTESIAN_POINT('Ctrl Pts',(7.49531483046176,2.60630700020248,-0.281520224309993));
#95464=CARTESIAN_POINT('Ctrl Pts',(7.49055600834388,2.621296797,-0.376258801708936));
#95465=CARTESIAN_POINT('Origin',(-2.92734586571086E-13,3.22948687199989,
-6.29379361127835E-14));
#95466=CARTESIAN_POINT('',(7.49768896323947,3.22840426987216,0.186172524292213));
#95467=CARTESIAN_POINT('',(7.49059383870793,3.1385254181866,-0.375504899172903));
#95468=CARTESIAN_POINT('Ctrl Pts',(7.49059383954544,3.138525418,-0.375504901384827));
#95469=CARTESIAN_POINT('Ctrl Pts',(7.49528245578119,3.15354292291116,-0.281976109185188));
#95470=CARTESIAN_POINT('Ctrl Pts',(7.49821906806929,3.16854801594089,-0.188365088600545));
#95471=CARTESIAN_POINT('Ctrl Pts',(7.50058442244902,3.19851525233201,-0.00109164250782899));
#95472=CARTESIAN_POINT('Ctrl Pts',(7.50001352343393,3.21347503482403,0.092555979525696));
#95473=CARTESIAN_POINT('Ctrl Pts',(7.49768896335334,3.22840427113122,0.186172524314138));
#95474=CARTESIAN_POINT('',(7.4618008792551,3.13852541980614,0.755994151517736));
#95475=CARTESIAN_POINT('Ctrl Pts',(7.46180090019942,3.13852541968788,0.755994148221503));
#95476=CARTESIAN_POINT('Ctrl Pts',(7.4860504720066,3.176642188,0.516646540994622));
#95477=CARTESIAN_POINT('Ctrl Pts',(7.49491115300642,3.214285714,0.276236875994415));
#95478=CARTESIAN_POINT('Ctrl Pts',(7.49657057771863,3.22133557900681,0.231213047961645));
#95479=CARTESIAN_POINT('Ctrl Pts',(7.49768896298581,3.22840426981376,0.186172533427897));
#95480=CARTESIAN_POINT('',(7.49751856071513,3.04797057404127,0.192913013134775));
#95481=CARTESIAN_POINT('Origin',(-0.192706250093664,3.08928601452239,-0.0115877305831265));
#95482=CARTESIAN_POINT('Ctrl Pts',(7.49751856079352,3.04797057416027,0.192913012927193));
#95483=CARTESIAN_POINT('Ctrl Pts',(7.49995628036005,3.06312724666373,0.0981716192870708));
#95484=CARTESIAN_POINT('Ctrl Pts',(7.50059811512331,3.07825740178565,0.00339777623310703));
#95485=CARTESIAN_POINT('Ctrl Pts',(7.49886566753833,3.10090880536359,-0.138786407457143));
#95486=CARTESIAN_POINT('Ctrl Pts',(7.4978384436537,3.10845283708619,-0.186190544052926));
#95487=CARTESIAN_POINT('Ctrl Pts',(7.49562410846093,3.11975033430075,-0.257254972428406));
#95488=CARTESIAN_POINT('Ctrl Pts',(7.49477437391748,3.12351106931505,-0.280923510404845));
#95489=CARTESIAN_POINT('Ctrl Pts',(7.49333186628946,3.12914719309778,-0.316413682842507));
#95490=CARTESIAN_POINT('Ctrl Pts',(7.49282321344814,3.13102454043743,-0.32823828869302));
#95491=CARTESIAN_POINT('Ctrl Pts',(7.49174678273641,3.13478885687642,-0.351954356252219));
#95492=CARTESIAN_POINT('Ctrl Pts',(7.49118216168839,3.13666362993207,-0.363769016638318));
#95493=CARTESIAN_POINT('Ctrl Pts',(7.49059383965076,3.13852541766671,-0.375504899283886));
#95494=CARTESIAN_POINT('Origin',(-2.82179343832881E-14,2.8407150569993,
4.6750797677575E-13));
#95495=CARTESIAN_POINT('',(0.344853648470777,2.75,-7.49206753559307));
#95496=CARTESIAN_POINT('',(-0.21812170991374,2.83963938431667,-7.49682752354381));
#95497=CARTESIAN_POINT('Ctrl Pts',(-0.218121710046857,2.83963938326183,
-7.49682752366668));
#95498=CARTESIAN_POINT('Ctrl Pts',(-0.124301827177169,2.8246344539578,-7.49955723209645));
#95499=CARTESIAN_POINT('Ctrl Pts',(-0.0304342443090152,2.80965517837476,
-7.50052565814021));
#95500=CARTESIAN_POINT('Ctrl Pts',(0.157272188344805,2.77976775476086,-7.49893806965916));
#95501=CARTESIAN_POINT('Ctrl Pts',(0.251096123377212,2.76486196385957,-7.49638311684237));
#95502=CARTESIAN_POINT('Ctrl Pts',(0.344853647954533,2.75000000170506,-7.49206753583365));
#95503=CARTESIAN_POINT('',(-0.218121709913735,2.66036061568333,-7.49682752354381));
#95504=CARTESIAN_POINT('Ctrl Pts',(0.344853648348658,2.74999999835741,-7.49206753581551));
#95505=CARTESIAN_POINT('Ctrl Pts',(0.251096125186365,2.7351380364273,-7.49638311676404));
#95506=CARTESIAN_POINT('Ctrl Pts',(0.157272191176333,2.72023224568898,-7.49893806958205));
#95507=CARTESIAN_POINT('Ctrl Pts',(-0.0304342414766552,2.69034482207722,
-7.50052565816943));
#95508=CARTESIAN_POINT('Ctrl Pts',(-0.124301825761971,2.67536554626854,
-7.49955723213764));
#95509=CARTESIAN_POINT('Ctrl Pts',(-0.218121710046853,2.66036061673817,
-7.49682752366669));
#95510=CARTESIAN_POINT('',(-0.786518123685502,2.75,-7.45864526828673));
#95511=CARTESIAN_POINT('Ctrl Pts',(-0.786518123401192,2.75000000173934,
-7.45864526821688));
#95512=CARTESIAN_POINT('Ctrl Pts',(-0.635720241859938,2.72598918212309,
-7.47454698532651));
#95513=CARTESIAN_POINT('Ctrl Pts',(-0.484816616171727,2.70215892392458,
-7.48583171136412));
#95514=CARTESIAN_POINT('Ctrl Pts',(-0.334222996511701,2.67857142890602,
-7.49254929789627));
#95515=CARTESIAN_POINT('Ctrl Pts',(-0.295567349309514,2.67251679064144,
-7.49427362521657));
#95516=CARTESIAN_POINT('Ctrl Pts',(-0.256864644539784,2.66644617679107,
-7.49570028979618));
#95517=CARTESIAN_POINT('Ctrl Pts',(-0.218121709824728,2.66036061481515,
-7.49682752356268));
#95518=CARTESIAN_POINT('Ctrl Pts',(-0.218121709824731,2.83963938518485,
-7.49682752356268));
#95519=CARTESIAN_POINT('Ctrl Pts',(-0.256864644539786,2.83355382320893,
-7.49570028979618));
#95520=CARTESIAN_POINT('Ctrl Pts',(-0.295567349307819,2.82748320939227,
-7.49427362497814));
#95521=CARTESIAN_POINT('Ctrl Pts',(-0.33422299662364,2.82142857109398,-7.49254929776551));
#95522=CARTESIAN_POINT('Ctrl Pts',(-0.484816616726417,2.7978410759441,-7.48583171165279));
#95523=CARTESIAN_POINT('Ctrl Pts',(-0.635720241859905,2.77401081787673,
-7.4745469853265));
#95524=CARTESIAN_POINT('Ctrl Pts',(-0.786518123401192,2.74999999826065,
-7.45864526821688));
#95525=CARTESIAN_POINT('Origin',(-8.38095573446691E-14,3.100341677,-4.9439619065339E-14));
#95526=CARTESIAN_POINT('',(0.353161049945379,3.00855922064419,-7.49168053798488));
#95527=CARTESIAN_POINT('',(-0.214163364586773,3.09925366864577,-7.49694162681412));
#95528=CARTESIAN_POINT('Ctrl Pts',(-0.214163365287477,3.09925366540454,
-7.49694164662956));
#95529=CARTESIAN_POINT('Ctrl Pts',(-0.119615787895196,3.08419557051511,
-7.49964256499181));
#95530=CARTESIAN_POINT('Ctrl Pts',(-0.0250402831176017,3.06910470896703,
-7.50055449258533));
#95531=CARTESIAN_POINT('Ctrl Pts',(0.11681030494971,3.04642798792313,-7.49923934606818));
#95532=CARTESIAN_POINT('Ctrl Pts',(0.16408237326809,3.03886383885786,-7.49835396754483));
#95533=CARTESIAN_POINT('Ctrl Pts',(0.23498468663855,3.02750792812686,-7.49635522220983));
#95534=CARTESIAN_POINT('Ctrl Pts',(0.25862389735179,3.02372003573565,-7.49557690126512));
#95535=CARTESIAN_POINT('Ctrl Pts',(0.294079065058776,3.01803612480972,-7.49424161735081));
#95536=CARTESIAN_POINT('Ctrl Pts',(0.305898173867865,3.01614092940207,-7.49376849262521));
#95537=CARTESIAN_POINT('Ctrl Pts',(0.329632892545769,3.01233417470685,-7.49276213568984));
#95538=CARTESIAN_POINT('Ctrl Pts',(0.341448322432607,3.01043867559549,-7.49223268032143));
#95539=CARTESIAN_POINT('Ctrl Pts',(0.353161055097876,3.00855921997396,-7.49168053704654));
#95540=CARTESIAN_POINT('',(-0.214686789545212,2.91791835699471,-7.49692666437975));
#95541=CARTESIAN_POINT('Ctrl Pts',(0.353161051407822,3.00855922143352,-7.4916805372205));
#95542=CARTESIAN_POINT('Ctrl Pts',(0.34143732161125,3.00667973111906,-7.49223319889911));
#95543=CARTESIAN_POINT('Ctrl Pts',(0.329609338416344,3.00478403192845,-7.49276319431832));
#95544=CARTESIAN_POINT('Ctrl Pts',(0.305848447833043,3.00097686606387,-7.49377054140901));
#95545=CARTESIAN_POINT('Ctrl Pts',(0.294017229147902,2.99908168399852,-7.49424406272989));
#95546=CARTESIAN_POINT('Ctrl Pts',(0.258527072016622,2.99339823798258,-7.49558031366932));
#95547=CARTESIAN_POINT('Ctrl Pts',(0.234864945505131,2.98961100215531,-7.49635904719672));
#95548=CARTESIAN_POINT('Ctrl Pts',(0.163899259634153,2.97825875917154,-7.49835822711598));
#95549=CARTESIAN_POINT('Ctrl Pts',(0.116586598825047,2.97069843941478,-7.49924308424233));
#95550=CARTESIAN_POINT('Ctrl Pts',(-0.0253904821596797,2.94803581687887,
-7.50055439646177));
#95551=CARTESIAN_POINT('Ctrl Pts',(-0.120062227954501,2.93295693655023,
-7.49963653001752));
#95552=CARTESIAN_POINT('Ctrl Pts',(-0.214696662028744,2.91791679016923,
-7.49692639308361));
#95553=CARTESIAN_POINT('',(-0.778247084124863,3.00855922118781,-7.45951282173075));
#95554=CARTESIAN_POINT('Origin',(0.0100862188859288,2.94642870621689,0.192647581726551));
#95555=CARTESIAN_POINT('Origin',(0.00710118688749452,3.08928538820124,0.192748080609783));
#95556=CARTESIAN_POINT('Origin',(-1.53436291450149E-12,2.97023924200033,
-1.48345962250329E-13));
#95557=CARTESIAN_POINT('',(7.49752438375815,2.96915797897799,0.192686562343938));
#95558=CARTESIAN_POINT('',(7.49055600845813,2.87870320295594,-0.37625879506456));
#95559=CARTESIAN_POINT('Ctrl Pts',(7.49055600834388,2.878703203,-0.376258801708937));
#95560=CARTESIAN_POINT('Ctrl Pts',(7.4953148304482,2.8936929997548,-0.281520224579953));
#95561=CARTESIAN_POINT('Ctrl Pts',(7.49827553104638,2.90873087383415,-0.18670685921018));
#95562=CARTESIAN_POINT('Ctrl Pts',(7.50059940835647,2.93889073574426,0.00299366898818003));
#95563=CARTESIAN_POINT('Ctrl Pts',(7.49996148554706,2.9540090782303,0.0978577998172472));
#95564=CARTESIAN_POINT('Ctrl Pts',(7.49752438400006,2.96915797874819,0.192686562386881));
#95565=CARTESIAN_POINT('',(7.46187696234892,2.87870320365575,0.755243147028956));
#95566=CARTESIAN_POINT('Origin',(-0.192836927089979,2.9464284653058,-0.00860198342095067));
#95567=CARTESIAN_POINT('',(7.49770826960434,2.78894740128786,0.185393371623732));
#95568=CARTESIAN_POINT('Ctrl Pts',(7.4977082697184,2.7889474004133,0.185393367694706));
#95569=CARTESIAN_POINT('Ctrl Pts',(7.49600058062463,2.79982120464723,0.254456008467217));
#95570=CARTESIAN_POINT('Ctrl Pts',(7.49334082631797,2.81065020634723,0.323400789690236));
#95571=CARTESIAN_POINT('Ctrl Pts',(7.48973882790671,2.82142857078767,0.392189105783304));
#95572=CARTESIAN_POINT('Ctrl Pts',(7.48340741183381,2.84037424974404,0.513101823476185));
#95573=CARTESIAN_POINT('Ctrl Pts',(7.47412902590999,2.85947647430091,0.634191540197448));
#95574=CARTESIAN_POINT('Ctrl Pts',(7.46187696100449,2.87870320435315,0.755243148621063));
#95575=CARTESIAN_POINT('Ctrl Pts',(7.49770826971422,2.78894740155606,0.185393371669134));
#95576=CARTESIAN_POINT('Ctrl Pts',(7.50002300113748,2.80384752900865,0.0917806347191898));
#95577=CARTESIAN_POINT('Ctrl Pts',(7.50058420321237,2.81878239210518,-0.0018623322285248));
#95578=CARTESIAN_POINT('Ctrl Pts',(7.49819984505442,2.84870859793545,-0.189127350065385));
#95579=CARTESIAN_POINT('Ctrl Pts',(7.49525383104411,2.86369758633394,-0.282734600033004));
#95580=CARTESIAN_POINT('Ctrl Pts',(7.49055600834388,2.878703203,-0.376258801708931));
#95581=CARTESIAN_POINT('Ctrl Pts',(0.201304349,3.009344995,7.247204741));
#95582=CARTESIAN_POINT('Ctrl Pts',(0.598071101,2.943588707,7.23618382));
#95583=CARTESIAN_POINT('Ctrl Pts',(0.991263374999999,2.878703203,7.181914572));
#95584=CARTESIAN_POINT('Ctrl Pts',(-0.037736949,3.009344995,7.499905061));
#95585=CARTESIAN_POINT('Ctrl Pts',(0.372864527,2.943588707,7.501971067));
#95586=CARTESIAN_POINT('Ctrl Pts',(0.781237513,2.878703203,7.459200222));
#95587=CARTESIAN_POINT('',(0.213503817067261,2.96915797893806,7.49696045860227));
#95588=CARTESIAN_POINT('',(0.781237505398224,2.87870320271434,7.45920022318093));
#95589=CARTESIAN_POINT('Origin',(0.0138847566270039,3.0892087125302,-0.187163919861857));
#95590=CARTESIAN_POINT('',(0.991263371067069,2.8787032034874,7.18191455661634));
#95591=CARTESIAN_POINT('',(0.886250438692909,2.87870320212873,7.32055739764249));
#95592=CARTESIAN_POINT('',(0.20604568399897,3.00855922136916,7.24707150249123));
#95593=CARTESIAN_POINT('Origin',(0.0078833829971733,3.08923052942512,-0.195171233689059));
#95594=CARTESIAN_POINT('Ctrl Pts',(0.213503815207119,2.9691579789368,7.49696045865927));
#95595=CARTESIAN_POINT('Ctrl Pts',(0.212222310116716,2.97541038103787,7.45527257747656));
#95596=CARTESIAN_POINT('Ctrl Pts',(0.210958287707541,2.98181495147342,7.41358339843693));
#95597=CARTESIAN_POINT('Ctrl Pts',(0.20847147405997,2.99493785104416,7.33030086491618));
#95598=CARTESIAN_POINT('Ctrl Pts',(0.207247253797146,3.00166370045464,7.28865974186892));
#95599=CARTESIAN_POINT('Ctrl Pts',(0.206045688483612,3.00855921915399,7.24707150199437));
#95600=CARTESIAN_POINT('Ctrl Pts',(0.961669527891964,2.87421362525411,7.18350692905047));
#95601=CARTESIAN_POINT('Ctrl Pts',(0.975080023200985,2.87645841412705,7.18166062121529));
#95602=CARTESIAN_POINT('Ctrl Pts',(0.988490518509999,2.878703203,7.17981431338));
#95603=CARTESIAN_POINT('Ctrl Pts',(1.37865591428,2.944013165,7.12609777192));
#95604=CARTESIAN_POINT('Ctrl Pts',(1.76070279869,3.00933735,7.03041767896));
#95605=CARTESIAN_POINT('Ctrl Pts',(0.964434538633709,2.87421362525411,7.18561754598276));
#95606=CARTESIAN_POINT('Ctrl Pts',(0.977848956816862,2.87645841412705,7.1837660589914));
#95607=CARTESIAN_POINT('Ctrl Pts',(0.991263375,2.878703203,7.181914572));
#95608=CARTESIAN_POINT('Ctrl Pts',(1.381542903,2.944013165,7.128047348));
#95609=CARTESIAN_POINT('Ctrl Pts',(1.763686919,3.00933735,7.032205092));
#95610=CARTESIAN_POINT('Ctrl Pts',(1.2415009216866,2.87421362525411,7.3971107566939));
#95611=CARTESIAN_POINT('Ctrl Pts',(1.25530842931717,2.87645841412705,7.39474029520778));
#95612=CARTESIAN_POINT('Ctrl Pts',(1.26911593694774,2.878703203,7.39236983372176));
#95613=CARTESIAN_POINT('Ctrl Pts',(1.67083202238253,2.944013165,7.32340354854395));
#95614=CARTESIAN_POINT('Ctrl Pts',(2.06270905602152,3.00933735,7.21131183416782));
#95615=CARTESIAN_POINT('',(1.26854901500601,2.87870320364628,7.39194043595267));
#95616=CARTESIAN_POINT('',(1.82013710546423,2.96915797900293,7.27578867997919));
#95617=CARTESIAN_POINT('Origin',(-0.0433008801937831,2.94642849080139,-0.18810913934697));
#95618=CARTESIAN_POINT('',(1.75913460167935,3.00855922008955,7.033345266035));
#95619=CARTESIAN_POINT('Ctrl Pts',(1.75913460568618,3.00855921928539,7.03334526489348));
#95620=CARTESIAN_POINT('Ctrl Pts',(1.76924832116047,3.00166370059594,7.07370289367572));
#95621=CARTESIAN_POINT('Ctrl Pts',(1.77939553036737,2.99493785113426,7.11410729951582));
#95622=CARTESIAN_POINT('Ctrl Pts',(1.79972748647054,2.98181495154672,7.19490814237825));
#95623=CARTESIAN_POINT('Ctrl Pts',(1.80992389783552,2.97541038112898,7.23535092406372));
#95624=CARTESIAN_POINT('Ctrl Pts',(1.82013710423511,2.9691579790021,7.27578868028949));
#95625=CARTESIAN_POINT('Origin',(-0.0383633275899339,2.9464287300554,-0.19584155044102));
#95626=CARTESIAN_POINT('',(1.12990618766699,2.87870320492457,7.28692750483482));
#95627=CARTESIAN_POINT('Origin',(9.36750677027476E-14,2.970239242,2.02962646689286E-13));
#95628=CARTESIAN_POINT('',(1.8272136544172,2.78894740126616,7.27401472765982));
#95629=CARTESIAN_POINT('Ctrl Pts',(1.8272136579114,2.78894740043443,7.27401472665859));
#95630=CARTESIAN_POINT('Ctrl Pts',(1.76021149589788,2.79982120465073,7.29084549616711));
#95631=CARTESIAN_POINT('Ctrl Pts',(1.69306819303316,2.81065020634441,7.30672737246874));
#95632=CARTESIAN_POINT('Ctrl Pts',(1.62582357463571,2.8214285708981,7.32165949085884));
#95633=CARTESIAN_POINT('Ctrl Pts',(1.50762429158704,2.84037425004919,7.34790643447895));
#95634=CARTESIAN_POINT('Ctrl Pts',(1.3884660660231,2.85947647430085,7.37136117628156));
#95635=CARTESIAN_POINT('Ctrl Pts',(1.26854901542685,2.87870320435315,7.39194043534716));
#95636=CARTESIAN_POINT('',(2.36648016283983,2.87870320271433,7.11686529676572));
#95637=CARTESIAN_POINT('Origin',(-0.0703573075978353,2.9464046053574,-0.177135214929172));
#95638=CARTESIAN_POINT('Origin',(-0.0266746805751597,3.08920866307571,-0.185773302501384));
#95639=CARTESIAN_POINT('Ctrl Pts',(1.754532759,3.009344995,7.034494637));
#95640=CARTESIAN_POINT('Ctrl Pts',(2.139654152,2.943588707,6.938438256));
#95641=CARTESIAN_POINT('Ctrl Pts',(2.511987525,2.878703203,6.800913077));
#95642=CARTESIAN_POINT('Ctrl Pts',(1.575403212,3.009344995,7.332673777));
#95643=CARTESIAN_POINT('Ctrl Pts',(1.976849185,2.943588707,7.2464243));
#95644=CARTESIAN_POINT('Ctrl Pts',(2.36648017,2.878703203,7.116865294));
#95645=CARTESIAN_POINT('',(2.51198751841429,2.8787032034984,6.80091306248545));
#95646=CARTESIAN_POINT('',(2.43923384245511,2.87870320212873,6.95888918726834));
#95647=CARTESIAN_POINT('Origin',(-0.034256928265696,3.08923055943144,-0.192302861328456));
#95648=CARTESIAN_POINT('Ctrl Pts',(2.48342787635727,2.87421362543563,6.80883000765615));
#95649=CARTESIAN_POINT('Ctrl Pts',(2.49612793959364,2.87645841421781,6.80414400555299));
#95650=CARTESIAN_POINT('Ctrl Pts',(2.50882800283,2.878703203,6.79945800345));
#95651=CARTESIAN_POINT('Ctrl Pts',(2.87832407923,2.944013165,6.66312329717));
#95652=CARTESIAN_POINT('Ctrl Pts',(3.23087052879,3.00933735,6.48755136434));
#95653=CARTESIAN_POINT('Ctrl Pts',(2.48658196293872,2.87421362543563,6.81029688395002));
#95654=CARTESIAN_POINT('Ctrl Pts',(2.49928474396936,2.87645841421781,6.80560498047503));
#95655=CARTESIAN_POINT('Ctrl Pts',(2.511987525,2.878703203,6.800913077));
#95656=CARTESIAN_POINT('Ctrl Pts',(2.881562673,2.944013165,6.664406676));
#95657=CARTESIAN_POINT('Ctrl Pts',(3.234169123,3.00933735,6.488655491));
#95658=CARTESIAN_POINT('Ctrl Pts',(2.8026354768333,2.87421362543563,6.95728441748712));
#95659=CARTESIAN_POINT('Ctrl Pts',(2.81561059294661,2.87645841421781,6.95200117027104));
#95660=CARTESIAN_POINT('Ctrl Pts',(2.82858570905992,2.878703203,6.94671792305481));
#95661=CARTESIAN_POINT('Ctrl Pts',(3.20608418331742,2.944013165,6.79300694691974));
#95662=CARTESIAN_POINT('Ctrl Pts',(3.56470294445965,3.00933735,6.59929389665744));
#95663=CARTESIAN_POINT('',(2.82793973365375,2.87870320364628,6.94642043584862));
#95664=CARTESIAN_POINT('',(3.34166280795495,2.96915797895592,6.71440910846434));
#95665=CARTESIAN_POINT('Origin',(-0.0827265550078515,2.94642849629458,-0.174403114624736));
#95666=CARTESIAN_POINT('',(3.22996834025014,3.00855922010428,6.49074762261723));
#95667=CARTESIAN_POINT('Ctrl Pts',(3.22996834425851,3.00855921924352,6.49074762046088));
#95668=CARTESIAN_POINT('Ctrl Pts',(3.24852130392303,3.00166370057168,6.52798756039884));
#95669=CARTESIAN_POINT('Ctrl Pts',(3.26711702995854,2.99493785111864,6.56526598359234));
#95670=CARTESIAN_POINT('Ctrl Pts',(3.30434341445289,2.98181495668542,6.63980694870173));
#95671=CARTESIAN_POINT('Ctrl Pts',(3.32299542485086,2.97541039175451,6.67711223927901));
#95672=CARTESIAN_POINT('Ctrl Pts',(3.34166280629983,2.96915797895513,6.71440910928904));
#95673=CARTESIAN_POINT('Origin',(-0.0795666252702048,2.94642872170379,-0.183016063846523));
#95674=CARTESIAN_POINT('',(2.66996362233808,2.87870320492457,6.87366675883567));
#95675=CARTESIAN_POINT('Origin',(-9.73613550891983E-14,2.97023924200033,
-3.51715184754298E-13));
#95676=CARTESIAN_POINT('',(3.34819256234159,2.78894740128846,6.71115538203976));
#95677=CARTESIAN_POINT('Ctrl Pts',(3.3481925660512,2.78894740039827,6.71115538033786));
#95678=CARTESIAN_POINT('Ctrl Pts',(3.2863749950435,2.79982120464277,6.74199614030772));
#95679=CARTESIAN_POINT('Ctrl Pts',(3.22421559910966,2.81065020634769,6.77194053268262));
#95680=CARTESIAN_POINT('Ctrl Pts',(3.16175308677193,2.82142857082205,6.80097915141608));
#95681=CARTESIAN_POINT('Ctrl Pts',(3.05195955474273,2.84037424983904,6.85202180653093));
#95682=CARTESIAN_POINT('Ctrl Pts',(2.94062925804189,2.8594764743009,6.9005436862566));
#95683=CARTESIAN_POINT('Ctrl Pts',(2.82793973391688,2.87870320435315,6.94642043515864));
#95684=CARTESIAN_POINT('',(3.84106883658366,2.87870320271408,6.44175365830848));
#95685=CARTESIAN_POINT('Origin',(-0.106791214160791,2.94640461889648,-0.15786910551179));
#95686=CARTESIAN_POINT('Origin',(-0.0659866315263863,3.08920870918657,-0.17569542356631));
#95687=CARTESIAN_POINT('Ctrl Pts',(3.225721167,3.009344995,6.492859382));
#95688=CARTESIAN_POINT('Ctrl Pts',(3.581189353,2.943588707,6.31625903));
#95689=CARTESIAN_POINT('Ctrl Pts',(3.91525393,2.878703203,6.101908444));
#95690=CARTESIAN_POINT('Ctrl Pts',(3.114879271,3.009344995,6.822574817));
#95691=CARTESIAN_POINT('Ctrl Pts',(3.488398571,2.943588707,6.652042788));
#95692=CARTESIAN_POINT('Ctrl Pts',(3.841068843,2.878703203,6.441753654));
#95693=CARTESIAN_POINT('',(3.91525392053432,2.87870320349625,6.10190843154593));
#95694=CARTESIAN_POINT('',(3.87816138194936,2.87870320212799,6.27183105181387));
#95695=CARTESIAN_POINT('Origin',(-0.0747953746061175,3.08923058068278,-0.180442555176319));
#95696=CARTESIAN_POINT('Ctrl Pts',(3.88906389553692,2.87421362532651,6.11577976177853));
#95697=CARTESIAN_POINT('Ctrl Pts',(3.90045968671849,2.87645841416325,6.10847317745435));
#95698=CARTESIAN_POINT('Ctrl Pts',(3.9118554779,2.878703203,6.10116659312999));
#95699=CARTESIAN_POINT('Ctrl Pts',(4.24340501024,2.944013165,5.88858858277999));
#95700=CARTESIAN_POINT('Ctrl Pts',(4.5499663445,3.00933735,5.64133435845));
#95701=CARTESIAN_POINT('Ctrl Pts',(3.89245957637044,2.87421362532651,6.11653430794216));
#95702=CARTESIAN_POINT('Ctrl Pts',(3.90385675318525,2.87645841416325,6.10922137597116));
#95703=CARTESIAN_POINT('Ctrl Pts',(3.91525393,2.878703203,6.101908444));
#95704=CARTESIAN_POINT('Ctrl Pts',(4.246843776,2.944013165,5.889145755));
#95705=CARTESIAN_POINT('Ctrl Pts',(4.553425174,3.00933735,5.641703571));
#95706=CARTESIAN_POINT('Ctrl Pts',(4.23272190964473,2.87421362532651,6.19214319192831));
#95707=CARTESIAN_POINT('Ctrl Pts',(4.24425793307692,2.87645841416325,6.1841941974943));
#95708=CARTESIAN_POINT('Ctrl Pts',(4.25579395650913,2.878703203,6.17624520306029));
#95709=CARTESIAN_POINT('Ctrl Pts',(4.59142341067223,2.944013165,5.9449768913485));
#95710=CARTESIAN_POINT('Ctrl Pts',(4.90001528472145,3.00933735,5.6787003118293));
#95711=CARTESIAN_POINT('',(4.25509913271638,2.87870320364628,6.17609353656161));
#95712=CARTESIAN_POINT('',(4.7069360695642,2.96915797893838,5.83907123054069));
#95713=CARTESIAN_POINT('Origin',(-0.11828387119569,2.94642851897792,-0.152541778771623));
#95714=CARTESIAN_POINT('',(4.54977234856429,3.00855922012106,5.64464983369177));
#95715=CARTESIAN_POINT('Ctrl Pts',(4.54977235220724,3.00855921929496,5.64464983057676));
#95716=CARTESIAN_POINT('Ctrl Pts',(4.57589704002969,3.00166370067037,5.67703078343159));
#95717=CARTESIAN_POINT('Ctrl Pts',(4.6020717677554,2.99493785110817,5.70944012703413));
#95718=CARTESIAN_POINT('Ctrl Pts',(4.65445194454172,2.98181495155238,5.77423581901457));
#95719=CARTESIAN_POINT('Ctrl Pts',(4.68068744031158,2.97541038108866,5.80665933175871));
#95720=CARTESIAN_POINT('Ctrl Pts',(4.70693606860236,2.96915797893756,5.83907123131948));
#95721=CARTESIAN_POINT('Origin',(-0.117049403438313,2.9464287394627,-0.161632706015527));
#95722=CARTESIAN_POINT('',(4.08517652503108,2.87870320492457,6.13900099413378));
#95723=CARTESIAN_POINT('Origin',(1.07769695945059E-12,2.97023924199989,
1.36609473733174E-12));
#95724=CARTESIAN_POINT('',(4.71261370775459,2.78894740132767,5.83448986989326));
#95725=CARTESIAN_POINT('Ctrl Pts',(4.71261371106242,2.78894740043244,5.83448986742808));
#95726=CARTESIAN_POINT('Ctrl Pts',(4.6588712522757,2.79982120466691,5.87789853788241));
#95727=CARTESIAN_POINT('Ctrl Pts',(4.60460226762575,2.81065020636038,5.92050527960023));
#95728=CARTESIAN_POINT('Ctrl Pts',(4.5498425389075,2.82142857082138,5.96229258530749));
#95729=CARTESIAN_POINT('Ctrl Pts',(4.45358858163541,2.84037424983719,6.03574425558343));
#95730=CARTESIAN_POINT('Ctrl Pts',(4.35529189432717,2.85947647430089,6.10706444342323));
#95731=CARTESIAN_POINT('Ctrl Pts',(4.25509913278488,2.87870320435315,6.17609353582243));
#95732=CARTESIAN_POINT('',(5.13605340166303,2.87870320271433,5.4654327785827));
#95733=CARTESIAN_POINT('Origin',(-0.138231745003453,2.94640460767842,-0.131221324898843));
#95734=CARTESIAN_POINT('Origin',(-0.102213261567797,3.08920872757977,-0.15740263547115));
#95735=CARTESIAN_POINT('Ctrl Pts',(4.546078438,3.009344995,5.647625239));
#95736=CARTESIAN_POINT('Ctrl Pts',(4.85527212,2.943588707,5.398738552));
#95737=CARTESIAN_POINT('Ctrl Pts',(5.135447414,2.878703203,5.117585355));
#95738=CARTESIAN_POINT('Ctrl Pts',(4.508707036,3.009344995,5.993459841));
#95739=CARTESIAN_POINT('Ctrl Pts',(4.83683431699999,2.943588707,5.746619148));
#95740=CARTESIAN_POINT('Ctrl Pts',(5.136053407,2.878703203,5.465432773));
#95741=CARTESIAN_POINT('',(5.13544740171401,2.87870320347604,5.11758534466438));
#95742=CARTESIAN_POINT('',(5.13575040666388,2.87870320212873,5.2915090677232));
#95743=CARTESIAN_POINT('Origin',(-0.111836554344424,3.08923061262737,-0.160145186282088));
#95744=CARTESIAN_POINT('Ctrl Pts',(5.11285161102639,2.87421362525373,5.13676245265013));
#95745=CARTESIAN_POINT('Ctrl Pts',(5.1224102754232,2.87645841412686,5.12717693379505));
#95746=CARTESIAN_POINT('Ctrl Pts',(5.13196893981999,2.878703203,5.11759141494));
#95747=CARTESIAN_POINT('Ctrl Pts',(5.41006903912,2.944013165,4.83871001114));
#95748=CARTESIAN_POINT('Ctrl Pts',(5.65631079023,3.00933735,4.53133482854));
#95749=CARTESIAN_POINT('Ctrl Pts',(5.11633010784345,2.87421362525373,5.13676938693466));
#95750=CARTESIAN_POINT('Ctrl Pts',(5.12588876092166,2.87645841412686,5.12717737096732));
#95751=CARTESIAN_POINT('Ctrl Pts',(5.135447414,2.878703203,5.117585355));
#95752=CARTESIAN_POINT('Ctrl Pts',(5.413547184,2.944013165,4.838514924));
#95753=CARTESIAN_POINT('Ctrl Pts',(5.65976812400001,3.00933735,4.530951863));
#95754=CARTESIAN_POINT('Ctrl Pts',(5.46489097127091,2.87421362525373,5.13746423310858));
#95755=CARTESIAN_POINT('Ctrl Pts',(5.47444849018795,2.87645841412686,5.12722117757431));
#95756=CARTESIAN_POINT('Ctrl Pts',(5.48400600910502,2.878703203,5.11697812203994));
#95757=CARTESIAN_POINT('Ctrl Pts',(5.76207278177934,2.944013165,4.81896632426267));
#95758=CARTESIAN_POINT('Ctrl Pts',(6.0062083559296,3.00933735,4.49257701135858));
#95759=CARTESIAN_POINT('',(5.4832948306121,2.87870320365809,5.11697936510087));
#95760=CARTESIAN_POINT('',(5.85211823264346,2.9691579789893,4.69070487109329));
#95761=CARTESIAN_POINT('Origin',(-0.14831033925738,2.94642847277019,-0.123547826397968));
#95762=CARTESIAN_POINT('',(5.656834059487,3.00855922008602,4.53461449353195));
#95763=CARTESIAN_POINT('Ctrl Pts',(5.65683406228931,3.00855921918535,4.53461448979404));
#95764=CARTESIAN_POINT('Ctrl Pts',(5.68930891736726,3.00166370050065,4.56062235843146));
#95765=CARTESIAN_POINT('Ctrl Pts',(5.72183874466791,2.9949378510848,4.58664719622671));
#95766=CARTESIAN_POINT('Ctrl Pts',(5.78692346058031,2.98181495152155,4.63866781124971));
#95767=CARTESIAN_POINT('Ctrl Pts',(5.81951568171008,2.97541038109961,4.66469342404267));
#95768=CARTESIAN_POINT('Ctrl Pts',(5.852118231867,2.96915797898848,4.69070487206631));
#95769=CARTESIAN_POINT('Origin',(-0.149059046436379,2.94642874945867,-0.132691610561059));
#95770=CARTESIAN_POINT('',(5.30937111469021,2.87870320492457,5.11728236662172));
#95771=CARTESIAN_POINT('Origin',(-4.69242700251726E-13,2.97023924200033,
-3.59521440396193E-13));
#95772=CARTESIAN_POINT('',(5.85667827404667,2.78894740128657,4.68501009565305));
#95773=CARTESIAN_POINT('Ctrl Pts',(5.85667827417289,2.78894740104823,4.68501009580207));
#95774=CARTESIAN_POINT('Ctrl Pts',(5.81352386782961,2.799821204639,4.73895693236775));
#95775=CARTESIAN_POINT('Ctrl Pts',(5.76968285191742,2.81065020634729,4.79223377956724));
#95776=CARTESIAN_POINT('Ctrl Pts',(5.72518641047971,2.8214285708838,4.84481584443312));
#95777=CARTESIAN_POINT('Ctrl Pts',(5.64697275514493,2.84037424976446,4.93724201088193));
#95778=CARTESIAN_POINT('Ctrl Pts',(5.56630592368743,2.85947647380641,5.02802565260594));
#95779=CARTESIAN_POINT('Ctrl Pts',(5.48329482921344,2.8787032036066,5.11697936380678));
#95780=CARTESIAN_POINT('',(6.19088181798404,2.87870320271433,4.233554336582));
#95781=CARTESIAN_POINT('Origin',(-0.163208569815573,2.94640456450875,-0.0984376413161392));
#95782=CARTESIAN_POINT('Origin',(-0.133660425928305,3.08920869346161,-0.13174977378177));
#95783=CARTESIAN_POINT('Ctrl Pts',(5.653866134,3.009344995,4.538314416));
#95784=CARTESIAN_POINT('Ctrl Pts',(5.902327759,2.943588707,4.22877906));
#95785=CARTESIAN_POINT('Ctrl Pts',(6.115513083,2.878703203,3.893969662));
#95786=CARTESIAN_POINT('Ctrl Pts',(5.691712671,3.009344995,4.884097344));
#95787=CARTESIAN_POINT('Ctrl Pts',(5.959105067,2.943588707,4.572489983));
#95788=CARTESIAN_POINT('Ctrl Pts',(6.19088182200001,2.878703203,4.23355433));
#95789=CARTESIAN_POINT('',(6.11551306924178,2.87870320348678,3.89396965459726));
#95790=CARTESIAN_POINT('',(6.15319744955395,2.87870320212873,4.06376200046081));
#95791=CARTESIAN_POINT('Origin',(-0.143648542792849,3.08923055370613,-0.132359630470066));
#95792=CARTESIAN_POINT('Ctrl Pts',(6.09756806636714,2.87421362525822,3.91755583942908));
#95793=CARTESIAN_POINT('Ctrl Pts',(6.10484265133856,2.87645841412911,3.90613959440954));
#95794=CARTESIAN_POINT('Ctrl Pts',(6.11211723631001,2.878703203,3.89472334939));
#95795=CARTESIAN_POINT('Ctrl Pts',(6.32376425318999,2.944013165,3.56257873745));
#95796=CARTESIAN_POINT('Ctrl Pts',(6.49817243005,3.00933735,3.20945511758));
#95797=CARTESIAN_POINT('Ctrl Pts',(6.10096672854019,2.87421362525822,3.91681483759963));
#95798=CARTESIAN_POINT('Ctrl Pts',(6.10823990577015,2.87645841412911,3.90539224979982));
#95799=CARTESIAN_POINT('Ctrl Pts',(6.115513083,2.878703203,3.893969662));
#95800=CARTESIAN_POINT('Ctrl Pts',(6.32711914299999,2.944013165,3.561640513));
#95801=CARTESIAN_POINT('Ctrl Pts',(6.501466607,3.00933735,3.208337881));
#95802=CARTESIAN_POINT('Ctrl Pts',(6.44152780532348,2.87421362525822,3.84256315617861));
#95803=CARTESIAN_POINT('Ctrl Pts',(6.44865992058245,2.87645841412911,3.83050499356452));
#95804=CARTESIAN_POINT('Ctrl Pts',(6.45579203584133,2.878703203,3.81844683095049));
#95805=CARTESIAN_POINT('Ctrl Pts',(6.66329403417121,2.944013165,3.46762624718633));
#95806=CARTESIAN_POINT('Ctrl Pts',(6.8315577993736,3.00933735,3.09638580299897));
#95807=CARTESIAN_POINT('',(6.45509774771361,2.87870320364628,3.81860093110838));
#95808=CARTESIAN_POINT('',(6.72366185127656,2.96915797897381,3.32300636522837));
#95809=CARTESIAN_POINT('Origin',(-0.171402023084778,2.94642845415883,-0.0887769886318324));
#95810=CARTESIAN_POINT('',(6.49938849676149,3.00855922009366,3.21254561858901));
#95811=CARTESIAN_POINT('Ctrl Pts',(6.49938849887401,3.00855921919985,3.21254561397554));
#95812=CARTESIAN_POINT('Ctrl Pts',(6.53669503270114,3.00166370052502,3.23096429927456));
#95813=CARTESIAN_POINT('Ctrl Pts',(6.57405890158005,2.99493785108369,3.2493877396616));
#95814=CARTESIAN_POINT('Ctrl Pts',(6.64880486723471,2.98181495152726,3.28620085165117));
#95815=CARTESIAN_POINT('Ctrl Pts',(6.68622983778637,2.97541038108343,3.30461163604335));
#95816=CARTESIAN_POINT('Ctrl Pts',(6.72366185073906,2.96915797897302,3.32300636632187));
#95817=CARTESIAN_POINT('Origin',(-0.174099247004787,2.94642876633121,-0.097546256532349));
#95818=CARTESIAN_POINT('',(6.2853054112379,2.87870320492457,3.85628530270651));
#95819=CARTESIAN_POINT('Origin',(-1.57426155444895E-13,2.970239242001,-3.53449908230274E-14));
#95820=CARTESIAN_POINT('',(6.72689107318561,2.78894740126561,3.31646445626045));
#95821=CARTESIAN_POINT('Ctrl Pts',(6.72689107500255,2.78894740038621,3.31646445271653));
#95822=CARTESIAN_POINT('Ctrl Pts',(6.69634256802001,2.79982120463123,3.37842696767838));
#95823=CARTESIAN_POINT('Ctrl Pts',(6.66497947801158,2.81065020634044,3.43988275429206));
#95824=CARTESIAN_POINT('Ctrl Pts',(6.63282692833449,2.82142857086638,3.50080089926231));
#95825=CARTESIAN_POINT('Ctrl Pts',(6.57631075775242,2.84037424996154,3.60787981825588));
#95826=CARTESIAN_POINT('Ctrl Pts',(6.51704567080299,2.85947647430086,3.71388197465343));
#95827=CARTESIAN_POINT('Ctrl Pts',(6.45509774747662,2.87870320435315,3.81860093040627));
#95828=CARTESIAN_POINT('',(6.9562314805007,2.87870320271433,2.80371959930828));
#95829=CARTESIAN_POINT('Origin',(-0.18055420657661,2.94640463077747,-0.0610512711219108));
#95830=CARTESIAN_POINT('Origin',(-0.158857905135916,3.08920872516404,-0.0999365369811978));
#95831=CARTESIAN_POINT('Ctrl Pts',(6.497285334,3.009344995,3.216797055));
#95832=CARTESIAN_POINT('Ctrl Pts',(6.673397112,2.943588707,2.861086559));
#95833=CARTESIAN_POINT('Ctrl Pts',(6.809624158,2.878703203,2.488276275));
#95834=CARTESIAN_POINT('Ctrl Pts',(6.608580148,3.009344995,3.546359884));
#95835=CARTESIAN_POINT('Ctrl Pts',(6.802734686,2.943588707,3.184556269));
#95836=CARTESIAN_POINT('Ctrl Pts',(6.956231483,2.878703203,2.803719592));
#95837=CARTESIAN_POINT('',(6.80962414281031,2.87870320347874,2.48827627106145));
#95838=CARTESIAN_POINT('',(6.88292781858177,2.87870320212873,2.64599793848983));
#95839=CARTESIAN_POINT('Origin',(-0.168743259941024,3.08923062687531,-0.098384840025989));
#95840=CARTESIAN_POINT('Ctrl Pts',(6.79716901704737,2.87421362534792,2.51516866831626));
#95841=CARTESIAN_POINT('Ctrl Pts',(6.80181937093871,2.87645841417397,2.5024555082831));
#95842=CARTESIAN_POINT('Ctrl Pts',(6.80646972483,2.878703203,2.48974234825));
#95843=CARTESIAN_POINT('Ctrl Pts',(6.94176727817,2.944013165,2.11986524042));
#95844=CARTESIAN_POINT('Ctrl Pts',(7.03618674890999,3.00933735,1.73750485288));
#95845=CARTESIAN_POINT('Ctrl Pts',(6.80032892689619,2.87421362534792,2.51371437879972));
#95846=CARTESIAN_POINT('Ctrl Pts',(6.80497654244815,2.87645841417397,2.50099532689983));
#95847=CARTESIAN_POINT('Ctrl Pts',(6.809624158,2.878703203,2.488276275));
#95848=CARTESIAN_POINT('Ctrl Pts',(6.944842042,2.944013165,2.118227749));
#95849=CARTESIAN_POINT('Ctrl Pts',(7.039163737,3.00933735,1.735705586));
#95850=CARTESIAN_POINT('Ctrl Pts',(7.11696595811632,2.87421362534792,2.36798809638245));
#95851=CARTESIAN_POINT('Ctrl Pts',(7.12133917986923,2.87645841417397,2.35467865321177));
#95852=CARTESIAN_POINT('Ctrl Pts',(7.12571240162204,2.878703203,2.34136921004108));
#95853=CARTESIAN_POINT('Ctrl Pts',(7.25294706315576,2.944013165,1.95414382044622));
#95854=CARTESIAN_POINT('Ctrl Pts',(7.33747119382016,3.00933735,1.55541103631185));
#95855=CARTESIAN_POINT('',(7.12506747388459,2.87870320365548,2.34166895685243));
#95856=CARTESIAN_POINT('',(7.28081451506283,2.96915797898314,1.79992777426841));
#95857=CARTESIAN_POINT('Origin',(-0.186479305376558,2.9464284651642,-0.0498551048602675));
#95858=CARTESIAN_POINT('',(7.03803875113726,3.00855922007997,1.74026168046718));
#95859=CARTESIAN_POINT('Ctrl Pts',(7.03803875201502,3.00855921921256,1.74026167631026));
#95860=CARTESIAN_POINT('Ctrl Pts',(7.07843255283472,3.0016637005282,1.7502299408843));
#95861=CARTESIAN_POINT('Ctrl Pts',(7.118883370277,2.99493785110666,1.76019052401283));
#95862=CARTESIAN_POINT('Ctrl Pts',(7.19979551660409,2.98181495661769,1.78007478494072));
#95863=CARTESIAN_POINT('Ctrl Pts',(7.24030324971683,2.97541039162867,1.79000986396595));
#95864=CARTESIAN_POINT('Ctrl Pts',(7.28081451460902,2.9691579789846,1.79992777604475));
#95865=CARTESIAN_POINT('Origin',(-0.190998271341551,2.94642869800802,-0.0578394435499486));
#95866=CARTESIAN_POINT('',(6.96734581257855,2.87870320492449,2.41497262381362));
#95867=CARTESIAN_POINT('Origin',(-1.09547787507935E-12,2.97023924200033,
-1.85181731060524E-13));
#95868=CARTESIAN_POINT('',(7.28256192199601,2.78894740128747,1.79284462519746));
#95869=CARTESIAN_POINT('Ctrl Pts',(7.28256192321671,2.78894740038391,1.79284462117268));
#95870=CARTESIAN_POINT('Ctrl Pts',(7.26604773257175,2.79982120463769,1.8599255130922));
#95871=CARTESIAN_POINT('Ctrl Pts',(7.24862907170715,2.81065020634741,1.92668663488117));
#95872=CARTESIAN_POINT('Ctrl Pts',(7.23032383120981,2.82142857087646,1.99309239523889));
#95873=CARTESIAN_POINT('Ctrl Pts',(7.19814777979972,2.84037424998939,2.10981717482112));
#95874=CARTESIAN_POINT('Ctrl Pts',(7.16305560768842,2.85947647430068,2.22608130136318));
#95875=CARTESIAN_POINT('Ctrl Pts',(7.12506747217466,2.87870320435307,2.34166895820505));
#95876=CARTESIAN_POINT('',(7.39631549110475,2.87870320271433,1.24278604964134));
#95877=CARTESIAN_POINT('Origin',(-0.189457228805128,2.94640462537924,-0.0208101341724251));
#95878=CARTESIAN_POINT('Origin',(-0.17662714545213,3.08920871805869,-0.0634502948560189));
#95879=CARTESIAN_POINT('Ctrl Pts',(7.036898692,3.009344995,1.744865839));
#95880=CARTESIAN_POINT('Ctrl Pts',(7.132425833,2.943588707,1.35961283));
#95881=CARTESIAN_POINT('Ctrl Pts',(7.185324776,2.878703203,0.966233856));
#95882=CARTESIAN_POINT('Ctrl Pts',(7.216437762,3.009344995,2.042798577));
#95883=CARTESIAN_POINT('Ctrl Pts',(7.328275993,2.943588707,1.647716243));
#95884=CARTESIAN_POINT('Ctrl Pts',(7.396315492,2.878703203,1.242786042));
#95885=CARTESIAN_POINT('',(7.18532476004359,2.8787032034815,0.96623385508769));
#95886=CARTESIAN_POINT('',(7.29082013319928,2.87870320212873,1.10450995428553));
#95887=CARTESIAN_POINT('Origin',(-0.185948094727437,3.08923058801028,-0.0598098675866138));
#95888=CARTESIAN_POINT('Ctrl Pts',(7.17894189898616,2.87421362534608,0.995175007239506));
#95889=CARTESIAN_POINT('Ctrl Pts',(7.18075057656315,2.87645841417304,0.981759385199748));
#95890=CARTESIAN_POINT('Ctrl Pts',(7.18255925414001,2.878703203,0.968343763159999));
#95891=CARTESIAN_POINT('Ctrl Pts',(7.23518098069,2.944013165,0.57802920212));
#95892=CARTESIAN_POINT('Ctrl Pts',(7.24519679643001,3.00933735,0.18431079146));
#95893=CARTESIAN_POINT('Ctrl Pts',(7.1817153026374,2.87421362534608,0.993075430992086));
#95894=CARTESIAN_POINT('Ctrl Pts',(7.18352003931876,2.87645841417304,0.979654643496043));
#95895=CARTESIAN_POINT('Ctrl Pts',(7.185324776,2.878703203,0.966233856));
#95896=CARTESIAN_POINT('Ctrl Pts',(7.237831846,2.944013165,0.575769010999999));
#95897=CARTESIAN_POINT('Ctrl Pts',(7.247717395,3.00933735,0.181913626));
#95898=CARTESIAN_POINT('Ctrl Pts',(7.45962269256269,2.87421362534609,0.782688546049605));
#95899=CARTESIAN_POINT('Ctrl Pts',(7.46103253396369,2.87645841417304,0.768750156842104));
#95900=CARTESIAN_POINT('Ctrl Pts',(7.4624423753646,2.878703203,0.754811767634591));
#95901=CARTESIAN_POINT('Ctrl Pts',(7.50346034873261,2.944013165,0.349287800947444));
#95902=CARTESIAN_POINT('Ctrl Pts',(7.50029259058361,3.00933735,-0.0582930225762464));
#95903=CARTESIAN_POINT('',(7.24759813578533,3.00855922012093,0.186605041169535));
#95904=CARTESIAN_POINT('Ctrl Pts',(7.24759813575441,3.00855921921561,0.186605036456814));
#95905=CARTESIAN_POINT('Ctrl Pts',(7.28919043403294,3.00166370056477,0.187656775431321));
#95906=CARTESIAN_POINT('Ctrl Pts',(7.33083676504322,2.9949378511043,0.188688755670289));
#95907=CARTESIAN_POINT('Ctrl Pts',(7.41413179084453,2.98181495154648,0.190714414764441));
#95908=CARTESIAN_POINT('Ctrl Pts',(7.45582826192075,2.97541038110894,0.191709252839048));
#95909=CARTESIAN_POINT('Ctrl Pts',(7.49752438372885,2.96915797897716,0.192686563589115));
#95910=CARTESIAN_POINT('Origin',(-0.198966747437768,2.94642872685435,-0.0154282146167841));
#95911=CARTESIAN_POINT('',(7.32360086760227,2.87870320492457,0.860738509892561));
#95912=CARTESIAN_POINT('Ctrl Pts',(7.247474489,3.009344995,0.191346636));
#95913=CARTESIAN_POINT('Ctrl Pts',(7.25795025,2.943588707,-0.205434883));
#95914=CARTESIAN_POINT('Ctrl Pts',(7.22504759300001,2.878703203,-0.600988585));
#95915=CARTESIAN_POINT('Ctrl Pts',(7.486862767,3.009344995,0.443718279));
#95916=CARTESIAN_POINT('Ctrl Pts',(7.511155258,2.943588707,0.033830836));
#95917=CARTESIAN_POINT('Ctrl Pts',(7.490556008,2.878703203,-0.376258802));
#95918=CARTESIAN_POINT('',(7.22504757715887,2.87870320349508,-0.600988582157999));
#95919=CARTESIAN_POINT('',(7.35780180085423,2.87870320212873,-0.488623688165908));
#95920=CARTESIAN_POINT('Origin',(-0.194458153582505,3.08923057649802,-0.0184381958679822));
#95921=CARTESIAN_POINT('Ctrl Pts',(7.22503543617682,2.87421362527074,-0.571351931454881));
#95922=CARTESIAN_POINT('Ctrl Pts',(7.22391786567334,2.87645841413537,-0.58484271615244));
#95923=CARTESIAN_POINT('Ctrl Pts',(7.22280029517,2.878703203,-0.59833350085));
#95924=CARTESIAN_POINT('Ctrl Pts',(7.19028566172,2.944013165,-0.99083484021));
#95925=CARTESIAN_POINT('Ctrl Pts',(7.11542949334,3.00933735,-1.37750143675));
#95926=CARTESIAN_POINT('Ctrl Pts',(7.22729265236689,2.87421362527074,-0.573998620574956));
#95927=CARTESIAN_POINT('Ctrl Pts',(7.22617012268338,2.87645841413537,-0.587493602787484));
#95928=CARTESIAN_POINT('Ctrl Pts',(7.22504759300001,2.878703203,-0.600988584999999));
#95929=CARTESIAN_POINT('Ctrl Pts',(7.192388677,2.944013165,-0.993612047));
#95930=CARTESIAN_POINT('Ctrl Pts',(7.117375842,3.00933735,-1.380384412));
#95931=CARTESIAN_POINT('Ctrl Pts',(7.45347576121302,2.87421362527074,-0.839208650499396));
#95932=CARTESIAN_POINT('Ctrl Pts',(7.4518562996145,2.87645841413536,-0.853124242393329));
#95933=CARTESIAN_POINT('Ctrl Pts',(7.45023683801584,2.878703203,-0.86703983428725));
#95934=CARTESIAN_POINT('Ctrl Pts',(7.40312016832172,2.944013165,-1.2719005283683));
#95935=CARTESIAN_POINT('Ctrl Pts',(7.31240864069362,3.00933735,-1.66927136382287));
#95936=CARTESIAN_POINT('',(7.44977737784609,2.87870320365574,-0.86649699318621));
#95937=CARTESIAN_POINT('',(7.36365834535818,2.96915797897503,-1.42356445975563));
#95938=CARTESIAN_POINT('Origin',(-0.190177538421263,2.9464284868015,0.0330533512148072));
#95939=CARTESIAN_POINT('',(7.11826788656465,3.00855922009091,-1.37577704263269));
#95940=CARTESIAN_POINT('Ctrl Pts',(7.11826788559849,3.00855921919469,-1.37577704683838));
#95941=CARTESIAN_POINT('Ctrl Pts',(7.15911387198548,3.00166370052759,-1.38369101187184));
#95942=CARTESIAN_POINT('Ctrl Pts',(7.20000837997906,2.99493785110683,-1.3916358889752));
#95943=CARTESIAN_POINT('Ctrl Pts',(7.28179147137155,2.98181495153996,-1.40756355721969));
#95944=CARTESIAN_POINT('Ctrl Pts',(7.32272696298951,2.97541038109973,-1.41555548667772));
#95945=CARTESIAN_POINT('Ctrl Pts',(7.36365834559492,2.96915797897421,-1.4235644585451));
#95946=CARTESIAN_POINT('Origin',(-0.197631358334211,2.94642873841696,0.0277044275786476));
#95947=CARTESIAN_POINT('',(7.33741248569151,2.87870320492457,-0.733742780585012));
#95948=CARTESIAN_POINT('Origin',(-1.99926880606327E-13,2.97023924200056,
6.41847686111419E-14));
#95949=CARTESIAN_POINT('',(7.36227011168011,2.78894740127468,-1.43072666945416));
#95950=CARTESIAN_POINT('Ctrl Pts',(7.36227011098476,2.78894740039408,-1.43072667338475));
#95951=CARTESIAN_POINT('Ctrl Pts',(7.37544877285625,2.79982120463674,-1.36291157598455));
#95952=CARTESIAN_POINT('Ctrl Pts',(7.38767229193052,2.81065020634305,-1.29500691682899));
#95953=CARTESIAN_POINT('Ctrl Pts',(7.39894196063855,2.82142857078376,-1.22705251018671));
#95954=CARTESIAN_POINT('Ctrl Pts',(7.41875122933032,2.84037424973322,-1.10760559749431));
#95955=CARTESIAN_POINT('Ctrl Pts',(7.43572047689678,2.85947647430088,-0.987352312321885));
#95956=CARTESIAN_POINT('Ctrl Pts',(7.44977737688105,2.87870320435315,-0.866496991366489));
#95957=CARTESIAN_POINT('',(7.23454645341812,2.87870320271433,-1.97771019567721));
#95958=CARTESIAN_POINT('Origin',(-0.180684634096219,2.94640460378407,0.0606642555156378));
#95959=CARTESIAN_POINT('Origin',(-0.186944872367999,3.08920871784849,0.016577968539003));
#95960=CARTESIAN_POINT('Ctrl Pts',(7.119166433,3.009344995,-1.371119723));
#95961=CARTESIAN_POINT('Ctrl Pts',(7.044100979,2.943588707,-1.76087669));
#95962=CARTESIAN_POINT('Ctrl Pts',(6.926935215,2.878703203,-2.140109468));
#95963=CARTESIAN_POINT('Ctrl Pts',(7.40721039,3.009344995,-1.176109793));
#95964=CARTESIAN_POINT('Ctrl Pts',(7.342821252,2.943588707,-1.581636462));
#95965=CARTESIAN_POINT('Ctrl Pts',(7.234546451,2.878703203,-1.977710203));
#95966=CARTESIAN_POINT('',(6.92693520013569,2.87870320350798,-2.1401094613818));
#95967=CARTESIAN_POINT('',(7.08074083449266,2.8787032021287,-2.05890983036663));
#95968=CARTESIAN_POINT('Origin',(-0.193875393915119,3.08923059316947,0.0237955986485733));
#95969=CARTESIAN_POINT('Ctrl Pts',(6.93329434686559,2.87421362526316,-2.11116308955185));
#95970=CARTESIAN_POINT('Ctrl Pts',(6.92930278461267,2.87645841413158,-2.12409822259592));
#95971=CARTESIAN_POINT('Ctrl Pts',(6.92531122236,2.878703203,-2.13703335564));
#95972=CARTESIAN_POINT('Ctrl Pts',(6.80918057741999,2.944013165,-2.51336854665));
#95973=CARTESIAN_POINT('Ctrl Pts',(6.65295261534001,3.00933735,-2.87490322868));
#95974=CARTESIAN_POINT('Ctrl Pts',(6.93492983066302,2.87421362526316,-2.11423313530778));
#95975=CARTESIAN_POINT('Ctrl Pts',(6.93093252283145,2.87645841413158,-2.12717130165389));
#95976=CARTESIAN_POINT('Ctrl Pts',(6.926935215,2.878703203,-2.140109468));
#95977=CARTESIAN_POINT('Ctrl Pts',(6.810637408,2.944013165,-2.51653291));
#95978=CARTESIAN_POINT('Ctrl Pts',(6.654233705,3.00933735,-2.878137209));
#95979=CARTESIAN_POINT('Ctrl Pts',(7.0988125865179,2.87421362526317,-2.42186538445608));
#95980=CARTESIAN_POINT('Ctrl Pts',(7.09423954612034,2.87645841413158,-2.4351075011659));
#95981=CARTESIAN_POINT('Ctrl Pts',(7.08966650572267,2.878703203,-2.44834961787577));
#95982=CARTESIAN_POINT('Ctrl Pts',(6.95661831629257,2.944013165,-2.83361620186825));
#95983=CARTESIAN_POINT('Ctrl Pts',(6.782604590907,3.00933735,-3.20219643111895));
#95984=CARTESIAN_POINT('',(7.08933448239759,2.87870320364628,-2.44772069546989));
#95985=CARTESIAN_POINT('',(6.88547582676876,2.96915797900449,-2.97325118946044));
#95986=CARTESIAN_POINT('Origin',(-0.178625803362676,2.94642847631061,0.0731631295020271));
#95987=CARTESIAN_POINT('',(6.65609534290466,3.00855922007134,-2.87382932098887));
#95988=CARTESIAN_POINT('Ctrl Pts',(6.65609534087897,3.00855921916919,-2.87382932529785));
#95989=CARTESIAN_POINT('Ctrl Pts',(6.69428510228388,3.00166370051113,-2.89033894558407));
#95990=CARTESIAN_POINT('Ctrl Pts',(6.73251560584482,2.99493785107109,-2.90688918613176));
#95991=CARTESIAN_POINT('Ctrl Pts',(6.80896267611153,2.98181495152546,-2.94002542125667));
#95992=CARTESIAN_POINT('Ctrl Pts',(6.84722308990285,2.97541038112037,-2.95663042439218));
#95993=CARTESIAN_POINT('Ctrl Pts',(6.88547582727347,2.96915797900365,-2.97325118829854));
#95994=CARTESIAN_POINT('Origin',(-0.187055439915118,2.94642874800422,0.0695416967131169));
#95995=CARTESIAN_POINT('',(7.00813485072502,2.87870320492457,-2.29391507461971));
#95996=CARTESIAN_POINT('Origin',(5.37330596683816E-13,2.97023924200022,
-1.88434337577981E-13));
#95997=CARTESIAN_POINT('',(6.88258038540432,2.78894740126419,-2.97994752197196));
#95998=CARTESIAN_POINT('Ctrl Pts',(6.88258038384381,2.78894740041576,-2.97994752537121));
#95999=CARTESIAN_POINT('Ctrl Pts',(6.91002917723491,2.79982120464213,-2.91655093023161));
#96000=CARTESIAN_POINT('Ctrl Pts',(6.93656441164617,2.81065020634171,-2.8528615397131));
#96001=CARTESIAN_POINT('Ctrl Pts',(6.96217879061306,2.82142857083718,-2.78891851496595));
#96002=CARTESIAN_POINT('Ctrl Pts',(7.00720248597009,2.84037424988088,-2.67652261174883));
#96003=CARTESIAN_POINT('Ctrl Pts',(7.04962590309075,2.85947647430089,-2.56272866850826));
#96004=CARTESIAN_POINT('Ctrl Pts',(7.0893344817164,2.87870320435315,-2.44772069575774));
#96005=CARTESIAN_POINT('',(6.64025754595189,2.87870320271433,-3.4866860663639));
#96006=CARTESIAN_POINT('Origin',(-0.163419285037631,2.94640460318537,0.0980878044349803));
#96007=CARTESIAN_POINT('Origin',(-0.179010304998681,3.08920866068137,0.0563779571333461));
#96008=CARTESIAN_POINT('Ctrl Pts',(6.657974068,3.009344995,-2.869474048));
#96009=CARTESIAN_POINT('Ctrl Pts',(6.500877375,2.943588707,-3.23398186));
#96010=CARTESIAN_POINT('Ctrl Pts',(6.304927044,2.878703203,-3.57916121));
#96011=CARTESIAN_POINT('Ctrl Pts',(6.981205087,3.009344995,-2.740944277));
#96012=CARTESIAN_POINT('Ctrl Pts',(6.831145085,2.943588707,-3.123148198));
#96013=CARTESIAN_POINT('Ctrl Pts',(6.640257542,2.878703203,-3.486686073));
#96014=CARTESIAN_POINT('',(6.30492703114527,2.87870320349741,-3.57916120050747));
#96015=CARTESIAN_POINT('',(6.47259229556122,2.87870320212873,-3.53292363680765));
#96016=CARTESIAN_POINT('Origin',(-0.184227357519026,3.08923058099144,0.0649167702287662));
#96017=CARTESIAN_POINT('Ctrl Pts',(6.31736011824193,2.87421362536507,-3.55225860772393));
#96018=CARTESIAN_POINT('Ctrl Pts',(6.31068120543596,2.87645841418253,-3.56403325637194));
#96019=CARTESIAN_POINT('Ctrl Pts',(6.30400229263001,2.878703203,-3.57580790502));
#96020=CARTESIAN_POINT('Ctrl Pts',(6.1096857769,2.944013165,-3.91837993219));
#96021=CARTESIAN_POINT('Ctrl Pts',(5.87939106768,3.00933735,-4.23787774194));
#96022=CARTESIAN_POINT('Ctrl Pts',(6.31829739625371,2.87421362536507,-3.55560845819292));
#96023=CARTESIAN_POINT('Ctrl Pts',(6.31161222012684,2.87645841418253,-3.56738483409645));
#96024=CARTESIAN_POINT('Ctrl Pts',(6.304927044,2.878703203,-3.57916121));
#96025=CARTESIAN_POINT('Ctrl Pts',(6.110428303,2.944013165,-3.92178349));
#96026=CARTESIAN_POINT('Ctrl Pts',(5.879946996,3.00933735,-4.24131151));
#96027=CARTESIAN_POINT('Ctrl Pts',(6.41221682473787,2.87421362536508,-3.89127838495085));
#96028=CARTESIAN_POINT('Ctrl Pts',(6.40490403598191,2.87645841418253,-3.90322783954293));
#96029=CARTESIAN_POINT('Ctrl Pts',(6.39759124722613,2.878703203,-3.91517729413501));
#96030=CARTESIAN_POINT('Ctrl Pts',(6.18483272311035,2.944013165,-4.26283513137004));
#96031=CARTESIAN_POINT('Ctrl Pts',(5.93565348803107,3.00933735,-4.58539035288206));
#96032=CARTESIAN_POINT('',(6.39740218615542,2.87870320364628,-3.91449170041254));
#96033=CARTESIAN_POINT('',(6.08533611102078,2.96915797896983,-4.38391199843602));
#96034=CARTESIAN_POINT('Origin',(-0.158721867595243,2.94642846403946,0.109851978861961));
#96035=CARTESIAN_POINT('',(5.88269117803425,3.00855922074793,-4.23750453416616));
#96036=CARTESIAN_POINT('Ctrl Pts',(5.88269117488078,3.00855921928978,-4.23750453812649));
#96037=CARTESIAN_POINT('Ctrl Pts',(5.91643900043501,3.00166370065495,-4.2618378423234));
#96038=CARTESIAN_POINT('Ctrl Pts',(5.95021788409653,2.99493785110104,-4.2862195759487));
#96039=CARTESIAN_POINT('Ctrl Pts',(6.01775435318733,2.98181495154895,-4.33501496450934));
#96040=CARTESIAN_POINT('Ctrl Pts',(6.05155067503837,2.97541038110632,-4.35945660995131));
#96041=CARTESIAN_POINT('Ctrl Pts',(6.08533611175129,2.96915797896901,-4.38391199742659));
#96042=CARTESIAN_POINT('Origin',(-0.167732537891877,2.94642877561658,0.10812709419047));
#96043=CARTESIAN_POINT('',(6.35116461858435,2.87870320492457,-3.74682644868655));
#96044=CARTESIAN_POINT('Origin',(5.49039980146659E-13,2.97023924200022,
-4.05925293378573E-13));
#96045=CARTESIAN_POINT('',(6.0810688504322,2.78894740130207,-4.38982934047308));
#96046=CARTESIAN_POINT('Ctrl Pts',(6.08106884814993,2.78894740043738,-4.38982934357451));
#96047=CARTESIAN_POINT('Ctrl Pts',(6.12150429781557,2.79982120466031,-4.33381560487324));
#96048=CARTESIAN_POINT('Ctrl Pts',(6.16111048936085,2.81065020635268,-4.27731952794972));
#96049=CARTESIAN_POINT('Ctrl Pts',(6.19987187858141,2.8214285708836,-4.22037778961493));
#96050=CARTESIAN_POINT('Ctrl Pts',(6.26800474235051,2.84037425000917,-4.1202884024779));
#96051=CARTESIAN_POINT('Ctrl Pts',(6.33389865714034,2.85947647430085,-4.01827467958502));
#96052=CARTESIAN_POINT('Ctrl Pts',(6.39740218542473,2.87870320435315,-3.91449170053438));
#96053=CARTESIAN_POINT('',(5.73547757627587,2.87870320271434,-4.83262837136912));
#96054=CARTESIAN_POINT('Origin',(-0.138512604171944,2.94640460791274,0.130924848640008));
#96055=CARTESIAN_POINT('Origin',(-0.162705727006365,3.08920870108171,0.0935419213033933));
#96056=CARTESIAN_POINT('Ctrl Pts',(5.885462235,3.009344995,-4.233654956));
#96057=CARTESIAN_POINT('Ctrl Pts',(5.653679971,2.943588707,-4.555869632));
#96058=CARTESIAN_POINT('Ctrl Pts',(5.388107493,2.878703203,-4.850855352));
#96059=CARTESIAN_POINT('Ctrl Pts',(6.228766394,3.009344995,-4.177615254));
#96060=CARTESIAN_POINT('Ctrl Pts',(6.000052166,2.943588707,-4.518624994));
#96061=CARTESIAN_POINT('Ctrl Pts',(5.735477571,2.878703203,-4.832628377));
#96062=CARTESIAN_POINT('',(5.38810748217986,2.87870320347741,-4.85085534039044));
#96063=CARTESIAN_POINT('',(5.56179253551006,2.87870320212873,-4.84174186046794));
#96064=CARTESIAN_POINT('Origin',(-0.165965131742308,3.08923060397874,0.103002543905989));
#96065=CARTESIAN_POINT('Ctrl Pts',(5.40603315323794,2.8742136253572,-4.8272544609917));
#96066=CARTESIAN_POINT('Ctrl Pts',(5.39697918824401,2.8764584141786,-4.83731805610593));
#96067=CARTESIAN_POINT('Ctrl Pts',(5.38792522325,2.878703203,-4.84738165122));
#96068=CARTESIAN_POINT('Ctrl Pts',(5.12450885906,2.944013165,-5.14017222832));
#96069=CARTESIAN_POINT('Ctrl Pts',(4.83091572861,3.00933735,-5.40269380138));
#96070=CARTESIAN_POINT('Ctrl Pts',(5.40622839938105,2.8742136253572,-4.83072748088307));
#96071=CARTESIAN_POINT('Ctrl Pts',(5.39716794619055,2.8764584141786,-4.84079141644154));
#96072=CARTESIAN_POINT('Ctrl Pts',(5.388107493,2.878703203,-4.850855352));
#96073=CARTESIAN_POINT('Ctrl Pts',(5.124502361,2.944013165,-5.143655834));
#96074=CARTESIAN_POINT('Ctrl Pts',(4.830720501,3.00933735,-5.406166798));
#96075=CARTESIAN_POINT('Ctrl Pts',(5.42579293193448,2.87421362535721,-5.17873953196392));
#96076=CARTESIAN_POINT('Ctrl Pts',(5.41608233257222,2.8764584141786,-5.18883758156331));
#96077=CARTESIAN_POINT('Ctrl Pts',(5.40637173320981,2.878703203,-5.19893563116283));
#96078=CARTESIAN_POINT('Ctrl Pts',(5.12385122646595,2.944013165,-5.4927286282283));
#96079=CARTESIAN_POINT('Ctrl Pts',(4.81115782554438,3.00933735,-5.75417651719669));
#96080=CARTESIAN_POINT('',(5.40633447466497,2.87870320364628,-5.1982254236792));
#96081=CARTESIAN_POINT('',(5.00065284185713,2.96915797901993,-5.58958595540412));
#96082=CARTESIAN_POINT('Origin',(-0.131396090152665,2.94642848507124,0.141404195005143));
#96083=CARTESIAN_POINT('',(4.83421891288071,3.00855922009732,-5.40303874586003));
#96084=CARTESIAN_POINT('Ctrl Pts',(4.8342189094851,3.00855921915052,-5.40303874868488));
#96085=CARTESIAN_POINT('Ctrl Pts',(4.86194678848687,3.00166370047611,-5.43405793901585));
#96086=CARTESIAN_POINT('Ctrl Pts',(4.88969458781813,2.99493785108942,-5.46513110214075));
#96087=CARTESIAN_POINT('Ctrl Pts',(4.94516250405332,2.98181495662009,-5.5273040023307));
#96088=CARTESIAN_POINT('Ctrl Pts',(4.97291443011225,2.9754103916399,-5.55843939755067));
#96089=CARTESIAN_POINT('Ctrl Pts',(5.00065284321323,2.96915797902156,-5.58958595417019));
#96090=CARTESIAN_POINT('Origin',(-0.140567026918474,2.94642871097474,0.141656766218079));
#96091=CARTESIAN_POINT('',(5.39722098865919,2.87870320492457,-5.02454038223562));
#96092=CARTESIAN_POINT('Origin',(-3.33934269125535E-13,2.97023924200011,
4.43221848112074E-13));
#96093=CARTESIAN_POINT('',(4.99521329427853,2.78894740128863,-5.59444761728865));
#96094=CARTESIAN_POINT('Ctrl Pts',(4.99521329131002,2.78894740039219,-5.59444762017117));
#96095=CARTESIAN_POINT('Ctrl Pts',(5.04674468096817,2.79982120464079,-5.54843587769016));
#96096=CARTESIAN_POINT('Ctrl Pts',(5.09756988842109,2.81065020634783,-5.50177480787537));
#96097=CARTESIAN_POINT('Ctrl Pts',(5.14766584842138,2.82142857087551,-5.45449688854607));
#96098=CARTESIAN_POINT('Ctrl Pts',(5.23572206310051,2.84037424998681,-5.37139408782123));
#96099=CARTESIAN_POINT('Ctrl Pts',(5.32200534986858,2.85947647430085,-5.28593063299671));
#96100=CARTESIAN_POINT('Ctrl Pts',(5.40633447392617,2.87870320435315,-5.19822542366011));
#96101=CARTESIAN_POINT('',(4.56251304938851,2.87870320271433,-5.95260234463916));
#96102=CARTESIAN_POINT('Origin',(-0.107129220033608,2.94640461850637,0.157639935299));
#96103=CARTESIAN_POINT('Origin',(-0.138792725147368,3.08920868830491,0.126331557648913));
#96104=CARTESIAN_POINT('Ctrl Pts',(4.837752729,3.009344995,-5.399874863));
#96105=CARTESIAN_POINT('Ctrl Pts',(4.542122774,2.943588707,-5.664730004));
#96106=CARTESIAN_POINT('Ctrl Pts',(4.219346023,2.878703203,-5.895728889));
#96107=CARTESIAN_POINT('Ctrl Pts',(5.185077507,3.009344995,-5.418945585));
#96108=CARTESIAN_POINT('Ctrl Pts',(4.888403477,2.943588707,-5.702815909));
#96109=CARTESIAN_POINT('Ctrl Pts',(4.562513043,2.878703203,-5.952602349));
#96110=CARTESIAN_POINT('',(4.21934601544481,2.87870320349341,-5.89572887525597));
#96111=CARTESIAN_POINT('',(4.39092953729476,2.87870320212873,-5.92416561581676));
#96112=CARTESIAN_POINT('Origin',(-0.139942396941389,3.08923058268686,0.136271951790612));
#96113=CARTESIAN_POINT('Ctrl Pts',(4.24192608543235,2.87421362529374,-5.87653326056445));
#96114=CARTESIAN_POINT('Ctrl Pts',(4.2309204215162,2.87645841414687,-5.88441523968227));
#96115=CARTESIAN_POINT('Ctrl Pts',(4.2199147576,2.878703203,-5.8922972188));
#96116=CARTESIAN_POINT('Ctrl Pts',(3.89971560339,2.944013165,-6.12161578297));
#96117=CARTESIAN_POINT('Ctrl Pts',(3.55655213791,3.00933735,-6.31488590327));
#96118=CARTESIAN_POINT('Ctrl Pts',(4.2413701702162,2.87421362529374,-5.87996705533547));
#96119=CARTESIAN_POINT('Ctrl Pts',(4.23035809660807,2.87645841414687,-5.88784797216778));
#96120=CARTESIAN_POINT('Ctrl Pts',(4.219346023,2.878703203,-5.895728889));
#96121=CARTESIAN_POINT('Ctrl Pts',(3.898960385,2.944013165,-6.125016547));
#96122=CARTESIAN_POINT('Ctrl Pts',(3.555614883,3.00933735,-6.31823573500001));
#96123=CARTESIAN_POINT('Ctrl Pts',(4.1856649912382,2.87421362529374,-6.22404857479066));
#96124=CARTESIAN_POINT('Ctrl Pts',(4.17401063797508,2.87645841414687,-6.23182304588729));
#96125=CARTESIAN_POINT('Ctrl Pts',(4.16235628471193,2.878703203,-6.2395975169839));
#96126=CARTESIAN_POINT('Ctrl Pts',(3.82328414093741,2.944013165,-6.46578823919032));
#96127=CARTESIAN_POINT('Ctrl Pts',(3.46169776941115,3.00933735,-6.65390378403689));
#96128=CARTESIAN_POINT('',(4.16247256938398,2.87870320365574,-6.2388959060018));
#96129=CARTESIAN_POINT('',(3.6821446043708,2.96915797895617,-6.53389708421412));
#96130=CARTESIAN_POINT('Origin',(-0.0979263322834728,2.94642846350857,0.16634440571257));
#96131=CARTESIAN_POINT('',(3.55970394316431,3.00855922005574,-6.31593287016463));
#96132=CARTESIAN_POINT('Ctrl Pts',(3.55970393905358,3.00855921908199,-6.31593287229377));
#96133=CARTESIAN_POINT('Ctrl Pts',(3.58011534677,3.00166370041136,-6.35218752553784));
#96134=CARTESIAN_POINT('Ctrl Pts',(3.60053460648103,2.99493785103531,-6.38849917192794));
#96135=CARTESIAN_POINT('Ctrl Pts',(3.64134039390338,2.98181495147748,-6.46114249472729));
#96136=CARTESIAN_POINT('Ctrl Pts',(3.66175032427549,2.97541038106563,-6.49751583846894));
#96137=CARTESIAN_POINT('Ctrl Pts',(3.68214460546018,2.96915797895535,-6.53389708360331));
#96138=CARTESIAN_POINT('Origin',(-0.10682872237075,2.94642875408866,0.168562830046286));
#96139=CARTESIAN_POINT('',(4.19090930285252,2.87870320492457,-6.06731239219452));
#96140=CARTESIAN_POINT('Origin',(-7.63278329429795E-14,2.97023924199967,
1.39211558947139E-13));
#96141=CARTESIAN_POINT('',(3.67578711653968,2.78894740127316,-6.5374757419103));
#96142=CARTESIAN_POINT('Ctrl Pts',(3.67578711304387,2.78894740038181,-6.53747574404648));
#96143=CARTESIAN_POINT('Ctrl Pts',(3.73600489189342,2.79982120463246,-6.50361745621602));
#96144=CARTESIAN_POINT('Ctrl Pts',(3.79567258490586,2.81065020634291,-6.46897321361542));
#96145=CARTESIAN_POINT('Ctrl Pts',(3.85476068413728,2.82142857084263,-6.43356977651691));
#96146=CARTESIAN_POINT('Ctrl Pts',(3.95862283830183,2.84037424989596,-6.3713393564955));
#96147=CARTESIAN_POINT('Ctrl Pts',(4.06126098658263,2.85947647430088,-6.30642234553358));
#96148=CARTESIAN_POINT('Ctrl Pts',(4.16247257015051,2.87870320435315,-6.23889590408228));
#96149=CARTESIAN_POINT('',(3.17621048313442,2.87870320271434,-6.79423924909755));
#96150=CARTESIAN_POINT('Origin',(-0.0707368491739291,2.94640461726311,0.176984353505357));
#96151=CARTESIAN_POINT('Origin',(-0.108390380535675,3.08920870998506,0.153214497359081));
#96152=CARTESIAN_POINT('Ctrl Pts',(3.563835282,3.009344995,-6.313602623));
#96153=CARTESIAN_POINT('Ctrl Pts',(3.218180965,2.943588707,-6.508713897));
#96154=CARTESIAN_POINT('Ctrl Pts',(2.853292624,2.878703203,-6.664924696));
#96155=CARTESIAN_POINT('Ctrl Pts',(3.898940158,3.009344995,-6.406892042));
#96156=CARTESIAN_POINT('Ctrl Pts',(3.548178474,2.943588707,-6.620349489));
#96157=CARTESIAN_POINT('Ctrl Pts',(3.176210476,2.878703203,-6.794239252));
#96158=CARTESIAN_POINT('',(2.85329261859847,2.87870320347467,-6.66492468100942));
#96159=CARTESIAN_POINT('',(3.01475155487866,2.87870320212873,-6.72958197181443));
#96160=CARTESIAN_POINT('Origin',(-0.107376206837705,3.08923053390024,0.163169527380586));
#96161=CARTESIAN_POINT('Ctrl Pts',(2.87947126959757,2.87421362535152,-6.65103189674269));
#96162=CARTESIAN_POINT('Ctrl Pts',(2.86702851957879,2.87645841417576,-6.65636370710636));
#96163=CARTESIAN_POINT('Ctrl Pts',(2.85458576956,2.878703203,-6.66169551747));
#96164=CARTESIAN_POINT('Ctrl Pts',(2.49257597954,2.944013165,-6.81681938857999));
#96165=CARTESIAN_POINT('Ctrl Pts',(2.11588812321,3.00933735,-6.93180095857));
#96166=CARTESIAN_POINT('Ctrl Pts',(2.87819018699049,2.87421362535152,-6.65426590596142));
#96167=CARTESIAN_POINT('Ctrl Pts',(2.86574140549524,2.87645841417576,-6.6595953009807));
#96168=CARTESIAN_POINT('Ctrl Pts',(2.853292624,2.878703203,-6.664924696));
#96169=CARTESIAN_POINT('Ctrl Pts',(2.491107354,2.944013165,-6.819978295));
#96170=CARTESIAN_POINT('Ctrl Pts',(2.114252666,3.00933735,-6.934870991));
#96171=CARTESIAN_POINT('Ctrl Pts',(2.74982000782131,2.87421362535152,-6.97832802384403));
#96172=CARTESIAN_POINT('Ctrl Pts',(2.73676684554007,2.87645841417576,-6.98341539060992));
#96173=CARTESIAN_POINT('Ctrl Pts',(2.72371368325884,2.878703203,-6.98850275737577));
#96174=CARTESIAN_POINT('Ctrl Pts',(2.3439445382234,2.944013165,-7.1365147781814));
#96175=CARTESIAN_POINT('Ctrl Pts',(1.9503725743425,3.00933735,-7.24250190481638));
#96176=CARTESIAN_POINT('',(2.72397807488941,2.87870320365573,-6.98784254743535));
#96177=CARTESIAN_POINT('',(2.19146337730603,2.96915797899442,-7.17269044818231));
#96178=CARTESIAN_POINT('Origin',(-0.0598777743908424,2.94642848835606,0.183506743041469));
#96179=CARTESIAN_POINT('',(2.1187411738591,3.00855922009277,-6.93350099308368));
#96180=CARTESIAN_POINT('Ctrl Pts',(2.11874116901794,3.00855921917228,-6.93350099440111));
#96181=CARTESIAN_POINT('Ctrl Pts',(2.13088169066033,3.00166370050573,-6.97329588324973));
#96182=CARTESIAN_POINT('Ctrl Pts',(2.1430176289345,2.99493785108816,-7.01314812101293));
#96183=CARTESIAN_POINT('Ctrl Pts',(2.16725323268625,2.98181495153355,-7.09286512136001));
#96184=CARTESIAN_POINT('Ctrl Pts',(2.17936679654682,2.97541038110711,-7.13277560835332));
#96185=CARTESIAN_POINT('Ctrl Pts',(2.19146337849108,2.9691579789936,-7.17269044782304));
#96186=CARTESIAN_POINT('Origin',(-0.0680950929918261,2.94642876632057,0.18758694096996));
#96187=CARTESIAN_POINT('',(2.78863535708515,2.87870320492457,-6.82638361797163));
#96188=CARTESIAN_POINT('Origin',(4.96889855650107E-13,2.97023924199989,
-1.6831154525665E-12));
#96189=CARTESIAN_POINT('',(2.18448521775634,2.78894740125864,-7.17481876632809));
#96190=CARTESIAN_POINT('Ctrl Pts',(2.18448521418145,2.78894740041504,-7.17481876732048));
#96191=CARTESIAN_POINT('Ctrl Pts',(2.2505736657173,2.7998212046406,-7.15469710993879));
#96192=CARTESIAN_POINT('Ctrl Pts',(2.31629384925405,2.81065020634061,-7.13368962084375));
#96193=CARTESIAN_POINT('Ctrl Pts',(2.38161119431194,2.82142857088646,-7.11181609123042));
#96194=CARTESIAN_POINT('Ctrl Pts',(2.49642281089811,2.84037425001707,-7.07336787714953));
#96195=CARTESIAN_POINT('Ctrl Pts',(2.61061657427729,2.85947647430087,-7.03203275809879));
#96196=CARTESIAN_POINT('Ctrl Pts',(2.7239780760405,2.87870320435315,-6.98784254573441));
#96197=CARTESIAN_POINT('',(1.64139184460424,2.87870320271434,-7.31818507670773));
#96198=CARTESIAN_POINT('Origin',(-0.0310366276400662,2.94640459783726,0.188052768844947));
#96199=CARTESIAN_POINT('Origin',(-0.0729196359696244,3.08920870897142,0.172932995349643));
#96200=CARTESIAN_POINT('Ctrl Pts',(2.123276858,3.009344995,-6.932113342));
#96201=CARTESIAN_POINT('Ctrl Pts',(1.743760591,2.943588707,-7.048357562));
#96202=CARTESIAN_POINT('Ctrl Pts',(1.353822432,2.878703203,-7.122476032));
#96203=CARTESIAN_POINT('Ctrl Pts',(2.430492701,3.009344995,-7.095259349));
#96204=CARTESIAN_POINT('Ctrl Pts',(2.042044589,2.943588707,-7.228322886));
#96205=CARTESIAN_POINT('Ctrl Pts',(1.641391837,2.878703203,-7.318185078));
#96206=CARTESIAN_POINT('',(1.35382243033776,2.87870320349874,-7.12247601598353));
#96207=CARTESIAN_POINT('',(1.49760713973443,2.87870320212873,-7.2203305539143));
#96208=CARTESIAN_POINT('Origin',(-0.0697891869278638,3.08923055983671,0.182437410565597));
#96209=CARTESIAN_POINT('Ctrl Pts',(1.38237557612321,2.87421362542889,-7.11453567379985));
#96210=CARTESIAN_POINT('Ctrl Pts',(1.36907754929659,2.87645841421444,-7.11706800587004));
#96211=CARTESIAN_POINT('Ctrl Pts',(1.35577952247,2.878703203,-7.11960033794));
#96212=CARTESIAN_POINT('Ctrl Pts',(0.968886273399999,2.944013165,-7.19327609412999));
#96213=CARTESIAN_POINT('Ctrl Pts',(0.57628753136,3.00933735,-7.22459270619));
#96214=CARTESIAN_POINT('Ctrl Pts',(1.38042922812558,2.87421362542889,-7.11741867878759));
#96215=CARTESIAN_POINT('Ctrl Pts',(1.36712583006278,2.87645841421444,-7.11994735539385));
#96216=CARTESIAN_POINT('Ctrl Pts',(1.353822432,2.878703203,-7.12247603199999));
#96217=CARTESIAN_POINT('Ctrl Pts',(0.966772911999999,2.944013165,-7.196045436));
#96218=CARTESIAN_POINT('Ctrl Pts',(0.574030344,3.00933735,-7.227239388));
#96219=CARTESIAN_POINT('Ctrl Pts',(1.18539649581848,2.87421362542889,-7.40630861043445));
#96220=CARTESIAN_POINT('Ctrl Pts',(1.17155487598325,2.87645841421444,-7.40847099329545));
#96221=CARTESIAN_POINT('Ctrl Pts',(1.15771325614798,2.878703203,-7.41063337615648));
#96222=CARTESIAN_POINT('Ctrl Pts',(0.755004693420168,2.944013165,-7.47354581735855));
#96223=CARTESIAN_POINT('Ctrl Pts',(0.347850124077315,3.00933735,-7.4924486854024));
#96224=CARTESIAN_POINT('',(1.1581133920687,2.87870320365573,-7.41004543795076));
#96225=CARTESIAN_POINT('',(0.598311757139471,2.96915797894638,-7.47609677821526));
#96226=CARTESIAN_POINT('Origin',(-0.0190293521124379,2.94642847731649,0.192088534679514));
#96227=CARTESIAN_POINT('',(0.578708421721079,3.00855922013913,-7.22686631479652));
#96228=CARTESIAN_POINT('Ctrl Pts',(0.578708417200027,3.0085592193911,-7.22686631503209));
#96229=CARTESIAN_POINT('Ctrl Pts',(0.582010375225272,3.0016637006968,-7.26834067461964));
#96230=CARTESIAN_POINT('Ctrl Pts',(0.585295528807544,2.99493785114926,-7.30987005778705));
#96231=CARTESIAN_POINT('Ctrl Pts',(0.591827716122462,2.98181495671242,-7.39293322468151));
#96232=CARTESIAN_POINT('Ctrl Pts',(0.59507849357419,2.97541039178165,-7.43451464653668));
#96233=CARTESIAN_POINT('Ctrl Pts',(0.598311758986549,2.96915797894511,-7.47609677807154));
#96234=CARTESIAN_POINT('Origin',(-0.0261773973727075,2.94642875462569,0.197839503071079));
#96235=CARTESIAN_POINT('',(1.25596792029945,2.87870320492457,-7.26626073296047));
#96236=CARTESIAN_POINT('Origin',(1.52183021501391E-13,2.97023924199944,
-1.55431223447522E-12));
#96237=CARTESIAN_POINT('',(0.591039218776085,2.78894740131378,-7.47667523986356));
#96238=CARTESIAN_POINT('Ctrl Pts',(0.591039214962054,2.78894740045328,-7.47667524011751));
#96239=CARTESIAN_POINT('Ctrl Pts',(0.659908116785784,2.79982120466984,-7.47123107939932));
#96240=CARTESIAN_POINT('Ctrl Pts',(0.728607788144424,2.81065020635683,-7.46484263043069));
#96241=CARTESIAN_POINT('Ctrl Pts',(0.797100212037056,2.82142857084698,-7.45752179009138));
#96242=CARTESIAN_POINT('Ctrl Pts',(0.917492825796067,2.84037424990796,-7.44465357697846));
#96243=CARTESIAN_POINT('Ctrl Pts',(1.03790263162977,2.85947647430088,-7.42883313360311));
#96244=CARTESIAN_POINT('Ctrl Pts',(1.15811339355452,2.87870320435315,-7.41004543653923));
#96245=CARTESIAN_POINT('',(0.0298235486719519,2.87870320271433,-7.49994070433841));
#96246=CARTESIAN_POINT('Origin',(0.0101147754068714,2.94640462088094,0.190328198298189));
#96247=CARTESIAN_POINT('Origin',(-0.0340393366165772,3.08920866174723,0.184565482605681));
#96248=CARTESIAN_POINT('Ctrl Pts',(0.583436368,3.009344995,-7.226486145));
#96249=CARTESIAN_POINT('Ctrl Pts',(0.18780391,2.943588707,-7.258427861));
#96250=CARTESIAN_POINT('Ctrl Pts',(-0.208950992,2.878703203,-7.246988304));
#96251=CARTESIAN_POINT('Ctrl Pts',(0.848398107,3.009344995,-7.45186021400001));
#96252=CARTESIAN_POINT('Ctrl Pts',(0.440426968,2.943588707,-7.498307938));
#96253=CARTESIAN_POINT('Ctrl Pts',(0.029823541,2.878703203,-7.499940704));
#96254=CARTESIAN_POINT('',(-0.208950990233284,2.87870320350635,-7.24698828830006));
#96255=CARTESIAN_POINT('',(-0.0895637201545536,2.87870320212873,-7.37346450406493));
#96256=CARTESIAN_POINT('Origin',(-0.0289389099765305,3.08923058488446,0.193174565987628));
#96257=CARTESIAN_POINT('Ctrl Pts',(-0.179358461221556,2.8742136252575,-7.24537166885229));
#96258=CARTESIAN_POINT('Ctrl Pts',(-0.192889964610784,2.87645841412874,
-7.24498611376108));
#96259=CARTESIAN_POINT('Ctrl Pts',(-0.206421468,2.878703203,-7.24460055867));
#96260=CARTESIAN_POINT('Ctrl Pts',(-0.60010747717,2.944013165,-7.23338320603999));
#96261=CARTESIAN_POINT('Ctrl Pts',(-0.990259625069999,3.00933735,-7.1795705277));
#96262=CARTESIAN_POINT('Ctrl Pts',(-0.181879065534904,2.8742136252575,-7.24776886349914));
#96263=CARTESIAN_POINT('Ctrl Pts',(-0.195415028767454,2.87645841412874,
-7.24737858374956));
#96264=CARTESIAN_POINT('Ctrl Pts',(-0.208950992,2.878703203,-7.246988304));
#96265=CARTESIAN_POINT('Ctrl Pts',(-0.602766756,2.944013165,-7.235633492));
#96266=CARTESIAN_POINT('Ctrl Pts',(-0.993032999,3.00933735,-7.181670103));
#96267=CARTESIAN_POINT('Ctrl Pts',(-0.434454836637015,2.87421362525749,
-7.48797843674292));
#96268=CARTESIAN_POINT('Ctrl Pts',(-0.448437696021408,2.87645841412875,
-7.48711472518749));
#96269=CARTESIAN_POINT('Ctrl Pts',(-0.462420555405793,2.878703203,-7.48625101363205));
#96270=CARTESIAN_POINT('Ctrl Pts',(-0.869238330894868,2.944013165,-7.46112216094301));
#96271=CARTESIAN_POINT('Ctrl Pts',(-1.27093741073838,3.00933735,-7.39205689301606));
#96272=CARTESIAN_POINT('',(-0.461903382889853,2.87870320364628,-7.48576283800869));
#96273=CARTESIAN_POINT('',(-1.02281625401732,2.96915797896033,-7.42992913193523));
#96274=CARTESIAN_POINT('Origin',(0.0227088631124259,2.9464284729253,0.191688079987331));
#96275=CARTESIAN_POINT('',(-0.988384093003342,3.00855922008486,-7.18231140161262));
#96276=CARTESIAN_POINT('Ctrl Pts',(-0.988384096897368,3.00855921917128,
-7.18231140092207));
#96277=CARTESIAN_POINT('Ctrl Pts',(-0.994075098219697,3.00166370049321,
-7.22352593649195));
#96278=CARTESIAN_POINT('Ctrl Pts',(-0.999794339433125,2.9949378510805,-7.26479059594575));
#96279=CARTESIAN_POINT('Ctrl Pts',(-1.01127100116623,2.98181495151466,-7.34731605168395));
#96280=CARTESIAN_POINT('Ctrl Pts',(-1.01703500703518,2.97541038107445,-7.38862418208822));
#96281=CARTESIAN_POINT('Ctrl Pts',(-1.02281625280334,2.96915797895953,-7.42992913210503));
#96282=CARTESIAN_POINT('Origin',(0.0169642529079538,2.94642871660925,0.198841623721504));
#96283=CARTESIAN_POINT('',(-0.33542718003798,2.87870320492457,-7.36637557104469));
#96284=CARTESIAN_POINT('Origin',(-6.66513285535464E-14,2.97023924199933,
-8.90346824045096E-13));
#96285=CARTESIAN_POINT('',(-1.03004311690319,2.78894740130355,-7.42893068869816));
#96286=CARTESIAN_POINT('Ctrl Pts',(-1.0300431208892,2.78894740042007,-7.42893068822525));
#96287=CARTESIAN_POINT('Ctrl Pts',(-0.961614001997674,2.79982120465479,
-7.43841858722712));
#96288=CARTESIAN_POINT('Ctrl Pts',(-0.893147163133885,2.8106502063526,-7.44694789537783));
#96289=CARTESIAN_POINT('Ctrl Pts',(-0.824682289782256,2.82142857084429,
-7.45452205871353));
#96290=CARTESIAN_POINT('Ctrl Pts',(-0.704338102554433,2.84037424990055,
-7.46783554994457));
#96291=CARTESIAN_POINT('Ctrl Pts',(-0.583342483860824,2.85947647430086,
-7.47826952876738));
#96292=CARTESIAN_POINT('Ctrl Pts',(-0.461903383331452,2.87870320435315,
-7.48576283741235));
#96293=CARTESIAN_POINT('',(-1.58313926454892,2.87870320271433,-7.33100743903185));
#96294=CARTESIAN_POINT('Origin',(0.050793168375533,2.94640459030149,0.183703662817273));
#96295=CARTESIAN_POINT('Origin',(0.00643263499772659,3.0892086783798,0.187568015178932));
#96296=CARTESIAN_POINT('Ctrl Pts',(-0.983684957,3.009344995,-7.182956488));
#96297=CARTESIAN_POINT('Ctrl Pts',(-1.376934274,2.943588707,-7.12910214));
#96298=CARTESIAN_POINT('Ctrl Pts',(-1.7619541,2.878703203,-7.032639458));
#96299=CARTESIAN_POINT('Ctrl Pts',(-0.77336664,3.009344995,-7.460020378));
#96300=CARTESIAN_POINT('Ctrl Pts',(-1.181784528,2.943588707,-7.417680444));
#96301=CARTESIAN_POINT('Ctrl Pts',(-1.583139272,2.878703203,-7.331007437));
#96302=CARTESIAN_POINT('',(-1.76195409466987,2.87870320350153,-7.03263944295868));
#96303=CARTESIAN_POINT('',(-1.67254668079349,2.87870320212873,-7.18182344871253));
#96304=CARTESIAN_POINT('Origin',(0.0132645304981956,3.08923054631695,0.19487939873126));
#96305=CARTESIAN_POINT('Ctrl Pts',(-1.73270589824458,2.87421362540002,-7.03742213803915));
#96306=CARTESIAN_POINT('Ctrl Pts',(-1.74583815922732,2.87645841420001,-7.0341367238745));
#96307=CARTESIAN_POINT('Ctrl Pts',(-1.75897042021,2.878703203,-7.03085130971));
#96308=CARTESIAN_POINT('Ctrl Pts',(-2.14104086967,2.944013165,-6.93526535782));
#96309=CARTESIAN_POINT('Ctrl Pts',(-2.51050334239,3.00933735,-6.79883961102));
#96310=CARTESIAN_POINT('Ctrl Pts',(-1.73568289820881,2.87421362540002,-7.0392214321956));
#96311=CARTESIAN_POINT('Ctrl Pts',(-1.74881849910441,2.87645841420001,-7.03593044509774));
#96312=CARTESIAN_POINT('Ctrl Pts',(-1.7619541,2.878703203,-7.032639458));
#96313=CARTESIAN_POINT('Ctrl Pts',(-2.144121721,2.944013165,-6.936891367));
#96314=CARTESIAN_POINT('Ctrl Pts',(-2.513663223,3.00933735,-6.80029390600001));
#96315=CARTESIAN_POINT('Ctrl Pts',(-2.03399154486928,2.87421362540002,-7.21951871510421));
#96316=CARTESIAN_POINT('Ctrl Pts',(-2.04746181990317,2.87645841420001,-7.21566929529133));
#96317=CARTESIAN_POINT('Ctrl Pts',(-2.06093209493699,2.878703203,-7.21181987547844));
#96318=CARTESIAN_POINT('Ctrl Pts',(-2.45283673674315,2.944013165,-7.0998247239959));
#96319=CARTESIAN_POINT('Ctrl Pts',(-2.83029732434841,3.00933735,-6.94602073587786));
#96320=CARTESIAN_POINT('',(-2.06032207028557,2.87870320364628,-7.21145428992307));
#96321=CARTESIAN_POINT('',(-2.59611851412711,2.96915797894434,-7.03634625720979));
#96322=CARTESIAN_POINT('Origin',(0.0633852977853117,2.94642849123412,0.18232499930925));
#96323=CARTESIAN_POINT('',(-2.50926086557918,3.00855922011313,-6.80191958859531));
#96324=CARTESIAN_POINT('Ctrl Pts',(-2.50926086955055,3.00855921921572,-6.80191958696962));
#96325=CARTESIAN_POINT('Ctrl Pts',(-2.52367872523229,3.00166370051747,-6.84094715263986));
#96326=CARTESIAN_POINT('Ctrl Pts',(-2.53813493563224,2.99493785112607,-6.88001759932214));
#96327=CARTESIAN_POINT('Ctrl Pts',(-2.56708381281762,2.9818149515234,-6.95814651287553));
#96328=CARTESIAN_POINT('Ctrl Pts',(-2.58159308632967,2.97541038107013,-6.99724979130255));
#96329=CARTESIAN_POINT('Ctrl Pts',(-2.59611851297962,2.96915797894355,-7.03634625763599));
#96330=CARTESIAN_POINT('Origin',(0.0593126565460807,2.94642874914839,0.190545812164119));
#96331=CARTESIAN_POINT('',(-1.91113807793474,2.87870320492457,-7.12204687560344));
#96332=CARTESIAN_POINT('Origin',(4.10912623372006E-13,2.97023924199956,
1.22167900795667E-12));
#96333=CARTESIAN_POINT('',(-2.60296178177553,2.78894740129189,-7.03381759525304));
#96334=CARTESIAN_POINT('Ctrl Pts',(-2.60296178585068,2.78894740038344,-7.03381759402443));
#96335=CARTESIAN_POINT('Ctrl Pts',(-2.53817211941089,2.79982120463919,-7.05779390899228));
#96336=CARTESIAN_POINT('Ctrl Pts',(-2.47313954621206,2.81065020634898,-7.0808421530776));
#96337=CARTESIAN_POINT('Ctrl Pts',(-2.40790356477809,2.82142857087124,-7.10295716073517));
#96338=CARTESIAN_POINT('Ctrl Pts',(-2.29323496508005,2.84037424997502,-7.14182983350586));
#96339=CARTESIAN_POINT('Ctrl Pts',(-2.17731115325935,2.85947647430088,-7.17803035289085));
#96340=CARTESIAN_POINT('Ctrl Pts',(-2.06032207062276,2.87870320435315,-7.21145428926619));
#96341=CARTESIAN_POINT('',(-3.12207624415868,2.87870320271433,-6.8192844145898));
#96342=CARTESIAN_POINT('Origin',(0.0890965170584079,2.94640463018758,0.168489748353048));
#96343=CARTESIAN_POINT('Origin',(0.0466038476664976,3.08920870044056,0.181800031890108));
#96344=CARTESIAN_POINT('Ctrl Pts',(-2.504810268,3.009344995,-6.803559768));
#96345=CARTESIAN_POINT('Ctrl Pts',(-2.877288541,2.943588707,-6.666427527));
#96346=CARTESIAN_POINT('Ctrl Pts',(-3.232570193,2.878703203,-6.48945220700001));
#96347=CARTESIAN_POINT('Ctrl Pts',(-2.358969622,3.009344995,-7.11935828));
#96348=CARTESIAN_POINT('Ctrl Pts',(-2.748737092,2.943588707,-6.990210457));
#96349=CARTESIAN_POINT('Ctrl Pts',(-3.122076251,2.878703203,-6.819284411));
#96350=CARTESIAN_POINT('',(-3.23257018454474,2.878703203489,-6.48945219339775));
#96351=CARTESIAN_POINT('',(-3.17732321717587,2.87870320212873,-6.65436831130342));
#96352=CARTESIAN_POINT('Origin',(0.0548477622940036,3.08923055998583,0.187471849778713));
#96353=CARTESIAN_POINT('Ctrl Pts',(-3.20503393312873,2.87421362546291,-6.50041056930446));
#96354=CARTESIAN_POINT('Ctrl Pts',(-3.2171529020443,2.87645841423145,-6.49437891844234));
#96355=CARTESIAN_POINT('Ctrl Pts',(-3.22927187096,2.878703203,-6.48834726758));
#96356=CARTESIAN_POINT('Ctrl Pts',(-3.58186157136,2.944013165,-6.31286220897));
#96357=CARTESIAN_POINT('Ctrl Pts',(-3.91335871321,3.00933735,-6.10020250954));
#96358=CARTESIAN_POINT('Ctrl Pts',(-3.20832812754588,2.87421362546291,-6.50152782997139));
#96359=CARTESIAN_POINT('Ctrl Pts',(-3.22044916027291,2.87645841423145,-6.49549001848572));
#96360=CARTESIAN_POINT('Ctrl Pts',(-3.232570193,2.878703203,-6.489452207));
#96361=CARTESIAN_POINT('Ctrl Pts',(-3.585219938,2.944013165,-6.313787911));
#96362=CARTESIAN_POINT('Ctrl Pts',(-3.916757348,3.00933735,-6.100943523));
#96363=CARTESIAN_POINT('Ctrl Pts',(-3.53842107018125,2.8742136254629,-6.61348232156619));
#96364=CARTESIAN_POINT('Ctrl Pts',(-3.55074890599567,2.87645841423145,-6.6068271881958));
#96365=CARTESIAN_POINT('Ctrl Pts',(-3.56307674181016,2.878703203,-6.60017205482557));
#96366=CARTESIAN_POINT('Ctrl Pts',(-3.92174322298085,2.944013165,-6.40654737458526));
#96367=CARTESIAN_POINT('Ctrl Pts',(-4.25731568083914,3.00933735,-6.17519636984648));
#96368=CARTESIAN_POINT('',(-3.5624023890913,2.87870320364628,-6.59994615371924));
#96369=CARTESIAN_POINT('',(-4.04802915911568,2.96915797899007,-6.31375165200505));
#96370=CARTESIAN_POINT('Origin',(0.101097921122694,2.94642846559488,0.164436471006835));
#96371=CARTESIAN_POINT('',(-3.91280738900488,3.00855922007331,-6.10347757543102));
#96372=CARTESIAN_POINT('Ctrl Pts',(-3.91280739300367,3.00855921915691,-6.10347757268442));
#96373=CARTESIAN_POINT('Ctrl Pts',(-3.93527794006492,3.00166370051067,-6.13849328278278));
#96374=CARTESIAN_POINT('Ctrl Pts',(-3.95779516364713,2.99493785106891,-6.17354262673068));
#96375=CARTESIAN_POINT('Ctrl Pts',(-4.00286262173748,2.98181495656297,-6.2436217500575));
#96376=CARTESIAN_POINT('Ctrl Pts',(-4.02543870508714,2.97541039152408,-6.27869171914441));
#96377=CARTESIAN_POINT('Ctrl Pts',(-4.04802915756938,2.9691579789933,-6.31375165296533));
#96378=CARTESIAN_POINT('Origin',(0.0988877438210358,2.94642876685686,0.173340571503577));
#96379=CARTESIAN_POINT('',(-3.39748628437228,2.87870320492457,-6.54469918351707));
#96380=CARTESIAN_POINT('Origin',(-8.00141203294302E-14,2.970239242,-1.25767452008319E-13));
#96381=CARTESIAN_POINT('',(-4.05416884645276,2.78894740128127,-6.30981100856562));
#96382=CARTESIAN_POINT('Ctrl Pts',(-4.05416885007228,2.78894740038107,-6.30981100648208));
#96383=CARTESIAN_POINT('Ctrl Pts',(-3.9960481289277,2.79982120463475,-6.34715463168828));
#96384=CARTESIAN_POINT('Ctrl Pts',(-3.93749067225874,2.81065020634522,-6.38364410164896));
#96385=CARTESIAN_POINT('Ctrl Pts',(-3.87853394488013,2.82142857080492,-6.41926588030258));
#96386=CARTESIAN_POINT('Ctrl Pts',(-3.77490270966395,2.84037424979169,-6.48188009002636));
#96387=CARTESIAN_POINT('Ctrl Pts',(-3.66947117360319,2.85947647430088,-6.54215445487876));
#96388=CARTESIAN_POINT('Ctrl Pts',(-3.56240238930578,2.87870320435315,-6.59994615301406));
#96389=CARTESIAN_POINT('',(-4.51502840909075,2.87870320271434,-5.98869922997258));
#96390=CARTESIAN_POINT('Origin',(0.123233813057545,2.94640457796691,0.145397461512357));
#96391=CARTESIAN_POINT('Origin',(0.0845957594067731,3.08920869620704,0.1675309736737));
#96392=CARTESIAN_POINT('Ctrl Pts',(-3.908813434,3.009344995,-6.106036156));
#96393=CARTESIAN_POINT('Ctrl Pts',(-4.243103994,2.943588707,-5.892038171));
#96394=CARTESIAN_POINT('Ctrl Pts',(-4.55203489600001,2.878703203,-5.642825383));
#96395=CARTESIAN_POINT('Ctrl Pts',(-3.834269807,3.009344995,-6.445802902));
#96396=CARTESIAN_POINT('Ctrl Pts',(-4.187161766,2.943588707,-6.235885999));
#96397=CARTESIAN_POINT('Ctrl Pts',(-4.515028415,2.878703203,-5.98869922500001));
#96398=CARTESIAN_POINT('',(-4.55203488468433,2.87870320348395,-5.64282537181518));
#96399=CARTESIAN_POINT('',(-4.53353165128382,2.87870320212873,-5.81576230728662));
#96400=CARTESIAN_POINT('Origin',(0.0938663525190531,3.08923056724444,0.171298211864391));
#96401=CARTESIAN_POINT('Ctrl Pts',(-4.52749814143103,2.87421362522429,-5.65944702767209));
#96402=CARTESIAN_POINT('Ctrl Pts',(-4.53803714951051,2.87645841411214,-5.65095117293104));
#96403=CARTESIAN_POINT('Ctrl Pts',(-4.54857615759,2.878703203,-5.64245531819));
#96404=CARTESIAN_POINT('Ctrl Pts',(-4.85519840653001,2.944013165,-5.39527663992));
#96405=CARTESIAN_POINT('Ctrl Pts',(-5.13322978040999,3.00933735,-5.11632672005));
#96406=CARTESIAN_POINT('Ctrl Pts',(-4.53095549742285,2.87421362522429,-5.65983001298227));
#96407=CARTESIAN_POINT('Ctrl Pts',(-4.54149519671143,2.87645841411214,-5.65132769799116));
#96408=CARTESIAN_POINT('Ctrl Pts',(-4.552034896,2.878703203,-5.642825383));
#96409=CARTESIAN_POINT('Ctrl Pts',(-4.858677255,2.944013165,-5.39545875));
#96410=CARTESIAN_POINT('Ctrl Pts',(-5.136708253,3.00933735,-5.116319803));
#96411=CARTESIAN_POINT('Ctrl Pts',(-4.8773979560828,2.87421362522429,-5.69820684568864));
#96412=CARTESIAN_POINT('Ctrl Pts',(-4.88800691759854,2.87645841411214,-5.68905718488251));
#96413=CARTESIAN_POINT('Ctrl Pts',(-4.89861587911412,2.878703203,-5.67990752407634));
#96414=CARTESIAN_POINT('Ctrl Pts',(-5.2072733556336,2.944013165,-5.41370699056625));
#96415=CARTESIAN_POINT('Ctrl Pts',(-5.48526668878461,3.00933735,-5.11562668380304));
#96416=CARTESIAN_POINT('',(-4.89790873033672,2.87870320364628,-5.67983187031397));
#96417=CARTESIAN_POINT('',(-5.3106584585667,2.96915797898921,-5.29593303699521));
#96418=CARTESIAN_POINT('Origin',(0.134083018405543,2.94642846777895,0.138858694066594));
#96419=CARTESIAN_POINT('',(-5.13339538778399,3.00855922013794,-5.11964373418263));
#96420=CARTESIAN_POINT('Ctrl Pts',(-5.13339539093452,3.00855921933033,-5.11964373083109));
#96421=CARTESIAN_POINT('Ctrl Pts',(-5.16286793163712,3.00166370066671,-5.14901028953704));
#96422=CARTESIAN_POINT('Ctrl Pts',(-5.19239328821135,2.99493785113664,-5.17839966207307));
#96423=CARTESIAN_POINT('Ctrl Pts',(-5.2514720567996,2.9818149515647,-5.23715222562473));
#96424=CARTESIAN_POINT('Ctrl Pts',(-5.28105935724491,2.97541038112397,-5.26654911421085));
#96425=CARTESIAN_POINT('Ctrl Pts',(-5.31065845768295,2.96915797898838,-5.29593303788525));
#96426=CARTESIAN_POINT('Origin',(0.13383883078985,2.94642871007955,0.148029969099221));
#96427=CARTESIAN_POINT('',(-4.72497180730675,2.87870320492457,-5.66132863117273));
#96428=CARTESIAN_POINT('Origin',(-1.34007388519208E-13,2.97023924199967,
-2.68882138776405E-14));
#96429=CARTESIAN_POINT('',(-5.3158074822294,2.78894740125489,-5.29076467184895));
#96430=CARTESIAN_POINT('Ctrl Pts',(-5.315807485249,2.78894740036227,-5.29076466905292));
#96431=CARTESIAN_POINT('Ctrl Pts',(-5.26707336984818,2.79982120462009,-5.33972945793396));
#96432=CARTESIAN_POINT('Ctrl Pts',(-5.21772911131924,2.81065020633716,-5.38795394643646));
#96433=CARTESIAN_POINT('Ctrl Pts',(-5.16780838853748,2.82142857088395,-5.43541686148898));
#96434=CARTESIAN_POINT('Ctrl Pts',(-5.08006019774948,2.84037425001013,-5.51884483931084));
#96435=CARTESIAN_POINT('Ctrl Pts',(-4.9900507994269,2.85947647430088,-5.60037468588646));
#96436=CARTESIAN_POINT('Ctrl Pts',(-4.89790873034857,2.87870320435315,-5.67983186957425));
#96437=CARTESIAN_POINT('',(-5.69686286429477,2.87870320271433,-4.87808912509862));
#96438=CARTESIAN_POINT('Origin',(0.151608896763318,2.94640461492605,0.11550657870882));
#96439=CARTESIAN_POINT('Origin',(0.118632343573259,3.08920869426911,0.145428778230158));
#96440=CARTESIAN_POINT('Ctrl Pts',(-5.130044829,3.009344995,-5.123001079));
#96441=CARTESIAN_POINT('Ctrl Pts',(-5.41051662,2.943588707,-4.84214366));
#96442=CARTESIAN_POINT('Ctrl Pts',(-5.658651506,2.878703203,-4.532346316));
#96443=CARTESIAN_POINT('Ctrl Pts',(-5.130283797,3.009344995,-5.470848943));
#96444=CARTESIAN_POINT('Ctrl Pts',(-5.429799409,2.943588707,-5.189978441));
#96445=CARTESIAN_POINT('Ctrl Pts',(-5.696862869,2.878703203,-4.878089119));
#96446=CARTESIAN_POINT('',(-5.65865149264154,2.87870320350527,-4.53234630772529));
#96447=CARTESIAN_POINT('',(-5.67775718408892,2.87870320212873,-4.70521772161613));
#96448=CARTESIAN_POINT('Origin',(0.128495716125747,3.08923059219918,0.147114741849005));
#96449=CARTESIAN_POINT('Ctrl Pts',(-5.63826157005105,2.87421362540045,-4.55385403199581));
#96450=CARTESIAN_POINT('Ctrl Pts',(-5.64672782401047,2.87645841420022,-4.54329123080791));
#96451=CARTESIAN_POINT('Ctrl Pts',(-5.65519407797001,2.878703203,-4.53272842962));
#96452=CARTESIAN_POINT('Ctrl Pts',(-5.90151155978999,2.944013165,-4.22541393114));
#96453=CARTESIAN_POINT('Ctrl Pts',(-6.11307672812999,3.00933735,-3.89321717911));
#96454=CARTESIAN_POINT('Ctrl Pts',(-5.64172042550909,2.87421362540045,-4.55348483398032));
#96455=CARTESIAN_POINT('Ctrl Pts',(-5.65018596575451,2.87645841420022,-4.54291557499019));
#96456=CARTESIAN_POINT('Ctrl Pts',(-5.658651506,2.878703203,-4.532346316));
#96457=CARTESIAN_POINT('Ctrl Pts',(-5.904948223,2.944013165,-4.224843934));
#96458=CARTESIAN_POINT('Ctrl Pts',(-6.116472389,3.00933735,-3.892462655));
#96459=CARTESIAN_POINT('Ctrl Pts',(-5.98831313732949,2.87421362540045,-4.51648954957949));
#96460=CARTESIAN_POINT('Ctrl Pts',(-5.99670716025377,2.87645841420022,-4.50527319005817));
#96461=CARTESIAN_POINT('Ctrl Pts',(-6.00510118317804,2.878703203,-4.49405683053692));
#96462=CARTESIAN_POINT('Ctrl Pts',(-6.24931717279247,2.944013165,-4.16772768358729));
#96463=CARTESIAN_POINT('Ctrl Pts',(-6.45673272182828,3.00933735,-3.81685598088723));
#96464=CARTESIAN_POINT('',(-6.00439430383142,2.87870320364628,-4.49413496160079));
#96465=CARTESIAN_POINT('',(-6.32496727096953,2.96915797898409,-4.03048247922108));
#96466=CARTESIAN_POINT('Origin',(0.160798983820203,2.9464284946586,0.106788522587034));
#96467=CARTESIAN_POINT('',(-6.11395152353537,3.00855922012302,-3.89642104262903));
#96468=CARTESIAN_POINT('Ctrl Pts',(-6.11395152592256,3.00855921933987,-3.89642103863776));
#96469=CARTESIAN_POINT('Ctrl Pts',(-6.1490479569122,3.00166370068712,-3.91876529849187));
#96470=CARTESIAN_POINT('Ctrl Pts',(-6.18420087352747,2.9949378511202,-3.94112048507939));
#96471=CARTESIAN_POINT('Ctrl Pts',(-6.25452847761625,2.98181495155569,-3.9857992574478));
#96472=CARTESIAN_POINT('Ctrl Pts',(-6.2897435054049,2.97541038112154,-4.00814846808177));
#96473=CARTESIAN_POINT('Ctrl Pts',(-6.32496727029219,2.96915797898326,-4.03048248028911));
#96474=CARTESIAN_POINT('Origin',(0.162531914113991,2.94642873184857,0.115797771320268));
#96475=CARTESIAN_POINT('',(-5.8315229001711,2.87870320492457,-4.51324064446962));
#96476=CARTESIAN_POINT('Origin',(-5.30391702779909E-13,2.97023924200056,
-3.57786716920216E-13));
#96477=CARTESIAN_POINT('',(-6.32888486767176,2.78894740126767,-4.02432805943019));
#96478=CARTESIAN_POINT('Ctrl Pts',(-6.32888487003153,2.78894740037185,-4.02432805603769));
#96479=CARTESIAN_POINT('Ctrl Pts',(-6.29181611341766,2.79982120462702,-4.0826244695479));
#96480=CARTESIAN_POINT('Ctrl Pts',(-6.25399233574641,2.81065020634096,-4.14032905322512));
#96481=CARTESIAN_POINT('Ctrl Pts',(-6.21544185532186,2.82142857091001,-4.1974137915234));
#96482=CARTESIAN_POINT('Ctrl Pts',(-6.14767971779934,2.84037425008215,-4.29775453722658));
#96483=CARTESIAN_POINT('Ctrl Pts',(-6.07730119665039,2.85947647430087,-4.39672762094291));
#96484=CARTESIAN_POINT('Ctrl Pts',(-6.00439430370237,2.87870320435315,-4.49413496087379));
#96485=CARTESIAN_POINT('',(-6.61231834271407,2.87870320271434,-3.53938499496242));
#96486=CARTESIAN_POINT('Origin',(0.17289507850705,2.94640462869725,0.0802147943709647));
#96487=CARTESIAN_POINT('Origin',(0.147121763688923,3.08920867755301,0.116526339563724));
#96488=CARTESIAN_POINT('Ctrl Pts',(-6.111401029,3.009344995,-3.900420166));
#96489=CARTESIAN_POINT('Ctrl Pts',(-6.32493950200001,2.943588707,-3.565835892));
#96490=CARTESIAN_POINT('Ctrl Pts',(-6.500675861,2.878703203,-3.209939773));
#96491=CARTESIAN_POINT('Ctrl Pts',(-6.186411418,3.009344995,-4.240084169));
#96492=CARTESIAN_POINT('Ctrl Pts',(-6.418545666,2.943588707,-3.90139326));
#96493=CARTESIAN_POINT('Ctrl Pts',(-6.612318346,2.878703203,-3.539384988));
#96494=CARTESIAN_POINT('',(-6.50067584637424,2.87870320347896,-3.20993976725337));
#96495=CARTESIAN_POINT('',(-6.55649710105352,2.87870320212873,-3.37466238525318));
#96496=CARTESIAN_POINT('Origin',(0.157116902266113,3.08923058993594,0.116052513379786));
#96497=CARTESIAN_POINT('Ctrl Pts',(-6.48538615356865,2.87421362538382,-3.23532788416263));
#96498=CARTESIAN_POINT('Ctrl Pts',(-6.49138378120933,2.87645841419191,-3.22319204100631));
#96499=CARTESIAN_POINT('Ctrl Pts',(-6.49738140885,2.878703203,-3.21105619785));
#96500=CARTESIAN_POINT('Ctrl Pts',(-6.6718765916,2.944013165,-2.85797556393));
#96501=CARTESIAN_POINT('Ctrl Pts',(-6.80708300218001,3.00933735,-2.48806512947));
#96502=CARTESIAN_POINT('Ctrl Pts',(-6.48868477624723,2.87421362538382,-3.23422376610241));
#96503=CARTESIAN_POINT('Ctrl Pts',(-6.4946803186236,2.87645841419191,-3.22208176955118));
#96504=CARTESIAN_POINT('Ctrl Pts',(-6.500675861,2.878703203,-3.209939773));
#96505=CARTESIAN_POINT('Ctrl Pts',(-6.675110375,2.944013165,-2.856680112));
#96506=CARTESIAN_POINT('Ctrl Pts',(-6.81023707400001,3.00933735,-2.486598279));
#96507=CARTESIAN_POINT('Ctrl Pts',(-6.81922145039138,2.87421362538383,-3.12358622217583));
#96508=CARTESIAN_POINT('Ctrl Pts',(-6.82500804000554,2.87645841419191,-3.11082762807001));
#96509=CARTESIAN_POINT('Ctrl Pts',(-6.83079462961964,2.878703203,-3.09806903396426));
#96510=CARTESIAN_POINT('Ctrl Pts',(-6.99914986484071,2.944013165,-2.72687006272138));
#96511=CARTESIAN_POINT('Ctrl Pts',(-7.12628910873856,3.00933735,-2.33961333314017));
#96512=CARTESIAN_POINT('',(-6.83012107408333,2.87870320365575,-3.09829729477548));
#96513=CARTESIAN_POINT('',(-7.04352764417412,2.96915797898783,-2.57657103907726));
#96514=CARTESIAN_POINT('Origin',(0.179995934489753,2.94642846182119,0.0697248336034639));
#96515=CARTESIAN_POINT('',(-6.80862608162002,3.00855922010261,-2.49100603347877));
#96516=CARTESIAN_POINT('Ctrl Pts',(-6.80862608309258,3.00855921927237,-2.49100602904712));
#96517=CARTESIAN_POINT('Ctrl Pts',(-6.84770533459544,3.00166370059657,-2.50528319728228));
#96518=CARTESIAN_POINT('Ctrl Pts',(-6.88684209941936,2.9949378511142,-2.51955889384014));
#96519=CARTESIAN_POINT('Ctrl Pts',(-6.96513006845013,2.98181495661202,-2.54807473423967));
#96520=CARTESIAN_POINT('Ctrl Pts',(-7.00432617261881,2.9754103915964,-2.56233122981507));
#96521=CARTESIAN_POINT('Ctrl Pts',(-7.04352764352837,2.96915797898996,-2.5765710407879));
#96522=CARTESIAN_POINT('Origin',(0.183624911733789,2.94642874499142,0.0781508407550076));
#96523=CARTESIAN_POINT('',(-6.66539846337813,2.87870320492457,-3.15411854132372));
#96524=CARTESIAN_POINT('Origin',(1.43765208071578E-12,2.97023924199989,
4.51895465491958E-13));
#96525=CARTESIAN_POINT('',(-7.04603063111017,2.78894740127532,-2.56971833965995));
#96526=CARTESIAN_POINT('Ctrl Pts',(-7.04603063233613,2.78894740042345,-2.56971833609903));
#96527=CARTESIAN_POINT('Ctrl Pts',(-7.0223605283775,2.79982120464813,-2.63462049873483));
#96528=CARTESIAN_POINT('Ctrl Pts',(-6.99782582942406,2.81065020634501,-2.69910697557628));
#96529=CARTESIAN_POINT('Ctrl Pts',(-6.97244816946066,2.82142857080435,-2.76314431783759));
#96530=CARTESIAN_POINT('Ctrl Pts',(-6.92784056788042,2.84037424979018,-2.87570600714895));
#96531=CARTESIAN_POINT('Ctrl Pts',(-6.88038374407231,2.85947647430088,-2.98749445823547));
#96532=CARTESIAN_POINT('Ctrl Pts',(-6.8301210723039,2.87870320435315,-3.09829729585191));
#96533=CARTESIAN_POINT('',(-7.218589164312,2.87870320271433,-2.0351831555464));
#96534=CARTESIAN_POINT('Origin',(0.186096308467992,2.94640459671127,0.0411719524297086));
#96535=CARTESIAN_POINT('Origin',(0.168731710661435,3.08920867055077,0.082175130974515));
#96536=CARTESIAN_POINT('Ctrl Pts',(-6.806994909,3.009344995,-2.49545994));
#96537=CARTESIAN_POINT('Ctrl Pts',(-6.943615243,2.943588707,-2.122793602));
#96538=CARTESIAN_POINT('Ctrl Pts',(-7.038735838,2.878703203,-1.737440013));
#96539=CARTESIAN_POINT('Ctrl Pts',(-6.953269318,3.009344995,-2.811057772));
#96540=CARTESIAN_POINT('Ctrl Pts',(-7.107167862,2.943588707,-2.430383266));
#96541=CARTESIAN_POINT('Ctrl Pts',(-7.218589166,2.878703203,-2.035183148));
#96542=CARTESIAN_POINT('',(-7.03873582220987,2.87870320348778,-1.73744001092693));
#96543=CARTESIAN_POINT('',(-7.1286625006325,2.87870320212873,-1.88631158566797));
#96544=CARTESIAN_POINT('Origin',(0.178391247383135,3.08923062900728,0.0795637173879721));
#96545=CARTESIAN_POINT('Ctrl Pts',(-7.02926128892046,2.87421362546414,-1.76552139884387));
#96546=CARTESIAN_POINT('Ctrl Pts',(-7.03250984778527,2.87645841423207,-1.75237997256197));
#96547=CARTESIAN_POINT('Ctrl Pts',(-7.03575840664999,2.878703203,-1.73923854628));
#96548=CARTESIAN_POINT('Ctrl Pts',(-7.13027209054,2.944013165,-1.35690143583));
#96549=CARTESIAN_POINT('Ctrl Pts',(-7.18279764011,3.00933735,-0.966573919529999));
#96550=CARTESIAN_POINT('Ctrl Pts',(-7.03224543889102,2.87421362546414,-1.76373398808801));
#96551=CARTESIAN_POINT('Ctrl Pts',(-7.03549063844558,2.87645841423207,-1.750587000544));
#96552=CARTESIAN_POINT('Ctrl Pts',(-7.038735838,2.878703203,-1.737440013));
#96553=CARTESIAN_POINT('Ctrl Pts',(-7.133151786,2.944013165,-1.354941103));
#96554=CARTESIAN_POINT('Ctrl Pts',(-7.185562642,3.00933735,-0.964463331));
#96555=CARTESIAN_POINT('Ctrl Pts',(-7.33127054800838,2.87421362546415,-1.58462747481222));
#96556=CARTESIAN_POINT('Ctrl Pts',(-7.33417912971884,2.87645841423207,-1.57092322405938));
#96557=CARTESIAN_POINT('Ctrl Pts',(-7.33708771142929,2.878703203,-1.55721897330654));
#96558=CARTESIAN_POINT('Ctrl Pts',(-7.42171008824157,2.944013165,-1.1585070282478));
#96559=CARTESIAN_POINT('Ctrl Pts',(-7.46262813804142,3.00933735,-0.752972966339245));
#96560=CARTESIAN_POINT('',(-7.33647897257464,2.87870320365574,-1.55758669204523));
#96561=CARTESIAN_POINT('',(-7.43274049270505,2.96915797897333,-1.00218200151024));
#96562=CARTESIAN_POINT('Origin',(0.190776647659696,2.94642846480955,0.0294009218485594));
#96563=CARTESIAN_POINT('',(-7.18493685125043,3.00855922004598,-0.969114350955477));
#96564=CARTESIAN_POINT('Ctrl Pts',(-7.18493685170426,3.00855921907439,-0.969114346370303));
#96565=CARTESIAN_POINT('Ctrl Pts',(-7.22617162141738,3.00166370041615,-0.97465683841719));
#96566=CARTESIAN_POINT('Ctrl Pts',(-7.26746224275235,2.99493785104705,-0.980185529411084));
#96567=CARTESIAN_POINT('Ctrl Pts',(-7.35004994567778,2.98181495654752,-0.991205086004124));
#96568=CARTESIAN_POINT('Ctrl Pts',(-7.3913943919297,2.97541039153636,-0.996702268783438));
#96569=CARTESIAN_POINT('Ctrl Pts',(-7.43274049243919,2.96915797897599,-1.00218200331461));
#96570=CARTESIAN_POINT('Origin',(0.196132190811885,2.94642874722832,0.0368498301381716));
#96571=CARTESIAN_POINT('',(-7.18760740282466,2.87870320492457,-1.64751336067173));
#96572=CARTESIAN_POINT('Origin',(-9.3198018746854E-13,2.97023924199933,
-5.52129956338243E-14));
#96573=CARTESIAN_POINT('',(-7.43371183306105,2.78894740126599,-0.994951446309474));
#96574=CARTESIAN_POINT('Ctrl Pts',(-7.43371183348005,2.78894740041728,-0.994951442589054));
#96575=CARTESIAN_POINT('Ctrl Pts',(-7.4245471698726,2.79982120464327,-1.06342460138507));
#96576=CARTESIAN_POINT('Ctrl Pts',(-7.41444876488241,2.81065020634229,-1.13167765525743));
#96577=CARTESIAN_POINT('Ctrl Pts',(-7.40343055618149,2.82142857082246,-1.19967328687996));
#96578=CARTESIAN_POINT('Ctrl Pts',(-7.38406329126841,2.84037424984021,-1.31919266278128));
#96579=CARTESIAN_POINT('Ctrl Pts',(-7.36174719434581,2.85947647430085,-1.43856937610525));
#96580=CARTESIAN_POINT('Ctrl Pts',(-7.33647897107824,2.87870320435315,-1.55758669346289));
#96581=CARTESIAN_POINT('',(-7.48732677997331,2.87870320271433,-0.435818413732416));
#96582=CARTESIAN_POINT('Origin',(0.190596323641602,2.9464046004507,0.000204179866555437));
#96583=CARTESIAN_POINT('Origin',(0.182451887430135,3.08920867961731,0.0439815725690257));
#96584=CARTESIAN_POINT('Ctrl Pts',(-7.184301272,3.009344995,-0.973814782));
#96585=CARTESIAN_POINT('Ctrl Pts',(-7.237615252,2.943588707,-0.580491841));
#96586=CARTESIAN_POINT('Ctrl Pts',(-7.24767235,2.878703203,-0.18369949));
#96587=CARTESIAN_POINT('Ctrl Pts',(-7.395000072,3.009344995,-1.250589437));
#96588=CARTESIAN_POINT('Ctrl Pts',(-7.463466788,2.943588707,-0.845731252));
#96589=CARTESIAN_POINT('Ctrl Pts',(-7.48732678,2.878703203,-0.435818406));
#96590=CARTESIAN_POINT('',(-7.24767233445532,2.87870320348066,-0.183699490833677));
#96591=CARTESIAN_POINT('',(-7.36749956477544,2.87870320212873,-0.309758953341122));
#96592=CARTESIAN_POINT('Origin',(0.191324778271704,3.08923051194625,0.0393547283114241));
#96593=CARTESIAN_POINT('Ctrl Pts',(-7.24445597850345,2.87421362531791,-0.213161097600263));
#96594=CARTESIAN_POINT('Ctrl Pts',(-7.24480356966667,2.87645841415895,-0.199628565955134));
#96595=CARTESIAN_POINT('Ctrl Pts',(-7.24515116083001,2.878703203,-0.18609603431));
#96596=CARTESIAN_POINT('Ctrl Pts',(-7.25526398982,2.944013165,0.20761989627));
#96597=CARTESIAN_POINT('Ctrl Pts',(-7.22265264346,3.00933735,0.600113212189999));
#96598=CARTESIAN_POINT('Ctrl Pts',(-7.24698612022989,2.87421362531791,-0.210773971470073));
#96599=CARTESIAN_POINT('Ctrl Pts',(-7.24732923511493,2.87645841415895,-0.197236730735039));
#96600=CARTESIAN_POINT('Ctrl Pts',(-7.24767235000001,2.878703203,-0.18369949));
#96601=CARTESIAN_POINT('Ctrl Pts',(-7.257654946,2.944013165,0.210153447));
#96602=CARTESIAN_POINT('Ctrl Pts',(-7.224899287,3.00933735,0.602768849999999));
#96603=CARTESIAN_POINT('Ctrl Pts',(-7.50051758257425,2.8742136253179,0.0284266915784136));
#96604=CARTESIAN_POINT('Ctrl Pts',(-7.5004121544549,2.87645841415895,0.0424358040815379));
#96605=CARTESIAN_POINT('Ctrl Pts',(-7.50030672633554,2.878703203,0.0564449165846612));
#96606=CARTESIAN_POINT('Ctrl Pts',(-7.49723939708658,2.944013165,0.464026506667312));
#96607=CARTESIAN_POINT('Ctrl Pts',(-7.45002296924085,3.00933735,0.868875578477823));
#96608=CARTESIAN_POINT('',(-7.49979126809725,2.87870320365573,0.0559549340228299));
#96609=CARTESIAN_POINT('',(-7.4744066564856,2.96915797898704,0.61906795124598));
#96610=CARTESIAN_POINT('Origin',(0.192636452580373,2.94642845830759,-0.0122977839134168));
#96611=CARTESIAN_POINT('',(-7.22528795887605,3.00855922068919,0.59809204170826));
#96612=CARTESIAN_POINT('Ctrl Pts',(-7.22528795819246,3.00855921913363,0.598092046812644));
#96613=CARTESIAN_POINT('Ctrl Pts',(-7.2667501538357,3.00166370046621,0.601543391562507));
#96614=CARTESIAN_POINT('Ctrl Pts',(-7.30826392881565,2.99493785104743,0.605020221165689));
#96615=CARTESIAN_POINT('Ctrl Pts',(-7.39128968801793,2.98181495150243,0.612012212856943));
#96616=CARTESIAN_POINT('Ctrl Pts',(-7.43284929343284,2.97541038109254,0.61553138801568));
#96617=CARTESIAN_POINT('Ctrl Pts',(-7.4744066565912,2.96915797898622,0.619067950003641));
#96618=CARTESIAN_POINT('Origin',(0.199468459704489,2.94642872644919,-0.00617432263199562));
#96619=CARTESIAN_POINT('',(-7.37373180839628,2.87870320492457,-0.0638722864739663));
#96620=CARTESIAN_POINT('Origin',(-5.72892427941341E-13,2.97023924200067,
-5.41220171977608E-14));
#96621=CARTESIAN_POINT('',(-7.47380093222391,2.78894740127503,0.62633827058956));
#96622=CARTESIAN_POINT('Ctrl Pts',(-7.47380093190115,2.78894740040347,0.62633827448373));
#96623=CARTESIAN_POINT('Ctrl Pts',(-7.47957023810749,2.79982120463978,0.557495848341243));
#96624=CARTESIAN_POINT('Ctrl Pts',(-7.48438031722103,2.81065020634327,0.488667654540507));
#96625=CARTESIAN_POINT('Ctrl Pts',(-7.48823675894358,2.82142857084232,0.419893134006143));
#96626=CARTESIAN_POINT('Ctrl Pts',(-7.49501542250106,2.84037424989509,0.299004664932385));
#96627=CARTESIAN_POINT('Ctrl Pts',(-7.49888352801377,2.85947647430086,0.177621611978818));
#96628=CARTESIAN_POINT('Ctrl Pts',(-7.49979126694244,2.87870320435315,0.0559549323218407));
#96629=CARTESIAN_POINT('',(-7.40596531758727,2.87870320271433,1.18392471247567));
#96630=CARTESIAN_POINT('Origin',(0.186184211535964,2.94640464720024,-0.0407731753774626));
#96631=CARTESIAN_POINT('Origin',(0.187641356349982,3.08920870438448,0.0037315182555403));
#96632=CARTESIAN_POINT('Ctrl Pts',(-7.225677693,3.009344995,0.593364874));
#96633=CARTESIAN_POINT('Ctrl Pts',(-7.19319241600001,2.943588707,0.988953072));
#96634=CARTESIAN_POINT('Ctrl Pts',(-7.117715759,2.878703203,1.378630618));
#96635=CARTESIAN_POINT('Ctrl Pts',(-7.490948841,3.009344995,0.36835507));
#96636=CARTESIAN_POINT('Ctrl Pts',(-7.470782301,2.943588707,0.778466215));
#96637=CARTESIAN_POINT('Ctrl Pts',(-7.405965316,2.878703203,1.18392472));
#96638=CARTESIAN_POINT('',(-7.11771574350775,2.87870320346112,1.37863061353755));
#96639=CARTESIAN_POINT('',(-7.26184053842887,2.87870320212873,1.28127766373548));
#96640=CARTESIAN_POINT('Origin',(0.195311683314985,3.08923059998896,-0.0026944978714246));
#96641=CARTESIAN_POINT('Ctrl Pts',(-7.12090795932426,2.87421362526545,1.34916638133665));
#96642=CARTESIAN_POINT('Ctrl Pts',(-7.11833832967722,2.87645841413273,1.36245725188334));
#96643=CARTESIAN_POINT('Ctrl Pts',(-7.11576870003,2.878703203,1.37574812243));
#96644=CARTESIAN_POINT('Ctrl Pts',(-7.04100780956999,2.944013165,1.76243315237));
#96645=CARTESIAN_POINT('Ctrl Pts',(-6.92478443736999,3.00933735,2.13873971657));
#96646=CARTESIAN_POINT('Ctrl Pts',(-7.12286578617501,2.87421362526545,1.35204160345241));
#96647=CARTESIAN_POINT('Ctrl Pts',(-7.12029077258757,2.87645841413273,1.36533611072621));
#96648=CARTESIAN_POINT('Ctrl Pts',(-7.117715759,2.878703203,1.378630618));
#96649=CARTESIAN_POINT('Ctrl Pts',(-7.04279822799999,2.944013165,1.765421455));
#96650=CARTESIAN_POINT('Ctrl Pts',(-6.926407672,3.00933735,2.141816229));
#96651=CARTESIAN_POINT('Ctrl Pts',(-7.31904875066755,2.87421362526546,1.64015165671574));
#96652=CARTESIAN_POINT('Ctrl Pts',(-7.31593424229251,2.87645841413272,1.65381058023419));
#96653=CARTESIAN_POINT('Ctrl Pts',(-7.3128197339176,2.878703203,1.66746950375257));
#96654=CARTESIAN_POINT('Ctrl Pts',(-7.22220612362153,2.944013165,2.06486267909898));
#96655=CARTESIAN_POINT('Ctrl Pts',(-7.08906300674669,3.00933735,2.45009646767011));
#96656=CARTESIAN_POINT('',(-7.31242165847653,2.87870320364628,1.66688016618383));
#96657=CARTESIAN_POINT('',(-7.16657787235505,2.9691579789703,2.21137097685948));
#96658=CARTESIAN_POINT('Origin',(0.185489064144846,2.94642850249844,-0.0534214073414038));
#96659=CARTESIAN_POINT('',(-6.92779263185941,3.00855922011726,2.13733231535534));
#96660=CARTESIAN_POINT('Ctrl Pts',(-6.92779263023839,3.00855921928044,2.13733232013128));
#96661=CARTESIAN_POINT('Ctrl Pts',(-6.96754352551728,3.0016637006159,2.14961612077638));
#96662=CARTESIAN_POINT('Ctrl Pts',(-7.00733931618843,2.99493785112561,2.1619358986615));
#96663=CARTESIAN_POINT('Ctrl Pts',(-7.08692087679833,2.98181495663568,2.18661249604047));
#96664=CARTESIAN_POINT('Ctrl Pts',(-7.12675228698315,2.97541039162993,2.19898347034704));
#96665=CARTESIAN_POINT('Ctrl Pts',(-7.16657787288143,2.9691579789718,2.21137097510419));
#96666=CARTESIAN_POINT('Origin',(0.193477601862492,2.94642873647769,-0.0489097679838857));
#96667=CARTESIAN_POINT('',(-7.21506870997276,2.87870320492457,1.52275538478368));
#96668=CARTESIAN_POINT('Origin',(-5.78963960107259E-13,2.97023924200022,
1.82362805412062E-13));
#96669=CARTESIAN_POINT('',(-7.16442340567892,2.78894740128806,2.21834110639615));
#96670=CARTESIAN_POINT('Ctrl Pts',(-7.16442340449826,2.78894740044059,2.218341109943));
#96671=CARTESIAN_POINT('Ctrl Pts',(-7.18485691423675,2.79982120465849,2.15234841177283));
#96672=CARTESIAN_POINT('Ctrl Pts',(-7.20435056352046,2.81065020634985,2.086163407635));
#96673=CARTESIAN_POINT('Ctrl Pts',(-7.22290133274774,2.82142857085343,2.0198258179021));
#96674=CARTESIAN_POINT('Ctrl Pts',(-7.25550896269093,2.8403742499258,1.90322086607327));
#96675=CARTESIAN_POINT('Ctrl Pts',(-7.28538040220174,2.85947647430087,1.78550720985898));
#96676=CARTESIAN_POINT('Ctrl Pts',(-7.31242165780932,2.87870320435315,1.66688016651236));
#96677=CARTESIAN_POINT('',(-6.97830914718863,2.87870320271433,2.74830883498448));
#96678=CARTESIAN_POINT('Origin',(0.173066247482618,2.94640463867172,-0.0798440046925969));
#96679=CARTESIAN_POINT('Origin',(0.184056299537407,3.08920868238395,-0.0366929833980065));
#96680=CARTESIAN_POINT('Ctrl Pts',(-6.929189456,3.009344995,2.132799448));
#96681=CARTESIAN_POINT('Ctrl Pts',(-6.812423898,2.943588707,2.512155639));
#96682=CARTESIAN_POINT('Ctrl Pts',(-6.654942689,2.878703203,2.87649749));
#96683=CARTESIAN_POINT('Ctrl Pts',(-7.236629169,3.009344995,1.970075703));
#96684=CARTESIAN_POINT('Ctrl Pts',(-7.128772338,2.943588707,2.366263468));
#96685=CARTESIAN_POINT('Ctrl Pts',(-6.978309144,2.878703203,2.748308842));
#96686=CARTESIAN_POINT('',(-6.65494267496771,2.8787032034983,2.87649748235107));
#96687=CARTESIAN_POINT('',(-6.81662591853887,2.87870320212873,2.81240316105823));
#96688=CARTESIAN_POINT('Origin',(0.190166153774641,3.08923059048807,-0.0446177339177142));
#96689=CARTESIAN_POINT('Ctrl Pts',(-6.66439419721484,2.87421362532376,2.8484083398753));
#96690=CARTESIAN_POINT('Ctrl Pts',(-6.65902749986735,2.87645841416188,2.86083608265768));
#96691=CARTESIAN_POINT('Ctrl Pts',(-6.65366080252,2.878703203,2.87326382544));
#96692=CARTESIAN_POINT('Ctrl Pts',(-6.49752192928999,2.944013165,3.23483699218));
#96693=CARTESIAN_POINT('Ctrl Pts',(-6.30312100693,3.00933735,3.57736112926));
#96694=CARTESIAN_POINT('Ctrl Pts',(-6.66568816340659,2.87421362532376,2.85163721580676));
#96695=CARTESIAN_POINT('Ctrl Pts',(-6.66031542620323,2.87645841416188,2.8640673529034));
#96696=CARTESIAN_POINT('Ctrl Pts',(-6.65494268900001,2.878703203,2.87649749));
#96697=CARTESIAN_POINT('Ctrl Pts',(-6.498628092,2.944013165,3.238140317));
#96698=CARTESIAN_POINT('Ctrl Pts',(-6.304044932,3.00933735,3.580714662));
#96699=CARTESIAN_POINT('Ctrl Pts',(-6.7953493351026,2.87421362532376,3.17518495546575));
#96700=CARTESIAN_POINT('Ctrl Pts',(-6.7893713774583,2.87645841416188,3.18785501350917));
#96701=CARTESIAN_POINT('Ctrl Pts',(-6.78339341981402,2.878703203,3.20052507155262));
#96702=CARTESIAN_POINT('Ctrl Pts',(-6.60947051893528,2.944013165,3.5691481666538));
#96703=CARTESIAN_POINT('Ctrl Pts',(-6.3966263362901,3.00933735,3.91675356870704));
#96704=CARTESIAN_POINT('',(-6.78313134128405,2.87870320364628,3.19986393784715));
#96705=CARTESIAN_POINT('',(-6.52364787174035,2.96915797895534,3.70027275209121));
#96706=CARTESIAN_POINT('Origin',(0.169668427901872,2.94642847961565,-0.092047134371907));
#96707=CARTESIAN_POINT('',(-6.30636142167441,3.00855922005457,3.57663330547928));
#96708=CARTESIAN_POINT('Ctrl Pts',(-6.30636141925212,3.00855921911747,3.57663330943115));
#96709=CARTESIAN_POINT('Ctrl Pts',(-6.34254230674416,3.00166370044041,3.59717518928132));
#96710=CARTESIAN_POINT('Ctrl Pts',(-6.37875930532485,2.99493785105421,3.61776185602894));
#96711=CARTESIAN_POINT('Ctrl Pts',(-6.45117555386215,2.9818149566436,3.65896921127782));
#96712=CARTESIAN_POINT('Ctrl Pts',(-6.48741633343306,2.97541039173818,3.67961353455249));
#96713=CARTESIAN_POINT('Ctrl Pts',(-6.52364787265427,2.96915797895447,3.70027275048276));
#96714=CARTESIAN_POINT('Origin',(0.178440093734214,2.94642876048637,-0.0893582737752734));
#96715=CARTESIAN_POINT('',(-6.7190370179336,2.87870320492457,3.03818070708917));
#96716=CARTESIAN_POINT('Origin',(-2.69315819645399E-13,2.97023924200022,
1.02565525517129E-13));
#96717=CARTESIAN_POINT('',(-6.52004540366864,2.78894740123955,3.70661677740616));
#96718=CARTESIAN_POINT('Ctrl Pts',(-6.52004540174397,2.78894740037085,3.70661678078457));
#96719=CARTESIAN_POINT('Ctrl Pts',(-6.55418766686882,2.79982120461768,3.64655955570536));
#96720=CARTESIAN_POINT('Ctrl Pts',(-6.58745338504171,2.81065020633199,3.5861124785167));
#96721=CARTESIAN_POINT('Ctrl Pts',(-6.61983106844917,2.82142857082093,3.52531369197218));
#96722=CARTESIAN_POINT('Ctrl Pts',(-6.6767429673408,2.84037424983601,3.41844457607452));
#96723=CARTESIAN_POINT('Ctrl Pts',(-6.73122098611541,2.85947647430085,3.30990447608648));
#96724=CARTESIAN_POINT('Ctrl Pts',(-6.78313134059163,2.87870320435315,3.19986393809974));
#96725=CARTESIAN_POINT('',(-6.22435499666414,2.87870320271433,4.18418509082716));
#96726=CARTESIAN_POINT('Origin',(0.151855941409106,2.94640463093673,-0.115181421971133));
#96727=CARTESIAN_POINT('Origin',(0.171865247837747,3.0892087258185,-0.0754017748086588));
#96728=CARTESIAN_POINT('Ctrl Pts',(-6.308700021,3.009344995,3.572506689));
#96729=CARTESIAN_POINT('Ctrl Pts',(-6.113114009,2.943588707,3.9178926));
#96730=CARTESIAN_POINT('Ctrl Pts',(-5.880991895,2.878703203,4.239862537));
#96731=CARTESIAN_POINT('Ctrl Pts',(-6.643932759,3.009344995,3.479677786));
#96732=CARTESIAN_POINT('Ctrl Pts',(-6.453428903,2.943588707,3.84341687));
#96733=CARTESIAN_POINT('Ctrl Pts',(-6.224354992,2.878703203,4.184185097));
#96734=CARTESIAN_POINT('',(-5.88099188278071,2.87870320349035,4.23986252603742));
#96735=CARTESIAN_POINT('',(-6.05267344655354,2.87870320212873,4.21202381261207));
#96736=CARTESIAN_POINT('Origin',(0.176128705036702,3.08923060890683,-0.0844547233562909));
#96737=CARTESIAN_POINT('Ctrl Pts',(-5.89626076918051,2.87421362531623,4.21446189044749));
#96738=CARTESIAN_POINT('Ctrl Pts',(-5.8883479448953,2.87645841415811,4.22544539823875));
#96739=CARTESIAN_POINT('Ctrl Pts',(-5.88043512061,2.878703203,4.23642890603));
#96740=CARTESIAN_POINT('Ctrl Pts',(-5.65021914495,2.944013165,4.5559834508));
#96741=CARTESIAN_POINT('Ctrl Pts',(-5.38673064420001,3.00933735,4.84870911242));
#96742=CARTESIAN_POINT('Ctrl Pts',(-5.89683037027871,2.87421362531623,4.2178934415251));
#96743=CARTESIAN_POINT('Ctrl Pts',(-5.88891113263942,2.87645841415811,4.22887798926253));
#96744=CARTESIAN_POINT('Ctrl Pts',(-5.880991895,2.878703203,4.239862537));
#96745=CARTESIAN_POINT('Ctrl Pts',(-5.650589329,2.944013165,4.559447338));
#96746=CARTESIAN_POINT('Ctrl Pts',(-5.386912058,3.00933735,4.852182858));
#96747=CARTESIAN_POINT('Ctrl Pts',(-5.95390693554475,2.87421362531623,4.56175013290872));
#96748=CARTESIAN_POINT('Ctrl Pts',(-5.94534505127836,2.87645841415811,4.57283888788507));
#96749=CARTESIAN_POINT('Ctrl Pts',(-5.93678316701207,2.878703203,4.58392764286153));
#96750=CARTESIAN_POINT('Ctrl Pts',(-5.6876834184535,2.944013165,4.90654425277428));
#96751=CARTESIAN_POINT('Ctrl Pts',(-5.40509052821043,3.00933735,5.20026762632871));
#96752=CARTESIAN_POINT('',(-5.93666933994906,2.87870320364628,4.58322562703605));
#96753=CARTESIAN_POINT('',(-5.57567934758532,2.96915797894798,5.0161538860231));
#96754=CARTESIAN_POINT('Origin',(0.145914193178012,2.9464284750525,-0.126368748783031));
#96755=CARTESIAN_POINT('',(-5.3900517594732,3.00855922011665,4.84869489727826));
#96756=CARTESIAN_POINT('Ctrl Pts',(-5.39005175646099,3.00855921928191,4.84869490041694));
#96757=CARTESIAN_POINT('Ctrl Pts',(-5.42097085771323,3.0016637006203,4.87653434368228));
#96758=CARTESIAN_POINT('Ctrl Pts',(-5.45191559860267,2.99493785111403,4.90442529016004));
#96759=CARTESIAN_POINT('Ctrl Pts',(-5.51378045129136,2.98181495260962,4.96023661051122));
#96760=CARTESIAN_POINT('Ctrl Pts',(-5.54473604521456,2.97541038325639,4.98818899810971));
#96761=CARTESIAN_POINT('Ctrl Pts',(-5.57567934830649,2.96915797897617,5.01615388499148));
#96762=CARTESIAN_POINT('Origin',(0.15505878287245,2.9464287453994,-0.125628383698799));
#96763=CARTESIAN_POINT('',(-5.90883062166377,2.87870320492457,4.41154407590484));
#96764=CARTESIAN_POINT('Ctrl Pts',(-5.39322278500001,3.009344995,4.845167489));
#96765=CARTESIAN_POINT('Ctrl Pts',(-5.127961704,2.943588707,5.14043325799999));
#96766=CARTESIAN_POINT('Ctrl Pts',(-4.832052457,2.878703203,5.404976323));
#96767=CARTESIAN_POINT('Ctrl Pts',(-5.740573438,3.009344995,4.826574003));
#96768=CARTESIAN_POINT('Ctrl Pts',(-5.476330305,2.943588707,5.140856372));
#96769=CARTESIAN_POINT('Ctrl Pts',(-5.179356919,2.878703203,5.424413508));
#96770=CARTESIAN_POINT('',(-5.17935691552083,2.8787032027125,5.42441350247272));
#96771=CARTESIAN_POINT('Origin',(0.151636229114196,3.08920894165074,-0.110583258555224));
#96772=CARTESIAN_POINT('',(-4.83205244725023,2.87870320348952,5.40497631046383));
#96773=CARTESIAN_POINT('',(-5.00570469192539,2.87870320212873,5.41469491187111));
#96774=CARTESIAN_POINT('Origin',(0.153855660404065,3.0892305891035,-0.120342688878163));
#96775=CARTESIAN_POINT('Origin',(-8.52182907573606E-13,2.97023924199978,
7.3595643468316E-13));
#96776=CARTESIAN_POINT('',(-5.57079732493957,2.78894740126208,5.02157516776139));
#96777=CARTESIAN_POINT('Ctrl Pts',(-5.57079732239725,2.78894740042159,5.02157517044124));
#96778=CARTESIAN_POINT('Ctrl Pts',(-5.61705188831202,2.79982120464436,4.97026162768222));
#96779=CARTESIAN_POINT('Ctrl Pts',(-5.66253420719846,2.81065020634201,4.91837891565976));
#96780=CARTESIAN_POINT('Ctrl Pts',(-5.70722486025001,2.82142857081912,4.86596181587965));
#96781=CARTESIAN_POINT('Ctrl Pts',(-5.7857798915122,2.84037424983099,4.77382561681668));
#96782=CARTESIAN_POINT('Ctrl Pts',(-5.86231715742168,2.85947647430087,4.6795342873684));
#96783=CARTESIAN_POINT('Ctrl Pts',(-5.93666933920597,2.87870320435315,4.58322562705654));
#96784=CARTESIAN_POINT('Origin',(0.12354331983747,2.94640418831007,-0.145131449832491));
#96785=CARTESIAN_POINT('Ctrl Pts',(-4.85242474194373,2.87421362524044,5.38345188573344));
#96786=CARTESIAN_POINT('Ctrl Pts',(-4.84233578539689,2.87645841412021,5.39247758205179));
#96787=CARTESIAN_POINT('Ctrl Pts',(-4.83224682884999,2.878703203,5.40150327837001));
#96788=CARTESIAN_POINT('Ctrl Pts',(-4.538718393,2.944013165,5.66409718592));
#96789=CARTESIAN_POINT('Ctrl Pts',(-4.21846274216001,3.00933735,5.89333684504));
#96790=CARTESIAN_POINT('Ctrl Pts',(-4.85224334403582,2.87421362524044,5.38692565646078));
#96791=CARTESIAN_POINT('Ctrl Pts',(-4.84214790051791,2.87645841412021,5.39595098973046));
#96792=CARTESIAN_POINT('Ctrl Pts',(-4.832052457,2.878703203,5.404976323));
#96793=CARTESIAN_POINT('Ctrl Pts',(-4.538335289,2.944013165,5.667559668));
#96794=CARTESIAN_POINT('Ctrl Pts',(-4.217893162,3.00933735,5.896768375));
#96795=CARTESIAN_POINT('Ctrl Pts',(-4.83406646628024,2.87421362524044,5.73501294467682));
#96796=CARTESIAN_POINT('Ctrl Pts',(-4.82332099939224,2.87645841412021,5.74400189885382));
#96797=CARTESIAN_POINT('Ctrl Pts',(-4.81257553250423,2.878703203,5.75299085303085));
#96798=CARTESIAN_POINT('Ctrl Pts',(-4.49994656305007,2.944013165,6.01451578350822));
#96799=CARTESIAN_POINT('Ctrl Pts',(-4.16081869483506,3.00933735,6.24062295032004));
#96800=CARTESIAN_POINT('',(-4.81261527617338,2.87870320365809,5.75228078483036));
#96801=CARTESIAN_POINT('',(-4.3669982542543,2.96915797894115,6.09748523951937));
#96802=CARTESIAN_POINT('Origin',(0.115337244766743,2.94642848604879,-0.154781540117167));
#96803=CARTESIAN_POINT('',(-4.22170926802649,3.00855922011897,5.894036904481));
#96804=CARTESIAN_POINT('Ctrl Pts',(-4.22170926388751,3.00855921923334,5.89403690726225));
#96805=CARTESIAN_POINT('Ctrl Pts',(-4.24592083658128,3.00166370058843,5.9278721725509));
#96806=CARTESIAN_POINT('Ctrl Pts',(-4.27014637778941,2.99493785108862,5.9617632487325));
#96807=CARTESIAN_POINT('Ctrl Pts',(-4.318567084774,2.9818149515275,6.02956885146576));
#96808=CARTESIAN_POINT('Ctrl Pts',(-4.34279002162138,2.97541038108071,6.0635222716142));
#96809=CARTESIAN_POINT('Ctrl Pts',(-4.36699825526788,2.96915797894033,6.09748523879675));
#96810=CARTESIAN_POINT('Origin',(0.124427177248334,2.94642874500272,-0.156024291755323));
#96811=CARTESIAN_POINT('',(-4.82233387355899,2.87870320492458,5.57862854666914));
#96812=CARTESIAN_POINT('Origin',(7.22729168178837E-13,2.97023924200044,
-9.77082997843937E-13));
#96813=CARTESIAN_POINT('',(-3.8921778798055,2.87870320271433,6.41100236735067));
#96814=CARTESIAN_POINT('Origin',(0.124320393650231,3.08920869069784,-0.140597308569476));
#96815=CARTESIAN_POINT('',(-4.36106495481666,2.78894740129025,6.1017302840077));
#96816=CARTESIAN_POINT('Ctrl Pts',(-4.36106495490976,2.7889474010463,6.10173028407192));
#96817=CARTESIAN_POINT('Ctrl Pts',(-4.41726900647749,2.7998212046449,6.06155979027827));
#96818=CARTESIAN_POINT('Ctrl Pts',(-4.47284122357436,2.81065020634812,6.02066742140645));
#96819=CARTESIAN_POINT('Ctrl Pts',(-4.52775516105136,2.8214285708076,5.97908297344064));
#96820=CARTESIAN_POINT('Ctrl Pts',(-4.62428017742959,2.84037424955422,5.90598787681786));
#96821=CARTESIAN_POINT('Ctrl Pts',(-4.71929789205897,2.85947647380709,5.8303542776607));
#96822=CARTESIAN_POINT('Ctrl Pts',(-4.81261527495825,2.87870320360758,5.75228078336553));
#96823=CARTESIAN_POINT('Origin',(0.0894574475054982,2.94640462797529,-0.168298699732703));
#96824=CARTESIAN_POINT('Ctrl Pts',(-4.225564445,3.009344995,5.891273642));
#96825=CARTESIAN_POINT('Ctrl Pts',(-3.903031608,2.943588707,6.12261297));
#96826=CARTESIAN_POINT('Ctrl Pts',(-3.557171616,2.878703203,6.317359424));
#96827=CARTESIAN_POINT('Ctrl Pts',(-4.568791283,3.009344995,5.94778498400001));
#96828=CARTESIAN_POINT('Ctrl Pts',(-4.243164588,2.943588707,6.197915143));
#96829=CARTESIAN_POINT('Ctrl Pts',(-3.892177873,2.878703203,6.411002371));
#96830=CARTESIAN_POINT('',(-3.55717160955683,2.8787032034775,6.31735940957115));
#96831=CARTESIAN_POINT('Origin',(0.124388509564735,3.08923057516672,-0.150603615695601));
#96832=CARTESIAN_POINT('',(-3.72467474911375,2.87870320212873,6.36418089479977));
#96833=CARTESIAN_POINT('Ctrl Pts',(-3.58169472559154,2.87421362531487,6.30071765536191));
#96834=CARTESIAN_POINT('Ctrl Pts',(-3.5699013855308,2.87645841415743,6.30736350839607));
#96835=CARTESIAN_POINT('Ctrl Pts',(-3.55810804547,2.878703203,6.31400936143));
#96836=CARTESIAN_POINT('Ctrl Pts',(-3.21499221354,2.944013165,6.50736403287));
#96837=CARTESIAN_POINT('Ctrl Pts',(-2.8529442122,3.00933735,6.6623986972));
#96838=CARTESIAN_POINT('Ctrl Pts',(-3.58077081065103,2.87421362531487,6.30407121606779));
#96839=CARTESIAN_POINT('Ctrl Pts',(-3.56897121332551,2.87645841415743,6.31071532003394));
#96840=CARTESIAN_POINT('Ctrl Pts',(-3.557171616,2.878703203,6.317359424));
#96841=CARTESIAN_POINT('Ctrl Pts',(-3.213873735,2.944013165,6.51066320800001));
#96842=CARTESIAN_POINT('Ctrl Pts',(-2.851650271,3.00933735,6.66562755700001));
#96843=CARTESIAN_POINT('Ctrl Pts',(-3.48819042137566,2.87421362531487,6.6401129250722));
#96844=CARTESIAN_POINT('Ctrl Pts',(-3.47576381827483,2.87645841415743,6.64658176465065));
#96845=CARTESIAN_POINT('Ctrl Pts',(-3.46333721517399,2.878703203,6.65305060422911));
#96846=CARTESIAN_POINT('Ctrl Pts',(-3.10179720708204,2.944013165,6.84125524024739));
#96847=CARTESIAN_POINT('Ctrl Pts',(-2.72199160358739,3.00933735,6.98917368021653));
#96848=CARTESIAN_POINT('',(-3.46352867565415,2.87870320365576,6.65236567872762));
#96849=CARTESIAN_POINT('',(-2.95412117554173,2.96915797898617,6.89370496034624));
#96850=CARTESIAN_POINT('Origin',(0.0793673339405909,2.9464285207357,-0.175957075573957));
#96851=CARTESIAN_POINT('',(-2.8559643433261,3.00855922006514,6.66378029754188));
#96852=CARTESIAN_POINT('Ctrl Pts',(-2.85596433928434,3.00855921920204,6.6637802991163));
#96853=CARTESIAN_POINT('Ctrl Pts',(-2.87233627702716,3.00166370051212,6.70202928740138));
#96854=CARTESIAN_POINT('Ctrl Pts',(-2.88870985871751,2.9949378510811,6.74033578394761));
#96855=CARTESIAN_POINT('Ctrl Pts',(-2.92142231603079,2.98181495151758,6.81696515014832));
#96856=CARTESIAN_POINT('Ctrl Pts',(-2.93777995225721,2.97541038108882,6.85533197352984));
#96857=CARTESIAN_POINT('Ctrl Pts',(-2.95412117667018,2.96915797898535,6.89370495986555));
#96858=CARTESIAN_POINT('Origin',(0.0879774927772421,2.94642876675558,-0.179124625771928));
#96859=CARTESIAN_POINT('',(-3.51035015303056,2.87870320492457,6.48486254679966));
#96860=CARTESIAN_POINT('Origin',(1.82145964977565E-14,2.97023924199967,
1.08853898117545E-13));
#96861=CARTESIAN_POINT('',(-2.94741403486527,2.78894740127924,6.89657527394928));
#96862=CARTESIAN_POINT('Ctrl Pts',(-2.94741403109273,2.78894740037632,6.89657527581036));
#96863=CARTESIAN_POINT('Ctrl Pts',(-3.01093953572611,2.79982120463271,6.86942615381304));
#96864=CARTESIAN_POINT('Ctrl Pts',(-3.07400315581137,2.81065020634479,6.84143620967188));
#96865=CARTESIAN_POINT('Ctrl Pts',(-3.1365726630489,2.82142857082642,6.81262885629397));
#96866=CARTESIAN_POINT('Ctrl Pts',(-3.24655426490462,2.84037424985116,6.76199270720585));
#96867=CARTESIAN_POINT('Ctrl Pts',(-3.35560950750758,2.85947647430088,6.7085533784839));
#96868=CARTESIAN_POINT('Ctrl Pts',(-3.4635286766403,2.87870320435315,6.65236567688422));
#96869=CARTESIAN_POINT('',(-2.42300492243708,2.87870320271434,7.09781988690226));
#96870=CARTESIAN_POINT('Origin',(0.0511867594797774,2.9464046138362,-0.183594736941044));
#96871=CARTESIAN_POINT('Origin',(0.09118953595046,3.08920869532132,-0.164035303891673));
#96872=CARTESIAN_POINT('Ctrl Pts',(-2.860323408,3.009344995,6.661910387));
#96873=CARTESIAN_POINT('Ctrl Pts',(-2.495600093,2.943588707,6.818506104));
#96874=CARTESIAN_POINT('Ctrl Pts',(-2.115961384,2.878703203,6.93434982));
#96875=CARTESIAN_POINT('Ctrl Pts',(-3.183377525,3.009344995,6.79088415));
#96876=CARTESIAN_POINT('Ctrl Pts',(-2.811593211,2.943588707,6.965166291));
#96877=CARTESIAN_POINT('Ctrl Pts',(-2.423004915,2.878703203,7.097819889));
#96878=CARTESIAN_POINT('',(-2.11596138092829,2.8787032035214,6.93434980424421));
#96879=CARTESIAN_POINT('',(-2.26948315458636,2.87870320212873,7.01608485285472));
#96880=CARTESIAN_POINT('Origin',(0.0891050703775054,3.08923060677095,-0.173822507783961));
#96881=CARTESIAN_POINT('Ctrl Pts',(-2.14348864496989,2.87421362536565,6.92336887051515));
#96882=CARTESIAN_POINT('Ctrl Pts',(-2.13054236483491,2.87645841418282,6.92732412760264));
#96883=CARTESIAN_POINT('Ctrl Pts',(-2.1175960847,2.878703203,6.93127938469));
#96884=CARTESIAN_POINT('Ctrl Pts',(-1.74093657126,2.944013165,7.04635376857));
#96885=CARTESIAN_POINT('Ctrl Pts',(-1.35402518099,3.00933735,7.11993419126));
#96886=CARTESIAN_POINT('Ctrl Pts',(-2.14186541422007,2.87421362536565,6.92644541242972));
#96887=CARTESIAN_POINT('Ctrl Pts',(-2.12891339911001,2.87645841418282,6.93039761621492));
#96888=CARTESIAN_POINT('Ctrl Pts',(-2.115961384,2.878703203,6.93434982));
#96889=CARTESIAN_POINT('Ctrl Pts',(-1.739135017,2.944013165,7.049335371));
#96890=CARTESIAN_POINT('Ctrl Pts',(-1.352067382,3.00933735,7.122809403));
#96891=CARTESIAN_POINT('Ctrl Pts',(-1.97921046829331,2.87421362536565,7.23472860556921));
#96892=CARTESIAN_POINT('Ctrl Pts',(-1.96568378315297,2.87645841418282,7.23837485487639));
#96893=CARTESIAN_POINT('Ctrl Pts',(-1.95215709801269,2.878703203,7.24202110418358));
#96894=CARTESIAN_POINT('Ctrl Pts',(-1.55861126165646,2.944013165,7.34810520522359));
#96895=CARTESIAN_POINT('Ctrl Pts',(-1.15588720928481,3.00933735,7.41091841655401));
#96896=CARTESIAN_POINT('',(-1.95249132098841,2.87870320365575,7.24139335021025));
#96897=CARTESIAN_POINT('',(-1.40311267351616,2.96915797892996,7.36758269877179));
#96898=CARTESIAN_POINT('Origin',(0.0396862188766633,2.94642847507453,-0.188904990300104));
#96899=CARTESIAN_POINT('',(-1.35667770072638,3.00855922010768,7.12193272850302));
#96900=CARTESIAN_POINT('Ctrl Pts',(-1.35667769588376,3.00855921925971,7.12193272928015));
#96901=CARTESIAN_POINT('Ctrl Pts',(-1.36444446482813,3.00166370057974,7.16280696003061));
#96902=CARTESIAN_POINT('Ctrl Pts',(-1.37220047685128,2.99493785109333,7.20373770835499));
#96903=CARTESIAN_POINT('Ctrl Pts',(-1.38767508043678,2.98181495662563,7.2856077020983));
#96904=CARTESIAN_POINT('Ctrl Pts',(-1.39540254430737,2.97541039165304,7.32659390134666));
#96905=CARTESIAN_POINT('Ctrl Pts',(-1.40311267532109,2.96915797893043,7.36758269842035));
#96906=CARTESIAN_POINT('Origin',(0.0474141165200966,2.94642877611754,-0.193849341569747));
#96907=CARTESIAN_POINT('',(-2.03422636050977,2.87870320492457,7.08787158219669));
#96908=CARTESIAN_POINT('Origin',(-1.15142270717961E-13,2.97023924199922,
8.89479462307108E-13));
#96909=CARTESIAN_POINT('',(-1.39594530977002,2.78894740124346,7.36894406900654));
#96910=CARTESIAN_POINT('Ctrl Pts',(-1.39594530611969,2.78894740040204,7.36894406960381));
#96911=CARTESIAN_POINT('Ctrl Pts',(-1.46382187831905,2.79982120463159,7.35608578463714));
#96912=CARTESIAN_POINT('Ctrl Pts',(-1.53142811658635,2.81065020633578,7.34230704400092));
#96913=CARTESIAN_POINT('Ctrl Pts',(-1.59872751298941,2.82142857082903,7.32762378513747));
#96914=CARTESIAN_POINT('Ctrl Pts',(-1.71702308128857,2.84037424985837,7.3018142747674));
#96915=CARTESIAN_POINT('Ctrl Pts',(-1.83501654880148,2.85947647430087,7.27306798144716));
#96916=CARTESIAN_POINT('Ctrl Pts',(-1.95249132234644,2.87870320435315,7.24139334862288));
#96917=CARTESIAN_POINT('',(-0.840534948682288,2.87870320271433,7.45275123752289));
#96918=CARTESIAN_POINT('Origin',(0.0105225791164858,2.94640460981423,-0.190305859621067));
#96919=CARTESIAN_POINT('Origin',(0.0537948407192751,3.08920870227923,-0.179803285374214));
#96920=CARTESIAN_POINT('Ctrl Pts',(-1.361336828,3.009344995,7.121043606));
#96921=CARTESIAN_POINT('Ctrl Pts',(-0.971477090999999,2.943588707,7.195573471));
#96922=CARTESIAN_POINT('Ctrl Pts',(-0.575811149,2.878703203,7.227097725));
#96923=CARTESIAN_POINT('Ctrl Pts',(-1.649112573,3.009344995,7.31644912000001));
#96924=CARTESIAN_POINT('Ctrl Pts',(-1.248554861,2.943588707,7.406734004));
#96925=CARTESIAN_POINT('Ctrl Pts',(-0.840534941,2.878703203,7.45275123800001));
#96926=CARTESIAN_POINT('',(-0.575811149137818,2.87870320291937,7.22709770862388));
#96927=CARTESIAN_POINT('',(-0.708173050321132,2.87870320212873,7.33992448098661));
#96928=CARTESIAN_POINT('Origin',(0.0496551467651213,3.0892306107498,-0.188913537216816));
#96929=CARTESIAN_POINT('Origin',(1.01210272801522E-13,2.97023924199933,
1.20823490101785E-12));
#96930=CARTESIAN_POINT('',(0.220796265851409,2.78894740126403,7.49674922941047));
#96931=CARTESIAN_POINT('',(-0.350157643002028,2.87870320365575,7.49182151673046));
#96932=CARTESIAN_POINT('Ctrl Pts',(0.220796270213487,2.78894740034443,7.49674922963154));
#96933=CARTESIAN_POINT('Ctrl Pts',(0.151742463241555,2.79982120461821,7.49878302093711));
#96934=CARTESIAN_POINT('Ctrl Pts',(0.0827547993552023,2.8106502063407,7.49985976246062));
#96935=CARTESIAN_POINT('Ctrl Pts',(0.0138723589321241,2.82142857082974,
7.49998717083208));
#96936=CARTESIAN_POINT('Ctrl Pts',(-0.107205806614306,2.84037424986034,
7.50021112251022));
#96937=CARTESIAN_POINT('Ctrl Pts',(-0.22862025575631,2.85947647430103,7.49750200929462));
#96938=CARTESIAN_POINT('Ctrl Pts',(-0.3501576446624,2.87870320435365,7.49182151547619));
#96939=CARTESIAN_POINT('Origin',(-0.0306335706352003,2.94640463429058,-0.188118757514659));
#96940=CARTESIAN_POINT('Origin',(-0.00185061631441531,2.94642847975205,
-0.193019681328986));
#96941=CARTESIAN_POINT('Ctrl Pts',(-0.605055418118393,2.87421362524808,
7.22229105134406));
#96942=CARTESIAN_POINT('Ctrl Pts',(-0.591561551124188,2.87645841412404,
7.22337076921714));
#96943=CARTESIAN_POINT('Ctrl Pts',(-0.57806768413,2.878703203,7.22445048709));
#96944=CARTESIAN_POINT('Ctrl Pts',(-0.18547667031,2.944013165,7.25586383469));
#96945=CARTESIAN_POINT('Ctrl Pts',(0.20820656273,3.00933735,7.24454947603));
#96946=CARTESIAN_POINT('Ctrl Pts',(-0.602808772038777,2.87421362524808,
7.22494671879012));
#96947=CARTESIAN_POINT('Ctrl Pts',(-0.589309960519383,2.87645841412404,
7.22602222189512));
#96948=CARTESIAN_POINT('Ctrl Pts',(-0.575811149000001,2.878703203,7.227097725));
#96949=CARTESIAN_POINT('Ctrl Pts',(-0.183076279,2.944013165,7.258388448));
#96950=CARTESIAN_POINT('Ctrl Pts',(0.210736675,3.00933735,7.246936598));
#96951=CARTESIAN_POINT('Ctrl Pts',(-0.377684835310627,2.87421362524809,
7.49105641693585));
#96952=CARTESIAN_POINT('Ctrl Pts',(-0.363690560359198,2.87645841412404,
7.49170958152752));
#96953=CARTESIAN_POINT('Ctrl Pts',(-0.349696285407776,2.878703203,7.49236274611927));
#96954=CARTESIAN_POINT('Ctrl Pts',(0.0574536141147641,2.944013165,7.51136593841193));
#96955=CARTESIAN_POINT('Ctrl Pts',(0.464265185679141,3.00933735,7.48613684418653));
#96956=CARTESIAN_POINT('Origin',(0.00463374273094159,2.94642873394642,-0.199509935818043));
#96957=CARTESIAN_POINT('',(-0.46298440445079,2.87870320492457,7.35945961974818));
#96958=CARTESIAN_POINT('Ctrl Pts',(-1.18865511349561,3.01309343441768,7.4057932170506));
#96959=CARTESIAN_POINT('Ctrl Pts',(-1.17466739473715,3.01082632770884,7.40798415865071));
#96960=CARTESIAN_POINT('Ctrl Pts',(-1.16067967597869,3.008559221,7.41017510025082));
#96961=CARTESIAN_POINT('Ctrl Pts',(-0.755006818590786,2.942808424,7.47371695111569));
#96962=CARTESIAN_POINT('Ctrl Pts',(-0.344821887743239,2.877933005,7.49259435614662));
#96963=CARTESIAN_POINT('Ctrl Pts',(-1.38356493866731,3.01309343441768,7.1168108876801));
#96964=CARTESIAN_POINT('Ctrl Pts',(-1.37012131683364,3.01082632770884,7.11937180234004));
#96965=CARTESIAN_POINT('Ctrl Pts',(-1.356677695,3.008559221,7.121932717));
#96966=CARTESIAN_POINT('Ctrl Pts',(-0.966784777,2.942808424,7.196204554));
#96967=CARTESIAN_POINT('Ctrl Pts',(-0.571114157,2.877933005,7.227470416));
#96968=CARTESIAN_POINT('',(-0.597132064613574,2.91791835922337,7.47619110706827));
#96969=CARTESIAN_POINT('Ctrl Pts',(-0.597132067174111,2.91791835924552,
7.4761910949071));
#96970=CARTESIAN_POINT('Ctrl Pts',(-0.593617782586462,2.91168301766321,
7.43463380428372));
#96971=CARTESIAN_POINT('Ctrl Pts',(-0.590083571577411,2.90530192562621,
7.39307657483869));
#96972=CARTESIAN_POINT('Ctrl Pts',(-0.58297921601715,2.89224022492298,7.31005814253514));
#96973=CARTESIAN_POINT('Ctrl Pts',(-0.579405192990811,2.88555248749285,
7.26855156492777));
#96974=CARTESIAN_POINT('Ctrl Pts',(-0.575811147778446,2.87870320302431,
7.22709772429943));
#96975=CARTESIAN_POINT('',(-1.16108395640224,3.00855922016356,7.40958056024041));
#96976=CARTESIAN_POINT('Origin',(0.0421309665231484,3.08925205799903,-0.185224272254657));
#96977=CARTESIAN_POINT('',(-1.25888083740932,3.00855921853322,7.26575663541678));
#96978=CARTESIAN_POINT('Ctrl Pts',(-2.43066974068,2.877925369,7.09788290211));
#96979=CARTESIAN_POINT('Ctrl Pts',(-2.04495695187,2.943232886,7.22997023301));
#96980=CARTESIAN_POINT('Ctrl Pts',(-1.64720201441,3.008559221,7.31948240046));
#96981=CARTESIAN_POINT('Ctrl Pts',(-2.427598248,2.877925369,7.096250189));
#96982=CARTESIAN_POINT('Ctrl Pts',(-2.041974184,2.943232886,7.228170609));
#96983=CARTESIAN_POINT('Ctrl Pts',(-1.644325536,3.008559221,7.317526463));
#96984=CARTESIAN_POINT('Ctrl Pts',(-2.12044898,2.877925369,6.932978878));
#96985=CARTESIAN_POINT('Ctrl Pts',(-1.743697397,2.943232886,7.048208208));
#96986=CARTESIAN_POINT('Ctrl Pts',(-1.356677695,3.008559221,7.121932717));
#96987=CARTESIAN_POINT('',(-1.64432554279485,3.00855922118749,7.31752646662718));
#96988=CARTESIAN_POINT('',(-1.50050161853982,3.00855922150568,7.21972958936822));
#96989=CARTESIAN_POINT('',(-2.1903315442912,2.917918359213,7.17303617034655));
#96990=CARTESIAN_POINT('Origin',(0.0519544797057715,2.94642873241194,-0.185783815546355));
#96991=CARTESIAN_POINT('Ctrl Pts',(-2.11596138347576,2.87870320309923,6.9343498203138));
#96992=CARTESIAN_POINT('Ctrl Pts',(-2.12838275208153,2.88555248752913,6.97406187955045));
#96993=CARTESIAN_POINT('Ctrl Pts',(-2.14079590348602,2.89224022492635,7.01382974697511));
#96994=CARTESIAN_POINT('Ctrl Pts',(-2.16558061665956,2.9053018965811,7.09337985114029));
#96995=CARTESIAN_POINT('Ctrl Pts',(-2.17796571374631,2.91168295872474,7.13320554516882));
#96996=CARTESIAN_POINT('Ctrl Pts',(-2.19033154210413,2.9179183592551,7.17303615867629));
#96997=CARTESIAN_POINT('Ctrl Pts',(-2.75289164401948,3.0130934341647,6.97712417439583));
#96998=CARTESIAN_POINT('Ctrl Pts',(-2.73970193875433,3.01082632758236,6.98227083876427));
#96999=CARTESIAN_POINT('Ctrl Pts',(-2.72651223348926,3.008559221,6.98741750313253));
#97000=CARTESIAN_POINT('Ctrl Pts',(-2.34398340131143,2.942808424,7.13668145337599));
#97001=CARTESIAN_POINT('Ctrl Pts',(-1.94744645126371,2.877933005,7.24329515157678));
#97002=CARTESIAN_POINT('Ctrl Pts',(-2.88112192756206,3.0130934341647,6.65299824119357));
#97003=CARTESIAN_POINT('Ctrl Pts',(-2.86854313178099,3.01082632758236,6.65838926409685));
#97004=CARTESIAN_POINT('Ctrl Pts',(-2.855964336,3.008559221,6.663780287));
#97005=CARTESIAN_POINT('Ctrl Pts',(-2.491153147,2.942808424,6.820131142));
#97006=CARTESIAN_POINT('Ctrl Pts',(-2.111454323,2.877933005,6.935723513));
#97007=CARTESIAN_POINT('',(-2.7267792535095,3.00855922016357,6.98674995484222));
#97008=CARTESIAN_POINT('Origin',(0.0809638181095518,3.08925204475167,-0.171837215531635));
#97009=CARTESIAN_POINT('',(-2.79137180550544,3.00855921853322,6.82526511527211));
#97010=CARTESIAN_POINT('Origin',(-1.18069616583671E-13,3.10034167700022,
4.57099635919889E-13));
#97011=CARTESIAN_POINT('',(-2.19083234810381,3.09925366546078,7.17288321534975));
#97012=CARTESIAN_POINT('Origin',(0.0548153802264575,3.08928542089756,-0.18492601784178));
#97013=CARTESIAN_POINT('Origin',(0.0785761698327736,2.94644891567482,-0.173890755843731));
#97014=CARTESIAN_POINT('Ctrl Pts',(-3.89967704495,2.877925369,6.40941620005));
#97015=CARTESIAN_POINT('Ctrl Pts',(-3.55137687838,2.943232886,6.62133224987));
#97016=CARTESIAN_POINT('Ctrl Pts',(-3.18216370068,3.008559221,6.79425722689));
#97017=CARTESIAN_POINT('Ctrl Pts',(-3.896326377,2.877925369,6.408481939));
#97018=CARTESIAN_POINT('Ctrl Pts',(-3.54807698,2.943232886,6.620215907));
#97019=CARTESIAN_POINT('Ctrl Pts',(-3.178934004,3.008559221,6.792965376));
#97020=CARTESIAN_POINT('Ctrl Pts',(-3.561259582,2.877925369,6.315055834));
#97021=CARTESIAN_POINT('Ctrl Pts',(-3.218087142,2.943232886,6.50858162000001));
#97022=CARTESIAN_POINT('Ctrl Pts',(-2.855964336,3.008559221,6.663780287));
#97023=CARTESIAN_POINT('',(-3.17893401143054,3.00855922118749,6.79296537808149));
#97024=CARTESIAN_POINT('',(-3.0174491728329,3.00855922150568,6.72837283022954));
#97025=CARTESIAN_POINT('',(-3.68111355336686,2.91791835921217,6.5344780342737));
#97026=CARTESIAN_POINT('Origin',(0.0906779232219468,2.94642872914588,-0.170271772116001));
#97027=CARTESIAN_POINT('Ctrl Pts',(-3.55717161529236,2.8787032030457,6.31735942487094));
#97028=CARTESIAN_POINT('Ctrl Pts',(-3.57783949806911,2.88555248749211,6.35347281116653));
#97029=CARTESIAN_POINT('Ctrl Pts',(-3.59851135292373,2.89224022489924,6.38964246730138));
#97030=CARTESIAN_POINT('Ctrl Pts',(-3.6398175358269,2.90530189702292,6.4620047559652));
#97031=CARTESIAN_POINT('Ctrl Pts',(-3.66047442494779,2.91168295963675,6.49823692039235));
#97032=CARTESIAN_POINT('Ctrl Pts',(-3.68111354879359,2.91791835926664,6.53447802340237));
#97033=CARTESIAN_POINT('Ctrl Pts',(-4.1884060227692,3.01309343424243,6.22221256008111));
#97034=CARTESIAN_POINT('Ctrl Pts',(-4.17663106600069,3.01082632762121,6.23007429516647));
#97035=CARTESIAN_POINT('Ctrl Pts',(-4.16485610923219,3.008559221,6.23793603025165));
#97036=CARTESIAN_POINT('Ctrl Pts',(-3.82335792607495,2.942808424,6.4659426633839));
#97037=CARTESIAN_POINT('Ctrl Pts',(-3.45901058280773,2.877933005,6.65530751471446));
#97038=CARTESIAN_POINT('Ctrl Pts',(-4.24396085829933,3.01309343424242,5.87809879068148));
#97039=CARTESIAN_POINT('Ctrl Pts',(-4.23283505814969,3.01082632762121,5.88606784384073));
#97040=CARTESIAN_POINT('Ctrl Pts',(-4.221709258,3.008559221,5.894036897));
#97041=CARTESIAN_POINT('Ctrl Pts',(-3.899037964,2.942808424,6.125155977));
#97042=CARTESIAN_POINT('Ctrl Pts',(-3.553065231,2.877933005,6.31966988600001));
#97043=CARTESIAN_POINT('',(-4.16497338333524,3.00855922016357,6.23722668743309));
#97044=CARTESIAN_POINT('Origin',(0.116010787647586,3.08925205701893,-0.150414833038365));
#97045=CARTESIAN_POINT('',(-4.19334132994663,3.00855921853322,6.0656317843953));
#97046=CARTESIAN_POINT('Origin',(-1.18720137887163E-12,3.10034167699922,
1.91296631313342E-12));
#97047=CARTESIAN_POINT('',(-3.68156976764921,3.09925366549505,6.53422099774608));
#97048=CARTESIAN_POINT('Origin',(0.0932874242518589,3.08928540831311,-0.16881882010959));
#97049=CARTESIAN_POINT('Origin',(0.114120485973642,2.94644892506214,-0.152933755915976));
#97050=CARTESIAN_POINT('Ctrl Pts',(-5.1863397847,2.877925369,5.42125231998));
#97051=CARTESIAN_POINT('Ctrl Pts',(-4.89173836931,2.943232886,5.70308813079));
#97052=CARTESIAN_POINT('Ctrl Pts',(-4.56833094893001,3.008559221,5.95134013681));
#97053=CARTESIAN_POINT('Ctrl Pts',(-5.182866615,2.877925369,5.421060196));
#97054=CARTESIAN_POINT('Ctrl Pts',(-4.88827564,2.943232886,5.70270726800001));
#97055=CARTESIAN_POINT('Ctrl Pts',(-4.564899051,3.008559221,5.950772778));
#97056=CARTESIAN_POINT('Ctrl Pts',(-4.835549645,2.877925369,5.401847798));
#97057=CARTESIAN_POINT('Ctrl Pts',(-4.542002709,2.943232886,5.664620989));
#97058=CARTESIAN_POINT('Ctrl Pts',(-4.221709258,3.008559221,5.894036897));
#97059=CARTESIAN_POINT('',(-4.56489905631851,3.00855922118773,5.95077277945273));
#97060=CARTESIAN_POINT('',(-4.39330415699359,3.00855922150568,5.92240483565023));
#97061=CARTESIAN_POINT('',(-4.9997707835736,2.91791835921264,5.59037496809944));
#97062=CARTESIAN_POINT('Origin',(0.125161223023473,2.94642873590838,-0.146797725607164));
#97063=CARTESIAN_POINT('Ctrl Pts',(-4.83205245536977,2.87870320302285,5.40497632402961));
#97064=CARTESIAN_POINT('Ctrl Pts',(-4.86000044535219,2.88555248748605,5.43580241560536));
#97065=CARTESIAN_POINT('Ctrl Pts',(-4.88796441085964,2.89224022491598,5.46668260764667));
#97066=CARTESIAN_POINT('Ctrl Pts',(-4.94386062906873,2.90530189649512,5.52847349533871));
#97067=CARTESIAN_POINT('Ctrl Pts',(-4.97182341329659,2.91168295853286,5.55941794837993));
#97068=CARTESIAN_POINT('Ctrl Pts',(-4.99977077667311,2.91791835925263,5.59037495841998));
#97069=CARTESIAN_POINT('Ctrl Pts',(-5.42807519061426,3.01309343423535,5.17635720193932));
#97070=CARTESIAN_POINT('Ctrl Pts',(-5.41826556645109,3.01082632761767,5.18656640164015));
#97071=CARTESIAN_POINT('Ctrl Pts',(-5.40845594228794,3.008559221,5.1967756013411));
#97072=CARTESIAN_POINT('Ctrl Pts',(-5.12395648294645,2.942808424,5.49286358054539));
#97073=CARTESIAN_POINT('Ctrl Pts',(-4.80883522363903,2.877933005,5.75612509561966));
#97074=CARTESIAN_POINT('Ctrl Pts',(-5.40835689648362,3.01309343423534,4.82834597343307));
#97075=CARTESIAN_POINT('Ctrl Pts',(-5.39920432224181,3.01082632761767,4.83852043271648));
#97076=CARTESIAN_POINT('Ctrl Pts',(-5.390051748,3.008559221,4.848694892));
#97077=CARTESIAN_POINT('Ctrl Pts',(-5.1246081,2.942808424,5.143775327));
#97078=CARTESIAN_POINT('Ctrl Pts',(-4.828538757,2.877933005,5.408115519));
#97079=CARTESIAN_POINT('',(-5.40841798704712,3.00855922016356,5.19605763176611));
#97080=CARTESIAN_POINT('Origin',(0.145633308193763,3.08925205901162,-0.121959380627193));
#97081=CARTESIAN_POINT('',(-5.39923487480588,3.00855921853322,5.02237625242081));
#97082=CARTESIAN_POINT('Origin',(4.34981911601184E-13,3.10034167700033,
-3.37837396946483E-13));
#97083=CARTESIAN_POINT('',(-5.00016107681818,3.09925366546916,5.59002586821102));
#97084=CARTESIAN_POINT('Origin',(0.127397609977411,3.08928538692933,-0.144818061837442));
#97085=CARTESIAN_POINT('Origin',(0.144328720891362,2.94644890452984,-0.12482579074787));
#97086=CARTESIAN_POINT('Ctrl Pts',(-6.23049503990001,2.877925369,4.17959670742));
#97087=CARTESIAN_POINT('Ctrl Pts',(-6.00336761087,2.943232886,4.51817394899));
#97088=CARTESIAN_POINT('Ctrl Pts',(-5.74088811843,3.008559221,4.83014499667001));
#97089=CARTESIAN_POINT('Ctrl Pts',(-6.22706177,2.877925369,4.180155704));
#97090=CARTESIAN_POINT('Ctrl Pts',(-5.999903964,2.943232886,4.518546375));
#97091=CARTESIAN_POINT('Ctrl Pts',(-5.737414491,3.008559221,4.83032865900001));
#97092=CARTESIAN_POINT('Ctrl Pts',(-5.88373478,2.877925369,4.236055362));
#97093=CARTESIAN_POINT('Ctrl Pts',(-5.653539277,2.943232886,4.555788976));
#97094=CARTESIAN_POINT('Ctrl Pts',(-5.390051748,3.008559221,4.848694892));
#97095=CARTESIAN_POINT('',(-5.73741449864667,3.00855922118759,4.83032865776541));
#97096=CARTESIAN_POINT('',(-5.56373312153765,3.00855922150568,4.83951177315742));
#97097=CARTESIAN_POINT('',(-6.0846442887004,2.91791835921996,4.384872182072));
#97098=CARTESIAN_POINT('Origin',(0.153792080298203,2.94642869722729,-0.116459622361765));
#97099=CARTESIAN_POINT('Ctrl Pts',(-5.88099189403477,2.8787032030517,4.23986253723746));
#97100=CARTESIAN_POINT('Ctrl Pts',(-5.91491317388903,2.88555248749573,4.2639599403647));
#97101=CARTESIAN_POINT('Ctrl Pts',(-5.9488616857871,2.89224022491036,4.28810674482912));
#97102=CARTESIAN_POINT('Ctrl Pts',(-6.01673429743481,2.90530189681822,4.33643696279344));
#97103=CARTESIAN_POINT('Ctrl Pts',(-6.05069547196218,2.91168295920914,4.36064678124216));
#97104=CARTESIAN_POINT('Ctrl Pts',(-6.08464427990727,2.91791835926124,4.3848721740921));
#97105=CARTESIAN_POINT('Ctrl Pts',(-6.41393359534823,3.01309343428173,3.88846113385415));
#97106=CARTESIAN_POINT('Ctrl Pts',(-6.40654799083191,3.01082632764086,3.90054042749791));
#97107=CARTESIAN_POINT('Ctrl Pts',(-6.39916238631558,3.008559221,3.91261972114173));
#97108=CARTESIAN_POINT('Ctrl Pts',(-6.18496452966363,2.942808424,4.26294430224455));
#97109=CARTESIAN_POINT('Ctrl Pts',(-5.93380407381153,2.877933005,4.58779266509604));
#97110=CARTESIAN_POINT('Ctrl Pts',(-6.31986417743961,3.01309343428173,3.55282506371949));
#97111=CARTESIAN_POINT('Ctrl Pts',(-6.31311279321987,3.01082632764086,3.56472918285974));
#97112=CARTESIAN_POINT('Ctrl Pts',(-6.306361409,3.008559221,3.576633302));
#97113=CARTESIAN_POINT('Ctrl Pts',(-6.110557257,2.942808424,3.921877459));
#97114=CARTESIAN_POINT('Ctrl Pts',(-5.87823517799999,2.877933005,4.243683681));
#97115=CARTESIAN_POINT('',(-6.39897097620884,3.00855922016355,3.91192669654753));
#97116=CARTESIAN_POINT('Origin',(0.168446060194178,3.08925205243713,-0.0878011240636639));
#97117=CARTESIAN_POINT('',(-6.35266619768326,3.00855921853322,3.74427998846434));
#97118=CARTESIAN_POINT('Origin',(-8.53050269311595E-13,3.10034167700022,
5.52509427098613E-13));
#97119=CARTESIAN_POINT('',(-6.08495041118462,3.09925366547201,4.38444734227687));
#97120=CARTESIAN_POINT('Origin',(0.155550450068147,3.08928541145801,-0.114045366557798));
#97121=CARTESIAN_POINT('Origin',(0.167788296014985,2.94644889903272,-0.0908810507973845));
#97122=CARTESIAN_POINT('Ctrl Pts',(-6.98331927221,2.877925369,2.7425077969));
#97123=CARTESIAN_POINT('Ctrl Pts',(-6.83428605413999,2.943232886,3.12199497441));
#97124=CARTESIAN_POINT('Ctrl Pts',(-6.64500774098,3.008559221,3.48309764438));
#97125=CARTESIAN_POINT('Ctrl Pts',(-6.980086438,2.877925369,2.743791776));
#97126=CARTESIAN_POINT('Ctrl Pts',(-6.830983446,2.943232886,3.123103275));
#97127=CARTESIAN_POINT('Ctrl Pts',(-6.641654807,3.008559221,3.48402374));
#97128=CARTESIAN_POINT('Ctrl Pts',(-6.656803017,2.877925369,2.872189686));
#97129=CARTESIAN_POINT('Ctrl Pts',(-6.500722632,2.943232886,3.233933334));
#97130=CARTESIAN_POINT('Ctrl Pts',(-6.306361409,3.008559221,3.576633302));
#97131=CARTESIAN_POINT('',(-6.64165481419034,3.00855922118751,3.48402373714726));
#97132=CARTESIAN_POINT('',(-6.4740081094864,3.00855922150568,3.5303285182742));
#97133=CARTESIAN_POINT('',(-6.88500659019446,2.91791835923352,2.97433764536223));
#97134=CARTESIAN_POINT('Origin',(0.175232140451512,2.94642872746011,-0.0806762294130415));
#97135=CARTESIAN_POINT('Ctrl Pts',(-6.65494268860888,2.87870320306324,2.87649749093035));
#97136=CARTESIAN_POINT('Ctrl Pts',(-6.69325113712358,2.88555248753272,2.89273943758659));
#97137=CARTESIAN_POINT('Ctrl Pts',(-6.73159680084652,2.89224022496146,2.90902377651066));
#97138=CARTESIAN_POINT('Ctrl Pts',(-6.80827217211815,2.90530189949898,2.94163346192576));
#97139=CARTESIAN_POINT('Ctrl Pts',(-6.84664376590286,2.91168296458449,2.95797662692451));
#97140=CARTESIAN_POINT('Ctrl Pts',(-6.8850065803265,2.91791835932858,2.97433763934861));
#97141=CARTESIAN_POINT('Ctrl Pts',(-7.09988359430054,3.01309343433985,2.4187449445366));
#97142=CARTESIAN_POINT('Ctrl Pts',(-7.09526735214123,3.01082632766993,2.4321295178125));
#97143=CARTESIAN_POINT('Ctrl Pts',(-7.09065110998202,3.008559221,2.44551409108841));
#97144=CARTESIAN_POINT('Ctrl Pts',(-6.95677051003518,2.942808424,2.83369448509874));
#97145=CARTESIAN_POINT('Ctrl Pts',(-6.78131484154021,2.877933005,3.20494014832406));
#97146=CARTESIAN_POINT('Ctrl Pts',(-6.93586163283426,3.01309343433985,2.11117800370404));
#97147=CARTESIAN_POINT('Ctrl Pts',(-6.9318271259172,3.01082632766993,2.12425515935203));
#97148=CARTESIAN_POINT('Ctrl Pts',(-6.92779261899999,3.008559221,2.137332315));
#97149=CARTESIAN_POINT('Ctrl Pts',(-6.810783548,2.942808424,2.51659696));
#97150=CARTESIAN_POINT('Ctrl Pts',(-6.653071856,2.877933005,2.880821911));
#97151=CARTESIAN_POINT('',(-7.09031519513093,3.00855922016356,2.44487841651762));
#97152=CARTESIAN_POINT('Origin',(0.183382530523761,3.08925209210665,-0.0495374482622934));
#97153=CARTESIAN_POINT('',(-7.00905390970135,3.00855921853322,2.29110535411744));
#97154=CARTESIAN_POINT('Origin',(-7.01261965163624E-13,3.10034167699956,
2.68014777038417E-13));
#97155=CARTESIAN_POINT('',(-6.88521422698715,3.09925366552651,2.97385693108467));
#97156=CARTESIAN_POINT('Origin',(0.176430221718098,3.08928538933908,-0.0779403288848335));
#97157=CARTESIAN_POINT('Origin',(0.183402201308652,2.94644894544234,-0.0526867791533125));
#97158=CARTESIAN_POINT('Ctrl Pts',(-7.40961125679,2.877925369,1.17718227082));
#97159=CARTESIAN_POINT('Ctrl Pts',(-7.34564087914,2.943232886,1.57983498574));
#97160=CARTESIAN_POINT('Ctrl Pts',(-7.23841418707,3.008559221,1.97318451829));
#97161=CARTESIAN_POINT('Ctrl Pts',(-7.406730022,2.877925369,1.179131195));
#97162=CARTESIAN_POINT('Ctrl Pts',(-7.342653736,2.943232886,1.581627338));
#97163=CARTESIAN_POINT('Ctrl Pts',(-7.235338726,3.008559221,1.974809744));
#97164=CARTESIAN_POINT('Ctrl Pts',(-7.118606543,2.877925369,1.374023613));
#97165=CARTESIAN_POINT('Ctrl Pts',(-7.043939422,2.943232886,1.760862564));
#97166=CARTESIAN_POINT('Ctrl Pts',(-6.92779261900001,3.008559221,2.137332315));
#97167=CARTESIAN_POINT('',(-7.23533873110783,3.00855922118775,1.97480974195313));
#97168=CARTESIAN_POINT('',(-7.08156567336568,3.00855922150568,2.05607102651839));
#97169=CARTESIAN_POINT('',(-7.36343363499263,2.91791835920902,1.42472638692165));
#97170=CARTESIAN_POINT('Origin',(0.18847804656132,2.94642872398803,-0.0411202707498361));
#97171=CARTESIAN_POINT('Ctrl Pts',(-7.11771575797658,2.87870320295267,1.37863061942183));
#97172=CARTESIAN_POINT('Ctrl Pts',(-7.15862011480401,2.88555248745624,1.38625765429204));
#97173=CARTESIAN_POINT('Ctrl Pts',(-7.19956992987178,2.89224022491387,1.39391809020301));
#97174=CARTESIAN_POINT('Ctrl Pts',(-7.28146277411364,2.90530189659957,1.40928243761697));
#97175=CARTESIAN_POINT('Ctrl Pts',(-7.32245053844715,2.91168295872708,1.41699474627592));
#97176=CARTESIAN_POINT('Ctrl Pts',(-7.36343362367443,2.91791835925492,1.42472638344372));
#97177=CARTESIAN_POINT('Ctrl Pts',(-7.45385092630109,3.01309343452991,0.835930928663964));
#97178=CARTESIAN_POINT('Ctrl Pts',(-7.45221989688324,3.01082632776496,0.849994934267147));
#97179=CARTESIAN_POINT('Ctrl Pts',(-7.45058886746543,3.008559221,0.864058939870347));
#97180=CARTESIAN_POINT('Ctrl Pts',(-7.40328563243026,2.942808424,1.27194426389399));
#97181=CARTESIAN_POINT('Ctrl Pts',(-7.31173886264471,2.877933005,1.67222819236713));
#97182=CARTESIAN_POINT('Ctrl Pts',(-7.22754590703971,3.01309343452991,0.57081460535899));
#97183=CARTESIAN_POINT('Ctrl Pts',(-7.22641692651976,3.01082632776496,0.584453324679495));
#97184=CARTESIAN_POINT('Ctrl Pts',(-7.225287946,3.008559221,0.598092044));
#97185=CARTESIAN_POINT('Ctrl Pts',(-7.19254517,2.942808424,0.993643183999999));
#97186=CARTESIAN_POINT('Ctrl Pts',(-7.116818287,2.877933005,1.38325611));
#97187=CARTESIAN_POINT('',(-7.45012415486043,3.00855922016356,0.863510338789426));
#97188=CARTESIAN_POINT('Origin',(0.189743965845582,3.08925208532173,-0.00895742294459656));
#97189=CARTESIAN_POINT('',(-7.3377060504996,3.00855921853322,0.730801179443037));
#97190=CARTESIAN_POINT('Origin',(-6.75241113023972E-13,3.10034167700089,
9.92044987824237E-14));
#97191=CARTESIAN_POINT('',(-7.363533078059,3.09925366545442,1.42421227530059));
#97192=CARTESIAN_POINT('Origin',(0.189060473729974,3.08928542070922,-0.0381908852368218));
#97193=CARTESIAN_POINT('Origin',(0.190440410096412,2.94644894857135,-0.0120289264421042));
#97194=CARTESIAN_POINT('Ctrl Pts',(-7.48943805504001,2.877925369,-0.44318699073));
#97195=CARTESIAN_POINT('Ctrl Pts',(-7.51352169964,2.943232886,-0.0361963315300001));
#97196=CARTESIAN_POINT('Ctrl Pts',(-7.49336043001001,3.008559221,0.37100747594));
#97197=CARTESIAN_POINT('Ctrl Pts',(-7.487043143,2.877925369,-0.440664251));
#97198=CARTESIAN_POINT('Ctrl Pts',(-7.510989697,2.943232886,-0.033803736));
#97199=CARTESIAN_POINT('Ctrl Pts',(-7.49070624700001,3.008559221,0.373255838));
#97200=CARTESIAN_POINT('Ctrl Pts',(-7.24755193900001,2.877925369,-0.188390278));
#97201=CARTESIAN_POINT('Ctrl Pts',(-7.257789433,2.943232886,0.205455817));
#97202=CARTESIAN_POINT('Ctrl Pts',(-7.225287946,3.008559221,0.598092044));
#97203=CARTESIAN_POINT('',(-7.4907062523096,3.00855922118742,0.373255832402714));
#97204=CARTESIAN_POINT('',(-7.35799709670449,3.00855922150568,0.485673937902005));
#97205=CARTESIAN_POINT('',(-7.49755470732808,2.91791835920472,-0.191503494391312));
#97206=CARTESIAN_POINT('Origin',(0.192911317041647,2.9464287636347,0.00035828858451639));
#97207=CARTESIAN_POINT('Ctrl Pts',(-7.24767235082839,2.87870320304189,-0.18369948845923));
#97208=CARTESIAN_POINT('Ctrl Pts',(-7.28925997327148,2.88555248749686,-0.185043996982772));
#97209=CARTESIAN_POINT('Ctrl Pts',(-7.33089917141281,2.89224022490725,-0.186365657539663));
#97210=CARTESIAN_POINT('Ctrl Pts',(-7.4141802834907,2.90530189604263,-0.188965060643359));
#97211=CARTESIAN_POINT('Ctrl Pts',(-7.45586769143985,2.91168295765171,-0.190244219085969));
#97212=CARTESIAN_POINT('Ctrl Pts',(-7.49755469545811,2.9179183592416,-0.191503495366743));
#97213=CARTESIAN_POINT('Ctrl Pts',(-7.45928447425713,3.0130934343785,-0.785970285244055));
#97214=CARTESIAN_POINT('Ctrl Pts',(-7.46071492280142,3.01082632768925,-0.771884465656615));
#97215=CARTESIAN_POINT('Ctrl Pts',(-7.46214537134582,3.008559221,-0.757798646069158));
#97216=CARTESIAN_POINT('Ctrl Pts',(-7.5036313465345,2.942808424,-0.349280657629427));
#97217=CARTESIAN_POINT('Ctrl Pts',(-7.50027410223868,2.877933005,0.0613247039030384));
#97218=CARTESIAN_POINT('Ctrl Pts',(-7.18127816733622,3.0130934343785,-0.996239447247901));
#97219=CARTESIAN_POINT('Ctrl Pts',(-7.18310750316813,3.01082632768925,-0.982676896623952));
#97220=CARTESIAN_POINT('Ctrl Pts',(-7.184936839,3.008559221,-0.969114346));
#97221=CARTESIAN_POINT('Ctrl Pts',(-7.237991373,2.942808424,-0.575772243));
#97222=CARTESIAN_POINT('Ctrl Pts',(-7.247790206,2.877933005,-0.178989209));
#97223=CARTESIAN_POINT('',(-7.46157359058,3.00855922016356,-0.75823452133945));
#97224=CARTESIAN_POINT('Origin',(0.187233646271958,3.08925209820063,0.0320413507772142));
#97225=CARTESIAN_POINT('',(-7.32325521222774,3.00855921853322,-0.863674445527309));
#97226=CARTESIAN_POINT('Origin',(1.72604985859692E-12,3.10034167700011,
6.96328845278815E-14));
#97227=CARTESIAN_POINT('',(-7.49754130651673,3.09925366544336,-0.192026963734092));
#97228=CARTESIAN_POINT('Origin',(0.192850144087738,3.08928539902374,0.00334440390494479));
#97229=CARTESIAN_POINT('Origin',(0.188574042439491,2.94644890795088,0.0291913744015247));
#97230=CARTESIAN_POINT('Ctrl Pts',(-7.21906705286,2.877925369,-2.04283331976));
#97231=CARTESIAN_POINT('Ctrl Pts',(-7.3300785955,2.943232886,-1.6505351487));
#97232=CARTESIAN_POINT('Ctrl Pts',(-7.39792546831,3.008559221,-1.24851746249));
#97233=CARTESIAN_POINT('Ctrl Pts',(-7.21727044700001,2.877925369,-2.039854725));
#97234=CARTESIAN_POINT('Ctrl Pts',(-7.328120127,2.943232886,-1.647654185));
#97235=CARTESIAN_POINT('Ctrl Pts',(-7.39581667,3.008559221,-1.245751095));
#97236=CARTESIAN_POINT('Ctrl Pts',(-7.037609861,2.877925369,-1.741995249));
#97237=CARTESIAN_POINT('Ctrl Pts',(-7.132273277,2.943232886,-1.359557815));
#97238=CARTESIAN_POINT('Ctrl Pts',(-7.184936839,3.008559221,-0.969114346));
#97239=CARTESIAN_POINT('',(-7.39581667399582,3.00855922118755,-1.24575110158274));
#97240=CARTESIAN_POINT('',(-7.29037675403373,3.00855922150568,-1.10743272356952));
#97241=CARTESIAN_POINT('',(-7.28109845410024,2.91791835917478,-1.79877888497127));
#97242=CARTESIAN_POINT('Origin',(0.188324448607423,2.94642871267471,0.041820229100854));
#97243=CARTESIAN_POINT('Ctrl Pts',(-7.03873583842746,2.87870320301111,-1.73744001218541));
#97244=CARTESIAN_POINT('Ctrl Pts',(-7.07906213591146,2.88555248744445,-1.74769319633835));
#97245=CARTESIAN_POINT('Ctrl Pts',(-7.11944371485452,2.8922402248462,-1.75793515394807));
#97246=CARTESIAN_POINT('Ctrl Pts',(-7.20021896298775,2.90530189548184,-1.7783767609778));
#97247=CARTESIAN_POINT('Ctrl Pts',(-7.24065675767129,2.91168295656746,-1.78858757293469));
#97248=CARTESIAN_POINT('Ctrl Pts',(-7.2810984424229,2.91791835922825,-1.79877888336987));
#97249=CARTESIAN_POINT('Ctrl Pts',(-7.11593016989708,3.01309343428781,-2.37112040385951));
#97250=CARTESIAN_POINT('Ctrl Pts',(-7.12035521010569,3.01082632764391,-2.35767140730608));
#97251=CARTESIAN_POINT('Ctrl Pts',(-7.12478025031426,3.008559221,-2.34422241075272));
#97252=CARTESIAN_POINT('Ctrl Pts',(-7.25311559847784,2.942808424,-1.95417360356047));
#97253=CARTESIAN_POINT('Ctrl Pts',(-7.33810486053925,2.877933005,-1.55244625908855));
#97254=CARTESIAN_POINT('Ctrl Pts',(-6.79922184224499,3.01309343428781,-2.5167104506348));
#97255=CARTESIAN_POINT('Ctrl Pts',(-6.80392395662256,3.01082632764391,-2.50385823831738));
#97256=CARTESIAN_POINT('Ctrl Pts',(-6.808626071,3.008559221,-2.491006026));
#97257=CARTESIAN_POINT('Ctrl Pts',(-6.944997145,2.942808424,-2.1182652));
#97258=CARTESIAN_POINT('Ctrl Pts',(-7.039863509,2.877933005,-1.732865192));
#97259=CARTESIAN_POINT('',(-7.12412813718847,3.00855922016357,-2.34452517951831));
#97260=CARTESIAN_POINT('Origin',(0.175968387386487,3.08925208219559,0.0715419718021096));
#97261=CARTESIAN_POINT('',(-6.96637709903875,3.00855921853322,-2.417765613795));
#97262=CARTESIAN_POINT('Origin',(2.5804011705155E-13,3.10034167700044,4.06575814682064E-14));
#97263=CARTESIAN_POINT('',(-7.28097283641159,3.09925366542632,-1.79928723503156));
#97264=CARTESIAN_POINT('Origin',(0.187622637445009,3.08928541987947,0.0447233372682446));
#97265=CARTESIAN_POINT('Origin',(0.1778901658128,2.94644891472726,0.0690467906906783));
#97266=CARTESIAN_POINT('Ctrl Pts',(-6.61114049838,2.877925369,-3.54695903503));
#97267=CARTESIAN_POINT('Ctrl Pts',(-6.80388916456,2.943232886,-3.18769677721));
#97268=CARTESIAN_POINT('Ctrl Pts',(-6.95657173252999,3.008559221,-2.80966311266));
#97269=CARTESIAN_POINT('Ctrl Pts',(-6.610026206,2.877925369,-3.543663861));
#97270=CARTESIAN_POINT('Ctrl Pts',(-6.80259580600001,2.943232886,-3.184462156));
#97271=CARTESIAN_POINT('Ctrl Pts',(-6.955106924,3.008559221,-2.806508092));
#97272=CARTESIAN_POINT('Ctrl Pts',(-6.498596968,2.877925369,-3.214146458));
#97273=CARTESIAN_POINT('Ctrl Pts',(-6.67325995,2.943232886,-2.861000035));
#97274=CARTESIAN_POINT('Ctrl Pts',(-6.80862607100001,3.008559221,-2.491006026));
#97275=CARTESIAN_POINT('',(-6.95510692647804,3.00855922118749,-2.8065080993318));
#97276=CARTESIAN_POINT('',(-6.88186649638477,3.00855922150568,-2.64875706189753));
#97277=CARTESIAN_POINT('',(-6.72418612977475,2.91791835923578,-3.32194537401143));
#97278=CARTESIAN_POINT('Origin',(0.174931003159876,2.94642873441672,0.081326479956936));
#97279=CARTESIAN_POINT('Ctrl Pts',(-6.50067586169062,2.87870320298644,-3.2099397714576));
#97280=CARTESIAN_POINT('Ctrl Pts',(-6.5378552213195,2.88555248745678,-3.22862220385387));
#97281=CARTESIAN_POINT('Ctrl Pts',(-6.57509098335056,2.89224022488905,-3.24730555608538));
#97282=CARTESIAN_POINT('Ctrl Pts',(-6.64958341887247,2.90530189713171,-3.28463354502223));
#97283=CARTESIAN_POINT('Ctrl Pts',(-6.68688078783159,2.91168295985056,-3.30329856955462));
#97284=CARTESIAN_POINT('Ctrl Pts',(-6.72418611854397,2.91791835926929,-3.3219453699723));
#97285=CARTESIAN_POINT('Ctrl Pts',(-6.43984287988421,3.01309343442669,-3.84539956829271));
#97286=CARTESIAN_POINT('Ctrl Pts',(-6.44705560205367,3.01082632771334,-3.8332162542701));
#97287=CARTESIAN_POINT('Ctrl Pts',(-6.45426832422315,3.008559221,-3.82103294024745));
#97288=CARTESIAN_POINT('Ctrl Pts',(-6.66345222738474,2.942808424,-3.46769156360501));
#97289=CARTESIAN_POINT('Ctrl Pts',(-6.8328139904108,2.877933005,-3.0936265599123));
#97290=CARTESIAN_POINT('Ctrl Pts',(-6.09924145999368,3.01309343442668,-3.91950287199552));
#97291=CARTESIAN_POINT('Ctrl Pts',(-6.1065964874969,3.01082632771334,-3.90796195249775));
#97292=CARTESIAN_POINT('Ctrl Pts',(-6.113951515,3.008559221,-3.896421033));
#97293=CARTESIAN_POINT('Ctrl Pts',(-6.327262568,2.942808424,-3.56171043));
#97294=CARTESIAN_POINT('Ctrl Pts',(-6.502760619,2.877933005,-3.205714324));
#97295=CARTESIAN_POINT('',(-6.45356637077136,3.00855922016357,-3.82118844541768));
#97296=CARTESIAN_POINT('Origin',(0.156474692526415,3.08925205823525,0.107697219502322));
#97297=CARTESIAN_POINT('',(-6.28375893558174,3.00855921853322,-3.85880474889426));
#97298=CARTESIAN_POINT('Origin',(1.22471477403963E-12,3.10034167700033,
6.61580165650655E-13));
#97299=CARTESIAN_POINT('',(-6.72395416877963,3.09925366545874,-3.32241483495412));
#97300=CARTESIAN_POINT('Origin',(0.1736215916407,3.08928536449683,0.0840108764691233));
#97301=CARTESIAN_POINT('Origin',(0.158887925882241,2.94644891559956,0.105673502394065));
#97302=CARTESIAN_POINT('Ctrl Pts',(-5.69408436183001,2.877925369,-4.88523288661));
#97303=CARTESIAN_POINT('Ctrl Pts',(-5.95955743762001,2.943232886,-4.57580524642));
#97304=CARTESIAN_POINT('Ctrl Pts',(-6.18993643594999,3.008559221,-4.23943203857));
#97305=CARTESIAN_POINT('Ctrl Pts',(-5.693704486,2.877925369,-4.88177521199999));
#97306=CARTESIAN_POINT('Ctrl Pts',(-5.958989665,2.943232886,-4.572368215));
#97307=CARTESIAN_POINT('Ctrl Pts',(-6.18918411,3.008559221,-4.23603589));
#97308=CARTESIAN_POINT('Ctrl Pts',(-5.65571690300001,2.877925369,-4.536007751));
#97309=CARTESIAN_POINT('Ctrl Pts',(-5.902212403,2.943232886,-4.228665073));
#97310=CARTESIAN_POINT('Ctrl Pts',(-6.113951515,3.008559221,-3.896421033));
#97311=CARTESIAN_POINT('',(-6.18918411085223,3.00855922118745,-4.23603589763653));
#97312=CARTESIAN_POINT('',(-6.15156781078797,3.00855922150568,-4.06622846409005));
#97313=CARTESIAN_POINT('',(-5.85285833527549,2.91791835920682,-4.68978138984361));
#97314=CARTESIAN_POINT('Origin',(0.153358491952596,2.94642875212302,0.117030173352469));
#97315=CARTESIAN_POINT('Ctrl Pts',(-5.65865150674991,2.87870320301381,-4.53234631577129));
#97316=CARTESIAN_POINT('Ctrl Pts',(-5.69094546277738,2.88555248747294,-4.55858442652626));
#97317=CARTESIAN_POINT('Ctrl Pts',(-5.72329430486643,2.89224022489121,-4.58483556042797));
#97318=CARTESIAN_POINT('Ctrl Pts',(-5.78802073411798,2.90530189705154,-4.63730451296399));
#97319=CARTESIAN_POINT('Ctrl Pts',(-5.82043368251407,2.91168295970418,-4.66355099107896));
#97320=CARTESIAN_POINT('Ctrl Pts',(-5.85285832531392,2.91791835926746,-4.6897813835981));
#97321=CARTESIAN_POINT('Ctrl Pts',(-5.46263569397422,3.01309343427872,-5.1398721217525));
#97322=CARTESIAN_POINT('Ctrl Pts',(-5.47229883877705,3.01082632763937,-5.1295241692268));
#97323=CARTESIAN_POINT('Ctrl Pts',(-5.48196198357988,3.008559221,-5.11917621670124));
#97324=CARTESIAN_POINT('Ctrl Pts',(-5.76221323479108,2.942808424,-4.81906412049076));
#97325=CARTESIAN_POINT('Ctrl Pts',(-6.00802833361441,2.877933005,-4.49015232226918));
#97326=CARTESIAN_POINT('Ctrl Pts',(-5.11406732750078,3.01309343427873,-5.13902369378443));
#97327=CARTESIAN_POINT('Ctrl Pts',(-5.12373135475034,3.01082632763937,-5.12933370839221));
#97328=CARTESIAN_POINT('Ctrl Pts',(-5.133395382,3.008559221,-5.119643723));
#97329=CARTESIAN_POINT('Ctrl Pts',(-5.413672226,2.942808424,-4.838614039));
#97330=CARTESIAN_POINT('Ctrl Pts',(-5.66159587,2.877933005,-4.528667818));
#97331=CARTESIAN_POINT('',(-5.48124301243205,3.00855922016357,-5.11917718699627));
#97332=CARTESIAN_POINT('Origin',(0.12966488231818,3.08925206018815,0.138816935313775));
#97333=CARTESIAN_POINT('',(-5.30731918799498,3.00855921853322,-5.11941046289062));
#97334=CARTESIAN_POINT('Origin',(1.8995222061946E-13,3.10034167700033,5.3776427755281E-14));
#97335=CARTESIAN_POINT('',(-5.8525308771641,3.09925366548655,-4.69019001010936));
#97336=CARTESIAN_POINT('Origin',(0.151502844515639,3.08928542269922,0.119370499732209));
#97337=CARTESIAN_POINT('Origin',(0.132456427435822,2.94644893686484,0.137359030828437));
#97338=CARTESIAN_POINT('Ctrl Pts',(-4.51077916970999,2.877925369,-5.99507867818));
#97339=CARTESIAN_POINT('Ctrl Pts',(-4.83656342825001,2.943232886,-5.74995414786));
#97340=CARTESIAN_POINT('Ctrl Pts',(-5.13386659043,3.008559221,-5.47096983334));
#97341=CARTESIAN_POINT('Ctrl Pts',(-4.511151473,2.877925369,-5.99162018));
#97342=CARTESIAN_POINT('Ctrl Pts',(-4.83674779000001,2.943232886,-5.746475418));
#97343=CARTESIAN_POINT('Ctrl Pts',(-5.133861925,3.008559221,-5.46749135700001));
#97344=CARTESIAN_POINT('Ctrl Pts',(-4.548381802,2.877925369,-5.645770362));
#97345=CARTESIAN_POINT('Ctrl Pts',(-4.85518396500001,2.943232886,-5.398602432));
#97346=CARTESIAN_POINT('Ctrl Pts',(-5.13339538200001,3.008559221,-5.119643723));
#97347=CARTESIAN_POINT('',(-5.1338619255737,3.00855922118768,-5.46749136247341));
#97348=CARTESIAN_POINT('',(-5.13362865127121,3.00855922150568,-5.29356754216145));
#97349=CARTESIAN_POINT('',(-4.70785739014204,2.91791835921984,-5.83832843962122));
#97350=CARTESIAN_POINT('Origin',(0.124615097880204,2.94642874656054,0.147261696058592));
#97351=CARTESIAN_POINT('Ctrl Pts',(-4.55203489682575,2.87870320305795,-5.6428253826466));
#97352=CARTESIAN_POINT('Ctrl Pts',(-4.57793341989185,2.88555248751722,-5.67539230694019));
#97353=CARTESIAN_POINT('Ctrl Pts',(-4.60388274619806,2.89224022493592,-5.70798374879017));
#97354=CARTESIAN_POINT('Ctrl Pts',(-4.65581663663197,2.90530189785697,-5.77314027923381));
#97355=CARTESIAN_POINT('Ctrl Pts',(-4.6818295747134,2.91168296129037,-5.80574095935479));
#97356=CARTESIAN_POINT('Ctrl Pts',(-4.70785738175949,2.91791835928726,-5.83832843143792));
#97357=CARTESIAN_POINT('Ctrl Pts',(-4.23000173511302,3.01309343431576,-6.19400996767578));
#97358=CARTESIAN_POINT('Ctrl Pts',(-4.24166346495119,3.01082632765788,-6.18598123495631));
#97359=CARTESIAN_POINT('Ctrl Pts',(-4.25332519478933,3.008559221,-6.17795250223672));
#97360=CARTESIAN_POINT('Ctrl Pts',(-4.59153955651358,2.942808424,-5.94510259489902));
#97361=CARTESIAN_POINT('Ctrl Pts',(-4.90231394849256,2.877933005,-5.67672355131862));
#97362=CARTESIAN_POINT('Ctrl Pts',(-3.88976508856774,3.01309343431575,-6.11824948059964));
#97363=CARTESIAN_POINT('Ctrl Pts',(-3.90128623678383,3.01082632765788,-6.11086352179979));
#97364=CARTESIAN_POINT('Ctrl Pts',(-3.912807385,3.008559221,-6.103477563));
#97365=CARTESIAN_POINT('Ctrl Pts',(-4.246944588,2.942808424,-5.889269433));
#97366=CARTESIAN_POINT('Ctrl Pts',(-4.555701191,2.877933005,-5.639865837));
#97367=CARTESIAN_POINT('',(-4.25262282382441,3.00855922016355,-6.17779889244642));
#97368=CARTESIAN_POINT('Origin',(0.0967918109286592,3.08925206385687,0.163445524649569));
#97369=CARTESIAN_POINT('',(-4.08271509389942,3.00855921853322,-6.14063823337773));
#97370=CARTESIAN_POINT('Origin',(-1.58727198051878E-13,3.10034167699978,
-3.5605199344424E-13));
#97371=CARTESIAN_POINT('',(-4.70744974629859,3.0992536654783,-5.83865711346283));
#97372=CARTESIAN_POINT('Origin',(0.122299545909472,3.08928544800128,0.149148174631047));
#97373=CARTESIAN_POINT('Origin',(0.0998316880435851,2.94644890557194,0.162622073715286));
#97374=CARTESIAN_POINT('Ctrl Pts',(-3.11655495708,2.877925369,-6.82460125420999));
#97375=CARTESIAN_POINT('Ctrl Pts',(-3.48741708843,2.943232886,-6.65524158477));
#97376=CARTESIAN_POINT('Ctrl Pts',(-3.83774284877,3.008559221,-6.44669115942001));
#97377=CARTESIAN_POINT('Ctrl Pts',(-3.117662031,2.877925369,-6.821303648));
#97378=CARTESIAN_POINT('Ctrl Pts',(-3.488344964,2.943232886,-6.65188381800001));
#97379=CARTESIAN_POINT('Ctrl Pts',(-3.838486062,3.008559221,-6.44329300500001));
#97380=CARTESIAN_POINT('Ctrl Pts',(-3.228369423,2.877925369,-6.491543027));
#97381=CARTESIAN_POINT('Ctrl Pts',(-3.581132521,2.943232886,-6.316107141));
#97382=CARTESIAN_POINT('Ctrl Pts',(-3.912807385,3.008559221,-6.103477563));
#97383=CARTESIAN_POINT('',(-3.83848606137266,3.0085592211877,-6.4432930104941));
#97384=CARTESIAN_POINT('',(-3.87564672085867,3.00855922150568,-6.27338528563179));
#97385=CARTESIAN_POINT('',(-3.34272226580324,2.91791835921079,-6.71388174049539));
#97386=CARTESIAN_POINT('Origin',(0.0900447143230324,2.94642872540765,0.170607277916067));
#97387=CARTESIAN_POINT('Ctrl Pts',(-3.23257019413014,2.87870320301883,-6.48945220613886));
#97388=CARTESIAN_POINT('Ctrl Pts',(-3.2508622980708,2.88555248747773,-6.52682515079375));
#97389=CARTESIAN_POINT('Ctrl Pts',(-3.26919874694083,2.89224022490049,-6.56423296099061));
#97390=CARTESIAN_POINT('Ctrl Pts',(-3.30591171996773,2.90530189646074,-6.63903041146088));
#97391=CARTESIAN_POINT('Ctrl Pts',(-3.32430830306973,2.911682958487,-6.67646090970598));
#97392=CARTESIAN_POINT('Ctrl Pts',(-3.34272225937116,2.91791835925212,-6.71388173051157));
#97393=CARTESIAN_POINT('Ctrl Pts',(-2.79957759524227,3.01309343436868,-6.95852279143793));
#97394=CARTESIAN_POINT('Ctrl Pts',(-2.81269262067868,3.01082632768435,-6.95318869316753));
#97395=CARTESIAN_POINT('Ctrl Pts',(-2.82580764611506,3.008559221,-6.9478545948972));
#97396=CARTESIAN_POINT('Ctrl Pts',(-3.20617059112771,2.942808424,-6.79315467937377));
#97397=CARTESIAN_POINT('Ctrl Pts',(-3.56737281165495,2.877933005,-6.59785749655774));
#97398=CARTESIAN_POINT('Ctrl Pts',(-2.48358175878518,3.01309343436869,-6.81139272192371));
#97399=CARTESIAN_POINT('Ctrl Pts',(-2.49642131189258,3.01082632768435,-6.80665614896187));
#97400=CARTESIAN_POINT('Ctrl Pts',(-2.509260865,3.008559221,-6.801919576));
#97401=CARTESIAN_POINT('Ctrl Pts',(-2.881634541,2.942808424,-6.664549134));
#97402=CARTESIAN_POINT('Ctrl Pts',(-3.236786987,2.877933005,-6.487349998));
#97403=CARTESIAN_POINT('',(-2.82515471777632,3.00855922016355,-6.94755358741828));
#97404=CARTESIAN_POINT('Origin',(0.0593929041144048,3.08925206325076,0.180431615768841));
#97405=CARTESIAN_POINT('',(-2.66720777989305,3.00855921853322,-6.87473658497311));
#97406=CARTESIAN_POINT('Origin',(-1.32272665043232E-13,3.10034167700067,
-2.12503625807159E-13));
#97407=CARTESIAN_POINT('',(-3.34225349745923,3.09925366545785,-6.71411509886201));
#97408=CARTESIAN_POINT('Origin',(0.0873777332247544,3.08928540246991,0.171951807331283));
#97409=CARTESIAN_POINT('Origin',(0.0625387623973611,2.94644889145861,0.180280994928028));
#97410=CARTESIAN_POINT('Ctrl Pts',(-1.576604098,2.877925369,-7.33501306085001));
#97411=CARTESIAN_POINT('Ctrl Pts',(-1.97520300205,2.943232886,-7.24933732122));
#97412=CARTESIAN_POINT('Ctrl Pts',(-2.36217051692,3.008559221,-7.12097237258));
#97413=CARTESIAN_POINT('Ctrl Pts',(-1.578394177,2.877925369,-7.332030539));
#97414=CARTESIAN_POINT('Ctrl Pts',(-1.976831005,2.943232886,-7.246257523));
#97415=CARTESIAN_POINT('Ctrl Pts',(-2.363626857,3.008559221,-7.117813434));
#97416=CARTESIAN_POINT('Ctrl Pts',(-1.757402077,2.877925369,-7.033778354));
#97417=CARTESIAN_POINT('Ctrl Pts',(-2.1396313,2.943232886,-6.938277701));
#97418=CARTESIAN_POINT('Ctrl Pts',(-2.509260865,3.008559221,-6.801919576));
#97419=CARTESIAN_POINT('',(-2.36362685520607,3.00855922118764,-7.11781343921217));
#97420=CARTESIAN_POINT('',(-2.43644385806964,3.00855922150568,-6.95986650602584));
#97421=CARTESIAN_POINT('',(-1.82128516328855,2.91791835917736,-7.27550139344267));
#97422=CARTESIAN_POINT('Origin',(0.0512640569840399,2.94642876615184,0.185975714800092));
#97423=CARTESIAN_POINT('Ctrl Pts',(-1.76195410109328,2.87870320313799,-7.03263945803826));
#97424=CARTESIAN_POINT('Ctrl Pts',(-1.77178446761464,2.88555248754599,-7.07307090546907));
#97425=CARTESIAN_POINT('Ctrl Pts',(-1.78165064719965,2.89224022492362,-7.11354593614641));
#97426=CARTESIAN_POINT('Ctrl Pts',(-1.80142604852422,2.90530189501338,-7.19448685877411));
#97427=CARTESIAN_POINT('Ctrl Pts',(-1.81134607668391,2.91168295556601,-7.23499696438467));
#97428=CARTESIAN_POINT('Ctrl Pts',(-1.821285159244,2.91791835921545,-7.27550138225621));
#97429=CARTESIAN_POINT('Ctrl Pts',(-1.23824831937288,3.01309343425735,-7.39766282394084));
#97430=CARTESIAN_POINT('Ctrl Pts',(-1.25220339591637,3.01082632762868,-7.39527277675328));
#97431=CARTESIAN_POINT('Ctrl Pts',(-1.26615847245984,3.008559221,-7.39288272956574));
#97432=CARTESIAN_POINT('Ctrl Pts',(-1.67088465221739,2.942808424,-7.32356640122884));
#97433=CARTESIAN_POINT('Ctrl Pts',(-2.06562528681077,2.877933005,-7.21048295867911));
#97434=CARTESIAN_POINT('Ctrl Pts',(-0.961268906319293,3.01309343425735,
-7.18604280915326));
#97435=CARTESIAN_POINT('Ctrl Pts',(-0.974826500659645,3.01082632762868,
-7.18417709907661));
#97436=CARTESIAN_POINT('Ctrl Pts',(-0.988384095,3.008559221,-7.182311389));
#97437=CARTESIAN_POINT('Ctrl Pts',(-1.381582466,2.942808424,-7.128201925));
#97438=CARTESIAN_POINT('Ctrl Pts',(-1.766524221,2.877933005,-7.031492884));
#97439=CARTESIAN_POINT('',(-1.26558551692927,3.00855922016356,-7.39244839919028));
#97440=CARTESIAN_POINT('Origin',(0.0192169037645398,3.08925205889063,0.188981087051618));
#97441=CARTESIAN_POINT('',(-1.12698479404631,3.00855921853322,-7.28737989481257));
#97442=CARTESIAN_POINT('Origin',(-2.46005472936961E-13,3.10034167699967,
-1.12800394025392E-12));
#97443=CARTESIAN_POINT('',(-1.82077718939073,3.09925366550626,-7.27562852432749));
#97444=CARTESIAN_POINT('Origin',(0.0483703533938834,3.08928542389148,0.186715408607567));
#97445=CARTESIAN_POINT('Origin',(0.0223215694314258,2.94644894993203,0.189510086032583));
#97446=CARTESIAN_POINT('Ctrl Pts',(0.03706701598,2.877925369,-7.50244780807));
#97447=CARTESIAN_POINT('Ctrl Pts',(-0.37063061727,2.943232886,-7.50446210275));
#97448=CARTESIAN_POINT('Ctrl Pts',(-0.77614571692,3.008559221,-7.46228483128));
#97449=CARTESIAN_POINT('Ctrl Pts',(0.034677634,2.877925369,-7.49991983));
#97450=CARTESIAN_POINT('Ctrl Pts',(-0.372882624,2.943232886,-7.501804281));
#97451=CARTESIAN_POINT('Ctrl Pts',(-0.778247087,3.008559221,-7.459512817));
#97452=CARTESIAN_POINT('Ctrl Pts',(-0.204260564,2.877925369,-7.247122023));
#97453=CARTESIAN_POINT('Ctrl Pts',(-0.598083297,2.943232886,-7.23602210600001));
#97454=CARTESIAN_POINT('Ctrl Pts',(-0.988384095,3.008559221,-7.182311389));
#97455=CARTESIAN_POINT('',(-0.88331558791762,3.00855922150568,-7.32091210337191));
#97456=CARTESIAN_POINT('Ctrl Pts',(-0.20895099349809,2.87870320312668,-7.24698830408616));
#97457=CARTESIAN_POINT('Ctrl Pts',(-0.20985996526507,2.88555248754736,-7.2885877250765));
#97458=CARTESIAN_POINT('Ctrl Pts',(-0.21079454375944,2.89224022494082,-7.33023740914598));
#97459=CARTESIAN_POINT('Ctrl Pts',(-0.212707701350711,2.9053018958938,-7.41353711031396));
#97460=CARTESIAN_POINT('Ctrl Pts',(-0.213687329218262,2.91168295475788,
-7.45523261427169));
#97461=CARTESIAN_POINT('Ctrl Pts',(-0.214686788680074,2.91791835670407,
-7.49692665869679));
#97462=CARTESIAN_POINT('Ctrl Pts',(0.363928114147479,3.01031422125333,-7.49137659943433));
#97463=CARTESIAN_POINT('Ctrl Pts',(0.358454361386452,3.00943672112667,-7.49163449536675));
#97464=CARTESIAN_POINT('Ctrl Pts',(0.352980608625425,3.008559221,-7.49189239129917));
#97465=CARTESIAN_POINT('Ctrl Pts',(-0.0571658924187911,2.942808424,-7.51121644902179));
#97466=CARTESIAN_POINT('Ctrl Pts',(-0.466970758802433,2.877933005,-7.48565195769581));
#97467=CARTESIAN_POINT('Ctrl Pts',(0.589268653938478,3.01031422125333,-7.2260206670324));
#97468=CARTESIAN_POINT('Ctrl Pts',(0.583988535469239,3.00943672112667,-7.2264434850162));
#97469=CARTESIAN_POINT('Ctrl Pts',(0.578708417,3.008559221,-7.226866303));
#97470=CARTESIAN_POINT('Ctrl Pts',(0.18307087,2.942808424,-7.258547916));
#97471=CARTESIAN_POINT('Ctrl Pts',(-0.213660746,2.877933005,-7.246850977));
#97472=CARTESIAN_POINT('',(0.465934748101219,3.00855921853322,-7.3592734190439));
#97473=CARTESIAN_POINT('Ctrl Pts',(1.64900491812,2.877925369,-7.31907643485));
#97474=CARTESIAN_POINT('Ctrl Pts',(1.25127204218,2.943232886,-7.40868657547001));
#97475=CARTESIAN_POINT('Ctrl Pts',(0.84617079334,3.008559221,-7.45466914569));
#97476=CARTESIAN_POINT('Ctrl Pts',(1.646127958,2.877925369,-7.317121206));
#97477=CARTESIAN_POINT('Ctrl Pts',(1.248501333,2.943232886,-7.406575007));
#97478=CARTESIAN_POINT('Ctrl Pts',(0.843522651,3.008559221,-7.452413672));
#97479=CARTESIAN_POINT('Ctrl Pts',(1.358431946,2.877925369,-7.121598321));
#97480=CARTESIAN_POINT('Ctrl Pts',(0.971430415,2.943232886,-7.19541816));
#97481=CARTESIAN_POINT('Ctrl Pts',(0.578708417,3.008559221,-7.226866303));
#97482=CARTESIAN_POINT('',(0.843522657377817,3.00855922118756,-7.45241367635266));
#97483=CARTESIAN_POINT('',(0.711115537090266,3.00855922150568,-7.33963998720059));
#97484=CARTESIAN_POINT('',(1.4019500970824,2.91791835924909,-7.3678040214789));
#97485=CARTESIAN_POINT('Origin',(-0.0315631804265319,2.94642870889188,0.190312136075106));
#97486=CARTESIAN_POINT('Ctrl Pts',(1.35382243093574,2.87870320305526,-7.12247603196901));
#97487=CARTESIAN_POINT('Ctrl Pts',(1.36187735611562,2.88555248751697,-7.16329828373009));
#97488=CARTESIAN_POINT('Ctrl Pts',(1.36991807837126,2.89224022494186,-7.20417512809119));
#97489=CARTESIAN_POINT('Ctrl Pts',(1.38595662582573,2.9053018985513,-7.28593861717606));
#97490=CARTESIAN_POINT('Ctrl Pts',(1.39396320871808,2.91168296268184,-7.32686992942572));
#97491=CARTESIAN_POINT('Ctrl Pts',(1.40195009630196,2.91791835930475,-7.36780400971366));
#97492=CARTESIAN_POINT('Ctrl Pts',(1.98239425956791,3.01309343443221,-7.23386391540278));
#97493=CARTESIAN_POINT('Ctrl Pts',(1.96872541981646,3.01082632771611,-7.23755435206928));
#97494=CARTESIAN_POINT('Ctrl Pts',(1.95505658006501,3.008559221,-7.24124478873574));
#97495=CARTESIAN_POINT('Ctrl Pts',(1.55863187657184,2.942808424,-7.34827510644113));
#97496=CARTESIAN_POINT('Ctrl Pts',(1.15289247445925,2.877933005,-7.41139064311515));
#97497=CARTESIAN_POINT('Ctrl Pts',(2.14491702942533,3.01309343443221,-6.92550215463664));
#97498=CARTESIAN_POINT('Ctrl Pts',(2.13182909821269,3.01082632771611,-6.92950156831831));
#97499=CARTESIAN_POINT('Ctrl Pts',(2.118741167,3.008559221,-6.933500982));
#97500=CARTESIAN_POINT('Ctrl Pts',(1.739164016,2.942808424,-7.049492274));
#97501=CARTESIAN_POINT('Ctrl Pts',(1.349193269,2.877933005,-7.123354373));
#97502=CARTESIAN_POINT('',(1.95539420948476,3.00855922016357,-7.24061002354905));
#97503=CARTESIAN_POINT('Origin',(-0.0619102307666214,3.08925202244823,0.179583189245777));
#97504=CARTESIAN_POINT('',(2.03706769954263,3.00855921853322,-7.08705549831994));
#97505=CARTESIAN_POINT('Origin',(-1.95102180938767E-13,3.10034167699989,
6.10188982674842E-13));
#97506=CARTESIAN_POINT('',(1.40246450243754,3.09925366544267,-7.36770610985706));
#97507=CARTESIAN_POINT('Origin',(-0.0345000262589518,3.0892854313886,0.189768554694597));
#97508=CARTESIAN_POINT('Origin',(-0.0593146635395822,2.94644893318334,0.181367007252413));
#97509=CARTESIAN_POINT('Ctrl Pts',(3.1838371828,2.877925369,-6.79347318230001));
#97510=CARTESIAN_POINT('Ctrl Pts',(2.81466661134,2.943232886,-6.96648909860001));
#97511=CARTESIAN_POINT('Ctrl Pts',(2.42892129841,3.008559221,-7.09848141564));
#97512=CARTESIAN_POINT('Ctrl Pts',(3.180607168,2.877925369,-6.792182127));
#97513=CARTESIAN_POINT('Ctrl Pts',(2.811506755,2.943232886,-6.96502251800001));
#97514=CARTESIAN_POINT('Ctrl Pts',(2.425850208,3.008559221,-7.096847946));
#97515=CARTESIAN_POINT('Ctrl Pts',(2.857605688,2.877925369,-6.663076597));
#97516=CARTESIAN_POINT('Ctrl Pts',(2.495521121,2.943232886,-6.818364458));
#97517=CARTESIAN_POINT('Ctrl Pts',(2.118741167,3.008559221,-6.933500982));
#97518=CARTESIAN_POINT('',(2.42585021516617,3.00855922118751,-7.09684794887307));
#97519=CARTESIAN_POINT('',(2.27229569045365,3.00855922150568,-7.01517446304328));
#97520=CARTESIAN_POINT('',(2.9530333567116,2.9179183592309,-6.89417102827685));
#97521=CARTESIAN_POINT('Origin',(-0.071736775555461,2.94642872856476,0.179077716464233));
#97522=CARTESIAN_POINT('Ctrl Pts',(2.85329262188022,2.87870320297217,-6.66492469631897));
#97523=CARTESIAN_POINT('Ctrl Pts',(2.86993480505275,2.88555248745112,-6.70306097574357));
#97524=CARTESIAN_POINT('Ctrl Pts',(2.88657485310286,2.89224022489599,-6.7412536246611));
#97525=CARTESIAN_POINT('Ctrl Pts',(2.9198151589043,2.90530189741744,-6.81765770875573));
#97526=CARTESIAN_POINT('Ctrl Pts',(2.93643357145378,2.91168296040963,-6.85591088368492));
#97527=CARTESIAN_POINT('Ctrl Pts',(2.95303335331849,2.91791835927626,-6.89417101691848));
#97528=CARTESIAN_POINT('Ctrl Pts',(3.49111389256556,3.01309343426058,-6.63858403115588));
#97529=CARTESIAN_POINT('Ctrl Pts',(3.47855795797211,3.01082632763029,-6.64512658367306));
#97530=CARTESIAN_POINT('Ctrl Pts',(3.46600202337865,3.008559221,-6.65166913619008));
#97531=CARTESIAN_POINT('Ctrl Pts',(3.10185386397271,2.942808424,-6.84141673635196));
#97532=CARTESIAN_POINT('Ctrl Pts',(2.71916839817603,2.877933005,-6.99027864620438));
#97533=CARTESIAN_POINT('Ctrl Pts',(3.58354830696306,3.01309343426058,-6.30249400563588));
#97534=CARTESIAN_POINT('Ctrl Pts',(3.57162612048153,3.0108263276303,-6.30921343331795));
#97535=CARTESIAN_POINT('Ctrl Pts',(3.559703934,3.008559221,-6.315932861));
#97536=CARTESIAN_POINT('Ctrl Pts',(3.213935785,2.942808424,-6.510810208));
#97537=CARTESIAN_POINT('Ctrl Pts',(2.848960505,2.877933005,-6.666777635));
#97538=CARTESIAN_POINT('',(3.46619530345603,3.00855922016358,-6.65097663113775));
#97539=CARTESIAN_POINT('Origin',(-0.0990680448027226,3.08925207644981,0.162076097716589));
#97540=CARTESIAN_POINT('',(3.51294962880404,3.00855921853322,-6.48345473929143));
#97541=CARTESIAN_POINT('Origin',(3.45643652588379E-13,3.10034167699945,
-8.7213222754734E-13));
#97542=CARTESIAN_POINT('',(2.95351468760115,3.09925366544939,-6.8939648237853));
#97543=CARTESIAN_POINT('Origin',(-0.0744880397876002,3.0892853942158,0.177915339575154));
#97544=CARTESIAN_POINT('Origin',(-0.0969165599810617,2.94644894008946,0.164376056078851));
#97545=CARTESIAN_POINT('Ctrl Pts',(4.56979675856999,2.877925369,-5.95021467344));
#97546=CARTESIAN_POINT('Ctrl Pts',(4.24645049813,2.943232886,-6.19854633505999));
#97547=CARTESIAN_POINT('Ctrl Pts',(3.89809814271,3.008559221,-6.41037658437));
#97548=CARTESIAN_POINT('Ctrl Pts',(4.566364721,2.877925369,-5.94964816));
#97549=CARTESIAN_POINT('Ctrl Pts',(4.243049246,2.943232886,-6.197793318));
#97550=CARTESIAN_POINT('Ctrl Pts',(3.894747705,3.008559221,-6.409441498));
#97551=CARTESIAN_POINT('Ctrl Pts',(4.223160964,2.877925369,-5.892996816));
#97552=CARTESIAN_POINT('Ctrl Pts',(3.902924033,2.943232886,-6.122491612));
#97553=CARTESIAN_POINT('Ctrl Pts',(3.559703934,3.008559221,-6.31593286100001));
#97554=CARTESIAN_POINT('',(3.89474771260811,3.00855922118748,-6.4094414992632));
#97555=CARTESIAN_POINT('',(3.72722582217893,3.00855922150568,-6.3626871779307));
#97556=CARTESIAN_POINT('',(4.36603605880988,2.91791835919084,-6.09817426023959));
#97557=CARTESIAN_POINT('Origin',(-0.108555880427207,2.94642873921719,0.159469471285798));
#97558=CARTESIAN_POINT('Ctrl Pts',(4.21934602252135,2.8787032030072,-5.89572888979621));
#97559=CARTESIAN_POINT('Ctrl Pts',(4.24379729330923,2.88555248746722,-5.92939598666343));
#97560=CARTESIAN_POINT('Ctrl Pts',(4.26825859668524,2.89224022488836,-5.9631185941482));
#97561=CARTESIAN_POINT('Ctrl Pts',(4.31714637918945,2.90530189662508,-6.03059070613479));
#97562=CARTESIAN_POINT('Ctrl Pts',(4.34159956115091,2.91168295883936,-6.06437707132088));
#97563=CARTESIAN_POINT('Ctrl Pts',(4.36603605311106,2.91791835925659,-6.09817425000079));
#97564=CARTESIAN_POINT('Ctrl Pts',(4.8365929217786,3.01309343425874,-5.73289133585869));
#97565=CARTESIAN_POINT('Ctrl Pts',(4.82573699335903,3.01082632762937,-5.74198008190041));
#97566=CARTESIAN_POINT('Ctrl Pts',(4.81488106493935,3.008559221,-5.75106882794202));
#97567=CARTESIAN_POINT('Ctrl Pts',(4.50003661231422,2.942808424,-6.0146613243089));
#97568=CARTESIAN_POINT('Ctrl Pts',(4.15829902992391,2.877933005,-6.2423089886404));
#97569=CARTESIAN_POINT('Ctrl Pts',(4.85461685012897,3.01309343425874,-5.38478824126976));
#97570=CARTESIAN_POINT('Ctrl Pts',(4.84441787606454,3.01082632762937,-5.39391349013488));
#97571=CARTESIAN_POINT('Ctrl Pts',(4.834218902,3.008559221,-5.403038739));
#97572=CARTESIAN_POINT('Ctrl Pts',(4.538427489,2.942808424,-5.66768989300001));
#97573=CARTESIAN_POINT('Ctrl Pts',(4.215513515,2.877933005,-5.898469785));
#97574=CARTESIAN_POINT('',(4.81492095813824,3.00855922016357,-5.75035096374377));
#97575=CARTESIAN_POINT('Origin',(-0.131593479604116,3.08925209839837,0.136990176737752));
#97576=CARTESIAN_POINT('',(4.82456993844337,3.00855921853322,-5.57669484259999));
#97577=CARTESIAN_POINT('Origin',(4.31946145518225E-13,3.10034167700033,
-5.37330596683816E-13));
#97578=CARTESIAN_POINT('',(4.36646180827853,3.09925366547195,-6.09786940478255));
#97579=CARTESIAN_POINT('Origin',(-0.110993050041802,3.08928540862611,0.157742983199022));
#97580=CARTESIAN_POINT('Origin',(-0.129986767072367,2.94644890496931,0.139698935014254));
#97581=CARTESIAN_POINT('Ctrl Pts',(5.74207771809,2.877925369,-4.82873074004));
#97582=CARTESIAN_POINT('Ctrl Pts',(5.47967508015,2.943232886,-5.14076643327));
#97583=CARTESIAN_POINT('Ctrl Pts',(5.18500425127,3.008559221,-5.4225296685));
#97584=CARTESIAN_POINT('Ctrl Pts',(5.738604136,2.877925369,-4.828915258));
#97585=CARTESIAN_POINT('Ctrl Pts',(5.476191471,2.943232886,-5.14076219));
#97586=CARTESIAN_POINT('Ctrl Pts',(5.181531129,3.008559221,-5.42233668900001));
#97587=CARTESIAN_POINT('Ctrl Pts',(5.391245927,2.877925369,-4.847367054));
#97588=CARTESIAN_POINT('Ctrl Pts',(5.127830556,2.943232886,-5.14033786300001));
#97589=CARTESIAN_POINT('Ctrl Pts',(4.83421890200001,3.008559221,-5.403038739));
#97590=CARTESIAN_POINT('',(5.18153113441456,3.00855922118773,-5.42233668988285));
#97591=CARTESIAN_POINT('',(5.00787501777894,3.00855922150568,-5.4126877118915));
#97592=CARTESIAN_POINT('',(5.57488776725939,2.91791835921303,-5.01703364133197));
#97593=CARTESIAN_POINT('Origin',(-0.140299164977526,2.94642873468267,0.132404891235894));
#97594=CARTESIAN_POINT('Ctrl Pts',(5.38810749193988,2.87870320295152,-4.85085535283309));
#97595=CARTESIAN_POINT('Ctrl Pts',(5.41922453632117,2.88555248744538,-4.87847903131057));
#97596=CARTESIAN_POINT('Ctrl Pts',(5.45036331187865,2.89224022489509,-4.9061547658748));
#97597=CARTESIAN_POINT('Ctrl Pts',(5.51261263464246,2.90530189660948,-4.96153998905137));
#97598=CARTESIAN_POINT('Ctrl Pts',(5.54375718430893,2.91168295877134,-4.9892797362151));
#97599=CARTESIAN_POINT('Ctrl Pts',(5.57488775937166,2.91791835925558,-5.01703363246046));
#97600=CARTESIAN_POINT('Ctrl Pts',(5.95591824100316,3.01309343431531,-4.55913501208992));
#97601=CARTESIAN_POINT('Ctrl Pts',(5.94726992978911,3.01082632765766,-4.57034497217893));
#97602=CARTESIAN_POINT('Ctrl Pts',(5.93862161857506,3.008559221,-4.58155493226809));
#97603=CARTESIAN_POINT('Ctrl Pts',(5.68780264933675,2.942808424,-4.90666703394516));
#97604=CARTESIAN_POINT('Ctrl Pts',(5.40299222083258,2.877933005,-5.20245589984858));
#97605=CARTESIAN_POINT('Ctrl Pts',(5.89868890410138,3.01309343431532,-4.21529576255416));
#97606=CARTESIAN_POINT('Ctrl Pts',(5.89069003505073,3.01082632765766,-4.22640014627709));
#97607=CARTESIAN_POINT('Ctrl Pts',(5.882691166,3.008559221,-4.23750453));
#97608=CARTESIAN_POINT('Ctrl Pts',(5.650707367,2.942808424,-4.55955469800001));
#97609=CARTESIAN_POINT('Ctrl Pts',(5.384953798,2.877933005,-4.854356043));
#97610=CARTESIAN_POINT('',(5.93850625965619,3.00855922016355,-4.58084527514519));
#97611=CARTESIAN_POINT('Origin',(-0.157965620748939,3.08925204684029,0.105498622484728));
#97612=CARTESIAN_POINT('',(5.91059871904763,3.00855921853322,-4.40917489237146));
#97613=CARTESIAN_POINT('Origin',(-3.02275565688959E-13,3.100341677,4.0462425077159E-13));
#97614=CARTESIAN_POINT('',(5.57523802806611,3.09925366543908,-5.01664438946001));
#97615=CARTESIAN_POINT('Origin',(-0.142308321067965,3.08928536684624,0.130194957196356));
#97616=CARTESIAN_POINT('Origin',(-0.156978694153445,2.94644889134558,0.10848936492422));
#97617=CARTESIAN_POINT('Ctrl Pts',(6.64586550476001,2.877925369,-3.48146072451));
#97618=CARTESIAN_POINT('Ctrl Pts',(6.45667614448,2.943232886,-3.84261000606));
#97619=CARTESIAN_POINT('Ctrl Pts',(6.22946532249,3.008559221,-4.18113129112));
#97620=CARTESIAN_POINT('Ctrl Pts',(6.642512799,2.877925369,-3.482387646));
#97621=CARTESIAN_POINT('Ctrl Pts',(6.453273068,2.943232886,-3.843354735));
#97622=CARTESIAN_POINT('Ctrl Pts',(6.226031915,3.008559221,-4.181689442));
#97623=CARTESIAN_POINT('Ctrl Pts',(6.307242223,2.877925369,-3.575079795));
#97624=CARTESIAN_POINT('Ctrl Pts',(6.11296542000001,2.943232886,-3.917827629));
#97625=CARTESIAN_POINT('Ctrl Pts',(5.882691166,3.008559221,-4.23750453));
#97626=CARTESIAN_POINT('',(6.22603192246108,3.00855922118754,-4.18168943994305));
#97627=CARTESIAN_POINT('',(6.0543615422724,3.00855922150568,-4.20959698345089));
#97628=CARTESIAN_POINT('',(6.52306391963344,2.91791835919899,-3.70130210519327));
#97629=CARTESIAN_POINT('Origin',(-0.165482309760923,2.94642871606807,0.0991492473473568));
#97630=CARTESIAN_POINT('Ctrl Pts',(6.3049270436911,2.87870320303805,-3.57916121057829));
#97631=CARTESIAN_POINT('Ctrl Pts',(6.34125486302186,2.88555248746677,-3.59944981817011));
#97632=CARTESIAN_POINT('Ctrl Pts',(6.37761509597951,2.89224022486561,-3.61978459314537));
#97633=CARTESIAN_POINT('Ctrl Pts',(6.45031524954148,2.90530189648302,-3.66049317608533));
#97634=CARTESIAN_POINT('Ctrl Pts',(6.48669488220596,2.9116829585802,-3.68088922557261));
#97635=CARTESIAN_POINT('Ctrl Pts',(6.52306391009491,2.91791835925355,-3.7013020982684));
#97636=CARTESIAN_POINT('Ctrl Pts',(6.79675144293879,3.01309343437702,-3.17219860221281));
#97637=CARTESIAN_POINT('Ctrl Pts',(6.79071513441644,3.01082632768851,-3.18500561110874));
#97638=CARTESIAN_POINT('Ctrl Pts',(6.78467882589409,3.008559221,-3.19781262000476));
#97639=CARTESIAN_POINT('Ctrl Pts',(6.60961335663601,2.942808424,-3.56924244567881));
#97640=CARTESIAN_POINT('Ctrl Pts',(6.39504749999349,2.877933005,-3.91934175591123));
#97641=CARTESIAN_POINT('Ctrl Pts',(6.6669448214866,3.01309343437701,-2.8487007390812));
#97642=CARTESIAN_POINT('Ctrl Pts',(6.66152007574329,3.01082632768851,-2.86126502904062));
#97643=CARTESIAN_POINT('Ctrl Pts',(6.65609533,3.008559221,-2.873829319));
#97644=CARTESIAN_POINT('Ctrl Pts',(6.49876645,2.942808424,-3.238219792));
#97645=CARTESIAN_POINT('Ctrl Pts',(6.302599626,2.877933005,-3.583258008));
#97646=CARTESIAN_POINT('',(6.78441360869358,3.00855922016356,-3.1971443530287));
#97647=CARTESIAN_POINT('Origin',(-0.176951505971167,3.08925206221049,0.0690741528171268));
#97648=CARTESIAN_POINT('',(6.72025447322881,3.00855921853322,-3.03548682471005));
#97649=CARTESIAN_POINT('Origin',(-8.14452671971111E-13,3.10034167700089,
4.8095208371457E-13));
#97650=CARTESIAN_POINT('',(6.52332231405112,3.09925366544977,-3.70084665820566));
#97651=CARTESIAN_POINT('Origin',(-0.166969114518551,3.08928541551715,0.0965588810779272));
#97652=CARTESIAN_POINT('Origin',(-0.176630635389806,2.94644889976632,0.0722071675918656));
#97653=CARTESIAN_POINT('Ctrl Pts',(7.23890000664,2.877925369,-1.97140147378));
#97654=CARTESIAN_POINT('Ctrl Pts',(7.13177020874,2.943232886,-2.36477740657));
#97655=CARTESIAN_POINT('Ctrl Pts',(6.98264351939001,3.008559221,-2.74422786226));
#97656=CARTESIAN_POINT('Ctrl Pts',(7.235824946,2.877925369,-1.973027457));
#97657=CARTESIAN_POINT('Ctrl Pts',(7.128606789,2.943232886,-2.366236285));
#97658=CARTESIAN_POINT('Ctrl Pts',(6.979410369,3.008559221,-2.745511045));
#97659=CARTESIAN_POINT('Ctrl Pts',(6.928318882,2.877925369,-2.135625779));
#97660=CARTESIAN_POINT('Ctrl Pts',(6.81226481500001,2.943232886,-2.512124128));
#97661=CARTESIAN_POINT('Ctrl Pts',(6.65609533,3.008559221,-2.873829319));
#97662=CARTESIAN_POINT('',(6.9794103743155,3.0085592211877,-2.74551104348943));
#97663=CARTESIAN_POINT('',(6.81775285068297,3.00855922150568,-2.80967017912947));
#97664=CARTESIAN_POINT('',(7.16622885296103,2.91791835924605,-2.21250179662255));
#97665=CARTESIAN_POINT('Origin',(-0.182927537908617,2.94642874070228,0.0612573726355285));
#97666=CARTESIAN_POINT('Ctrl Pts',(6.92693521466343,2.87870320306878,-2.14010946824917));
#97667=CARTESIAN_POINT('Ctrl Pts',(6.96677516062568,2.88555248753215,-2.15211433211194));
#97668=CARTESIAN_POINT('Ctrl Pts',(7.00665668705788,2.89224022495434,-2.16415731607856));
#97669=CARTESIAN_POINT('Ctrl Pts',(7.08640830760725,2.9053018989249,-2.18828577534183));
#97670=CARTESIAN_POINT('Ctrl Pts',(7.12632196852394,2.91168296343591,-2.20038443586059));
#97671=CARTESIAN_POINT('Ctrl Pts',(7.166228842292,2.91791835931419,-2.21250179176944));
#97672=CARTESIAN_POINT('Ctrl Pts',(7.31977610100223,3.01309343437182,-1.63693371248333));
#97673=CARTESIAN_POINT('Ctrl Pts',(7.31663404636609,3.01082632768591,-1.65073892851269));
#97674=CARTESIAN_POINT('Ctrl Pts',(7.31349199172984,3.008559221,-1.66454414454206));
#97675=CARTESIAN_POINT('Ctrl Pts',(7.22236588909272,2.942808424,-2.06492404828789));
#97676=CARTESIAN_POINT('Ctrl Pts',(7.08807746584068,2.877933005,-2.45296354772446));
#97677=CARTESIAN_POINT('Ctrl Pts',(7.12346180852388,3.01309343437182,-1.34890363637351));
#97678=CARTESIAN_POINT('Ctrl Pts',(7.12086484126195,3.01082632768591,-1.36234034018676));
#97679=CARTESIAN_POINT('Ctrl Pts',(7.118267874,3.008559221,-1.375777044));
#97680=CARTESIAN_POINT('Ctrl Pts',(7.04295043600001,2.942808424,-1.765469329));
#97681=CARTESIAN_POINT('Ctrl Pts',(6.925542901,2.877933005,-2.144610811));
#97682=CARTESIAN_POINT('',(7.31308931751528,3.00855922016356,-1.66394851513886));
#97683=CARTESIAN_POINT('Origin',(-0.187663364952104,3.08925205844719,0.0294198893682893));
#97684=CARTESIAN_POINT('',(7.21567859711876,3.00855921853322,-1.51986276769344));
#97685=CARTESIAN_POINT('Origin',(-1.64972202565394E-12,3.100341677,5.011182441228E-13));
#97686=CARTESIAN_POINT('',(7.16638329838837,3.09925366545765,-2.2120014507076));
#97687=CARTESIAN_POINT('Origin',(-0.183822865913644,3.08928540630914,0.0584079944972435));
#97688=CARTESIAN_POINT('Origin',(-0.188023592722597,2.94644890831842,0.0325486638177702));
#97689=CARTESIAN_POINT('Ctrl Pts',(7.4934515901,2.877925369,-0.36916168223));
#97690=CARTESIAN_POINT('Ctrl Pts',(7.473390625,2.943232886,-0.7763704436));
#97691=CARTESIAN_POINT('Ctrl Pts',(7.40932106577,3.008559221,-1.17900738859));
#97692=CARTESIAN_POINT('Ctrl Pts',(7.490797961,2.877925369,-0.371410698));
#97693=CARTESIAN_POINT('Ctrl Pts',(7.47061478,2.943232886,-0.778475256));
#97694=CARTESIAN_POINT('Ctrl Pts',(7.406439351,3.008559221,-1.180955603));
#97695=CARTESIAN_POINT('Ctrl Pts',(7.225435051,2.877925369,-0.596312275));
#97696=CARTESIAN_POINT('Ctrl Pts',(7.19303028,2.943232886,-0.988956496));
#97697=CARTESIAN_POINT('Ctrl Pts',(7.11826787400001,3.008559221,-1.375777044));
#97698=CARTESIAN_POINT('',(7.40643935690396,3.00855922118749,-1.1809555980013));
#97699=CARTESIAN_POINT('',(7.26235361303831,3.00855922150574,-1.27836632044191));
#97700=CARTESIAN_POINT('',(7.47430889007143,2.91791835920043,-0.620247362827596));
#97701=CARTESIAN_POINT('Origin',(-0.191819194413607,2.94642872304643,0.0205011828756771));
#97702=CARTESIAN_POINT('Ctrl Pts',(7.22504759247685,2.87870320299642,-0.600988586293256));
#97703=CARTESIAN_POINT('Ctrl Pts',(7.26653679368753,2.88555248744925,-0.604148372301362));
#97704=CARTESIAN_POINT('Ctrl Pts',(7.30807479791577,2.89224022487032,-0.607336448616159));
#97705=CARTESIAN_POINT('Ctrl Pts',(7.39114876161084,2.90530189663738,-0.613756555677362));
#97706=CARTESIAN_POINT('Ctrl Pts',(7.43273010190432,2.91168295887499,-0.616992097636169));
#97707=CARTESIAN_POINT('Ctrl Pts',(7.47430887852099,2.91791835925716,-0.620247360538585));
#97708=CARTESIAN_POINT('Ctrl Pts',(7.50053616437872,3.01309343429141,-0.0251276216729472));
#97709=CARTESIAN_POINT('Ctrl Pts',(7.50043528258605,3.0108263276457,-0.0392855280246127));
#97710=CARTESIAN_POINT('Ctrl Pts',(7.50033440079339,3.008559221,-0.0534434343762788));
#97711=CARTESIAN_POINT('Ctrl Pts',(7.49740861947476,2.942808424,-0.464052096406355));
#97712=CARTESIAN_POINT('Ctrl Pts',(7.44967680772641,2.877933005,-0.871887489858721));
#97713=CARTESIAN_POINT('Ctrl Pts',(7.24689363902802,3.01309343429141,0.213966701145049));
#97714=CARTESIAN_POINT('Ctrl Pts',(7.24724588151406,3.0108263276457,0.200285869072528));
#97715=CARTESIAN_POINT('Ctrl Pts',(7.247598124,3.008559221,0.186605037));
#97716=CARTESIAN_POINT('Ctrl Pts',(7.257813887,2.942808424,-0.210167481));
#97717=CARTESIAN_POINT('Ctrl Pts',(7.224655486,2.877933005,-0.605683996000001));
#97718=CARTESIAN_POINT('',(7.49981309817101,3.00855922016355,-0.0529482935119721));
#97719=CARTESIAN_POINT('Origin',(-0.189600522067149,3.08925208754637,-0.0116100011989929));
#97720=CARTESIAN_POINT('',(7.37370560986287,3.00855921853322,0.0668283836308336));
#97721=CARTESIAN_POINT('Origin',(-1.23295471055052E-12,3.10034167699989,
9.98990657991722E-14));
#97722=CARTESIAN_POINT('',(7.47435216511154,3.09925366543305,-0.619725513626576));
#97723=CARTESIAN_POINT('Origin',(-0.19208124950314,3.08928537215579,0.0175259825682194));
#97724=CARTESIAN_POINT('Origin',(-0.190624840073971,2.94644892047951,-0.00863181313441378));
#97725=CARTESIAN_POINT('Ctrl Pts',(7.39761770582,2.877925369,1.25033969985));
#97726=CARTESIAN_POINT('Ctrl Pts',(7.46556360084,2.943232886,0.84833873868));
#97727=CARTESIAN_POINT('Ctrl Pts',(7.48954699437,3.008559221,0.44134215973));
#97728=CARTESIAN_POINT('Ctrl Pts',(7.395509589,2.877925369,1.247572813));
#97729=CARTESIAN_POINT('Ctrl Pts',(7.463305126,2.943232886,0.845686411));
#97730=CARTESIAN_POINT('Ctrl Pts',(7.487151461,3.008559221,0.43882001));
#97731=CARTESIAN_POINT('Ctrl Pts',(7.184697907,2.877925369,0.970884128));
#97732=CARTESIAN_POINT('Ctrl Pts',(7.237457642,2.943232886,0.580453643));
#97733=CARTESIAN_POINT('Ctrl Pts',(7.247598124,3.008559221,0.186605037));
#97734=CARTESIAN_POINT('',(7.48715146569571,3.00855922118754,0.438820016133631));
#97735=CARTESIAN_POINT('',(7.36737479236834,3.00855922150568,0.312712526601943));
#97736=CARTESIAN_POINT('',(7.43289855028286,2.91791835921972,1.00100914803522));
#97737=CARTESIAN_POINT('Origin',(-0.191741974370172,2.94642869754464,-0.0212136133593398));
#97738=CARTESIAN_POINT('Ctrl Pts',(7.18532477592923,2.87870320303117,0.966233854152873));
#97739=CARTESIAN_POINT('Ctrl Pts',(7.22652324323512,2.88555248748559,0.972066894051458));
#97740=CARTESIAN_POINT('Ctrl Pts',(7.26777545414825,2.89224022490859,0.977882796247031));
#97741=CARTESIAN_POINT('Ctrl Pts',(7.35028732932028,2.90530189689843,0.989471234464394));
#97742=CARTESIAN_POINT('Ctrl Pts',(7.39159206841385,2.91168295936306,0.995250096922327));
#97743=CARTESIAN_POINT('Ctrl Pts',(7.4328985384329,2.91791835926312,1.00100914773029));
#97744=CARTESIAN_POINT('Ctrl Pts',(7.33057949306216,3.01309343423581,1.58785340936343));
#97745=CARTESIAN_POINT('Ctrl Pts',(7.33352450114769,3.01082632761791,1.57400482053784));
#97746=CARTESIAN_POINT('Ctrl Pts',(7.33646950923327,3.008559221,1.56015623171219));
#97747=CARTESIAN_POINT('Ctrl Pts',(7.42188085569069,2.942808424,1.15851841485023));
#97748=CARTESIAN_POINT('Ctrl Pts',(7.4629375410039,2.877933005,0.749957057499588));
#97749=CARTESIAN_POINT('Ctrl Pts',(7.03146877652035,3.01309343423581,1.76683219387563));
#97750=CARTESIAN_POINT('Ctrl Pts',(7.03475375826022,3.01082632761791,1.75354693393781));
#97751=CARTESIAN_POINT('Ctrl Pts',(7.03803874,3.008559221,1.740261674));
#97752=CARTESIAN_POINT('Ctrl Pts',(7.133310028,2.942808424,1.354961564));
#97753=CARTESIAN_POINT('Ctrl Pts',(7.185951211,2.877933005,0.961563929));
#97754=CARTESIAN_POINT('',(7.3358539538905,3.00855922016357,1.56052773146292));
#97755=CARTESIAN_POINT('Origin',(-0.182671985471999,3.08925207572926,-0.0520970703534511));
#97756=CARTESIAN_POINT('',(7.18694634311339,3.00855921853322,1.65039471424761));
#97757=CARTESIAN_POINT('Origin',(-1.37476835471162E-12,3.100341677,-2.28576923014256E-13));
#97758=CARTESIAN_POINT('',(7.43282863131925,3.09925366549807,1.0015281002253));
#97759=CARTESIAN_POINT('Origin',(-0.191357879377316,3.08928538259554,-0.0241755478480393));
#97760=CARTESIAN_POINT('Origin',(-0.184312315726758,2.94644892100903,-0.0494086674092373));
#97761=CARTESIAN_POINT('Ctrl Pts',(6.95587943833,2.877925369,2.81137658738));
#97762=CARTESIAN_POINT('Ctrl Pts',(7.10865512091,2.943232886,2.43338054406));
#97763=CARTESIAN_POINT('Ctrl Pts',(7.2195700295,3.008559221,2.04105504014));
#97764=CARTESIAN_POINT('Ctrl Pts',(6.954415407,2.877925369,2.808221206));
#97765=CARTESIAN_POINT('Ctrl Pts',(7.10701962,2.943232886,2.430304721));
#97766=CARTESIAN_POINT('Ctrl Pts',(7.21777269,3.008559221,2.038076888));
#97767=CARTESIAN_POINT('Ctrl Pts',(6.80801227400001,2.877925369,2.492683068));
#97768=CARTESIAN_POINT('Ctrl Pts',(6.943469529,2.943232886,2.122722415));
#97769=CARTESIAN_POINT('Ctrl Pts',(7.03803874,3.008559221,1.740261674));
#97770=CARTESIAN_POINT('',(7.21777269325456,3.00855922118747,2.03807689497795));
#97771=CARTESIAN_POINT('',(7.12790571420459,3.00855922150568,1.88916928400112));
#97772=CARTESIAN_POINT('',(7.04393413548324,2.91791835922453,2.57545958400812));
#97773=CARTESIAN_POINT('Origin',(-0.182698656706801,2.94642872972437,-0.0619364437379809));
#97774=CARTESIAN_POINT('Ctrl Pts',(6.80962415877199,2.87870320302982,2.48827627387171));
#97775=CARTESIAN_POINT('Ctrl Pts',(6.84860549753355,2.88555248748783,2.50282939327934));
#97776=CARTESIAN_POINT('Ctrl Pts',(6.88764300755156,2.89224022490975,2.51737732889852));
#97777=CARTESIAN_POINT('Ctrl Pts',(6.96573463276544,2.90530189749325,2.54643245134944));
#97778=CARTESIAN_POINT('Ctrl Pts',(7.00483140947897,2.9116829605772,2.56095550664469));
#97779=CARTESIAN_POINT('Ctrl Pts',(7.04393412401197,2.9179183592784,2.57545958125269));
#97780=CARTESIAN_POINT('Ctrl Pts',(6.81785307114309,3.0130934344198,3.12658818002624));
#97781=CARTESIAN_POINT('Ctrl Pts',(6.82370626405869,3.01082632770991,3.11369645271363));
#97782=CARTESIAN_POINT('Ctrl Pts',(6.82955945697441,3.008559221,3.10080472540109));
#97783=CARTESIAN_POINT('Ctrl Pts',(6.99931419217042,2.942808424,2.72691789343058));
#97784=CARTESIAN_POINT('Ctrl Pts',(7.12723960983362,2.877933005,2.33673444667371));
#97785=CARTESIAN_POINT('Ctrl Pts',(6.48726024873397,3.0130934344198,3.23708257895296));
#97786=CARTESIAN_POINT('Ctrl Pts',(6.49332436786697,3.01082632770991,3.22481409447648));
#97787=CARTESIAN_POINT('Ctrl Pts',(6.499388487,3.008559221,3.21254561));
#97788=CARTESIAN_POINT('Ctrl Pts',(6.67526052,2.942808424,2.856734113));
#97789=CARTESIAN_POINT('Ctrl Pts',(6.811239844,2.877933005,2.483850194));
#97790=CARTESIAN_POINT('',(6.82887843149303,3.00855922016357,3.10103521348777));
#97791=CARTESIAN_POINT('Origin',(-0.16720171822584,3.08925211066832,-0.0901480920089814));
#97792=CARTESIAN_POINT('',(6.66413345302227,3.00855921853322,3.15679042217479));
#97793=CARTESIAN_POINT('Origin',(3.60822483003176E-13,3.10034167699911,
1.28369537222284E-13));
#97794=CARTESIAN_POINT('',(7.0437542921393,3.09925366545849,2.5759513724016));
#97795=CARTESIAN_POINT('Origin',(-0.181687328973064,3.08928539963458,-0.0647467316431227));
#97796=CARTESIAN_POINT('Origin',(-0.169381881647932,2.94644890184184,-0.0878752678220951));
#97797=CARTESIAN_POINT('Ctrl Pts',(6.18889198036999,2.877925369,4.24095662977));
#97798=CARTESIAN_POINT('Ctrl Pts',(6.41935382777,2.943232886,3.90464017938));
#97799=CARTESIAN_POINT('Ctrl Pts',(6.61201399403,3.008559221,3.54533045445));
#97800=CARTESIAN_POINT('Ctrl Pts',(6.188140491,2.877925369,4.237560296));
#97801=CARTESIAN_POINT('Ctrl Pts',(6.418417775,2.943232886,3.901284683));
#97802=CARTESIAN_POINT('Ctrl Pts',(6.61089889000001,3.008559221,3.542035555));
#97803=CARTESIAN_POINT('Ctrl Pts',(6.11299155399999,2.877925369,3.897926919));
#97804=CARTESIAN_POINT('Ctrl Pts',(6.324812498,2.943232886,3.565735045));
#97805=CARTESIAN_POINT('Ctrl Pts',(6.499388487,3.008559221,3.21254561));
#97806=CARTESIAN_POINT('',(6.61089889168035,3.00855922118749,3.5420355625124));
#97807=CARTESIAN_POINT('',(6.55514368707799,3.0085592215057,3.37729058526005));
#97808=CARTESIAN_POINT('',(6.32560318942504,2.91791835919154,4.0294843921115));
#97809=CARTESIAN_POINT('Origin',(-0.165112878023673,2.94642872513648,-0.0997632859033443));
#97810=CARTESIAN_POINT('Ctrl Pts',(6.11551308427135,2.87870320302233,3.89396966096815));
#97811=CARTESIAN_POINT('Ctrl Pts',(6.15045457056271,2.8855524874798,3.91656237190437));
#97812=CARTESIAN_POINT('Ctrl Pts',(6.1854520291735,2.89224022489624,3.93916209546234));
#97813=CARTESIAN_POINT('Ctrl Pts',(6.25547191867812,2.90530189663992,3.98432531331739));
#97814=CARTESIAN_POINT('Ctrl Pts',(6.29053260184279,2.91168295886177,4.00691347567795));
#97815=CARTESIAN_POINT('Ctrl Pts',(6.32560317889203,2.91791835925685,4.0294843869756));
#97816=CARTESIAN_POINT('Ctrl Pts',(5.98633141818167,3.01309343439026,4.51912716191478));
#97817=CARTESIAN_POINT('Ctrl Pts',(5.99481910694851,3.01082632769513,4.50779509954357));
#97818=CARTESIAN_POINT('Ctrl Pts',(6.00330679571537,3.008559221,4.49646303717236));
#97819=CARTESIAN_POINT('Ctrl Pts',(6.2494673766473,2.942808424,4.16780972140263));
#97820=CARTESIAN_POINT('Ctrl Pts',(6.45827987543194,2.877933005,3.81424873072673));
#97821=CARTESIAN_POINT('Ctrl Pts',(5.63971464235043,3.01309343439026,4.55597057842557));
#97822=CARTESIAN_POINT('Ctrl Pts',(5.64827434717523,3.01082632769513,4.54529253071275));
#97823=CARTESIAN_POINT('Ctrl Pts',(5.65683405200001,3.008559221,4.534614483));
#97824=CARTESIAN_POINT('Ctrl Pts',(5.905083248,2.942808424,4.224928949));
#97825=CARTESIAN_POINT('Ctrl Pts',(6.118042472,2.877933005,3.889994385));
#97826=CARTESIAN_POINT('',(6.00259214409304,3.00855922016357,4.49654173624063));
#97827=CARTESIAN_POINT('Origin',(-0.143913387883455,3.08925206949373,-0.123983845329459));
#97828=CARTESIAN_POINT('',(5.82971308973404,3.00855921853322,4.51557811846257));
#97829=CARTESIAN_POINT('Origin',(2.78856798763272E-13,3.100341677,1.81278603239576E-13));
#97830=CARTESIAN_POINT('',(6.32532183056699,3.09925366549247,4.02992602189084));
#97831=CARTESIAN_POINT('Origin',(-0.163520847236953,3.08928539071856,-0.102290334525119));
#97832=CARTESIAN_POINT('Origin',(-0.14653118572046,2.94644889901171,-0.122232846529689));
#97833=CARTESIAN_POINT('Ctrl Pts',(5.1325188116,2.877925369,5.47223425438));
#97834=CARTESIAN_POINT('Ctrl Pts',(5.42989068484001,2.943232886,5.19332318041001));
#97835=CARTESIAN_POINT('Ctrl Pts',(5.69528753253,3.008559221,4.88383015693));
#97836=CARTESIAN_POINT('Ctrl Pts',(5.132515003,2.877925369,5.468755777));
#97837=CARTESIAN_POINT('Ctrl Pts',(5.429697849,2.943232886,5.18984491));
#97838=CARTESIAN_POINT('Ctrl Pts',(5.694906805,3.008559221,4.880372576));
#97839=CARTESIAN_POINT('Ctrl Pts',(5.132134143,2.877925369,5.120908039));
#97840=CARTESIAN_POINT('Ctrl Pts',(5.410414265,2.943232886,4.842017869));
#97841=CARTESIAN_POINT('Ctrl Pts',(5.656834052,3.008559221,4.534614483));
#97842=CARTESIAN_POINT('',(5.69490680616228,3.0085592211877,4.8803725814005));
#97843=CARTESIAN_POINT('',(5.67587042651797,3.00855922150568,4.70749353188976));
#97844=CARTESIAN_POINT('',(5.31149406848905,2.917918359164,5.29509498865337));
#97845=CARTESIAN_POINT('Origin',(-0.139806310419599,2.94642872523138,-0.132925095633846));
#97846=CARTESIAN_POINT('Ctrl Pts',(5.13544741496531,2.8787032030605,5.1175853537983));
#97847=CARTESIAN_POINT('Ctrl Pts',(5.16471522369949,2.88555248750377,5.14716124648086));
#97848=CARTESIAN_POINT('Ctrl Pts',(5.19403618863513,2.89224022490984,5.17675602021783));
#97849=CARTESIAN_POINT('Ctrl Pts',(5.25271028727322,2.90530189488208,5.23591554579191));
#97850=CARTESIAN_POINT('Ctrl Pts',(5.2820954749823,2.91168295528719,5.26551261105691));
#97851=CARTESIAN_POINT('Ctrl Pts',(5.31149405931312,2.91791835921186,5.29509498119979));
#97852=CARTESIAN_POINT('Ctrl Pts',(4.87489556082486,3.01309343436845,5.70035678014367));
#97853=CARTESIAN_POINT('Ctrl Pts',(4.88562087052289,3.01082632768423,5.69111425733716));
#97854=CARTESIAN_POINT('Ctrl Pts',(4.89634618022078,3.008559221,5.68187173453059));
#97855=CARTESIAN_POINT('Ctrl Pts',(5.20740241132506,2.942808424,5.41381939934602));
#97856=CARTESIAN_POINT('Ctrl Pts',(5.4873381521754,2.877933005,5.11341298321379));
#97857=CARTESIAN_POINT('Ctrl Pts',(4.52846224745558,3.01309343436846,5.66182645664609));
#97858=CARTESIAN_POINT('Ctrl Pts',(4.5391172957278,3.01082632768423,5.65323813932303));
#97859=CARTESIAN_POINT('Ctrl Pts',(4.549772344,3.008559221,5.644649822));
#97860=CARTESIAN_POINT('Ctrl Pts',(4.85879084800001,2.942808424,5.395570803));
#97861=CARTESIAN_POINT('Ctrl Pts',(5.138772234,2.877933005,5.114246761));
#97862=CARTESIAN_POINT('',(4.89563131846189,3.00855922016355,5.68179496485426));
#97863=CARTESIAN_POINT('Origin',(-0.113895955393939,3.08925208356024,-0.152022352616782));
#97864=CARTESIAN_POINT('',(4.72270182137908,3.00855921853322,5.66322240019098));
#97865=CARTESIAN_POINT('Origin',(-3.77302356024956E-14,3.100341677,-3.51281503885303E-14));
#97866=CARTESIAN_POINT('',(5.31112435035528,3.09925366548904,5.29546580931712));
#97867=CARTESIAN_POINT('Origin',(-0.137708370213362,3.08928540048914,-0.135050933526252));
#97868=CARTESIAN_POINT('Origin',(-0.116828942207328,2.94644888520062,-0.150875016634339));
#97869=CARTESIAN_POINT('Ctrl Pts',(3.83615476674,2.877925369,6.44763628624));
#97870=CARTESIAN_POINT('Ctrl Pts',(4.18653188712,2.943232886,6.23917216139));
#97871=CARTESIAN_POINT('Ctrl Pts',(4.51225575563,3.008559221,5.99396738978));
#97872=CARTESIAN_POINT('Ctrl Pts',(3.836898817,2.877925369,6.444238315));
#97873=CARTESIAN_POINT('Ctrl Pts',(4.187091285,2.943232886,6.235733757));
#97874=CARTESIAN_POINT('Ctrl Pts',(4.512627207,3.008559221,5.9905088));
#97875=CARTESIAN_POINT('Ctrl Pts',(3.911303843,2.877925369,6.104441191));
#97876=CARTESIAN_POINT('Ctrl Pts',(4.243031073,2.943232886,5.891893318));
#97877=CARTESIAN_POINT('Ctrl Pts',(4.549772344,3.008559221,5.644649822));
#97878=CARTESIAN_POINT('',(4.51262720696789,3.00855922118776,5.99050880554579));
#97879=CARTESIAN_POINT('',(4.53119977305047,3.0085592215057,5.81757931290789));
#97880=CARTESIAN_POINT('',(4.04902538805296,2.91791835924187,6.31311282809917));
#97881=CARTESIAN_POINT('Origin',(-0.107962680822556,2.94642870747082,-0.15987151407948));
#97882=CARTESIAN_POINT('Ctrl Pts',(3.91525393165377,2.87870320305441,6.10190844352905));
#97883=CARTESIAN_POINT('Ctrl Pts',(3.93747953250698,2.88555248749456,6.1370845819654));
#97884=CARTESIAN_POINT('Ctrl Pts',(3.95975298798327,2.89224022490414,6.17229058701452));
#97885=CARTESIAN_POINT('Ctrl Pts',(4.00433778169506,2.90530189846678,6.24268021169786));
#97886=CARTESIAN_POINT('Ctrl Pts',(4.02667347970861,2.91168296256646,6.27790228240161));
#97887=CARTESIAN_POINT('Ctrl Pts',(4.04902538054254,2.91791835930351,6.31311281906005));
#97888=CARTESIAN_POINT('Ctrl Pts',(3.5355150063926,3.01309343420852,6.61504405096348));
#97889=CARTESIAN_POINT('Ctrl Pts',(3.5479764330658,3.01082632760426,6.60832323795142));
#97890=CARTESIAN_POINT('Ctrl Pts',(3.56043785973906,3.008559221,6.60160242493936));
#97891=CARTESIAN_POINT('Ctrl Pts',(3.9218450974854,2.942808424,6.40668489825574));
#97892=CARTESIAN_POINT('Ctrl Pts',(4.25981459580143,2.877933005,6.17347972710565));
#97893=CARTESIAN_POINT('Ctrl Pts',(3.20546399185573,3.01309343420852,6.50294162320019));
#97894=CARTESIAN_POINT('Ctrl Pts',(3.21771616492783,3.01082632760426,6.4968446166001));
#97895=CARTESIAN_POINT('Ctrl Pts',(3.229968338,3.008559221,6.49074761));
#97896=CARTESIAN_POINT('Ctrl Pts',(3.585306787,2.942808424,6.313921764));
#97897=CARTESIAN_POINT('Ctrl Pts',(3.919218717,2.877933005,6.099362643));
#97898=CARTESIAN_POINT('',(3.55975621426659,3.00855922016355,6.60137377596147));
#97899=CARTESIAN_POINT('Origin',(-0.0785529492724818,3.08925207262269,-0.172952618710034));
#97900=CARTESIAN_POINT('',(3.3948622650675,3.00855921853322,6.54606069746625));
#97901=CARTESIAN_POINT('Origin',(4.56665955050894E-13,3.10034167699978,
6.96057794735694E-13));
#97902=CARTESIAN_POINT('',(4.04858459835594,3.09925366545561,6.31339550070091));
#97903=CARTESIAN_POINT('Origin',(-0.105456859436555,3.08928538134748,-0.161496726582855));
#97904=CARTESIAN_POINT('Origin',(-0.0816639073474729,2.94644894146221,-0.172462423706753));
#97905=CARTESIAN_POINT('Ctrl Pts',(2.36041638985,2.877925369,7.12155401276));
#97906=CARTESIAN_POINT('Ctrl Pts',(2.74741551223,2.943232886,6.9932843864));
#97907=CARTESIAN_POINT('Ctrl Pts',(3.11823591539,3.008559221,6.82383336981));
#97908=CARTESIAN_POINT('Ctrl Pts',(2.361873508,2.877925369,7.118395433));
#97909=CARTESIAN_POINT('Ctrl Pts',(2.748700987,2.943232886,6.990046624));
#97910=CARTESIAN_POINT('Ctrl Pts',(3.119342177,3.008559221,6.820535491));
#97911=CARTESIAN_POINT('Ctrl Pts',(2.507585323,2.877925369,6.802537457));
#97912=CARTESIAN_POINT('Ctrl Pts',(2.877248464,2.943232886,6.666270384));
#97913=CARTESIAN_POINT('Ctrl Pts',(3.229968338,3.008559221,6.49074761));
#97914=CARTESIAN_POINT('',(3.11934217580073,3.00855922118776,6.82053549638459));
#97915=CARTESIAN_POINT('',(3.17465525469764,3.0085592215057,6.65564155183669));
#97916=CARTESIAN_POINT('',(2.5972287809459,2.91791835920175,7.03593652892802));
#97917=CARTESIAN_POINT('Origin',(-0.0710709945505126,2.94642870905485,-0.17934275964715));
#97918=CARTESIAN_POINT('Ctrl Pts',(2.51198752636156,2.87870320303939,6.8009130764396));
#97919=CARTESIAN_POINT('Ctrl Pts',(2.52613167518388,2.88555248749972,6.84004466358328));
#97920=CARTESIAN_POINT('Ctrl Pts',(2.54031613932612,2.89224022492161,6.87921570642526));
#97921=CARTESIAN_POINT('Ctrl Pts',(2.5687268716989,2.90530189613789,6.95754405958114));
#97922=CARTESIAN_POINT('Ctrl Pts',(2.58296866366645,2.91168295781116,6.99674415685239));
#97923=CARTESIAN_POINT('Ctrl Pts',(2.59722877565496,2.91791835924352,7.03593651830473));
#97924=CARTESIAN_POINT('Ctrl Pts',(2.03081769722786,3.01309343440098,7.22041921455049));
#97925=CARTESIAN_POINT('Ctrl Pts',(2.04443255938671,3.0108263277005,7.2165343686569));
#97926=CARTESIAN_POINT('Ctrl Pts',(2.05804742154557,3.008559221,7.21264952276332));
#97927=CARTESIAN_POINT('Ctrl Pts',(2.45290666561806,2.942808424,7.09998093346858));
#97928=CARTESIAN_POINT('Ctrl Pts',(2.83310684306066,2.877933005,6.94488142064696));
#97929=CARTESIAN_POINT('Ctrl Pts',(1.73258180030284,3.01309343440098,7.03998646713984));
#97930=CARTESIAN_POINT('Ctrl Pts',(1.74585820115142,3.0108263277005,7.03666586006987));
#97931=CARTESIAN_POINT('Ctrl Pts',(1.759134602,3.008559221,7.033345253));
#97932=CARTESIAN_POINT('Ctrl Pts',(2.144177766,2.942808424,6.93704076));
#97933=CARTESIAN_POINT('Ctrl Pts',(2.516406889,2.877933005,6.799279107));
#97934=CARTESIAN_POINT('',(2.05743086531991,3.00855922016355,7.21227968582777));
#97935=CARTESIAN_POINT('Origin',(-0.0395366255264623,3.08925206834798,-0.185795359950095));
#97936=CARTESIAN_POINT('',(1.908282721884,3.00855921853322,7.12281247141579));
#97937=CARTESIAN_POINT('Origin',(1.93204827136917E-13,3.10034167700056,
4.70543742858709E-13));
#97938=CARTESIAN_POINT('',(2.59673753012002,3.09925366546135,7.0361178357594));
#97939=CARTESIAN_POINT('Origin',(-0.068274347774625,3.08928543181574,-0.180391257391856));
#97940=CARTESIAN_POINT('Origin',(-0.0426803358656677,2.94644893093892,-0.18598572011913));
#97941=CARTESIAN_POINT('Ctrl Pts',(0.77430756518,2.877925369,7.46247578759));
#97942=CARTESIAN_POINT('Ctrl Pts',(1.17983304171,2.943232886,7.42039840523001));
#97943=CARTESIAN_POINT('Ctrl Pts',(1.57841082871,3.008559221,7.33462448469));
#97944=CARTESIAN_POINT('Ctrl Pts',(0.776409618,2.877925369,7.459704291));
#97945=CARTESIAN_POINT('Ctrl Pts',(1.181784486,2.943232886,7.417512679));
#97946=CARTESIAN_POINT('Ctrl Pts',(1.580200173,3.008559221,7.331641522));
#97947=CARTESIAN_POINT('Ctrl Pts',(0.9866149,2.877925369,7.182554632));
#97948=CARTESIAN_POINT('Ctrl Pts',(1.376928915,2.943232886,7.128940056));
#97949=CARTESIAN_POINT('Ctrl Pts',(1.759134602,3.008559221,7.033345253));
#97950=CARTESIAN_POINT('',(1.58020017063694,3.00855922118764,7.33164152700582));
#97951=CARTESIAN_POINT('',(1.6696673844759,3.00855922150568,7.18249338820299));
#97952=CARTESIAN_POINT('',(1.02398864236711,2.91791835919281,7.42976765700797));
#97953=CARTESIAN_POINT('Origin',(-0.0308560152958731,2.94642874674394,-0.190428015592459));
#97954=CARTESIAN_POINT('Ctrl Pts',(0.991263375971088,2.87870320295771,7.18191457174582));
#97955=CARTESIAN_POINT('Ctrl Pts',(0.996664707981171,2.8855524874312,7.22317185808551));
#97956=CARTESIAN_POINT('Ctrl Pts',(1.00209693091953,2.89224022486283,7.26447634427217));
#97957=CARTESIAN_POINT('Ctrl Pts',(1.01300515576209,2.90530189631038,7.34708089317344));
#97958=CARTESIAN_POINT('Ctrl Pts',(1.01848712055922,2.91168295820948,7.38842607981061));
#97959=CARTESIAN_POINT('Ctrl Pts',(1.02398863947782,2.91791835924874,7.42976764558548));
#97960=CARTESIAN_POINT('Ctrl Pts',(0.431161610006125,3.01309343448858,7.48817560015396));
#97961=CARTESIAN_POINT('Ctrl Pts',(0.445293291560477,3.01082632774429,7.48730837269801));
#97962=CARTESIAN_POINT('Ctrl Pts',(0.459424973114821,3.008559221,7.48644114524202));
#97963=CARTESIAN_POINT('Ctrl Pts',(0.869273043783379,2.942808424,7.46128975060442));
#97964=CARTESIAN_POINT('Ctrl Pts',(1.27392616357086,2.877933005,7.39154817729766));
#97965=CARTESIAN_POINT('Ctrl Pts',(0.178686009798803,3.01309343448857,7.24784936885774));
#97966=CARTESIAN_POINT('Ctrl Pts',(0.192365848399401,3.01082632774429,7.24746042942882));
#97967=CARTESIAN_POINT('Ctrl Pts',(0.206045687,3.008559221,7.24707149000001));
#97968=CARTESIAN_POINT('Ctrl Pts',(0.602789375,2.942808424,7.23579144));
#97969=CARTESIAN_POINT('Ctrl Pts',(0.995930671,2.877933005,7.18126883600001));
#97970=CARTESIAN_POINT('',(0.458902335631921,3.00855922016356,7.48594741351763));
#97971=CARTESIAN_POINT('Origin',(0.0013282379281003,3.08925208342711,-0.189950700615894));
#97972=CARTESIAN_POINT('',(0.332473999383933,3.00855921853322,7.36650945118224));
#97973=CARTESIAN_POINT('Origin',(1.94180609092154E-13,3.10034167700033,
1.34354333214404E-12));
#97974=CARTESIAN_POINT('',(1.02346990113189,3.09925366544343,7.42983912063186));
#97975=CARTESIAN_POINT('Origin',(-0.0278993116907882,3.08928541688475,-0.190850557821854));
#97976=CARTESIAN_POINT('Origin',(-0.00170107075175882,2.94644892730587,
-0.190812579955236));
#97977=CARTESIAN_POINT('Origin',(1.23451663930525E-13,3.10034167700011,
-6.50521303491303E-15));
#97978=CARTESIAN_POINT('',(-0.0328302415903184,3.00855922118746,7.49992815038451));
#97979=CARTESIAN_POINT('Origin',(0.0108017888965188,2.94642871640652,-0.192608996549439));
#97980=CARTESIAN_POINT('',(-0.597654043017233,3.09925366546969,7.47614938614295));
#97981=CARTESIAN_POINT('Origin',(0.0137802093178851,3.08928541963158,-0.192386424768728));
#97982=CARTESIAN_POINT('Origin',(0.0393577271373455,2.94644892036822,-0.186716823481069));
#97983=CARTESIAN_POINT('Ctrl Pts',(-0.848007020840001,2.877925369,7.45446048832));
#97984=CARTESIAN_POINT('Ctrl Pts',(-0.44291711145,2.943232886,7.50054284272));
#97985=CARTESIAN_POINT('Ctrl Pts',(-0.03521899321,3.008559221,7.50245671155));
#97986=CARTESIAN_POINT('Ctrl Pts',(-0.845358323000001,2.877925369,7.452205667));
#97987=CARTESIAN_POINT('Ctrl Pts',(-0.440390945,2.943232886,7.498144086));
#97988=CARTESIAN_POINT('Ctrl Pts',(-0.032830234,3.008559221,7.499928145));
#97989=CARTESIAN_POINT('Ctrl Pts',(-0.580488539,2.877925369,7.226723535));
#97990=CARTESIAN_POINT('Ctrl Pts',(-0.1877743,2.943232886,7.258268414));
#97991=CARTESIAN_POINT('Ctrl Pts',(0.206045687,3.008559221,7.24707149));
#97992=CARTESIAN_POINT('',(0.0866077233954782,3.00855922150568,7.37349981753647));
#97993=CARTESIAN_POINT('Ctrl Pts',(-0.029340091,2.749235821,7.49994261));
#97994=CARTESIAN_POINT('Ctrl Pts',(0.377052547,2.813580595,7.501532435));
#97995=CARTESIAN_POINT('Ctrl Pts',(0.781237513,2.878703203,7.459200222));
#97996=CARTESIAN_POINT('Ctrl Pts',(0.209418136,2.749235821,7.24697482));
#97997=CARTESIAN_POINT('Ctrl Pts',(0.602103436,2.813580595,7.23562726800001));
#97998=CARTESIAN_POINT('Ctrl Pts',(0.991263375,2.878703203,7.181914572));
#97999=CARTESIAN_POINT('',(0.21408150377158,2.75000000010809,7.24683856069753));
#98000=CARTESIAN_POINT('Origin',(-0.0379385088426389,2.94638854356868,-0.192403914175406));
#98001=CARTESIAN_POINT('Ctrl Pts',(0.214081499285152,2.75000000023897,7.24683856080862));
#98002=CARTESIAN_POINT('Ctrl Pts',(0.215310080966762,2.75681548608773,7.28842710418195));
#98003=CARTESIAN_POINT('Ctrl Pts',(0.216481064139149,2.76346377140411,7.33007120365252));
#98004=CARTESIAN_POINT('Ctrl Pts',(0.218715591036004,2.77643548664992,7.41336050560333));
#98005=CARTESIAN_POINT('Ctrl Pts',(0.219780458532496,2.78276663813192,7.45505532086176));
#98006=CARTESIAN_POINT('Ctrl Pts',(0.220796264044522,2.78894740126139,7.49674922945488));
#98007=CARTESIAN_POINT('Ctrl Pts',(1.26042412866189,2.88000589655946,7.39333476721524));
#98008=CARTESIAN_POINT('Ctrl Pts',(1.26448657633095,2.87935454977973,7.39263760060762));
#98009=CARTESIAN_POINT('Ctrl Pts',(1.268549024,2.878703203,7.391940434));
#98010=CARTESIAN_POINT('Ctrl Pts',(1.448039577,2.84992484,7.36113762));
#98011=CARTESIAN_POINT('Ctrl Pts',(1.625823574,2.821428571,7.321659491));
#98012=CARTESIAN_POINT('Ctrl Pts',(1.849718912,2.785541304,7.27194203));
#98013=CARTESIAN_POINT('Ctrl Pts',(2.070158035,2.7492206,7.208636883));
#98014=CARTESIAN_POINT('Ctrl Pts',(0.983369330860882,2.88000589655946,7.18300412502963));
#98015=CARTESIAN_POINT('Ctrl Pts',(0.987316352930441,2.87935454977973,7.18245934851482));
#98016=CARTESIAN_POINT('Ctrl Pts',(0.991263374999999,2.878703203,7.181914572));
#98017=CARTESIAN_POINT('Ctrl Pts',(1.165654095,2.84992484,7.157844788));
#98018=CARTESIAN_POINT('Ctrl Pts',(1.338671059,2.821428571,7.125339276));
#98019=CARTESIAN_POINT('Ctrl Pts',(1.556562952,2.785541304,7.084402899));
#98020=CARTESIAN_POINT('Ctrl Pts',(1.771546394,2.7492206,7.030229255));
#98021=CARTESIAN_POINT('',(1.76693247181021,2.75000000024246,7.03139031398057));
#98022=CARTESIAN_POINT('Ctrl Pts',(1.76693247079244,2.75000000016349,7.03139031557349));
#98023=CARTESIAN_POINT('Ctrl Pts',(1.554222808,2.785926731,7.08484255300001));
#98024=CARTESIAN_POINT('Ctrl Pts',(1.338671059,2.821428571,7.125339276));
#98025=CARTESIAN_POINT('Ctrl Pts',(1.16565409579847,2.84992483975151,7.15784478833025));
#98026=CARTESIAN_POINT('Ctrl Pts',(0.991263377398236,2.8787032050476,7.1819145845472));
#98027=CARTESIAN_POINT('Ctrl Pts',(1.82721365293106,2.78894740126369,7.27401472802548));
#98028=CARTESIAN_POINT('Ctrl Pts',(1.81725845690575,2.78276652545196,7.23351322969728));
#98029=CARTESIAN_POINT('Ctrl Pts',(1.80725542864887,2.77643543151709,7.19302252590466));
#98030=CARTESIAN_POINT('Ctrl Pts',(1.7871684916059,2.7634637717899,7.11216118491727));
#98031=CARTESIAN_POINT('Ctrl Pts',(1.77707263610211,2.75681548728098,7.07174243303508));
#98032=CARTESIAN_POINT('Ctrl Pts',(1.766932470127,2.75000000123112,7.03139031423657));
#98033=CARTESIAN_POINT('Ctrl Pts',(1.583611829,2.749235821,7.330905372));
#98034=CARTESIAN_POINT('Ctrl Pts',(1.980844998,2.813580595,7.24509562400001));
#98035=CARTESIAN_POINT('Ctrl Pts',(2.36648017,2.878703203,7.116865294));
#98036=CARTESIAN_POINT('Ctrl Pts',(1.762407424,2.749235821,7.032525867));
#98037=CARTESIAN_POINT('Ctrl Pts',(2.143472571,2.813580595,6.937027883));
#98038=CARTESIAN_POINT('Ctrl Pts',(2.511987525,2.878703203,6.800913077));
#98039=CARTESIAN_POINT('Origin',(-0.0784132692517919,2.94638885126936,-0.179751477231472));
#98040=CARTESIAN_POINT('Ctrl Pts',(2.82030454263079,2.88000589655946,6.94952877882882));
#98041=CARTESIAN_POINT('Ctrl Pts',(2.8241221423154,2.87935454977973,6.94797460541441));
#98042=CARTESIAN_POINT('Ctrl Pts',(2.827939742,2.878703203,6.946420432));
#98043=CARTESIAN_POINT('Ctrl Pts',(2.996612211,2.84992484,6.877752607));
#98044=CARTESIAN_POINT('Ctrl Pts',(3.161753086,2.821428571,6.800979152));
#98045=CARTESIAN_POINT('Ctrl Pts',(3.369726091,2.785541304,6.704293178));
#98046=CARTESIAN_POINT('Ctrl Pts',(3.571402735,2.7492206,6.595080174));
#98047=CARTESIAN_POINT('Ctrl Pts',(2.50451226091208,2.88000589655946,6.8036741430437));
#98048=CARTESIAN_POINT('Ctrl Pts',(2.50824989295604,2.87935454977973,6.80229361002185));
#98049=CARTESIAN_POINT('Ctrl Pts',(2.511987525,2.878703203,6.800913077));
#98050=CARTESIAN_POINT('Ctrl Pts',(2.677126795,2.84992484,6.739917181));
#98051=CARTESIAN_POINT('Ctrl Pts',(2.839110994,2.821428571,6.670978097));
#98052=CARTESIAN_POINT('Ctrl Pts',(3.043108585,2.785541304,6.584158473));
#98053=CARTESIAN_POINT('Ctrl Pts',(3.241420102,2.7492206,6.485036293));
#98054=CARTESIAN_POINT('',(3.2371636440605,2.75000000044536,6.48716206480851));
#98055=CARTESIAN_POINT('Ctrl Pts',(3.23716364325933,2.75000000162247,6.48716206668083));
#98056=CARTESIAN_POINT('Ctrl Pts',(3.040917665,2.785926731,6.58509091));
#98057=CARTESIAN_POINT('Ctrl Pts',(2.839110994,2.821428571,6.670978097));
#98058=CARTESIAN_POINT('Ctrl Pts',(2.67712679515999,2.84992483971241,6.73991718073424));
#98059=CARTESIAN_POINT('Ctrl Pts',(2.51198753070824,2.87870320492457,6.80091308879405));
#98060=CARTESIAN_POINT('Ctrl Pts',(3.34819256082345,2.7889474012859,6.71115538278797));
#98061=CARTESIAN_POINT('Ctrl Pts',(3.32976346314604,2.78276651747819,6.67374081136571));
#98062=CARTESIAN_POINT('Ctrl Pts',(3.31129000853237,2.77643542761869,6.63634713883759));
#98063=CARTESIAN_POINT('Ctrl Pts',(3.27428990639928,2.76346377185177,6.56169441127519));
#98064=CARTESIAN_POINT('Ctrl Pts',(3.25574124988583,2.75681548744549,6.52439093826907));
#98065=CARTESIAN_POINT('Ctrl Pts',(3.2371636426348,2.7500000013915,6.48716206534674));
#98066=CARTESIAN_POINT('Ctrl Pts',(3.122515819,2.749235821,6.819083146));
#98067=CARTESIAN_POINT('Ctrl Pts',(3.492015338,2.813580595,6.649886193));
#98068=CARTESIAN_POINT('Ctrl Pts',(3.841068843,2.878703203,6.441753654));
#98069=CARTESIAN_POINT('Ctrl Pts',(3.232988499,2.749235821,6.489243821));
#98070=CARTESIAN_POINT('Ctrl Pts',(3.584615312,2.813580595,6.314060784));
#98071=CARTESIAN_POINT('Ctrl Pts',(3.91525393,2.878703203,6.101908444));
#98072=CARTESIAN_POINT('Origin',(-0.115221125141765,2.94638888321458,-0.158692166271711));
#98073=CARTESIAN_POINT('Ctrl Pts',(4.24831064998266,2.88000589655946,6.18077054856216));
#98074=CARTESIAN_POINT('Ctrl Pts',(4.25170489499133,2.87935454977973,6.17843203978108));
#98075=CARTESIAN_POINT('Ctrl Pts',(4.25509914,2.878703203,6.176093531));
#98076=CARTESIAN_POINT('Ctrl Pts',(4.405066589,2.84992484,6.072771527));
#98077=CARTESIAN_POINT('Ctrl Pts',(4.549842538,2.821428571,5.962292586));
#98078=CARTESIAN_POINT('Ctrl Pts',(4.732168624,2.785541304,5.823159028));
#98079=CARTESIAN_POINT('Ctrl Pts',(4.905652612,2.7492206,5.673144847));
#98080=CARTESIAN_POINT('Ctrl Pts',(3.90854698097101,2.88000589655946,6.10621191864682));
#98081=CARTESIAN_POINT('Ctrl Pts',(3.9119004554855,2.87935454977973,6.1040601813234));
#98082=CARTESIAN_POINT('Ctrl Pts',(3.91525393,2.878703203,6.101908444));
#98083=CARTESIAN_POINT('Ctrl Pts',(4.063420022,2.84992484,6.006838537));
#98084=CARTESIAN_POINT('Ctrl Pts',(4.206797255,2.821428571,5.904689396));
#98085=CARTESIAN_POINT('Ctrl Pts',(4.387361843,2.785541304,5.776046115));
#98086=CARTESIAN_POINT('Ctrl Pts',(4.559728608,2.7492206,5.63661024200001));
#98087=CARTESIAN_POINT('',(4.55602864185247,2.75000000024269,5.63960132672671));
#98088=CARTESIAN_POINT('Ctrl Pts',(4.55602864156567,2.75000000016349,5.6396013285999));
#98089=CARTESIAN_POINT('Ctrl Pts',(4.385422592,2.785926731,5.777427735));
#98090=CARTESIAN_POINT('Ctrl Pts',(4.206797255,2.821428571,5.904689396));
#98091=CARTESIAN_POINT('Ctrl Pts',(4.06342002219976,2.84992483978415,6.00683853671871));
#98092=CARTESIAN_POINT('Ctrl Pts',(3.91525393793725,2.87870320492457,6.10190845425346));
#98093=CARTESIAN_POINT('Ctrl Pts',(4.71261370641487,2.78894740132361,5.83448987095168));
#98094=CARTESIAN_POINT('Ctrl Pts',(4.68657244114061,2.78276651684776,5.80191173920188));
#98095=CARTESIAN_POINT('Ctrl Pts',(4.66049235275823,2.77643542728415,5.76936355833918));
#98096=CARTESIAN_POINT('Ctrl Pts',(4.60830916401841,2.763463771782,5.70441009966584));
#98097=CARTESIAN_POINT('Ctrl Pts',(4.58217502077462,2.75681548733964,5.67196617377621));
#98098=CARTESIAN_POINT('Ctrl Pts',(4.55602864065931,2.75000000128407,5.63960132747132));
#98099=CARTESIAN_POINT('Ctrl Pts',(4.51541444,2.749235821,5.988408172));
#98100=CARTESIAN_POINT('Ctrl Pts',(4.839902922,2.813580595,5.743735475));
#98101=CARTESIAN_POINT('Ctrl Pts',(5.136053407,2.878703203,5.465432773));
#98102=CARTESIAN_POINT('Ctrl Pts',(4.552398626,2.749235821,5.642531945));
#98103=CARTESIAN_POINT('Ctrl Pts',(4.858145424,2.813580595,5.39585522));
#98104=CARTESIAN_POINT('Ctrl Pts',(5.135447414,2.878703203,5.117585355));
#98105=CARTESIAN_POINT('Origin',(-0.14664156078291,2.94638884551593,-0.130213051369702));
#98106=CARTESIAN_POINT('Ctrl Pts',(5.47767047366261,2.88000589655946,5.12300635715573));
#98107=CARTESIAN_POINT('Ctrl Pts',(5.48048265283131,2.87935454977973,5.11999285907787));
#98108=CARTESIAN_POINT('Ctrl Pts',(5.483294832,2.878703203,5.116979361));
#98109=CARTESIAN_POINT('Ctrl Pts',(5.607544948,2.84992484,4.98383440000001));
#98110=CARTESIAN_POINT('Ctrl Pts',(5.72518641,2.821428571,4.844815845));
#98111=CARTESIAN_POINT('Ctrl Pts',(5.87334021100001,2.785541304,4.669740434));
#98112=CARTESIAN_POINT('Ctrl Pts',(6.01051962500001,2.7492206,4.485939572));
#98113=CARTESIAN_POINT('Ctrl Pts',(5.12982238961246,2.88000589655946,5.12323001261221));
#98114=CARTESIAN_POINT('Ctrl Pts',(5.13263490180623,2.87935454977973,5.12040768380611));
#98115=CARTESIAN_POINT('Ctrl Pts',(5.135447414,2.878703203,5.117585355));
#98116=CARTESIAN_POINT('Ctrl Pts',(5.259712244,2.84992484,4.992886799));
#98117=CARTESIAN_POINT('Ctrl Pts',(5.377778351,2.821428571,4.862303981));
#98118=CARTESIAN_POINT('Ctrl Pts',(5.526466937,2.785541304,4.69785226000001));
#98119=CARTESIAN_POINT('Ctrl Pts',(5.664829272,2.7492206,4.524622561));
#98120=CARTESIAN_POINT('',(5.66185880360023,2.75000000045047,4.52833909919778));
#98121=CARTESIAN_POINT('Ctrl Pts',(5.66185880364956,2.75000000162248,4.52833910122305));
#98122=CARTESIAN_POINT('Ctrl Pts',(5.524870032,2.785926731,4.69961846000001));
#98123=CARTESIAN_POINT('Ctrl Pts',(5.377778351,2.821428571,4.862303981));
#98124=CARTESIAN_POINT('Ctrl Pts',(5.2597122443229,2.84992483969487,4.99288679854226));
#98125=CARTESIAN_POINT('Ctrl Pts',(5.13544742381051,2.87870320490793,5.11758536321659));
#98126=CARTESIAN_POINT('Ctrl Pts',(5.85667827296398,2.788947401284,4.6850100969931));
#98127=CARTESIAN_POINT('Ctrl Pts',(5.82424314032519,2.78276663833772,4.65879224167537));
#98128=CARTESIAN_POINT('Ctrl Pts',(5.79177555452673,2.77643548702863,4.632611192457));
#98129=CARTESIAN_POINT('Ctrl Pts',(5.72684900691137,2.76346377178021,4.58039391214018));
#98130=CARTESIAN_POINT('Ctrl Pts',(5.69435138024918,2.7568154873266,4.5543265754526));
#98131=CARTESIAN_POINT('Ctrl Pts',(5.66185880267492,2.75000000127586,4.52833910013824));
#98132=CARTESIAN_POINT('Ctrl Pts',(5.697177301,2.749235821,4.877721886));
#98133=CARTESIAN_POINT('Ctrl Pts',(5.961482025,2.813580595,4.56901407));
#98134=CARTESIAN_POINT('Ctrl Pts',(6.190881822,2.878703203,4.23355433));
#98135=CARTESIAN_POINT('Ctrl Pts',(5.658943652,2.749235821,4.531981548));
#98136=CARTESIAN_POINT('Ctrl Pts',(5.90451405500001,2.813580595,4.225345463));
#98137=CARTESIAN_POINT('Ctrl Pts',(6.115513083,2.878703203,3.893969662));
#98138=CARTESIAN_POINT('Origin',(-0.171205151932938,2.94638883973356,-0.0956451587712737));
#98139=CARTESIAN_POINT('Ctrl Pts',(6.45090051407246,2.88000589655946,3.82569608212552));
#98140=CARTESIAN_POINT('Ctrl Pts',(6.45299913303623,2.87935454977973,3.82214850256276));
#98141=CARTESIAN_POINT('Ctrl Pts',(6.455097752,2.878703203,3.818600923));
#98142=CARTESIAN_POINT('Ctrl Pts',(6.54782073800001,2.84992484,3.661858715));
#98143=CARTESIAN_POINT('Ctrl Pts',(6.632826928,2.821428571,3.5008009));
#98144=CARTESIAN_POINT('Ctrl Pts',(6.739880937,2.785541304,3.297969967));
#98145=CARTESIAN_POINT('Ctrl Pts',(6.834341421,2.7492206,3.088976748));
#98146=CARTESIAN_POINT('Ctrl Pts',(6.11123300303657,2.88000589655946,3.90069156461084));
#98147=CARTESIAN_POINT('Ctrl Pts',(6.11337304301828,2.87935454977973,3.89733061330542));
#98148=CARTESIAN_POINT('Ctrl Pts',(6.115513083,2.878703203,3.893969662));
#98149=CARTESIAN_POINT('Ctrl Pts',(6.210066168,2.84992484,3.745473224));
#98150=CARTESIAN_POINT('Ctrl Pts',(6.297300509,2.821428571,3.592562637));
#98151=CARTESIAN_POINT('Ctrl Pts',(6.40716058,2.785541304,3.399992054));
#98152=CARTESIAN_POINT('Ctrl Pts',(6.50504881499999,2.7492206,3.201068558));
#98153=CARTESIAN_POINT('',(6.50294674171202,2.75000000026814,3.2053367675602));
#98154=CARTESIAN_POINT('Ctrl Pts',(6.50294674267293,2.75,3.20533676908474));
#98155=CARTESIAN_POINT('Ctrl Pts',(6.40598069,2.785926731,3.402060249));
#98156=CARTESIAN_POINT('Ctrl Pts',(6.297300509,2.821428571,3.592562637));
#98157=CARTESIAN_POINT('Ctrl Pts',(6.2100661683652,2.8499248397502,3.74547322388404));
#98158=CARTESIAN_POINT('Ctrl Pts',(6.11551309476877,2.87870320492457,3.89396966791537));
#98159=CARTESIAN_POINT('Ctrl Pts',(6.72689107244661,2.78894740126306,3.31646445774121));
#98160=CARTESIAN_POINT('Ctrl Pts',(6.68957747469991,2.78276651961456,3.29783179824251));
#98161=CARTESIAN_POINT('Ctrl Pts',(6.65224119222599,2.77643542866125,3.27924260987598));
#98162=CARTESIAN_POINT('Ctrl Pts',(6.57760775536984,2.76346377180691,3.2422035959284));
#98163=CARTESIAN_POINT('Ctrl Pts',(6.54026619878664,2.75681548744809,3.22373172855374));
#98164=CARTESIAN_POINT('Ctrl Pts',(6.50294674040865,2.75000000137438,3.2053367697946));
#98165=CARTESIAN_POINT('Ctrl Pts',(6.612546483,2.749235821,3.538958747));
#98166=CARTESIAN_POINT('Ctrl Pts',(6.804308854,2.813580595,3.180650644));
#98167=CARTESIAN_POINT('Ctrl Pts',(6.956231483,2.878703203,2.803719592));
#98168=CARTESIAN_POINT('Ctrl Pts',(6.500882762,2.749235821,3.209520729));
#98169=CARTESIAN_POINT('Ctrl Pts',(6.674794172,2.813580595,2.857263248));
#98170=CARTESIAN_POINT('Ctrl Pts',(6.809624158,2.878703203,2.488276275));
#98171=CARTESIAN_POINT('Origin',(-0.187763342433521,2.94638886487291,-0.0566049644485317));
#98172=CARTESIAN_POINT('Ctrl Pts',(7.122493615628,2.88000589655946,2.34950051031494));
#98173=CARTESIAN_POINT('Ctrl Pts',(7.123780545314,2.87935454977973,2.34558473015747));
#98174=CARTESIAN_POINT('Ctrl Pts',(7.125067475,2.878703203,2.34166895));
#98175=CARTESIAN_POINT('Ctrl Pts',(7.181927708,2.84992484,2.168658587));
#98176=CARTESIAN_POINT('Ctrl Pts',(7.230323831,2.821428571,1.993092396));
#98177=CARTESIAN_POINT('Ctrl Pts',(7.291272322,2.785541304,1.77199009));
#98178=CARTESIAN_POINT('Ctrl Pts',(7.338597007,2.7492206,1.547576804));
#98179=CARTESIAN_POINT('Ctrl Pts',(6.80688915428054,2.88000589655946,2.49576111393228));
#98180=CARTESIAN_POINT('Ctrl Pts',(6.80825665614027,2.87935454977973,2.49201869446614));
#98181=CARTESIAN_POINT('Ctrl Pts',(6.809624158,2.878703203,2.488276275));
#98182=CARTESIAN_POINT('Ctrl Pts',(6.87004430000001,2.84992484,2.322925483));
#98183=CARTESIAN_POINT('Ctrl Pts',(6.922367894,2.821428571,2.154837056));
#98184=CARTESIAN_POINT('Ctrl Pts',(6.988262514,2.785541304,1.943151999));
#98185=CARTESIAN_POINT('Ctrl Pts',(7.041099506,2.7492206,1.727836146));
#98186=CARTESIAN_POINT('',(7.03996411640098,2.75000000026578,1.73245645140282));
#98187=CARTESIAN_POINT('Ctrl Pts',(7.03996411761487,2.75,1.73245645286228));
#98188=CARTESIAN_POINT('Ctrl Pts',(6.987554811,2.785926731,1.945425482));
#98189=CARTESIAN_POINT('Ctrl Pts',(6.922367894,2.821428571,2.154837056));
#98190=CARTESIAN_POINT('Ctrl Pts',(6.87004429936856,2.84992483969281,2.32292548252339));
#98191=CARTESIAN_POINT('Ctrl Pts',(6.80962417063931,2.87870320490785,2.48827627862319));
#98192=CARTESIAN_POINT('Ctrl Pts',(7.28256192157162,2.78894740128486,1.79284462688592));
#98193=CARTESIAN_POINT('Ctrl Pts',(7.24211600089717,2.78276663836325,1.78266910448061));
#98194=CARTESIAN_POINT('Ctrl Pts',(7.20165608093829,2.77643548706781,1.77254061309088));
#98195=CARTESIAN_POINT('Ctrl Pts',(7.12080487551314,2.76346377184109,1.75241144266078));
#98196=CARTESIAN_POINT('Ctrl Pts',(7.0803654380908,2.75681548742949,1.74239876794969));
#98197=CARTESIAN_POINT('Ctrl Pts',(7.03996411571497,2.7500000013588,1.73245645344123));
#98198=CARTESIAN_POINT('Ctrl Pts',(7.21872034,2.749235821,2.03471783));
#98199=CARTESIAN_POINT('Ctrl Pts',(7.328973763,2.813580595,1.64356353));
#98200=CARTESIAN_POINT('Ctrl Pts',(7.396315492,2.878703203,1.242786042));
#98201=CARTESIAN_POINT('Ctrl Pts',(7.03884782,2.749235821,1.736986289));
#98202=CARTESIAN_POINT('Ctrl Pts',(7.132968332,2.813580595,1.35557858));
#98203=CARTESIAN_POINT('Ctrl Pts',(7.185324776,2.878703203,0.966233856));
#98204=CARTESIAN_POINT('Origin',(-0.19554187319157,2.94638884092586,-0.0149179997582567));
#98205=CARTESIAN_POINT('Ctrl Pts',(7.46104683197357,2.88000589655946,0.763444906506437));
#98206=CARTESIAN_POINT('Ctrl Pts',(7.46146189698679,2.87935454977973,0.759344023253219));
#98207=CARTESIAN_POINT('Ctrl Pts',(7.461876962,2.878703203,0.75524314));
#98208=CARTESIAN_POINT('Ctrl Pts',(7.480215721,2.84992484,0.574054393));
#98209=CARTESIAN_POINT('Ctrl Pts',(7.489738828,2.821428571,0.392189107));
#98210=CARTESIAN_POINT('Ctrl Pts',(7.501731916,2.785541304,0.163153925));
#98211=CARTESIAN_POINT('Ctrl Pts',(7.499707954,2.7492206,-0.066186111));
#98212=CARTESIAN_POINT('Ctrl Pts',(7.18426273431808,2.88000589655946,0.974131648515827));
#98213=CARTESIAN_POINT('Ctrl Pts',(7.18479375515905,2.87935454977973,0.970182752257913));
#98214=CARTESIAN_POINT('Ctrl Pts',(7.185324776,2.878703203,0.966233856));
#98215=CARTESIAN_POINT('Ctrl Pts',(7.208786795,2.84992484,0.791760329));
#98216=CARTESIAN_POINT('Ctrl Pts',(7.22375305,2.821428571,0.616353689));
#98217=CARTESIAN_POINT('Ctrl Pts',(7.242601061,2.785541304,0.395452316));
#98218=CARTESIAN_POINT('Ctrl Pts',(7.247916209,2.7492206,0.173812037));
#98219=CARTESIAN_POINT('',(7.24780059356986,2.75000000025782,0.178568397596697));
#98220=CARTESIAN_POINT('Ctrl Pts',(7.24780059505537,2.75,0.178568398956853));
#98221=CARTESIAN_POINT('Ctrl Pts',(7.242398635,2.785926731,0.397824782));
#98222=CARTESIAN_POINT('Ctrl Pts',(7.22375305,2.821428571,0.616353689));
#98223=CARTESIAN_POINT('Ctrl Pts',(7.20878679508297,2.84992483970705,0.791760328629913));
#98224=CARTESIAN_POINT('Ctrl Pts',(7.18532478887201,2.87870320490792,0.96623385656718));
#98225=CARTESIAN_POINT('Ctrl Pts',(7.49770826955606,2.78894740128533,0.185393373255829));
#98226=CARTESIAN_POINT('Ctrl Pts',(7.45601972509689,2.78276652118434,0.184150402711579));
#98227=CARTESIAN_POINT('Ctrl Pts',(7.41432882982761,2.776435429465,0.182956410174987));
#98228=CARTESIAN_POINT('Ctrl Pts',(7.33104107382006,2.76346377183417,0.180678478153404));
#98229=CARTESIAN_POINT('Ctrl Pts',(7.28939465918434,2.75681548747345,0.179593178041244));
#98230=CARTESIAN_POINT('Ctrl Pts',(7.24780059333909,2.75000000138697,0.17856839945361));
#98231=CARTESIAN_POINT('Ctrl Pts',(7.48735485800001,2.749235821,0.435335768));
#98232=CARTESIAN_POINT('Ctrl Pts',(7.510944005,2.813580595,0.029625212));
#98233=CARTESIAN_POINT('Ctrl Pts',(7.490556008,2.878703203,-0.376258802));
#98234=CARTESIAN_POINT('Ctrl Pts',(7.247684177,2.749235821,0.183232301));
#98235=CARTESIAN_POINT('Ctrl Pts',(7.25761282,2.813580595,-0.209491436));
#98236=CARTESIAN_POINT('Ctrl Pts',(7.22504759300001,2.878703203,-0.600988584999999));
#98237=CARTESIAN_POINT('Origin',(-0.194177019746913,2.94638878624266,0.0274664884888842));
#98238=CARTESIAN_POINT('Ctrl Pts',(7.4507297913676,2.88000589655946,-0.858308532813974));
#98239=CARTESIAN_POINT('Ctrl Pts',(7.4502535836838,2.87935454977973,-0.862402766406987));
#98240=CARTESIAN_POINT('Ctrl Pts',(7.449777376,2.878703203,-0.866497000000001));
#98241=CARTESIAN_POINT('Ctrl Pts',(7.428737159,2.84992484,-1.047391946));
#98242=CARTESIAN_POINT('Ctrl Pts',(7.398941961,2.821428571,-1.227052509));
#98243=CARTESIAN_POINT('Ctrl Pts',(7.361418864,2.785541304,-1.453311135));
#98244=CARTESIAN_POINT('Ctrl Pts',(7.310140893,2.7492206,-1.676854237));
#98245=CARTESIAN_POINT('Ctrl Pts',(7.22570817320211,2.88000589655946,-0.59304713093671));
#98246=CARTESIAN_POINT('Ctrl Pts',(7.22537788310106,2.87935454977973,-0.597017857968355));
#98247=CARTESIAN_POINT('Ctrl Pts',(7.22504759300001,2.878703203,-0.600988585));
#98248=CARTESIAN_POINT('Ctrl Pts',(7.210454432,2.84992484,-0.776426658));
#98249=CARTESIAN_POINT('Ctrl Pts',(7.187363542,2.821428571,-0.95094969));
#98250=CARTESIAN_POINT('Ctrl Pts',(7.158283632,2.785541304,-1.170738277));
#98251=CARTESIAN_POINT('Ctrl Pts',(7.115828406,2.7492206,-1.38833933));
#98252=CARTESIAN_POINT('',(7.11673797040537,2.75000000043277,-1.38366931702854));
#98253=CARTESIAN_POINT('Ctrl Pts',(7.1167379718967,2.75000000141664,-1.38366931622182));
#98254=CARTESIAN_POINT('Ctrl Pts',(7.14471280398305,2.77401081869193,-1.23978407374445));
#98255=CARTESIAN_POINT('Ctrl Pts',(7.16825029397474,2.79784107588195,-1.09540934537186));
#98256=CARTESIAN_POINT('Ctrl Pts',(7.18736354220351,2.82142857104559,-0.950949689938156));
#98257=CARTESIAN_POINT('Ctrl Pts',(7.20271546736448,2.84037424985117,-0.834918454286328));
#98258=CARTESIAN_POINT('Ctrl Pts',(7.21529795469166,2.85947647450026,-0.718198182562453));
#98259=CARTESIAN_POINT('Ctrl Pts',(7.22504760539514,2.8787032049138,-0.600988586830895));
#98260=CARTESIAN_POINT('Ctrl Pts',(7.36227011198848,2.78894740127213,-1.43072666782516));
#98261=CARTESIAN_POINT('Ctrl Pts',(7.32128900964024,2.7827665194972,-1.42297877156182));
#98262=CARTESIAN_POINT('Ctrl Pts',(7.28031615707141,2.77643542860496,-1.41518254022359));
#98263=CARTESIAN_POINT('Ctrl Pts',(7.19848593954923,2.76346377177154,-1.39950281104338));
#98264=CARTESIAN_POINT('Ctrl Pts',(7.15757988751625,2.75681548741898,-1.39160998951429));
#98265=CARTESIAN_POINT('Ctrl Pts',(7.11673797065868,2.75000000134449,-1.38366931494318));
#98266=CARTESIAN_POINT('Ctrl Pts',(7.40588898400001,2.749235821,-1.18440211));
#98267=CARTESIAN_POINT('Ctrl Pts',(7.341710853,2.813580595,-1.585698348));
#98268=CARTESIAN_POINT('Ctrl Pts',(7.234546451,2.878703203,-1.977710203));
#98269=CARTESIAN_POINT('Ctrl Pts',(7.117626877,2.749235821,-1.379089427));
#98270=CARTESIAN_POINT('Ctrl Pts',(7.042899399,2.813580595,-1.764765866));
#98271=CARTESIAN_POINT('Ctrl Pts',(6.926935215,2.878703203,-2.140109468));
#98272=CARTESIAN_POINT('Origin',(-0.183732929338554,2.94638880069341,0.0685666915785357));
#98273=CARTESIAN_POINT('Ctrl Pts',(7.09202490579439,2.88000589655946,-2.43992841977617));
#98274=CARTESIAN_POINT('Ctrl Pts',(7.0906796923972,2.87935454977973,-2.44382456188808));
#98275=CARTESIAN_POINT('Ctrl Pts',(7.089334479,2.878703203,-2.447720704));
#98276=CARTESIAN_POINT('Ctrl Pts',(7.029899105,2.84992484,-2.619863402));
#98277=CARTESIAN_POINT('Ctrl Pts',(6.962178791,2.821428571,-2.788918514));
#98278=CARTESIAN_POINT('Ctrl Pts',(6.876894047,2.785541304,-3.001820982));
#98279=CARTESIAN_POINT('Ctrl Pts',(6.778759767,2.7492206,-3.209114522));
#98280=CARTESIAN_POINT('Ctrl Pts',(6.92928752908958,2.88000589655946,-2.13249568594101));
#98281=CARTESIAN_POINT('Ctrl Pts',(6.92811137204479,2.87935454977973,-2.13630257697051));
#98282=CARTESIAN_POINT('Ctrl Pts',(6.926935215,2.878703203,-2.140109468));
#98283=CARTESIAN_POINT('Ctrl Pts',(6.874969234,2.84992484,-2.308308798));
#98284=CARTESIAN_POINT('Ctrl Pts',(6.814900903,2.821428571,-2.47378772));
#98285=CARTESIAN_POINT('Ctrl Pts',(6.73925281500001,2.785541304,-2.68218645));
#98286=CARTESIAN_POINT('Ctrl Pts',(6.651012375,2.7492206,-2.885573493));
#98287=CARTESIAN_POINT('',(6.65290458904496,2.75000000047527,-2.88120819072644));
#98288=CARTESIAN_POINT('Ctrl Pts',(6.65290459080522,2.75000000185147,-2.88120818990272));
#98289=CARTESIAN_POINT('Ctrl Pts',(6.740065271,2.785926731,-2.679948262));
#98290=CARTESIAN_POINT('Ctrl Pts',(6.814900903,2.821428571,-2.47378772));
#98291=CARTESIAN_POINT('Ctrl Pts',(6.87496923456513,2.84992483975882,-2.3083087984779));
#98292=CARTESIAN_POINT('Ctrl Pts',(6.92693522677083,2.8787032050476,-2.14010947208691));
#98293=CARTESIAN_POINT('Ctrl Pts',(6.88258038601945,2.78894740126168,-2.97994752053213));
#98294=CARTESIAN_POINT('Ctrl Pts',(6.84422299668878,2.78276652415432,-2.96357105245644));
#98295=CARTESIAN_POINT('Ctrl Pts',(6.80588401050304,2.77643543089794,-2.94714913391392));
#98296=CARTESIAN_POINT('Ctrl Pts',(6.72933760291006,2.76346377181668,-2.91424490424444));
#98297=CARTESIAN_POINT('Ctrl Pts',(6.69108463461263,2.75681548741193,-2.89774302018045));
#98298=CARTESIAN_POINT('Ctrl Pts',(6.65290458957586,2.75000000137046,-2.88120818913158));
#98299=CARTESIAN_POINT('Ctrl Pts',(6.978131972,2.749235821,-2.748758662));
#98300=CARTESIAN_POINT('Ctrl Pts',(6.829187461,2.813580595,-3.126876416));
#98301=CARTESIAN_POINT('Ctrl Pts',(6.640257542,2.878703203,-3.486686073));
#98302=CARTESIAN_POINT('Ctrl Pts',(6.654757254,2.749235821,-2.876926465));
#98303=CARTESIAN_POINT('Ctrl Pts',(6.49886783,2.813580595,-3.237521805));
#98304=CARTESIAN_POINT('Ctrl Pts',(6.304927044,2.878703203,-3.57916121));
#98305=CARTESIAN_POINT('Origin',(-0.164697410767518,2.94638883839802,0.106460730702383));
#98306=CARTESIAN_POINT('Ctrl Pts',(6.40170481785586,2.88000589655946,-3.90745996532277));
#98307=CARTESIAN_POINT('Ctrl Pts',(6.39955349942792,2.87935454977973,-3.91097583666138));
#98308=CARTESIAN_POINT('Ctrl Pts',(6.397402181,2.878703203,-3.914491708));
#98309=CARTESIAN_POINT('Ctrl Pts',(6.302350782,2.84992484,-4.069832956));
#98310=CARTESIAN_POINT('Ctrl Pts',(6.199871879,2.821428571,-4.220377789));
#98311=CARTESIAN_POINT('Ctrl Pts',(6.070813308,2.785541304,-4.409969017));
#98312=CARTESIAN_POINT('Ctrl Pts',(5.93041137,2.7492206,-4.591320179));
#98313=CARTESIAN_POINT('Ctrl Pts',(6.30886110036269,2.88000589655946,-3.5722311118992));
#98314=CARTESIAN_POINT('Ctrl Pts',(6.30689407218134,2.87935454977973,-3.5756961609496));
#98315=CARTESIAN_POINT('Ctrl Pts',(6.304927044,2.878703203,-3.57916121));
#98316=CARTESIAN_POINT('Ctrl Pts',(6.218018115,2.84992484,-3.732256984));
#98317=CARTESIAN_POINT('Ctrl Pts',(6.123781072,2.821428571,-3.880954185));
#98318=CARTESIAN_POINT('Ctrl Pts',(6.005102028,2.785541304,-4.068218566));
#98319=CARTESIAN_POINT('Ctrl Pts',(5.875202398,2.7492206,-4.247881446));
#98320=CARTESIAN_POINT('',(5.87798878412016,2.7500000002675,-4.24402497383028));
#98321=CARTESIAN_POINT('Ctrl Pts',(5.87798878596976,2.74999999999996,-4.24402497389632));
#98322=CARTESIAN_POINT('Ctrl Pts',(6.006376632,2.785926731,-4.06620736));
#98323=CARTESIAN_POINT('Ctrl Pts',(6.123781072,2.821428571,-3.880954185));
#98324=CARTESIAN_POINT('Ctrl Pts',(6.21801811524083,2.84992483970532,-3.73225698449517));
#98325=CARTESIAN_POINT('Ctrl Pts',(6.30492705467579,2.8787032050476,-3.57916121655526));
#98326=CARTESIAN_POINT('Ctrl Pts',(6.08106885136325,2.78894740129956,-4.38982933917005));
#98327=CARTESIAN_POINT('Ctrl Pts',(6.04712868686565,2.78276652304603,-4.36559003441779));
#98328=CARTESIAN_POINT('Ctrl Pts',(6.01321627542074,2.77643543037613,-4.34131030485512));
#98329=CARTESIAN_POINT('Ctrl Pts',(5.94553291982872,2.76346377180304,-4.29272014485417));
#98330=CARTESIAN_POINT('Ctrl Pts',(5.91172170255795,2.75681548751259,-4.26838080876083));
#98331=CARTESIAN_POINT('Ctrl Pts',(5.8779887853427,2.75000000141989,-4.24402497181459));
#98332=CARTESIAN_POINT('Ctrl Pts',(6.224085265,2.749235821,-4.184586314));
#98333=CARTESIAN_POINT('Ctrl Pts',(5.997338854,2.813580595,-4.521845218));
#98334=CARTESIAN_POINT('Ctrl Pts',(5.735477571,2.878703203,-4.832628377));
#98335=CARTESIAN_POINT('Ctrl Pts',(5.88071857899999,2.749235821,-4.24024162));
#98336=CARTESIAN_POINT('Ctrl Pts',(5.650956424,2.813580595,-4.558894822));
#98337=CARTESIAN_POINT('Ctrl Pts',(5.388107493,2.878703203,-4.850855352));
#98338=CARTESIAN_POINT('Origin',(-0.137961245383964,2.94638883689837,0.139377039713766));
#98339=CARTESIAN_POINT('Ctrl Pts',(5.41204812843507,2.88000589655946,-5.19228302529162));
#98340=CARTESIAN_POINT('Ctrl Pts',(5.40919129821753,2.87935454977973,-5.19525422764581));
#98341=CARTESIAN_POINT('Ctrl Pts',(5.406334468,2.878703203,-5.19822543));
#98342=CARTESIAN_POINT('Ctrl Pts',(5.280111541,2.84992484,-5.329501645));
#98343=CARTESIAN_POINT('Ctrl Pts',(5.147665849,2.821428571,-5.454496888));
#98344=CARTESIAN_POINT('Ctrl Pts',(4.980868086,2.785541304,-5.611911801));
#98345=CARTESIAN_POINT('Ctrl Pts',(4.80476352700001,2.7492206,-5.758840808));
#98346=CARTESIAN_POINT('Ctrl Pts',(5.3934393395294,2.88000589655946,-4.84493298157681));
#98347=CARTESIAN_POINT('Ctrl Pts',(5.3907734162647,2.87935454977973,-4.8478941667884));
#98348=CARTESIAN_POINT('Ctrl Pts',(5.388107493,2.878703203,-4.850855352));
#98349=CARTESIAN_POINT('Ctrl Pts',(5.270319381,2.84992484,-4.981688981));
#98350=CARTESIAN_POINT('Ctrl Pts',(5.146320044,2.821428571,-5.106651545));
#98351=CARTESIAN_POINT('Ctrl Pts',(4.990159343,2.785541304,-5.264025303));
#98352=CARTESIAN_POINT('Ctrl Pts',(4.82467448700001,2.7492206,-5.411563184));
#98353=CARTESIAN_POINT('',(4.82822475600757,2.75000000027563,-5.40839586469098));
#98354=CARTESIAN_POINT('Ctrl Pts',(4.82822475768938,2.74999999999996,-5.40839586525515));
#98355=CARTESIAN_POINT('Ctrl Pts',(4.991836498,2.785926731,-5.26233512));
#98356=CARTESIAN_POINT('Ctrl Pts',(5.146320044,2.821428571,-5.106651545));
#98357=CARTESIAN_POINT('Ctrl Pts',(5.27031938038601,2.84992483973463,-4.98168898130263));
#98358=CARTESIAN_POINT('Ctrl Pts',(5.38810750192403,2.87870320504759,-4.8508553615638));
#98359=CARTESIAN_POINT('Ctrl Pts',(4.9952132955519,2.78894740128604,-5.5944476161405));
#98360=CARTESIAN_POINT('Ctrl Pts',(4.96727788840992,2.78276663837147,-5.56347945870876));
#98361=CARTESIAN_POINT('Ctrl Pts',(4.93937747636574,2.77643548707661,-5.53247690297568));
#98362=CARTESIAN_POINT('Ctrl Pts',(4.8837217249102,2.76346377181458,-5.47047256236194));
#98363=CARTESIAN_POINT('Ctrl Pts',(4.85593323279021,2.75681548746043,-5.43943385396049));
#98364=CARTESIAN_POINT('Ctrl Pts',(4.82822475775813,2.75000000134421,-5.40839586289356));
#98365=CARTESIAN_POINT('Ctrl Pts',(5.179007248,2.749235821,-5.42474736));
#98366=CARTESIAN_POINT('Ctrl Pts',(4.88506134700001,2.813580595,-5.705377563));
#98367=CARTESIAN_POINT('Ctrl Pts',(4.562513043,2.878703203,-5.952602349));
#98368=CARTESIAN_POINT('Ctrl Pts',(4.83170403900001,2.749235821,-5.405287789));
#98369=CARTESIAN_POINT('Ctrl Pts',(4.538812577,2.813580595,-5.667098985));
#98370=CARTESIAN_POINT('Ctrl Pts',(4.219346023,2.878703203,-5.895728889));
#98371=CARTESIAN_POINT('Origin',(-0.104773817285174,2.94638886113406,0.165776052385654));
#98372=CARTESIAN_POINT('Ctrl Pts',(4.16933008259264,2.88000589655946,-6.23432070250419));
#98373=CARTESIAN_POINT('Ctrl Pts',(4.16590132279632,2.87935454977973,-6.23660830575209));
#98374=CARTESIAN_POINT('Ctrl Pts',(4.162472563,2.878703203,-6.238895909));
#98375=CARTESIAN_POINT('Ctrl Pts',(4.010980152,2.84992484,-6.339968761));
#98376=CARTESIAN_POINT('Ctrl Pts',(3.854760685,2.821428571,-6.433569776));
#98377=CARTESIAN_POINT('Ctrl Pts',(3.658023008,2.785541304,-6.551447827));
#98378=CARTESIAN_POINT('Ctrl Pts',(3.454450283,2.7492206,-6.65708444));
#98379=CARTESIAN_POINT('Ctrl Pts',(4.2258263484876,2.88000589655946,-5.89109116970949));
#98380=CARTESIAN_POINT('Ctrl Pts',(4.2225861857438,2.87935454977973,-5.89341002935475));
#98381=CARTESIAN_POINT('Ctrl Pts',(4.219346023,2.878703203,-5.895728889));
#98382=CARTESIAN_POINT('Ctrl Pts',(4.076186369,2.84992484,-5.998182738));
#98383=CARTESIAN_POINT('Ctrl Pts',(3.928222811,2.821428571,-6.093567555));
#98384=CARTESIAN_POINT('Ctrl Pts',(3.741882354,2.785541304,-6.213692068));
#98385=CARTESIAN_POINT('Ctrl Pts',(3.548550158,2.7492206,-6.322206243));
#98386=CARTESIAN_POINT('',(3.55269830451331,2.75000000024693,-6.31987617435455));
#98387=CARTESIAN_POINT('Ctrl Pts',(3.55269830625484,2.75000000016345,-6.31987617483064));
#98388=CARTESIAN_POINT('Ctrl Pts',(3.743883638,2.785926731,-6.212401939));
#98389=CARTESIAN_POINT('Ctrl Pts',(3.928222811,2.821428571,-6.093567555));
#98390=CARTESIAN_POINT('Ctrl Pts',(4.0761863682735,2.84992483973599,-5.998182738085));
#98391=CARTESIAN_POINT('Ctrl Pts',(4.21934602997973,2.8787032050476,-5.89572889991465));
#98392=CARTESIAN_POINT('Ctrl Pts',(3.67578711801594,2.78894740127026,-6.53747574106815));
#98393=CARTESIAN_POINT('Ctrl Pts',(3.6551616581691,2.78276651685819,-6.50122560259924));
#98394=CARTESIAN_POINT('Ctrl Pts',(3.63457839151704,2.77643542724564,-6.46495048364397));
#98395=CARTESIAN_POINT('Ctrl Pts',(3.59355312984129,2.76346377175075,-6.39243176256808));
#98396=CARTESIAN_POINT('Ctrl Pts',(3.57308672133439,2.7568154872162,-6.35614501636298));
#98397=CARTESIAN_POINT('Ctrl Pts',(3.55269830576612,2.75000000121139,-6.31987617346905));
#98398=CARTESIAN_POINT('Ctrl Pts',(3.891764609,2.749235821,-6.41125325));
#98399=CARTESIAN_POINT('Ctrl Pts',(3.544363801,2.813580595,-6.622132794));
#98400=CARTESIAN_POINT('Ctrl Pts',(3.176210476,2.878703203,-6.794239252));
#98401=CARTESIAN_POINT('Ctrl Pts',(3.556764388,2.749235821,-6.317588708));
#98402=CARTESIAN_POINT('Ctrl Pts',(3.214438897,2.813580595,-6.510315898));
#98403=CARTESIAN_POINT('Ctrl Pts',(2.853292624,2.878703203,-6.664924696));
#98404=CARTESIAN_POINT('Origin',(-0.0666871484641607,2.94638884487929,0.184423190316368));
#98405=CARTESIAN_POINT('Ctrl Pts',(2.7316587967451,2.88000589655946,-6.98484847227732));
#98406=CARTESIAN_POINT('Ctrl Pts',(2.72781843237254,2.87935454977973,-6.98634551063867));
#98407=CARTESIAN_POINT('Ctrl Pts',(2.723978068,2.878703203,-6.987842549));
#98408=CARTESIAN_POINT('Ctrl Pts',(2.55429979,2.84992484,-7.053985984));
#98409=CARTESIAN_POINT('Ctrl Pts',(2.381611195,2.821428571,-7.111816091));
#98410=CARTESIAN_POINT('Ctrl Pts',(2.164132839,2.785541304,-7.18464543300001));
#98411=CARTESIAN_POINT('Ctrl Pts',(1.942610782,2.7492206,-7.244050203));
#98412=CARTESIAN_POINT('Ctrl Pts',(2.86061841568769,2.88000589655946,-6.66178848243677));
#98413=CARTESIAN_POINT('Ctrl Pts',(2.85695551984384,2.87935454977973,-6.66335658921838));
#98414=CARTESIAN_POINT('Ctrl Pts',(2.853292624,2.878703203,-6.664924696));
#98415=CARTESIAN_POINT('Ctrl Pts',(2.691455413,2.84992484,-6.734208137));
#98416=CARTESIAN_POINT('Ctrl Pts',(2.526446244,2.821428571,-6.795555119));
#98417=CARTESIAN_POINT('Ctrl Pts',(2.318639105,2.785541304,-6.872813497));
#98418=CARTESIAN_POINT('Ctrl Pts',(2.106499568,2.7492206,-6.937229964));
#98419=CARTESIAN_POINT('',(2.11105162895206,2.75000000045156,-6.93584610146047));
#98420=CARTESIAN_POINT('Ctrl Pts',(2.11105163018686,2.75000000149723,-6.93584610247036));
#98421=CARTESIAN_POINT('Ctrl Pts',(2.25127962185001,2.77401081870091,-6.89316514097695));
#98422=CARTESIAN_POINT('Ctrl Pts',(2.38986159184462,2.79784107586595,-6.8463344557346));
#98423=CARTESIAN_POINT('Ctrl Pts',(2.52644624442886,2.82142857108152,-6.79555511891881));
#98424=CARTESIAN_POINT('Ctrl Pts',(2.63615221022049,2.84037424987091,-6.75476871934872));
#98425=CARTESIAN_POINT('Ctrl Pts',(2.74516971923028,2.85947647446867,-6.71121273845926));
#98426=CARTESIAN_POINT('Ctrl Pts',(2.85329262766578,2.87870320485789,-6.66492470846333));
#98427=CARTESIAN_POINT('Ctrl Pts',(2.18448521924249,2.78894740125615,-7.17481876586772));
#98428=CARTESIAN_POINT('Ctrl Pts',(2.17213469480052,2.78276652450666,-7.13498232068391));
#98429=CARTESIAN_POINT('Ctrl Pts',(2.15983072388931,2.77643543109502,-7.09513047430933));
#98430=CARTESIAN_POINT('Ctrl Pts',(2.1353539846267,2.76346377185901,-7.01548795904971));
#98431=CARTESIAN_POINT('Ctrl Pts',(2.123166647678,2.75681548752113,-6.97564990509851));
#98432=CARTESIAN_POINT('Ctrl Pts',(2.11105163107829,2.75000000147961,-6.93584610063728));
#98433=CARTESIAN_POINT('Ctrl Pts',(2.422547381,2.749235821,-7.097976063));
#98434=CARTESIAN_POINT('Ctrl Pts',(2.037935743,2.813580595,-7.22924445600001));
#98435=CARTESIAN_POINT('Ctrl Pts',(1.641391837,2.878703203,-7.318185078));
#98436=CARTESIAN_POINT('Ctrl Pts',(2.115514388,2.749235821,-6.934486201));
#98437=CARTESIAN_POINT('Ctrl Pts',(1.739761628,2.813580595,-7.049117675));
#98438=CARTESIAN_POINT('Ctrl Pts',(1.353822432,2.878703203,-7.12247603199999));
#98439=CARTESIAN_POINT('Origin',(-0.025482542469567,2.9463888725141,0.194447476129106));
#98440=CARTESIAN_POINT('Ctrl Pts',(1.16625818054415,2.88000589655946,-7.40877249081791));
#98441=CARTESIAN_POINT('Ctrl Pts',(1.16218578277208,2.87935454977973,-7.40940896440895));
#98442=CARTESIAN_POINT('Ctrl Pts',(1.158113385,2.878703203,-7.410045438));
#98443=CARTESIAN_POINT('Ctrl Pts',(0.978183208000001,2.84992484,-7.438166661));
#98444=CARTESIAN_POINT('Ctrl Pts',(0.797100213,2.821428571,-7.45752179));
#98445=CARTESIAN_POINT('Ctrl Pts',(0.569050224,2.785541304,-7.481897005));
#98446=CARTESIAN_POINT('Ctrl Pts',(0.33993696,2.7492206,-7.49229223));
#98447=CARTESIAN_POINT('Ctrl Pts',(1.36165114397053,2.88000589655946,-7.12098797003829));
#98448=CARTESIAN_POINT('Ctrl Pts',(1.35773678798527,2.87935454977973,-7.12173200101915));
#98449=CARTESIAN_POINT('Ctrl Pts',(1.353822432,2.878703203,-7.122476032));
#98450=CARTESIAN_POINT('Ctrl Pts',(1.180874993,2.84992484,-7.15534944800001));
#98451=CARTESIAN_POINT('Ctrl Pts',(1.00653586,2.821428571,-7.179790078));
#98452=CARTESIAN_POINT('Ctrl Pts',(0.786978868000001,2.785541304,-7.210569806));
#98453=CARTESIAN_POINT('Ctrl Pts',(0.5659514,2.7492206,-7.227876522));
#98454=CARTESIAN_POINT('',(0.570694525309022,2.75000000042798,-7.22750357172063));
#98455=CARTESIAN_POINT('Ctrl Pts',(0.570694526447554,2.75000000139598,-7.22750357294847));
#98456=CARTESIAN_POINT('Ctrl Pts',(0.716819210598589,2.77401081875601,-7.21596534234186));
#98457=CARTESIAN_POINT('Ctrl Pts',(0.862228424556655,2.79784107595042,-7.20002055938569));
#98458=CARTESIAN_POINT('Ctrl Pts',(1.00653586005971,2.82142857101764,-7.17979007804883));
#98459=CARTESIAN_POINT('Ctrl Pts',(1.12244483064415,2.84037424974774,-7.16354078149041));
#98460=CARTESIAN_POINT('Ctrl Pts',(1.2382768204656,2.85947647457669,-7.14443865681336));
#98461=CARTESIAN_POINT('Ctrl Pts',(1.35382243337963,2.87870320492291,-7.12247604475633));
#98462=CARTESIAN_POINT('Ctrl Pts',(0.591039220362235,2.78894740131128,-7.47667523973043));
#98463=CARTESIAN_POINT('Ctrl Pts',(0.587541101836393,2.78276652346789,-7.43511514349877));
#98464=CARTESIAN_POINT('Ctrl Pts',(0.584091760165538,2.77643543057668,-7.39355002482526));
#98465=CARTESIAN_POINT('Ctrl Pts',(0.577308060245671,2.76346377183966,-7.31050773528907));
#98466=CARTESIAN_POINT('Ctrl Pts',(0.573969660415607,2.75681548743311,-7.26898115542804));
#98467=CARTESIAN_POINT('Ctrl Pts',(0.570694527575213,2.75000000136005,-7.22750357138854));
#98468=CARTESIAN_POINT('Ctrl Pts',(0.840054531,2.749235821,-7.45280540400001));
#98469=CARTESIAN_POINT('Ctrl Pts',(0.436216075,2.813580595,-7.498324682));
#98470=CARTESIAN_POINT('Ctrl Pts',(0.029823541,2.878703203,-7.499940704));
#98471=CARTESIAN_POINT('Ctrl Pts',(0.575345286,2.749235821,-7.227134827));
#98472=CARTESIAN_POINT('Ctrl Pts',(0.183735038,2.813580595,-7.25831054400001));
#98473=CARTESIAN_POINT('Ctrl Pts',(-0.208950992,2.878703203,-7.246988304));
#98474=CARTESIAN_POINT('Origin',(0.0169136900852243,2.94638889602872,0.195379449224228));
#98475=CARTESIAN_POINT('Ctrl Pts',(-0.453675371239687,2.88000589655946,
-7.48627054085738));
#98476=CARTESIAN_POINT('Ctrl Pts',(-0.457789381619843,2.87935454977973,
-7.48601668892869));
#98477=CARTESIAN_POINT('Ctrl Pts',(-0.461903392,2.878703203,-7.485762837));
#98478=CARTESIAN_POINT('Ctrl Pts',(-0.643672133,2.84992484,-7.474546933));
#98479=CARTESIAN_POINT('Ctrl Pts',(-0.824682289,2.821428571,-7.454522059));
#98480=CARTESIAN_POINT('Ctrl Pts',(-1.052640546,2.785541304,-7.429303388));
#98481=CARTESIAN_POINT('Ctrl Pts',(-1.278631936,2.7492206,-7.390202999));
#98482=CARTESIAN_POINT('Ctrl Pts',(-0.200985421661271,2.88000589655946,
-7.24721797370008));
#98483=CARTESIAN_POINT('Ctrl Pts',(-0.204968206830636,2.87935454977973,
-7.24710313885004));
#98484=CARTESIAN_POINT('Ctrl Pts',(-0.208950992,2.878703203,-7.246988304));
#98485=CARTESIAN_POINT('Ctrl Pts',(-0.384921828,2.84992484,-7.241914572));
#98486=CARTESIAN_POINT('Ctrl Pts',(-0.560439023,2.821428571,-7.228306033));
#98487=CARTESIAN_POINT('Ctrl Pts',(-0.781479626,2.785541304,-7.211167885));
#98488=CARTESIAN_POINT('Ctrl Pts',(-1.001060027,2.7492206,-7.180555607));
#98489=CARTESIAN_POINT('',(-0.996347619664787,2.7500000002595,-7.18121100776154));
#98490=CARTESIAN_POINT('Ctrl Pts',(-0.99634761870574,2.74999999999996,-7.18121100943214));
#98491=CARTESIAN_POINT('Ctrl Pts',(-0.779105665,2.785926731,-7.211351947));
#98492=CARTESIAN_POINT('Ctrl Pts',(-0.560439023,2.821428571,-7.228306033));
#98493=CARTESIAN_POINT('Ctrl Pts',(-0.384921828241024,2.84992483977763,
-7.24191457215127));
#98494=CARTESIAN_POINT('Ctrl Pts',(-0.208950993485686,2.87870320492457,
-7.24698831685028));
#98495=CARTESIAN_POINT('Ctrl Pts',(-1.03004311525275,2.788947401301,-7.42893068891883));
#98496=CARTESIAN_POINT('Ctrl Pts',(-1.02452525383604,2.78276651929034,-7.38759022460058));
#98497=CARTESIAN_POINT('Ctrl Pts',(-1.01895868193285,2.77643542852002,-7.34625538356977));
#98498=CARTESIAN_POINT('Ctrl Pts',(-1.00773214704204,2.76346377185447,-7.26369629468472));
#98499=CARTESIAN_POINT('Ctrl Pts',(-1.00206550982274,2.75681548744204,-7.22242292579477));
#98500=CARTESIAN_POINT('Ctrl Pts',(-0.996347617450642,2.75000000138088,
-7.18121100788328));
#98501=CARTESIAN_POINT('Ctrl Pts',(-0.781718335,2.749235821,-7.45914984700001));
#98502=CARTESIAN_POINT('Ctrl Pts',(-1.185900572,2.813580595,-7.41679158));
#98503=CARTESIAN_POINT('Ctrl Pts',(-1.583139272,2.878703203,-7.33100743700001));
#98504=CARTESIAN_POINT('Ctrl Pts',(-0.991726322,2.749235821,-7.18185066));
#98505=CARTESIAN_POINT('Ctrl Pts',(-1.380882798,2.813580595,-7.128112879));
#98506=CARTESIAN_POINT('Ctrl Pts',(-1.7619541,2.878703203,-7.032639458));
#98507=CARTESIAN_POINT('Origin',(0.0585190337265659,2.94638888514094,0.187175510455847));
#98508=CARTESIAN_POINT('Ctrl Pts',(-2.05239556607029,2.88000589655946,-7.21371890228333));
#98509=CARTESIAN_POINT('Ctrl Pts',(-2.05635882253515,2.87935454977973,-7.21258659464167));
#98510=CARTESIAN_POINT('Ctrl Pts',(-2.060322079,2.878703203,-7.211454287));
#98511=CARTESIAN_POINT('Ctrl Pts',(-2.235430081,2.84992484,-7.161425698));
#98512=CARTESIAN_POINT('Ctrl Pts',(-2.407903564,2.821428571,-7.102957161));
#98513=CARTESIAN_POINT('Ctrl Pts',(-2.625111015,2.785541304,-7.029323802));
#98514=CARTESIAN_POINT('Ctrl Pts',(-2.837413424,2.7492206,-6.94255609));
#98515=CARTESIAN_POINT('Ctrl Pts',(-1.7542241324767,2.88000589655946,-7.03457612031035));
#98516=CARTESIAN_POINT('Ctrl Pts',(-1.75808911623835,2.87935454977973,-7.03360778915517));
#98517=CARTESIAN_POINT('Ctrl Pts',(-1.7619541,2.878703203,-7.032639458));
#98518=CARTESIAN_POINT('Ctrl Pts',(-1.932720133,2.84992484,-6.989855819));
#98519=CARTESIAN_POINT('Ctrl Pts',(-2.1012084,2.821428571,-6.938834431));
#98520=CARTESIAN_POINT('Ctrl Pts',(-2.313397001,2.785541304,-6.874579768));
#98521=CARTESIAN_POINT('Ctrl Pts',(-2.521263,2.7492206,-6.797479892));
#98522=CARTESIAN_POINT('',(-2.51680165745917,2.75000000047524,-6.79913299826488));
#98523=CARTESIAN_POINT('Ctrl Pts',(-2.51680165660779,2.75000000185138,-6.7991329999353));
#98524=CARTESIAN_POINT('Ctrl Pts',(-2.31111811,2.785926731,-6.875269858));
#98525=CARTESIAN_POINT('Ctrl Pts',(-2.1012084,2.821428571,-6.938834431));
#98526=CARTESIAN_POINT('Ctrl Pts',(-1.93272013410292,2.84992483971974,-6.98985581810938));
#98527=CARTESIAN_POINT('Ctrl Pts',(-1.76195410407895,2.87870320490793,-7.03263947015886));
#98528=CARTESIAN_POINT('Ctrl Pts',(-2.60296178012173,2.78894740128928,-7.03381759585592));
#98529=CARTESIAN_POINT('Ctrl Pts',(-2.58868622042987,2.78276663834398,-6.99463058061894));
#98530=CARTESIAN_POINT('Ctrl Pts',(-2.57436387749908,2.77643548705439,-6.95545837171158));
#98531=CARTESIAN_POINT('Ctrl Pts',(-2.54565191949826,2.76346377181111,-6.8772424882146));
#98532=CARTESIAN_POINT('Ctrl Pts',(-2.53124521094672,2.75681548741717,-6.83815222720877));
#98533=CARTESIAN_POINT('Ctrl Pts',(-2.51680165578597,2.75000000137606,-6.79913299872689));
#98534=CARTESIAN_POINT('Ctrl Pts',(-2.366938921,2.749235821,-7.116712734));
#98535=CARTESIAN_POINT('Ctrl Pts',(-2.752565827,2.813580595,-6.98845754600001));
#98536=CARTESIAN_POINT('Ctrl Pts',(-3.122076251,2.878703203,-6.819284411));
#98537=CARTESIAN_POINT('Ctrl Pts',(-2.51242591,2.749235821,-6.800751138));
#98538=CARTESIAN_POINT('Ctrl Pts',(-2.880932089,2.813580595,-6.664612578));
#98539=CARTESIAN_POINT('Ctrl Pts',(-3.232570193,2.878703203,-6.489452207));
#98540=CARTESIAN_POINT('Origin',(0.0973881573878738,2.94638888876476,0.17021974700001));
#98541=CARTESIAN_POINT('Ctrl Pts',(-3.55514802690122,2.88000589655946,-6.60386178482548));
#98542=CARTESIAN_POINT('Ctrl Pts',(-3.55877521195061,2.87935454977973,-6.60190396691274));
#98543=CARTESIAN_POINT('Ctrl Pts',(-3.562402397,2.878703203,-6.599946149));
#98544=CARTESIAN_POINT('Ctrl Pts',(-3.722661803,2.84992484,-6.513444156));
#98545=CARTESIAN_POINT('Ctrl Pts',(-3.878533944,2.821428571,-6.419265881));
#98546=CARTESIAN_POINT('Ctrl Pts',(-4.07483421,2.785541304,-6.300660847));
#98547=CARTESIAN_POINT('Ctrl Pts',(-4.263520614,2.7492206,-6.17028297400001));
#98548=CARTESIAN_POINT('Ctrl Pts',(-3.22543727298635,2.88000589655946,-6.49300530576195));
#98549=CARTESIAN_POINT('Ctrl Pts',(-3.22900373299317,2.87935454977973,-6.49122875638097));
#98550=CARTESIAN_POINT('Ctrl Pts',(-3.232570193,2.878703203,-6.48945220700001));
#98551=CARTESIAN_POINT('Ctrl Pts',(-3.390146593,2.84992484,-6.410959176));
#98552=CARTESIAN_POINT('Ctrl Pts',(-3.543727607,2.821428571,-6.324910643));
#98553=CARTESIAN_POINT('Ctrl Pts',(-3.737142503,2.785541304,-6.216543941));
#98554=CARTESIAN_POINT('Ctrl Pts',(-3.923574516,2.7492206,-6.096561573));
#98555=CARTESIAN_POINT('',(-3.91957284629739,2.75000000039545,-6.09913508692617));
#98556=CARTESIAN_POINT('Ctrl Pts',(-3.91957284582379,2.75000000142008,-6.09913508857399));
#98557=CARTESIAN_POINT('Ctrl Pts',(-3.79626135934077,2.77401081874129,-6.17838047435427));
#98558=CARTESIAN_POINT('Ctrl Pts',(-3.67085272138319,2.79784107591957,-6.25368485012352));
#98559=CARTESIAN_POINT('Ctrl Pts',(-3.54372760682947,2.82142857107553,-6.32491064329474));
#98560=CARTESIAN_POINT('Ctrl Pts',(-3.44161962337708,2.84037424986775,-6.38211981217387));
#98561=CARTESIAN_POINT('Ctrl Pts',(-3.33784646698797,2.85947647448721,-6.43701127592068));
#98562=CARTESIAN_POINT('Ctrl Pts',(-3.23257019957148,2.87870320490967,-6.48945221791298));
#98563=CARTESIAN_POINT('Ctrl Pts',(-4.05416884499283,2.78894740127868,-6.30981100949365));
#98564=CARTESIAN_POINT('Ctrl Pts',(-4.03180299006025,2.78276663833503,-6.27460898818553));
#98565=CARTESIAN_POINT('Ctrl Pts',(-4.00939462848932,2.77643548702787,-6.23943148401241));
#98566=CARTESIAN_POINT('Ctrl Pts',(-3.96453983709971,2.76346377177556,-6.16921646676086));
#98567=CARTESIAN_POINT('Ctrl Pts',(-3.94206669854191,2.75681548733472,-6.13413713072467));
#98568=CARTESIAN_POINT('Ctrl Pts',(-3.91957284478361,2.75000000127954,-6.09913508772685));
#98569=CARTESIAN_POINT('Ctrl Pts',(-3.841484074,2.749235821,-6.441506043));
#98570=CARTESIAN_POINT('Ctrl Pts',(-4.190524162,2.813580595,-6.233351005));
#98571=CARTESIAN_POINT('Ctrl Pts',(-4.515028415,2.878703203,-5.988699225));
#98572=CARTESIAN_POINT('Ctrl Pts',(-3.915647254,2.749235821,-6.10165605200001));
#98573=CARTESIAN_POINT('Ctrl Pts',(-4.246272197,2.813580595,-5.8894824));
#98574=CARTESIAN_POINT('Ctrl Pts',(-4.552034896,2.878703203,-5.642825383));
#98575=CARTESIAN_POINT('Origin',(0.131703323042633,2.94638880656141,0.145304330238902));
#98576=CARTESIAN_POINT('Ctrl Pts',(-4.89166571598322,2.88000589655946,-5.68521542954546));
#98577=CARTESIAN_POINT('Ctrl Pts',(-4.8947872264916,2.87935454977973,-5.68252364677273));
#98578=CARTESIAN_POINT('Ctrl Pts',(-4.897908737,2.878703203,-5.679831864));
#98579=CARTESIAN_POINT('Ctrl Pts',(-5.035825996,2.84992484,-5.560901205));
#98580=CARTESIAN_POINT('Ctrl Pts',(-5.167808388,2.821428571,-5.435416862));
#98581=CARTESIAN_POINT('Ctrl Pts',(-5.334022687,2.785541304,-5.277385994));
#98582=CARTESIAN_POINT('Ctrl Pts',(-5.490270318,2.7492206,-5.109494284));
#98583=CARTESIAN_POINT('Ctrl Pts',(-4.5458325508932,2.88000589655946,-5.64782877921422));
#98584=CARTESIAN_POINT('Ctrl Pts',(-4.54893372344661,2.87935454977973,-5.64532708110711));
#98585=CARTESIAN_POINT('Ctrl Pts',(-4.55203489600001,2.878703203,-5.642825383));
#98586=CARTESIAN_POINT('Ctrl Pts',(-4.689053566,2.84992484,-5.532293208));
#98587=CARTESIAN_POINT('Ctrl Pts',(-4.82054605,2.821428571,-5.415241063));
#98588=CARTESIAN_POINT('Ctrl Pts',(-4.986143376,2.785541304,-5.267829429));
#98589=CARTESIAN_POINT('Ctrl Pts',(-5.14242405,2.7492206,-5.11057481));
#98590=CARTESIAN_POINT('',(-5.13906916740632,2.75000000026844,-5.11394839761507));
#98591=CARTESIAN_POINT('Ctrl Pts',(-5.13906916779104,2.74999999999911,-5.11394839941762));
#98592=CARTESIAN_POINT('Ctrl Pts',(-4.984364872,2.785926731,-5.26941262000001));
#98593=CARTESIAN_POINT('Ctrl Pts',(-4.82054605,2.821428571,-5.415241063));
#98594=CARTESIAN_POINT('Ctrl Pts',(-4.68905356671078,2.84992483968629,-5.53229320762546));
#98595=CARTESIAN_POINT('Ctrl Pts',(-4.55203490458502,2.87870320490793,-5.64282539268874));
#98596=CARTESIAN_POINT('Ctrl Pts',(-5.31580748100935,2.78894740125035,-5.29076467304406));
#98597=CARTESIAN_POINT('Ctrl Pts',(-5.28639655245168,2.7827665162488,-5.26119306918344));
#98598=CARTESIAN_POINT('Ctrl Pts',(-5.25695027077263,2.77643542702018,-5.23165544233194));
#98599=CARTESIAN_POINT('Ctrl Pts',(-5.19805027904343,2.76346377184499,-5.17272474019516));
#98600=CARTESIAN_POINT('Ctrl Pts',(-5.1685615301564,2.75681548751552,-5.14329660039426));
#98601=CARTESIAN_POINT('Ctrl Pts',(-5.13906916559948,2.75000000145262,-5.11394839915577));
#98602=CARTESIAN_POINT('Ctrl Pts',(-5.136405701,2.749235821,-5.465101689));
#98603=CARTESIAN_POINT('Ctrl Pts',(-5.432538246,2.813580595,-5.186779898));
#98604=CARTESIAN_POINT('Ctrl Pts',(-5.696862869,2.878703203,-4.878089119));
#98605=CARTESIAN_POINT('Ctrl Pts',(-5.135777285,2.749235821,-5.11725431000001));
#98606=CARTESIAN_POINT('Ctrl Pts',(-5.413061337,2.813580595,-4.838966571));
#98607=CARTESIAN_POINT('Ctrl Pts',(-5.658651506,2.878703203,-4.532346316));
#98608=CARTESIAN_POINT('Origin',(0.159860395255516,2.94638884086943,0.113594925728563));
#98609=CARTESIAN_POINT('Ctrl Pts',(-5.9994545538008,2.88000589655946,-4.50073471974354));
#98610=CARTESIAN_POINT('Ctrl Pts',(-6.0019244314004,2.87935454977973,-4.49743483687177));
#98611=CARTESIAN_POINT('Ctrl Pts',(-6.004394309,2.878703203,-4.494134954));
#98612=CARTESIAN_POINT('Ctrl Pts',(-6.113520563,2.84992484,-4.348336694));
#98613=CARTESIAN_POINT('Ctrl Pts',(-6.215441855,2.821428571,-4.197413792));
#98614=CARTESIAN_POINT('Ctrl Pts',(-6.343798191,2.785541304,-4.007346437));
#98615=CARTESIAN_POINT('Ctrl Pts',(-6.460301084,2.7492206,-3.80979132));
#98616=CARTESIAN_POINT('Ctrl Pts',(-5.65366975057634,2.88000589655946,-4.53856605649532));
#98617=CARTESIAN_POINT('Ctrl Pts',(-5.65616062828817,2.87935454977973,-4.53545618624766));
#98618=CARTESIAN_POINT('Ctrl Pts',(-5.658651506,2.878703203,-4.532346316));
#98619=CARTESIAN_POINT('Ctrl Pts',(-5.768705605,2.84992484,-4.394943357));
#98620=CARTESIAN_POINT('Ctrl Pts',(-5.871961118,2.821428571,-4.25236083));
#98621=CARTESIAN_POINT('Ctrl Pts',(-6.001997726,2.785541304,-4.072797068));
#98622=CARTESIAN_POINT('Ctrl Pts',(-6.12081955,2.7492206,-3.88562325));
#98623=CARTESIAN_POINT('',(-6.11826832419047,2.75000000024419,-3.88963916514864));
#98624=CARTESIAN_POINT('Ctrl Pts',(-6.11826832477835,2.74999999999996,-3.88963916703005));
#98625=CARTESIAN_POINT('Ctrl Pts',(-6.000601142,2.785926731,-4.074725571));
#98626=CARTESIAN_POINT('Ctrl Pts',(-5.871961118,2.821428571,-4.25236083));
#98627=CARTESIAN_POINT('Ctrl Pts',(-5.76870560553419,2.84992483976829,-4.39494335711938));
#98628=CARTESIAN_POINT('Ctrl Pts',(-5.65865151622557,2.8787032050476,-4.53234632367778));
#98629=CARTESIAN_POINT('Ctrl Pts',(-6.32888486674515,2.78894740126507,-4.02432806087191));
#98630=CARTESIAN_POINT('Ctrl Pts',(-6.29380522164559,2.78276663834483,-4.00177075055515));
#98631=CARTESIAN_POINT('Ctrl Pts',(-6.25869729295988,2.77643548704644,-3.97925353934966));
#98632=CARTESIAN_POINT('Ctrl Pts',(-6.18850566656785,2.76346377182085,-3.93436215385666));
#98633=CARTESIAN_POINT('Ctrl Pts',(-6.15338016783904,2.75681548743132,-3.91196123690154));
#98634=CARTESIAN_POINT('Ctrl Pts',(-6.11826832270252,2.75000000136865,-3.88963916714581));
#98635=CARTESIAN_POINT('Ctrl Pts',(-6.19115470600001,2.749235821,-4.233155254));
#98636=CARTESIAN_POINT('Ctrl Pts',(-6.420532878,2.813580595,-3.897680728));
#98637=CARTESIAN_POINT('Ctrl Pts',(-6.612318346,2.878703203,-3.539384988));
#98638=CARTESIAN_POINT('Ctrl Pts',(-6.115764078,2.749235821,-3.893575445));
#98639=CARTESIAN_POINT('Ctrl Pts',(-6.326741745,2.813580595,-3.562186043));
#98640=CARTESIAN_POINT('Ctrl Pts',(-6.500675861,2.878703203,-3.209939773));
#98641=CARTESIAN_POINT('Origin',(0.180542670106106,2.94638889073077,0.0765739682539879));
#98642=CARTESIAN_POINT('Ctrl Pts',(-6.82671556406542,2.88000589655946,-3.10580465625746));
#98643=CARTESIAN_POINT('Ctrl Pts',(-6.82841832003271,2.87935454977973,-3.10205097212873));
#98644=CARTESIAN_POINT('Ctrl Pts',(-6.830121076,2.878703203,-3.098297288));
#98645=CARTESIAN_POINT('Ctrl Pts',(-6.905353703,2.84992484,-2.932448791));
#98646=CARTESIAN_POINT('Ctrl Pts',(-6.972448169,2.821428571,-2.763144319));
#98647=CARTESIAN_POINT('Ctrl Pts',(-7.056944742,2.785541304,-2.549927814));
#98648=CARTESIAN_POINT('Ctrl Pts',(-7.128255352,2.7492206,-2.331946748));
#98649=CARTESIAN_POINT('Ctrl Pts',(-6.49714763659028,2.88000589655946,-3.21708502956251));
#98650=CARTESIAN_POINT('Ctrl Pts',(-6.49891174879514,2.87935454977973,-3.21351240128125));
#98651=CARTESIAN_POINT('Ctrl Pts',(-6.500675861,2.878703203,-3.209939773));
#98652=CARTESIAN_POINT('Ctrl Pts',(-6.578619382,2.84992484,-3.052090841));
#98653=CARTESIAN_POINT('Ctrl Pts',(-6.64880981,2.821428571,-2.890644931));
#98654=CARTESIAN_POINT('Ctrl Pts',(-6.737205333,2.785541304,-2.687325243));
#98655=CARTESIAN_POINT('Ctrl Pts',(-6.813012331,2.7492206,-2.478984264));
#98656=CARTESIAN_POINT('',(-6.81138405458469,2.75000000026527,-2.48345472752655));
#98657=CARTESIAN_POINT('Ctrl Pts',(-6.81138405566465,2.74999999999996,-2.4834547290353));
#98658=CARTESIAN_POINT('Ctrl Pts',(-6.736255972,2.785926731,-2.689508882));
#98659=CARTESIAN_POINT('Ctrl Pts',(-6.64880981,2.821428571,-2.890644931));
#98660=CARTESIAN_POINT('Ctrl Pts',(-6.57861938257659,2.84992483974429,-3.05209084090307));
#98661=CARTESIAN_POINT('Ctrl Pts',(-6.50067587308103,2.87870320492457,-3.2099397776958));
#98662=CARTESIAN_POINT('Ctrl Pts',(-7.04603063056367,2.78894740127283,-2.56971834113614));
#98663=CARTESIAN_POINT('Ctrl Pts',(-7.00692124906874,2.78276652391527,-2.55522922667437));
#98664=CARTESIAN_POINT('Ctrl Pts',(-6.96779397438999,2.77643543079175,-2.54078576580088));
#98665=CARTESIAN_POINT('Ctrl Pts',(-6.88959340745289,2.76346377181563,-2.51203316538067));
#98666=CARTESIAN_POINT('Ctrl Pts',(-6.850473588529,2.75681548744948,-2.49770691330304));
#98667=CARTESIAN_POINT('Ctrl Pts',(-6.81138405359718,2.75000000138084,-2.48345472970154));
#98668=CARTESIAN_POINT('Ctrl Pts',(-6.956412198,2.749235821,-2.803271184));
#98669=CARTESIAN_POINT('Ctrl Pts',(-7.10831053000001,2.813580595,-2.42633034));
#98670=CARTESIAN_POINT('Ctrl Pts',(-7.218589166,2.878703203,-2.035183148));
#98671=CARTESIAN_POINT('Ctrl Pts',(-6.80978454,2.749235821,-2.487837318));
#98672=CARTESIAN_POINT('Ctrl Pts',(-6.944590741,2.813580595,-2.118841655));
#98673=CARTESIAN_POINT('Ctrl Pts',(-7.038735838,2.878703203,-1.737440013));
#98674=CARTESIAN_POINT('Origin',(0.192782843529136,2.94638888841761,0.035972377766566));
#98675=CARTESIAN_POINT('Ctrl Pts',(-7.33476694232736,2.88000589655946,-1.56565061954801));
#98676=CARTESIAN_POINT('Ctrl Pts',(-7.33562295766368,2.87935454977973,-1.561618652274));
#98677=CARTESIAN_POINT('Ctrl Pts',(-7.336478973,2.878703203,-1.557586685));
#98678=CARTESIAN_POINT('Ctrl Pts',(-7.374300178,2.84992484,-1.379442843));
#98679=CARTESIAN_POINT('Ctrl Pts',(-7.403430556,2.821428571,-1.199673288));
#98680=CARTESIAN_POINT('Ctrl Pts',(-7.4401164,2.785541304,-0.973277401));
#98681=CARTESIAN_POINT('Ctrl Pts',(-7.462900322,2.7492206,-0.745062938000001));
#98682=CARTESIAN_POINT('Ctrl Pts',(-7.03682612043755,2.88000589655946,-1.74517668140246));
#98683=CARTESIAN_POINT('Ctrl Pts',(-7.03778097921877,2.87935454977973,-1.74130834720123));
#98684=CARTESIAN_POINT('Ctrl Pts',(-7.038735838,2.878703203,-1.737440013));
#98685=CARTESIAN_POINT('Ctrl Pts',(-7.080924229,2.84992484,-1.566525948));
#98686=CARTESIAN_POINT('Ctrl Pts',(-7.114767544,2.821428571,-1.393765687));
#98687=CARTESIAN_POINT('Ctrl Pts',(-7.157388707,2.785541304,-1.176197076));
#98688=CARTESIAN_POINT('Ctrl Pts',(-7.186636227,2.7492206,-0.95643073));
#98689=CARTESIAN_POINT('',(-7.18600703588704,2.75000000047524,-0.961146708048971));
#98690=CARTESIAN_POINT('Ctrl Pts',(-7.18600703699163,2.75000000185138,-0.961146709604796));
#98691=CARTESIAN_POINT('Ctrl Pts',(-7.156930959,2.785926731,-1.178533747));
#98692=CARTESIAN_POINT('Ctrl Pts',(-7.114767544,2.821428571,-1.393765687));
#98693=CARTESIAN_POINT('Ctrl Pts',(-7.0809242289375,2.84992483971582,-1.56652594736781));
#98694=CARTESIAN_POINT('Ctrl Pts',(-7.03873585046811,2.87870320490792,-1.73744001534874));
#98695=CARTESIAN_POINT('Ctrl Pts',(-7.43371183284565,2.78894740126349,-0.994951447861542));
#98696=CARTESIAN_POINT('Ctrl Pts',(-7.39240207702832,2.78276652412189,-0.989208442067899));
#98697=CARTESIAN_POINT('Ctrl Pts',(-7.35108465833632,2.77643543088597,-0.983513868720913));
#98698=CARTESIAN_POINT('Ctrl Pts',(-7.26853141724985,2.76346377178727,-0.972244298473256));
#98699=CARTESIAN_POINT('Ctrl Pts',(-7.22724647698605,2.75681548737656,-0.966662590939243));
#98700=CARTESIAN_POINT('Ctrl Pts',(-7.18600703548563,2.75000000130361,-0.961146710026586));
#98701=CARTESIAN_POINT('Ctrl Pts',(-7.396395587,2.749235821,-1.242309269));
#98702=CARTESIAN_POINT('Ctrl Pts',(-7.463711481,2.813580595,-0.841527441));
#98703=CARTESIAN_POINT('Ctrl Pts',(-7.48732678,2.878703203,-0.435818406));
#98704=CARTESIAN_POINT('Ctrl Pts',(-7.185387045,2.749235821,-0.965770684));
#98705=CARTESIAN_POINT('Ctrl Pts',(-7.237718391,2.813580595,-0.576422586));
#98706=CARTESIAN_POINT('Ctrl Pts',(-7.24767235000001,2.878703203,-0.18369949));
#98707=CARTESIAN_POINT('Origin',(0.196008725215265,2.94638886097645,-0.00631123273774178));
#98708=CARTESIAN_POINT('Ctrl Pts',(-7.49985277021764,2.88000589655946,0.0477115007758101));
#98709=CARTESIAN_POINT('Ctrl Pts',(-7.49982201860882,2.87935454977973,0.0518332208879051));
#98710=CARTESIAN_POINT('Ctrl Pts',(-7.499791267,2.878703203,0.055954941));
#98711=CARTESIAN_POINT('Ctrl Pts',(-7.498432573,2.84992484,0.23806432));
#98712=CARTESIAN_POINT('Ctrl Pts',(-7.488236759,2.821428571,0.419893133));
#98713=CARTESIAN_POINT('Ctrl Pts',(-7.475396485,2.785541304,0.648882381));
#98714=CARTESIAN_POINT('Ctrl Pts',(-7.448588368,2.7492206,0.876659187));
#98715=CARTESIAN_POINT('Ctrl Pts',(-7.24747043558839,2.88000589655946,-0.191665812214019));
#98716=CARTESIAN_POINT('Ctrl Pts',(-7.2475713927942,2.87935454977973,-0.187682651107009));
#98717=CARTESIAN_POINT('Ctrl Pts',(-7.24767235,2.878703203,-0.18369949));
#98718=CARTESIAN_POINT('Ctrl Pts',(-7.252132928,2.84992484,-0.007712044));
#98719=CARTESIAN_POINT('Ctrl Pts',(-7.248046656,2.821428571,0.168284491));
#98720=CARTESIAN_POINT('Ctrl Pts',(-7.24290054,2.785541304,0.38992876));
#98721=CARTESIAN_POINT('Ctrl Pts',(-7.224221001,2.7492206,0.610844443));
#98722=CARTESIAN_POINT('',(-7.22462031605779,2.75000000025979,0.606103464216765));
#98723=CARTESIAN_POINT('Ctrl Pts',(-7.22462031767412,2.74999999999996,0.606103463201151));
#98724=CARTESIAN_POINT('Ctrl Pts',(-7.242955809,2.785926731,0.387548315));
#98725=CARTESIAN_POINT('Ctrl Pts',(-7.248046656,2.821428571,0.168284491));
#98726=CARTESIAN_POINT('Ctrl Pts',(-7.25213292811546,2.84992483969163,-0.00771204260381877));
#98727=CARTESIAN_POINT('Ctrl Pts',(-7.24767236317298,2.87870320490793,-0.183699489006381));
#98728=CARTESIAN_POINT('Ctrl Pts',(-7.47380093235172,2.78894740127252,0.626338268970036));
#98729=CARTESIAN_POINT('Ctrl Pts',(-7.43222238196124,2.78276652157547,0.623066628776044));
#98730=CARTESIAN_POINT('Ctrl Pts',(-7.39064678568942,2.77643542964108,0.619746043259463));
#98731=CARTESIAN_POINT('Ctrl Pts',(-7.3076009770964,2.76346377183828,0.613005631471951));
#98732=CARTESIAN_POINT('Ctrl Pts',(-7.26608135367996,2.75681548745084,0.609581800093443));
#98733=CARTESIAN_POINT('Ctrl Pts',(-7.22462031606358,2.75000000139655,0.606103461920369));
#98734=CARTESIAN_POINT('Ctrl Pts',(-7.490531739,2.749235821,0.376741646));
#98735=CARTESIAN_POINT('Ctrl Pts',(-7.47011757900001,2.813580595,0.782624346));
#98736=CARTESIAN_POINT('Ctrl Pts',(-7.40596531600001,2.878703203,1.18392472));
#98737=CARTESIAN_POINT('Ctrl Pts',(-7.225008838,2.749235821,0.601454314));
#98738=CARTESIAN_POINT('Ctrl Pts',(-7.192418375,2.813580595,0.992949363));
#98739=CARTESIAN_POINT('Ctrl Pts',(-7.117715759,2.878703203,1.378630618));
#98740=CARTESIAN_POINT('Origin',(0.190069426067424,2.94638891401156,-0.0482997700442647));
#98741=CARTESIAN_POINT('Ctrl Pts',(-7.31425381724154,2.88000589655946,1.65884268319525));
#98742=CARTESIAN_POINT('Ctrl Pts',(-7.31333773662077,2.87935454977973,1.66286142909763));
#98743=CARTESIAN_POINT('Ctrl Pts',(-7.312421656,2.878703203,1.666880175));
#98744=CARTESIAN_POINT('Ctrl Pts',(-7.271946595,2.84992484,1.844439859));
#98745=CARTESIAN_POINT('Ctrl Pts',(-7.222901333,2.821428571,2.019825817));
#98746=CARTESIAN_POINT('Ctrl Pts',(-7.161135338,2.785541304,2.240701145));
#98747=CARTESIAN_POINT('Ctrl Pts',(-7.085988699,2.7492206,2.457389703));
#98748=CARTESIAN_POINT('Ctrl Pts',(-7.11923108909293,2.88000589655946,1.37080713833006));
#98749=CARTESIAN_POINT('Ctrl Pts',(-7.11847342404647,2.87935454977973,1.37471887816503));
#98750=CARTESIAN_POINT('Ctrl Pts',(-7.117715759,2.878703203,1.378630618));
#98751=CARTESIAN_POINT('Ctrl Pts',(-7.084239951,2.84992484,1.551462468));
#98752=CARTESIAN_POINT('Ctrl Pts',(-7.042415162,2.821428571,1.722465874));
#98753=CARTESIAN_POINT('Ctrl Pts',(-6.989742393,2.785541304,1.937821959));
#98754=CARTESIAN_POINT('Ctrl Pts',(-6.92400923,2.7492206,2.149557208));
#98755=CARTESIAN_POINT('',(-6.92541837970349,2.75000000043858,2.1450129119477));
#98756=CARTESIAN_POINT('Ctrl Pts',(-6.92541838123497,2.75000000140029,2.14501291150036));
#98757=CARTESIAN_POINT('Ctrl Pts',(-6.96878595450075,2.7740108187138,2.00499574194987));
#98758=CARTESIAN_POINT('Ctrl Pts',(-7.00779512042091,2.79784107590582,1.86401219475765));
#98759=CARTESIAN_POINT('Ctrl Pts',(-7.04241516218228,2.82142857108703,1.7224658735676));
#98760=CARTESIAN_POINT('Ctrl Pts',(-7.07022227669528,2.84037424985765,1.60877465310127));
#98761=CARTESIAN_POINT('Ctrl Pts',(-7.09535068652136,2.85947647453636,1.49409900678069));
#98762=CARTESIAN_POINT('Ctrl Pts',(-7.11771577132896,2.87870320488967,1.37863062164941));
#98763=CARTESIAN_POINT('Ctrl Pts',(-7.1644234061344,2.78894740128559,2.21834110489946));
#98764=CARTESIAN_POINT('Ctrl Pts',(-7.12452026293291,2.78276652435089,2.20620779999514));
#98765=CARTESIAN_POINT('Ctrl Pts',(-7.08463049941589,2.77643543102928,2.19402732086459));
#98766=CARTESIAN_POINT('Ctrl Pts',(-7.0049752368222,2.76346377186035,2.16959209955829));
#98767=CARTESIAN_POINT('Ctrl Pts',(-6.96516234191877,2.75681548748643,2.15732282375446));
#98768=CARTESIAN_POINT('Ctrl Pts',(-6.92541838025487,2.75000000140094,2.1450129096347));
#98769=CARTESIAN_POINT('Ctrl Pts',(-7.234418952,2.749235821,1.978176541));
#98770=CARTESIAN_POINT('Ctrl Pts',(-7.127229281,2.813580595,2.370181488));
#98771=CARTESIAN_POINT('Ctrl Pts',(-6.978309144,2.878703203,2.748308842));
#98772=CARTESIAN_POINT('Ctrl Pts',(-6.926797248,2.749235821,2.140555977));
#98773=CARTESIAN_POINT('Ctrl Pts',(-6.810808868,2.813580595,2.515892103));
#98774=CARTESIAN_POINT('Ctrl Pts',(-6.65494268900001,2.878703203,2.87649749));
#98775=CARTESIAN_POINT('Origin',(0.175242662804203,2.94638889345237,-0.0880298495019172));
#98776=CARTESIAN_POINT('Ctrl Pts',(-6.78664848652661,2.88000589655946,3.19240822682198));
#98777=CARTESIAN_POINT('Ctrl Pts',(-6.7848899117633,2.87935454977973,3.19613608641099));
#98778=CARTESIAN_POINT('Ctrl Pts',(-6.783131337,2.878703203,3.199863946));
#98779=CARTESIAN_POINT('Ctrl Pts',(-6.705432476,2.84992484,3.364571441));
#98780=CARTESIAN_POINT('Ctrl Pts',(-6.619831069,2.821428571,3.525313691));
#98781=CARTESIAN_POINT('Ctrl Pts',(-6.512027462,2.785541304,3.727747213));
#98782=CARTESIAN_POINT('Ctrl Pts',(-6.392056075,2.7492206,3.923215407));
#98783=CARTESIAN_POINT('Ctrl Pts',(-6.65810440838206,2.88000589655946,2.86918267012378));
#98784=CARTESIAN_POINT('Ctrl Pts',(-6.65652354869103,2.87935454977973,2.87284008006189));
#98785=CARTESIAN_POINT('Ctrl Pts',(-6.654942689,2.878703203,2.87649749));
#98786=CARTESIAN_POINT('Ctrl Pts',(-6.585095788,2.84992484,3.038092318));
#98787=CARTESIAN_POINT('Ctrl Pts',(-6.507488162,2.821428571,3.196106666));
#98788=CARTESIAN_POINT('Ctrl Pts',(-6.40975166,2.785541304,3.395104758));
#98789=CARTESIAN_POINT('Ctrl Pts',(-6.300038482,2.7492206,3.587759067));
#98790=CARTESIAN_POINT('',(-6.30239157604247,2.75000000044397,3.58362393917865));
#98791=CARTESIAN_POINT('Ctrl Pts',(-6.30239157771542,2.75000000149012,3.58362393887883));
#98792=CARTESIAN_POINT('Ctrl Pts',(-6.37484479418816,2.77401081887672,3.45620303955513));
#98793=CARTESIAN_POINT('Ctrl Pts',(-6.44324924287563,2.79784107603871,3.32690142699863));
#98794=CARTESIAN_POINT('Ctrl Pts',(-6.50748816226137,2.82142857106589,3.19610666587472));
#98795=CARTESIAN_POINT('Ctrl Pts',(-6.55908541327254,2.84037424976114,3.09105119099027));
#98796=CARTESIAN_POINT('Ctrl Pts',(-6.60827820948216,2.85947647458613,2.9844584625883));
#98797=CARTESIAN_POINT('Ctrl Pts',(-6.65494270044249,2.87870320494007,2.87649749609288));
#98798=CARTESIAN_POINT('Ctrl Pts',(-6.52004540446191,2.78894740123703,3.70661677599489));
#98799=CARTESIAN_POINT('Ctrl Pts',(-6.4836834607068,2.78276652164253,3.68618913596105));
#98800=CARTESIAN_POINT('Ctrl Pts',(-6.44734474878675,2.7764354296662,3.66571831425722));
#98801=CARTESIAN_POINT('Ctrl Pts',(-6.37480463932654,2.76346377182802,3.62473085209843));
#98802=CARTESIAN_POINT('Ctrl Pts',(-6.33856007921744,2.75681548745698,3.60418982954241));
#98803=CARTESIAN_POINT('Ctrl Pts',(-6.30239157687467,2.75000000139314,3.58362393740054));
#98804=CARTESIAN_POINT('Ctrl Pts',(-6.640032775,2.749235821,3.4871141));
#98805=CARTESIAN_POINT('Ctrl Pts',(-6.451079663,2.813580595,3.846911578));
#98806=CARTESIAN_POINT('Ctrl Pts',(-6.224354992,2.878703203,4.184185097));
#98807=CARTESIAN_POINT('Ctrl Pts',(-6.304696317,2.749235821,3.579567621));
#98808=CARTESIAN_POINT('Ctrl Pts',(-6.110733509,2.813580595,3.921194524));
#98809=CARTESIAN_POINT('Ctrl Pts',(-5.880991895,2.878703203,4.239862537));
#98810=CARTESIAN_POINT('Origin',(0.152221680070309,2.94638885833933,-0.12364368640523));
#98811=CARTESIAN_POINT('Ctrl Pts',(-5.94170701373572,2.88000589655946,4.57670030852734));
#98812=CARTESIAN_POINT('Ctrl Pts',(-5.93918817386786,2.87935454977973,4.57996297126367));
#98813=CARTESIAN_POINT('Ctrl Pts',(-5.936669334,2.878703203,4.583225634));
#98814=CARTESIAN_POINT('Ctrl Pts',(-5.825379787,2.84992484,4.727379402));
#98815=CARTESIAN_POINT('Ctrl Pts',(-5.707224861,2.821428571,4.865961815));
#98816=CARTESIAN_POINT('Ctrl Pts',(-5.558424419,2.785541304,5.040487965));
#98817=CARTESIAN_POINT('Ctrl Pts',(-5.399238013,2.7492206,5.20559592));
#98818=CARTESIAN_POINT('Ctrl Pts',(-5.88565216516249,2.88000589655946,4.23339840973982));
#98819=CARTESIAN_POINT('Ctrl Pts',(-5.88332203008124,2.87935454977973,4.23663047336991));
#98820=CARTESIAN_POINT('Ctrl Pts',(-5.880991895,2.878703203,4.239862537));
#98821=CARTESIAN_POINT('Ctrl Pts',(-5.778039865,2.84992484,4.382664349));
#98822=CARTESIAN_POINT('Ctrl Pts',(-5.668278248,2.821428571,4.520301063));
#98823=CARTESIAN_POINT('Ctrl Pts',(-5.530048064,2.785541304,4.693636231));
#98824=CARTESIAN_POINT('Ctrl Pts',(-5.38148493800001,2.7492206,4.858201299));
#98825=CARTESIAN_POINT('',(-5.38467194767664,2.75000000042058,4.85466869391466));
#98826=CARTESIAN_POINT('Ctrl Pts',(-5.38467194961098,2.75000000141392,4.85466869376423));
#98827=CARTESIAN_POINT('Ctrl Pts',(-5.48282297663001,2.77401081878987,4.74580212481635));
#98828=CARTESIAN_POINT('Ctrl Pts',(-5.57742419173345,2.79784107597051,4.63422844676064));
#98829=CARTESIAN_POINT('Ctrl Pts',(-5.66827824813469,2.8214285710255,4.52030106320043));
#98830=CARTESIAN_POINT('Ctrl Pts',(-5.74125300605112,2.84037424975707,4.42879361097015));
#98831=CARTESIAN_POINT('Ctrl Pts',(-5.81220998726546,2.85947647451415,4.33526795795914));
#98832=CARTESIAN_POINT('Ctrl Pts',(-5.88099190465141,2.87870320491434,4.23986254478712));
#98833=CARTESIAN_POINT('Ctrl Pts',(-5.57079732597209,2.78894740125962,5.0215751666047));
#98834=CARTESIAN_POINT('Ctrl Pts',(-5.53967685848314,2.78276652471571,4.99380838402595));
#98835=CARTESIAN_POINT('Ctrl Pts',(-5.50858833888163,2.77643543117326,4.96600440247965));
#98836=CARTESIAN_POINT('Ctrl Pts',(-5.44655526262357,2.7634637717922,4.91038121850665));
#98837=CARTESIAN_POINT('Ctrl Pts',(-5.41557379272587,2.75681548734966,4.88252892431589));
#98838=CARTESIAN_POINT('Ctrl Pts',(-5.38467194888147,2.75000000126181,4.8546686923725));
#98839=CARTESIAN_POINT('Ctrl Pts',(-5.73516604600001,2.749235821,4.832998079));
#98840=CARTESIAN_POINT('Ctrl Pts',(-5.47328473,2.813580595,5.143764358));
#98841=CARTESIAN_POINT('Ctrl Pts',(-5.179356919,2.878703203,5.424413508));
#98842=CARTESIAN_POINT('Ctrl Pts',(-5.387794793,2.749235821,4.851202662));
#98843=CARTESIAN_POINT('Ctrl Pts',(-5.124927042,2.813580595,5.143146247));
#98844=CARTESIAN_POINT('Ctrl Pts',(-4.832052457,2.878703203,5.404976323));
#98845=CARTESIAN_POINT('Origin',(0.122083007002124,2.9463888135562,-0.153476030171616));
#98846=CARTESIAN_POINT('Ctrl Pts',(-4.81893792566327,2.88000589655946,5.74699097129102));
#98847=CARTESIAN_POINT('Ctrl Pts',(-4.81577659883164,2.87935454977973,5.74963587864552));
#98848=CARTESIAN_POINT('Ctrl Pts',(-4.812615272,2.878703203,5.752280786));
#98849=CARTESIAN_POINT('Ctrl Pts',(-4.672938814,2.84992484,5.86914035499999));
#98850=CARTESIAN_POINT('Ctrl Pts',(-4.527755162,2.821428571,5.979082973));
#98851=CARTESIAN_POINT('Ctrl Pts',(-4.344915628,2.785541304,6.117541102));
#98852=CARTESIAN_POINT('Ctrl Pts',(-4.153957582,2.7492206,6.244568552));
#98853=CARTESIAN_POINT('Ctrl Pts',(-4.83799336891228,2.88000589655946,5.39966514376146));
#98854=CARTESIAN_POINT('Ctrl Pts',(-4.83502291295614,2.87935454977973,5.40232073338072));
#98855=CARTESIAN_POINT('Ctrl Pts',(-4.832052457,2.878703203,5.404976323));
#98856=CARTESIAN_POINT('Ctrl Pts',(-4.70080922,2.84992484,5.522307865));
#98857=CARTESIAN_POINT('Ctrl Pts',(-4.564025943,2.821428571,5.633131207));
#98858=CARTESIAN_POINT('Ctrl Pts',(-4.391765567,2.785541304,5.772698491));
#98859=CARTESIAN_POINT('Ctrl Pts',(-4.211299138,2.7492206,5.901479439));
#98860=CARTESIAN_POINT('',(-4.21517104353124,2.75000000044712,5.89871453642188));
#98861=CARTESIAN_POINT('Ctrl Pts',(-4.21517104541032,2.75000000162255,5.89871453663159));
#98862=CARTESIAN_POINT('Ctrl Pts',(-4.393615631,2.785926731,5.771199548));
#98863=CARTESIAN_POINT('Ctrl Pts',(-4.564025943,2.821428571,5.633131207));
#98864=CARTESIAN_POINT('Ctrl Pts',(-4.70080921954997,2.8499248397042,5.52230786541046));
#98865=CARTESIAN_POINT('Ctrl Pts',(-4.83205246474551,2.87870320492458,5.4049763335841));
#98866=CARTESIAN_POINT('Ctrl Pts',(-4.36106495617808,2.78894740128769,6.10173028302463));
#98867=CARTESIAN_POINT('Ctrl Pts',(-4.33664107985251,2.78276651828651,6.06792265660883));
#98868=CARTESIAN_POINT('Ctrl Pts',(-4.31225644017267,2.77643542799327,6.03408562264512));
#98869=CARTESIAN_POINT('Ctrl Pts',(-4.26363101483272,2.76346377178398,5.96642761673698));
#98870=CARTESIAN_POINT('Ctrl Pts',(-4.23936129430749,2.75681548734638,5.93256639350245));
#98871=CARTESIAN_POINT('Ctrl Pts',(-4.21517104463714,2.75000000130795,5.8987145354583));
#98872=CARTESIAN_POINT('Ctrl Pts',(-4.562129326,2.749235821,5.952896439));
#98873=CARTESIAN_POINT('Ctrl Pts',(-4.239565086,2.813580595,6.200100433));
#98874=CARTESIAN_POINT('Ctrl Pts',(-3.892177873,2.878703203,6.411002371));
#98875=CARTESIAN_POINT('Ctrl Pts',(-4.218965973,2.749235821,5.896000858));
#98876=CARTESIAN_POINT('Ctrl Pts',(-3.899484683,2.813580595,6.124610169));
#98877=CARTESIAN_POINT('Ctrl Pts',(-3.557171616,2.878703203,6.317359424));
#98878=CARTESIAN_POINT('Origin',(0.0862359136157109,2.94638886271948,-0.176132018933817));
#98879=CARTESIAN_POINT('Ctrl Pts',(-3.47084065632979,2.88000589655946,6.6485587228404));
#98880=CARTESIAN_POINT('Ctrl Pts',(-3.4671846626649,2.87935454977973,6.6504622019202));
#98881=CARTESIAN_POINT('Ctrl Pts',(-3.463528669,2.878703203,6.652365681));
#98882=CARTESIAN_POINT('Ctrl Pts',(-3.301996416,2.84992484,6.736466829));
#98883=CARTESIAN_POINT('Ctrl Pts',(-3.136572664,2.821428571,6.812628856));
#98884=CARTESIAN_POINT('Ctrl Pts',(-2.928243412,2.785541304,6.908544816));
#98885=CARTESIAN_POINT('Ctrl Pts',(-2.714442712,2.7492206,6.9915521));
#98886=CARTESIAN_POINT('Ctrl Pts',(-3.56411537921917,2.88000589655946,6.313449537644));
#98887=CARTESIAN_POINT('Ctrl Pts',(-3.56064349760959,2.87935454977973,6.315404480822));
#98888=CARTESIAN_POINT('Ctrl Pts',(-3.557171616,2.878703203,6.317359424));
#98889=CARTESIAN_POINT('Ctrl Pts',(-3.40377396,2.84992484,6.403734403));
#98890=CARTESIAN_POINT('Ctrl Pts',(-3.246364857,2.821428571,6.482562396));
#98891=CARTESIAN_POINT('Ctrl Pts',(-3.048128992,2.785541304,6.581835786));
#98892=CARTESIAN_POINT('Ctrl Pts',(-2.844197672,2.7492206,6.668810959));
#98893=CARTESIAN_POINT('',(-2.84857342605668,2.75000000026644,6.66694304465092));
#98894=CARTESIAN_POINT('Ctrl Pts',(-2.84857342756987,2.75,6.66694304567485));
#98895=CARTESIAN_POINT('Ctrl Pts',(-3.050258032,2.785926731,6.580769596));
#98896=CARTESIAN_POINT('Ctrl Pts',(-3.246364857,2.821428571,6.482562396));
#98897=CARTESIAN_POINT('Ctrl Pts',(-3.40377395943923,2.84992483970815,6.40373440364824));
#98898=CARTESIAN_POINT('Ctrl Pts',(-3.55717162115202,2.87870320490792,6.31735943591912));
#98899=CARTESIAN_POINT('Ctrl Pts',(-2.94741403646362,2.78894740127666,6.89657527325697));
#98900=CARTESIAN_POINT('Ctrl Pts',(-2.9308291392667,2.78276663836071,6.85830838235336));
#98901=CARTESIAN_POINT('Ctrl Pts',(-2.91428838878772,2.77643548708084,6.82002006788011));
#98902=CARTESIAN_POINT('Ctrl Pts',(-2.88134412019285,2.76346377183966,6.74349049123431));
#98903=CARTESIAN_POINT('Ctrl Pts',(-2.86492097451376,2.75681548747854,6.70520365258805));
#98904=CARTESIAN_POINT('Ctrl Pts',(-2.84857342828654,2.75000000140052,6.66694304349615));
#98905=CARTESIAN_POINT('Ctrl Pts',(-3.17577251,2.749235821,6.79444397800001));
#98906=CARTESIAN_POINT('Ctrl Pts',(-2.807608091,2.813580595,6.966526703));
#98907=CARTESIAN_POINT('Ctrl Pts',(-2.423004915,2.878703203,7.097819889));
#98908=CARTESIAN_POINT('Ctrl Pts',(-2.852862993,2.749235821,6.665108607));
#98909=CARTESIAN_POINT('Ctrl Pts',(-2.491706754,2.813580595,6.819694125));
#98910=CARTESIAN_POINT('Ctrl Pts',(-2.115961384,2.878703203,6.93434982));
#98911=CARTESIAN_POINT('Origin',(0.0463567587563665,2.94638889285433,-0.19055282367663));
#98912=CARTESIAN_POINT('Ctrl Pts',(-1.96045073457827,2.88000589655946,7.239247258558));
#98913=CARTESIAN_POINT('Ctrl Pts',(-1.95647102428913,2.87935454977973,7.240320304779));
#98914=CARTESIAN_POINT('Ctrl Pts',(-1.952491314,2.878703203,7.241393351));
#98915=CARTESIAN_POINT('Ctrl Pts',(-1.776656335,2.84992484,7.288803601));
#98916=CARTESIAN_POINT('Ctrl Pts',(-1.598727514,2.821428571,7.327623785));
#98917=CARTESIAN_POINT('Ctrl Pts',(-1.374649788,2.785541304,7.376512652));
#98918=CARTESIAN_POINT('Ctrl Pts',(-1.148003517,2.7492206,7.41161844200001));
#98919=CARTESIAN_POINT('Ctrl Pts',(-2.12358331591636,2.88000589655946,6.93202404846616));
#98920=CARTESIAN_POINT('Ctrl Pts',(-2.11977234995818,2.87935454977973,6.93318693423308));
#98921=CARTESIAN_POINT('Ctrl Pts',(-2.115961384,2.878703203,6.93434982));
#98922=CARTESIAN_POINT('Ctrl Pts',(-1.947582012,2.84992484,6.985729438));
#98923=CARTESIAN_POINT('Ctrl Pts',(-1.776907359,2.821428571,7.028876172));
#98924=CARTESIAN_POINT('Ctrl Pts',(-1.561965294,2.785541304,7.083213754));
#98925=CARTESIAN_POINT('Ctrl Pts',(-1.344104683,2.7492206,7.12431629));
#98926=CARTESIAN_POINT('',(-1.3487796814196,2.7499999998901,7.12343270402948));
#98927=CARTESIAN_POINT('Ctrl Pts',(-1.34877968312061,2.75,7.12343270523327));
#98928=CARTESIAN_POINT('Ctrl Pts',(-1.564273757,2.785926731,7.082630172));
#98929=CARTESIAN_POINT('Ctrl Pts',(-1.776907359,2.821428571,7.028876172));
#98930=CARTESIAN_POINT('Ctrl Pts',(-1.94758201266314,2.84992483974664,6.98572943782307));
#98931=CARTESIAN_POINT('Ctrl Pts',(-2.11596138701272,2.8787032050476,6.93434983239584));
#98932=CARTESIAN_POINT('Ctrl Pts',(-1.39594531129416,2.78894740124099,7.36894406871015));
#98933=CARTESIAN_POINT('Ctrl Pts',(-1.38797426353557,2.7827665245471,7.32800582015064));
#98934=CARTESIAN_POINT('Ctrl Pts',(-1.38005116146418,2.77643543111063,7.28705729346634));
#98935=CARTESIAN_POINT('Ctrl Pts',(-1.36432877629868,2.76346377184232,7.20523524465428));
#98936=CARTESIAN_POINT('Ctrl Pts',(-1.35652013321739,2.75681548748474,7.16431303999871));
#98937=CARTESIAN_POINT('Ctrl Pts',(-1.34877968347368,2.75000000143294,7.12343270338333));
#98938=CARTESIAN_POINT('Ctrl Pts',(-1.6409201,2.749235821,7.318290868));
#98939=CARTESIAN_POINT('Ctrl Pts',(-1.244370462,2.813580595,7.407205928));
#98940=CARTESIAN_POINT('Ctrl Pts',(-0.840534941,2.878703203,7.452751238));
#98941=CARTESIAN_POINT('Ctrl Pts',(-1.353363311,2.749235821,7.122563285));
#98942=CARTESIAN_POINT('Ctrl Pts',(-0.967419387,2.813580595,7.195896764));
#98943=CARTESIAN_POINT('Ctrl Pts',(-0.575811149000001,2.878703203,7.227097725));
#98944=CARTESIAN_POINT('Origin',(0.00430989000333039,2.94638757434166,-0.19606265922411));
#98945=CARTESIAN_POINT('Ctrl Pts',(-0.3583923162207,2.88000589655946,7.49143663814594));
#98946=CARTESIAN_POINT('Ctrl Pts',(-0.35427497611035,2.87935454977973,7.49162907707297));
#98947=CARTESIAN_POINT('Ctrl Pts',(-0.350157636,2.878703203,7.491821516));
#98948=CARTESIAN_POINT('Ctrl Pts',(-0.168241778,2.84992484,7.500324018));
#98949=CARTESIAN_POINT('Ctrl Pts',(0.013872358,2.821428571,7.499987171));
#98950=CARTESIAN_POINT('Ctrl Pts',(0.243220932,2.785541304,7.499562956));
#98951=CARTESIAN_POINT('Ctrl Pts',(0.472115046,2.7492206,7.485125743));
#98952=CARTESIAN_POINT('Ctrl Pts',(-0.583754856471104,2.88000589655946,
7.22646481878787));
#98953=CARTESIAN_POINT('Ctrl Pts',(-0.579783002735552,2.87935454977973,
7.22678127189393));
#98954=CARTESIAN_POINT('Ctrl Pts',(-0.575811149,2.878703203,7.227097725));
#98955=CARTESIAN_POINT('Ctrl Pts',(-0.400323295,2.84992484,7.241079528));
#98956=CARTESIAN_POINT('Ctrl Pts',(-0.224363648,2.821428571,7.24652751));
#98957=CARTESIAN_POINT('Ctrl Pts',(-0.002765835,2.785541304,7.253388519));
#98958=CARTESIAN_POINT('Ctrl Pts',(0.218837146,2.7492206,7.24669651));
#98959=CARTESIAN_POINT('Ctrl Pts',(0.214081503710257,2.74999999962186,7.24683856131898));
#98960=CARTESIAN_POINT('Ctrl Pts',(0.0675659028784404,2.77401081851383,
7.2511668310443));
#98961=CARTESIAN_POINT('Ctrl Pts',(-0.078714851124164,2.79784107628333,
7.25103702122927));
#98962=CARTESIAN_POINT('Ctrl Pts',(-0.224363649180743,2.82142857122736,
7.24652751019394));
#98963=CARTESIAN_POINT('Ctrl Pts',(-0.341350013056901,2.84037424965354,
7.24290543172649));
#98964=CARTESIAN_POINT('Ctrl Pts',(-0.45856829321948,2.85947647439222,7.23643892552997));
#98965=CARTESIAN_POINT('Ctrl Pts',(-0.575811148978606,2.87870320488418,
7.22709773758857));
#98966=CARTESIAN_POINT('Ctrl Pts',(-1.38354074570591,3.00402491777226,7.11681549624605));
#98967=CARTESIAN_POINT('Ctrl Pts',(-1.37010922035295,3.00629206938617,7.11937410662298));
#98968=CARTESIAN_POINT('Ctrl Pts',(-1.356677695,3.008559221,7.121932717));
#98969=CARTESIAN_POINT('Ctrl Pts',(-0.967145401,3.074309666,7.196135858));
#98970=CARTESIAN_POINT('Ctrl Pts',(-0.571843906,3.139297275,7.227412715));
#98971=CARTESIAN_POINT('Ctrl Pts',(-1.18863048763931,3.00402491777233,7.40579634984612));
#98972=CARTESIAN_POINT('Ctrl Pts',(-1.17465535648591,3.00629206938616,7.40798532109787));
#98973=CARTESIAN_POINT('Ctrl Pts',(-1.16068022533253,3.008559221,7.41017429234949));
#98974=CARTESIAN_POINT('Ctrl Pts',(-0.755382632239146,3.074309666,7.47365740173177));
#98975=CARTESIAN_POINT('Ctrl Pts',(-0.345579041149821,3.139297275,7.49255875910434));
#98976=CARTESIAN_POINT('',(-0.576538528010638,3.13852541863614,7.22703973359675));
#98977=CARTESIAN_POINT('Ctrl Pts',(-0.576538527949452,3.13852541811464,
7.22703973501174));
#98978=CARTESIAN_POINT('Ctrl Pts',(-0.580097416125384,3.13166453921389,
7.26849592895408));
#98979=CARTESIAN_POINT('Ctrl Pts',(-0.583636789832934,3.12496635677949,
7.3100051760473));
#98980=CARTESIAN_POINT('Ctrl Pts',(-0.590672705697527,3.11188594211542,
7.39302866755765));
#98981=CARTESIAN_POINT('Ctrl Pts',(-0.594173108964219,3.10549653061751,
7.43458851627657));
#98982=CARTESIAN_POINT('Ctrl Pts',(-0.597654041416069,3.09925366546798,
7.4761493862768));
#98983=CARTESIAN_POINT('Origin',(0.046862716923752,2.94646386697818,-0.190697407010468));
#98984=CARTESIAN_POINT('Ctrl Pts',(-2.121152813,3.13930489,6.932763572));
#98985=CARTESIAN_POINT('Ctrl Pts',(-1.744059979,3.07388663,7.048139138));
#98986=CARTESIAN_POINT('Ctrl Pts',(-1.356677695,3.008559221,7.121932717));
#98987=CARTESIAN_POINT('Ctrl Pts',(-2.428318655,3.13930489,7.0960037));
#98988=CARTESIAN_POINT('Ctrl Pts',(-2.042346724,3.07388663,7.22808689500001));
#98989=CARTESIAN_POINT('Ctrl Pts',(-1.644325536,3.008559221,7.317526463));
#98990=CARTESIAN_POINT('',(-2.11665928922809,3.13852541864585,6.93413681937955));
#98991=CARTESIAN_POINT('Origin',(0.0504307652673577,3.08928610040167,-0.193189497028357));
#98992=CARTESIAN_POINT('Ctrl Pts',(-2.19083234638042,3.0992536654612,7.17288321586642));
#98993=CARTESIAN_POINT('Ctrl Pts',(-2.17849833215872,3.10549658403016,7.13304197249726));
#98994=CARTESIAN_POINT('Ctrl Pts',(-2.16614568311497,3.11188596847193,7.09320643365134));
#98995=CARTESIAN_POINT('Ctrl Pts',(-2.14142655079244,3.12496644434497,7.01363612678527));
#98996=CARTESIAN_POINT('Ctrl Pts',(-2.12904675200634,3.13166458238639,6.97385848625679));
#98997=CARTESIAN_POINT('Ctrl Pts',(-2.11665928998501,3.13852541825092,6.93413682009051));
#98998=CARTESIAN_POINT('Ctrl Pts',(-2.8810992937521,3.00402491751786,6.65300794161889));
#98999=CARTESIAN_POINT('Ctrl Pts',(-2.86853181487605,3.00629206925893,6.65839411430946));
#99000=CARTESIAN_POINT('Ctrl Pts',(-2.855964336,3.008559221,6.663780287));
#99001=CARTESIAN_POINT('Ctrl Pts',(-2.491490572,3.074309666,6.819986528));
#99002=CARTESIAN_POINT('Ctrl Pts',(-2.112154606,3.139297275,6.935510285));
#99003=CARTESIAN_POINT('Ctrl Pts',(-2.75286827026256,3.00402491751786,6.97713252668685));
#99004=CARTESIAN_POINT('Ctrl Pts',(-2.73969043327862,3.00629206925893,6.98227456139302));
#99005=CARTESIAN_POINT('Ctrl Pts',(-2.72651259629476,3.008559221,6.98741659609931));
#99006=CARTESIAN_POINT('Ctrl Pts',(-2.34433762753113,3.074309666,7.13654250770801));
#99007=CARTESIAN_POINT('Ctrl Pts',(-1.94817824988654,3.139297275,7.24309761967647));
#99008=CARTESIAN_POINT('Origin',(0.0867605426050477,2.94646406243098,-0.176162716798953));
#99009=CARTESIAN_POINT('Ctrl Pts',(-3.561900676,3.13930489,6.314694258));
#99010=CARTESIAN_POINT('Ctrl Pts',(-3.218426399,3.07388663,6.508436221));
#99011=CARTESIAN_POINT('Ctrl Pts',(-2.855964336,3.008559221,6.663780287));
#99012=CARTESIAN_POINT('Ctrl Pts',(-3.896976953,3.13930489,6.408086347));
#99013=CARTESIAN_POINT('Ctrl Pts',(-3.548422814,3.07388663,6.620054066));
#99014=CARTESIAN_POINT('Ctrl Pts',(-3.178934004,3.008559221,6.792965376));
#99015=CARTESIAN_POINT('',(-3.55780741585257,3.13852541863812,6.31700137505845));
#99016=CARTESIAN_POINT('Origin',(0.0907828019625706,3.08928565424525,-0.177833967385367));
#99017=CARTESIAN_POINT('Ctrl Pts',(-3.68156976613604,3.09925366549553,6.53422099858765));
#99018=CARTESIAN_POINT('Ctrl Pts',(-3.66095960104766,3.10549653063559,6.49796298013341));
#99019=CARTESIAN_POINT('Ctrl Pts',(-3.64033219339726,3.11188594217017,6.46171406386782));
#99020=CARTESIAN_POINT('Ctrl Pts',(-3.59908558327855,3.12496646037402,6.38931771480979));
#99021=CARTESIAN_POINT('Ctrl Pts',(-3.57844422745511,3.13166459020887,6.35313139156989));
#99022=CARTESIAN_POINT('Ctrl Pts',(-3.55780741727561,3.13852541813074,6.31700137561132));
#99023=CARTESIAN_POINT('Ctrl Pts',(-4.24394083812014,3.00402491760373,5.87811313046301));
#99024=CARTESIAN_POINT('Ctrl Pts',(-4.23282504806003,3.00629206930187,5.8860750137315));
#99025=CARTESIAN_POINT('Ctrl Pts',(-4.221709258,3.008559221,5.894036897));
#99026=CARTESIAN_POINT('Ctrl Pts',(-3.899336413,3.074309666,6.124942208));
#99027=CARTESIAN_POINT('Ctrl Pts',(-3.553703304,3.139297275,6.319311104));
#99028=CARTESIAN_POINT('Ctrl Pts',(-4.18838499015742,3.00402491760373,6.22222574229489));
#99029=CARTESIAN_POINT('Ctrl Pts',(-4.17662062936595,3.00629206930187,6.23008040435059));
#99030=CARTESIAN_POINT('Ctrl Pts',(-4.16485626857438,3.008559221,6.23793506640633));
#99031=CARTESIAN_POINT('Ctrl Pts',(-3.82367400105311,3.074309666,6.46573081819198));
#99032=CARTESIAN_POINT('Ctrl Pts',(-3.45968280922227,3.139297275,6.65495728658097));
#99033=CARTESIAN_POINT('Origin',(0.122601975476209,2.94646403066942,-0.153393243281784));
#99034=CARTESIAN_POINT('Ctrl Pts',(-4.836098022,3.13930489,5.401356859));
#99035=CARTESIAN_POINT('Ctrl Pts',(-4.542302778,3.07388663,5.664406059));
#99036=CARTESIAN_POINT('Ctrl Pts',(-4.221709258,3.008559221,5.894036897));
#99037=CARTESIAN_POINT('Ctrl Pts',(-5.183416941,3.13930489,5.42053399799999));
#99038=CARTESIAN_POINT('Ctrl Pts',(-4.888578597,3.07388663,5.702474866));
#99039=CARTESIAN_POINT('Ctrl Pts',(-4.564899051,3.008559221,5.950772778));
#99040=CARTESIAN_POINT('',(-4.83259642193341,3.13852541864044,5.40448996693194));
#99041=CARTESIAN_POINT('Origin',(0.126887787059965,3.0892861071041,-0.154158578376543));
#99042=CARTESIAN_POINT('Ctrl Pts',(-5.00016107556263,3.09925366546734,5.5900258693423));
#99043=CARTESIAN_POINT('Ctrl Pts',(-4.97223836249971,3.10549653062517,5.55904611943078));
#99044=CARTESIAN_POINT('Ctrl Pts',(-4.94430076676525,3.11188594216358,5.52807896560806));
#99045=CARTESIAN_POINT('Ctrl Pts',(-4.88845539869022,3.12496646175563,5.46624199840628));
#99046=CARTESIAN_POINT('Ctrl Pts',(-4.86051763957211,3.13166459091205,5.43533897604021));
#99047=CARTESIAN_POINT('Ctrl Pts',(-4.83259642384329,3.13852541817872,5.40448996692781));
#99048=CARTESIAN_POINT('Ctrl Pts',(-5.40834042663095,3.00402491769086,4.8283642821389));
#99049=CARTESIAN_POINT('Ctrl Pts',(-5.3991960873154,3.00629206934543,4.83852958706951));
#99050=CARTESIAN_POINT('Ctrl Pts',(-5.390051748,3.008559221,4.848694892));
#99051=CARTESIAN_POINT('Ctrl Pts',(-5.124853618,3.074309666,5.143502397));
#99052=CARTESIAN_POINT('Ctrl Pts',(-4.829084786,3.139297275,5.407627958));
#99053=CARTESIAN_POINT('Ctrl Pts',(-5.4280574831546,3.00402491769085,5.17637459770828));
#99054=CARTESIAN_POINT('Ctrl Pts',(-5.41825668693024,3.00629206934543,5.18657461173586));
#99055=CARTESIAN_POINT('Ctrl Pts',(-5.40845589070588,3.008559221,5.19677462576344));
#99056=CARTESIAN_POINT('Ctrl Pts',(-5.12421962807818,3.074309666,5.49258874122631));
#99057=CARTESIAN_POINT('Ctrl Pts',(-4.8094164452404,3.139297275,5.75563854733654));
#99058=CARTESIAN_POINT('Origin',(0.152710607699467,2.94646400129146,-0.123451173810367));
#99059=CARTESIAN_POINT('Ctrl Pts',(-5.884164799,3.13930489,4.235458017));
#99060=CARTESIAN_POINT('Ctrl Pts',(-5.653786127,3.07388663,4.555514565));
#99061=CARTESIAN_POINT('Ctrl Pts',(-5.390051748,3.008559221,4.848694892));
#99062=CARTESIAN_POINT('Ctrl Pts',(-6.227486113,3.13930489,4.179523504));
#99063=CARTESIAN_POINT('Ctrl Pts',(-6.000149879,3.07388663,4.51825428));
#99064=CARTESIAN_POINT('Ctrl Pts',(-5.737414491,3.008559221,4.830328659));
#99065=CARTESIAN_POINT('',(-5.88141858947571,3.13852541860795,4.23927061567422));
#99066=CARTESIAN_POINT('Origin',(0.157060863461149,3.08928612816204,-0.123277390314245));
#99067=CARTESIAN_POINT('Ctrl Pts',(-6.0849504101184,3.099253665473,4.38444734373401));
#99068=CARTESIAN_POINT('Ctrl Pts',(-6.05102049225407,3.10549658433644,4.36019423237365));
#99069=CARTESIAN_POINT('Ctrl Pts',(-6.01707919397285,3.11188596863484,4.33595694134614));
#99070=CARTESIAN_POINT('Ctrl Pts',(-5.94924644971696,3.12496646698919,4.28757086998459));
#99071=CARTESIAN_POINT('Ctrl Pts',(-5.91531863784531,3.13166459351811,4.26339614570836));
#99072=CARTESIAN_POINT('Ctrl Pts',(-5.88141859215413,3.13852541824126,4.23927061437438));
#99073=CARTESIAN_POINT('Ctrl Pts',(-6.31985202855174,3.00402491761906,3.55284648476577));
#99074=CARTESIAN_POINT('Ctrl Pts',(-6.31310671877591,3.00629206930957,3.56473989338288));
#99075=CARTESIAN_POINT('Ctrl Pts',(-6.306361409,3.008559221,3.576633302));
#99076=CARTESIAN_POINT('Ctrl Pts',(-6.11073836300001,3.074309666,3.921558131));
#99077=CARTESIAN_POINT('Ctrl Pts',(-5.87866363,3.139297275,4.243090139));
#99078=CARTESIAN_POINT('Ctrl Pts',(-6.41392004154672,3.00402491761906,3.88848192939998));
#99079=CARTESIAN_POINT('Ctrl Pts',(-6.40654108388342,3.00629206930957,3.90055035443249));
#99080=CARTESIAN_POINT('Ctrl Pts',(-6.39916212622019,3.008559221,3.912618779465));
#99081=CARTESIAN_POINT('Ctrl Pts',(-6.18516244016494,3.074309666,4.26261931965024));
#99082=CARTESIAN_POINT('Ctrl Pts',(-5.93426711363373,3.139297275,4.587192546093));
#99083=CARTESIAN_POINT('Origin',(0.17567859128684,2.94646403076769,-0.0877366492637827));
#99084=CARTESIAN_POINT('Ctrl Pts',(-6.65709457100001,3.13930489,2.871513865));
#99085=CARTESIAN_POINT('Ctrl Pts',(-6.500904721,3.07388663,3.233612273));
#99086=CARTESIAN_POINT('Ctrl Pts',(-6.306361409,3.008559221,3.576633302));
#99087=CARTESIAN_POINT('Ctrl Pts',(-6.980364955,3.13930489,2.743083136));
#99088=CARTESIAN_POINT('Ctrl Pts',(-6.83116082000001,3.07388663,3.122765145));
#99089=CARTESIAN_POINT('Ctrl Pts',(-6.641654807,3.008559221,3.48402374));
#99090=CARTESIAN_POINT('',(-6.65523216194324,3.13852541861274,2.8758276813969));
#99091=CARTESIAN_POINT('Origin',(0.179889870119069,3.08928612550937,-0.0866317942447253));
#99092=CARTESIAN_POINT('Ctrl Pts',(-6.88521422635454,3.09925366552483,2.97385693256406));
#99093=CARTESIAN_POINT('Ctrl Pts',(-6.84686419892947,3.10549653068322,2.95746491590425));
#99094=CARTESIAN_POINT('Ctrl Pts',(-6.80850595347592,3.11188594219784,2.94109058031538));
#99095=CARTESIAN_POINT('Ctrl Pts',(-6.73185741844377,3.12496645889943,2.90841773763592));
#99096=CARTESIAN_POINT('Ctrl Pts',(-6.69352594351918,3.13166458955811,2.89210167091627));
#99097=CARTESIAN_POINT('Ctrl Pts',(-6.65523216371794,3.13852541826953,2.87582767950766));
#99098=CARTESIAN_POINT('Ctrl Pts',(-6.93585437234022,3.00402491788988,2.1112015374355));
#99099=CARTESIAN_POINT('Ctrl Pts',(-6.93182349567006,3.00629206944494,2.12426692621775));
#99100=CARTESIAN_POINT('Ctrl Pts',(-6.92779261900001,3.008559221,2.137332315));
#99101=CARTESIAN_POINT('Ctrl Pts',(-6.810891773,3.074309666,2.516246166));
#99102=CARTESIAN_POINT('Ctrl Pts',(-6.653362696,3.139297275,2.880150141));
#99103=CARTESIAN_POINT('Ctrl Pts',(-7.09987482717042,3.0040249178898,2.41876816939517));
#99104=CARTESIAN_POINT('Ctrl Pts',(-7.09526274034048,3.00629206944494,2.43214069834475));
#99105=CARTESIAN_POINT('Ctrl Pts',(-7.09065065351051,3.008559221,2.44551322729433));
#99106=CARTESIAN_POINT('Ctrl Pts',(-6.95689393099661,3.074309666,2.8333345563295));
#99107=CARTESIAN_POINT('Ctrl Pts',(-6.78163804750084,3.139297275,3.20425451918572));
#99108=CARTESIAN_POINT('Origin',(0.1904321565972,2.94646407124334,-0.047919731841701));
#99109=CARTESIAN_POINT('Ctrl Pts',(-7.118745999,3.13930489,1.373300916));
#99110=CARTESIAN_POINT('Ctrl Pts',(-7.044048235,3.07388663,1.760509866));
#99111=CARTESIAN_POINT('Ctrl Pts',(-6.92779261899999,3.008559221,2.137332315));
#99112=CARTESIAN_POINT('Ctrl Pts',(-7.406849691,3.13930489,1.178379249));
#99113=CARTESIAN_POINT('Ctrl Pts',(-7.342754274,3.07388663,1.581258982));
#99114=CARTESIAN_POINT('Ctrl Pts',(-7.235338726,3.008559221,1.974809744));
#99115=CARTESIAN_POINT('',(-7.11785447482644,3.13852541860989,1.37791424072262));
#99116=CARTESIAN_POINT('Origin',(0.19430736713235,3.08928609441336,-0.0459353841119275));
#99117=CARTESIAN_POINT('Ctrl Pts',(-7.36353307773095,3.09925366545253,1.42421227703033));
#99118=CARTESIAN_POINT('Ctrl Pts',(-7.3225555122514,3.10549658262431,1.41644755423299));
#99119=CARTESIAN_POINT('Ctrl Pts',(-7.28157424400658,3.11188596777925,1.40870196489128));
#99120=CARTESIAN_POINT('Ctrl Pts',(-7.19969419612704,3.12496645535936,1.39327019884434));
#99121=CARTESIAN_POINT('Ctrl Pts',(-7.15875140609062,3.13166458779982,1.38557572453528));
#99122=CARTESIAN_POINT('Ctrl Pts',(-7.11785447620099,3.13852541823332,1.37791423874308));
#99123=CARTESIAN_POINT('Ctrl Pts',(-7.22754387541306,3.00402491762742,0.570839149256198));
#99124=CARTESIAN_POINT('Ctrl Pts',(-7.22641591070655,3.00629206931375,0.584465596628102));
#99125=CARTESIAN_POINT('Ctrl Pts',(-7.225287946,3.008559221,0.598092044));
#99126=CARTESIAN_POINT('Ctrl Pts',(-7.192575454,3.074309666,0.993277326));
#99127=CARTESIAN_POINT('Ctrl Pts',(-7.116957917,3.139297275,1.382537524));
#99128=CARTESIAN_POINT('Ctrl Pts',(-7.45384735688251,3.00402491762749,0.835955494763049));
#99129=CARTESIAN_POINT('Ctrl Pts',(-7.45221779643275,3.00629206931374,0.850006844585464));
#99130=CARTESIAN_POINT('Ctrl Pts',(-7.45058823598314,3.008559221,0.86405819440788));
#99131=CARTESIAN_POINT('Ctrl Pts',(-7.40332879350009,3.074309666,1.27156621836309));
#99132=CARTESIAN_POINT('Ctrl Pts',(-7.31190712241195,3.139297275,1.67148911287974));
#99133=CARTESIAN_POINT('Origin',(0.196281286854735,2.94646418661912,-0.00586212603608402));
#99134=CARTESIAN_POINT('Ctrl Pts',(-7.247532776,3.13930489,-0.189126057));
#99135=CARTESIAN_POINT('Ctrl Pts',(-7.257819883,3.07388663,0.205087974));
#99136=CARTESIAN_POINT('Ctrl Pts',(-7.225287946,3.008559221,0.598092044));
#99137=CARTESIAN_POINT('Ctrl Pts',(-7.486998367,3.13930489,-0.441424342));
#99138=CARTESIAN_POINT('Ctrl Pts',(-7.511008699,3.07388663,-0.034185093));
#99139=CARTESIAN_POINT('Ctrl Pts',(-7.490706247,3.008559221,0.373255838));
#99140=CARTESIAN_POINT('',(-7.24765382364659,3.13852541862919,-0.184428939472681));
#99141=CARTESIAN_POINT('Origin',(0.199639167738409,3.08928608524063,-0.0030910937600424));
#99142=CARTESIAN_POINT('Ctrl Pts',(-7.49754130656375,3.09925366544167,-0.19202696212638));
#99143=CARTESIAN_POINT('Ctrl Pts',(-7.45585293515826,3.10549653062226,-0.190801194864911));
#99144=CARTESIAN_POINT('Ctrl Pts',(-7.41416452940221,3.11188594215044,-0.189555930012976));
#99145=CARTESIAN_POINT('Ctrl Pts',(-7.33088131199607,3.12496644638324,-0.187025116539695));
#99146=CARTESIAN_POINT('Ctrl Pts',(-7.28924162669241,3.13166458338676,-0.185738207668968));
#99147=CARTESIAN_POINT('Ctrl Pts',(-7.24765382450455,3.13852541823566,-0.184428940115855));
#99148=CARTESIAN_POINT('Ctrl Pts',(-7.18128145949877,3.00402491793428,-0.996215039478427));
#99149=CARTESIAN_POINT('Ctrl Pts',(-7.18310914924944,3.00629206946718,-0.982664692739221));
#99150=CARTESIAN_POINT('Ctrl Pts',(-7.184936839,3.008559221,-0.969114346));
#99151=CARTESIAN_POINT('Ctrl Pts',(-7.237942301,3.074309666,-0.576136058000001));
#99152=CARTESIAN_POINT('Ctrl Pts',(-7.24777209600001,3.139297275,-0.179721011));
#99153=CARTESIAN_POINT('Ctrl Pts',(-7.45928626934456,3.00402491793435,-0.785945525194474));
#99154=CARTESIAN_POINT('Ctrl Pts',(-7.46071543184991,3.00629206946717,-0.77187238178124));
#99155=CARTESIAN_POINT('Ctrl Pts',(-7.4621445943553,3.008559221,-0.757799238368011));
#99156=CARTESIAN_POINT('Ctrl Pts',(-7.50359223001004,3.074309666,-0.349659143376739));
#99157=CARTESIAN_POINT('Ctrl Pts',(-7.50027954852915,3.139297275,0.0605667338100289));
#99158=CARTESIAN_POINT('Origin',(0.192952530454407,2.94646401362825,0.0364696205494065));
#99159=CARTESIAN_POINT('Ctrl Pts',(-7.03743297500001,3.13930489,-1.742709706));
#99160=CARTESIAN_POINT('Ctrl Pts',(-7.132223939,3.07388663,-1.359923604));
#99161=CARTESIAN_POINT('Ctrl Pts',(-7.184936839,3.008559221,-0.969114346));
#99162=CARTESIAN_POINT('Ctrl Pts',(-7.217063321,3.13930489,-2.040587421));
#99163=CARTESIAN_POINT('Ctrl Pts',(-7.328056705,3.07388663,-1.648030711));
#99164=CARTESIAN_POINT('Ctrl Pts',(-7.39581666999999,3.008559221,-1.245751095));
#99165=CARTESIAN_POINT('',(-7.03856093433481,3.13852541864668,-1.7381484266357));
#99166=CARTESIAN_POINT('Origin',(0.195638787581568,3.08928568804237,0.0398981238858506));
#99167=CARTESIAN_POINT('Ctrl Pts',(-7.28097283682832,3.09925366542448,-1.7992872333711));
#99168=CARTESIAN_POINT('Ctrl Pts',(-7.24052262012714,3.10549653059928,-1.78912835643529));
#99169=CARTESIAN_POINT('Ctrl Pts',(-7.20007656102457,3.11188594216363,-1.77895043030792));
#99170=CARTESIAN_POINT('Ctrl Pts',(-7.11928453719344,3.12496644183097,-1.75857536327087));
#99171=CARTESIAN_POINT('Ctrl Pts',(-7.07889499698815,3.13166458114327,-1.74836723648591));
#99172=CARTESIAN_POINT('Ctrl Pts',(-7.03856093505771,3.13852541823511,-1.73814842746672));
#99173=CARTESIAN_POINT('Ctrl Pts',(-6.79923030407032,3.00402491787842,-2.51668732206627));
#99174=CARTESIAN_POINT('Ctrl Pts',(-6.80392818753517,3.00629206943921,-2.5038466740331));
#99175=CARTESIAN_POINT('Ctrl Pts',(-6.80862607100001,3.008559221,-2.491006026));
#99176=CARTESIAN_POINT('Ctrl Pts',(-6.944871011,3.074309666,-2.11860996));
#99177=CARTESIAN_POINT('Ctrl Pts',(-7.039688507,3.139297275,-1.733575992));
#99178=CARTESIAN_POINT('Ctrl Pts',(-7.11593724543511,3.00402491787835,-2.37109660944742));
#99179=CARTESIAN_POINT('Ctrl Pts',(-7.12035830480933,3.00629206943921,-2.35765971580576));
#99180=CARTESIAN_POINT('Ctrl Pts',(-7.12477936418368,3.008559221,-2.34422282216417));
#99181=CARTESIAN_POINT('Ctrl Pts',(-7.25299603317955,3.074309666,-1.95453483145745));
#99182=CARTESIAN_POINT('Ctrl Pts',(-7.33794723813668,3.139297275,-1.55318767880479));
#99183=CARTESIAN_POINT('Origin',(0.180601220226997,2.94646402715384,0.0770959809799848));
#99184=CARTESIAN_POINT('Ctrl Pts',(-6.49827063,3.13930489,-3.214806186));
#99185=CARTESIAN_POINT('Ctrl Pts',(-6.673133131,3.07388663,-2.861346666));
#99186=CARTESIAN_POINT('Ctrl Pts',(-6.808626071,3.008559221,-2.491006026));
#99187=CARTESIAN_POINT('Ctrl Pts',(-6.609666415,3.13930489,-3.5443349));
#99188=CARTESIAN_POINT('Ctrl Pts',(-6.802452925,3.07388663,-3.184816244));
#99189=CARTESIAN_POINT('Ctrl Pts',(-6.955106924,3.008559221,-2.806508092));
#99190=CARTESIAN_POINT('',(-6.50035275870565,3.13852541865559,-3.21059402478549));
#99191=CARTESIAN_POINT('Origin',(0.182487905431642,3.08928570436188,0.0810218689438846));
#99192=CARTESIAN_POINT('Ctrl Pts',(-6.72395416956975,3.09925366545775,-3.32241483335559));
#99193=CARTESIAN_POINT('Ctrl Pts',(-6.68663319932783,3.10549658336818,-3.30379770709166));
#99194=CARTESIAN_POINT('Ctrl Pts',(-6.64932086725242,3.11188596813281,-3.28516311143848));
#99195=CARTESIAN_POINT('Ctrl Pts',(-6.57479782539728,3.12496645509081,-3.2478965415174));
#99196=CARTESIAN_POINT('Ctrl Pts',(-6.53754705603529,3.13166458763075,-3.22924453809411));
#99197=CARTESIAN_POINT('Ctrl Pts',(-6.50035275940382,3.13852541818432,-3.21059402611261));
#99198=CARTESIAN_POINT('Ctrl Pts',(-6.09925469563289,3.00402491764879,-3.91948210370576));
#99199=CARTESIAN_POINT('Ctrl Pts',(-6.10660310531644,3.00629206932443,-3.90795156835288));
#99200=CARTESIAN_POINT('Ctrl Pts',(-6.113951515,3.008559221,-3.896421033));
#99201=CARTESIAN_POINT('Ctrl Pts',(-6.32706527,3.074309666,-3.562020014));
#99202=CARTESIAN_POINT('Ctrl Pts',(-6.50243690800001,3.139297275,-3.206370886));
#99203=CARTESIAN_POINT('Ctrl Pts',(-6.43985490483353,3.00402491764879,-3.84537785166561));
#99204=CARTESIAN_POINT('Ctrl Pts',(-6.447061137608,3.00629206932443,-3.83320550160551));
#99205=CARTESIAN_POINT('Ctrl Pts',(-6.4542673703825,3.008559221,-3.82103315154535));
#99206=CARTESIAN_POINT('Ctrl Pts',(-6.66325780397382,3.074309666,-3.46801864361758));
#99207=CARTESIAN_POINT('Ctrl Pts',(-6.83250066964433,3.139297275,-3.09431676171783));
#99208=CARTESIAN_POINT('Origin',(0.159805770112958,2.94646404539155,0.114117596465717));
#99209=CARTESIAN_POINT('Ctrl Pts',(-5.655256373,3.13930489,-4.536581902));
#99210=CARTESIAN_POINT('Ctrl Pts',(-5.902014034,3.07388663,-4.228976338));
#99211=CARTESIAN_POINT('Ctrl Pts',(-6.113951515,3.008559221,-3.896421033));
#99212=CARTESIAN_POINT('Ctrl Pts',(-5.693208854,3.13930489,-4.882353218));
#99213=CARTESIAN_POINT('Ctrl Pts',(-5.95877400500001,3.07388663,-4.57268331000001));
#99214=CARTESIAN_POINT('Ctrl Pts',(-6.18918411,3.008559221,-4.23603589));
#99215=CARTESIAN_POINT('',(-5.65819531291536,3.13852541863521,-4.53291581460281));
#99216=CARTESIAN_POINT('Origin',(0.160802047155685,3.0892861315675,0.118355714622324));
#99217=CARTESIAN_POINT('Ctrl Pts',(-5.85253087821732,3.09925366548479,-4.69019000880487));
#99218=CARTESIAN_POINT('Ctrl Pts',(-5.82008485761707,3.10549653062906,-4.66398545664411));
#99219=CARTESIAN_POINT('Ctrl Pts',(-5.78765060893418,3.11188594215404,-4.6377653617038));
#99220=CARTESIAN_POINT('Ctrl Pts',(-5.72288094570733,3.12496645732173,-4.58534969921783));
#99221=CARTESIAN_POINT('Ctrl Pts',(-5.69051071395346,3.1316645887218,-4.55912595969914));
#99222=CARTESIAN_POINT('Ctrl Pts',(-5.65819531327755,3.13852541816991,-4.53291581617428));
#99223=CARTESIAN_POINT('Ctrl Pts',(-5.11408471774542,3.00402491766956,-5.13900625685091));
#99224=CARTESIAN_POINT('Ctrl Pts',(-5.1237400498727,3.00629206933482,-5.12932498992548));
#99225=CARTESIAN_POINT('Ctrl Pts',(-5.13339538200001,3.008559221,-5.119643723));
#99226=CARTESIAN_POINT('Ctrl Pts',(-5.41341298900001,3.074309666,-4.838873972));
#99227=CARTESIAN_POINT('Ctrl Pts',(-5.661138586,3.139297275,-4.529239441));
#99228=CARTESIAN_POINT('Ctrl Pts',(-5.46265210565695,3.00402491766956,-5.13985349841155));
#99229=CARTESIAN_POINT('Ctrl Pts',(-5.47230655614691,3.00629206933482,-5.12951485821149));
#99230=CARTESIAN_POINT('Ctrl Pts',(-5.48196100663686,3.008559221,-5.11917621801155));
#99231=CARTESIAN_POINT('Ctrl Pts',(-5.76195304496934,3.074309666,-4.81934175864121));
#99232=CARTESIAN_POINT('Ctrl Pts',(-6.00757396465741,3.139297275,-4.49075903226973));
#99233=CARTESIAN_POINT('Origin',(0.131537820878708,2.94646399269151,0.145803241099463));
#99234=CARTESIAN_POINT('Ctrl Pts',(-4.547808613,3.13930489,-5.64623209));
#99235=CARTESIAN_POINT('Ctrl Pts',(-4.854923321,3.07388663,-5.398863776));
#99236=CARTESIAN_POINT('Ctrl Pts',(-5.133395382,3.008559221,-5.119643723));
#99237=CARTESIAN_POINT('Ctrl Pts',(-4.510543174,3.13930489,-5.992078127));
#99238=CARTESIAN_POINT('Ctrl Pts',(-4.83646943600001,3.07388663,-5.746736787));
#99239=CARTESIAN_POINT('Ctrl Pts',(-5.133861925,3.008559221,-5.46749135700001));
#99240=CARTESIAN_POINT('',(-4.55146694340282,3.1385254185988,-5.64328349840464));
#99241=CARTESIAN_POINT('Origin',(0.131599621199766,3.08928611816713,0.150156326073493));
#99242=CARTESIAN_POINT('Ctrl Pts',(-4.70744974767339,3.09925366547641,-5.8386571123626));
#99243=CARTESIAN_POINT('Ctrl Pts',(-4.68139528364441,3.10549658273153,-5.8060900009365));
#99244=CARTESIAN_POINT('Ctrl Pts',(-4.65535599040796,3.11188596783253,-5.77351065652436));
#99245=CARTESIAN_POINT('Ctrl Pts',(-4.60336851064653,3.12496646117916,-5.70839698870686));
#99246=CARTESIAN_POINT('Ctrl Pts',(-4.57739241382684,3.13166459063262,-5.67582771278378));
#99247=CARTESIAN_POINT('Ctrl Pts',(-4.55146694245507,3.13852541818957,-5.64328350085494));
#99248=CARTESIAN_POINT('Ctrl Pts',(-3.88978582096491,3.00402491769316,-6.11823618949679));
#99249=CARTESIAN_POINT('Ctrl Pts',(-3.90129660298243,3.00629206934662,-6.1108568762484));
#99250=CARTESIAN_POINT('Ctrl Pts',(-3.912807385,3.008559221,-6.103477563));
#99251=CARTESIAN_POINT('Ctrl Pts',(-4.246635534,3.074309666,-5.889467561));
#99252=CARTESIAN_POINT('Ctrl Pts',(-4.55513171500001,3.139297275,-5.640325794));
#99253=CARTESIAN_POINT('Ctrl Pts',(-4.23002176692898,3.00402491769317,-6.19399530754654));
#99254=CARTESIAN_POINT('Ctrl Pts',(-4.24167300366235,3.00629206934662,-6.18597380052345));
#99255=CARTESIAN_POINT('Ctrl Pts',(-4.25332424039563,3.008559221,-6.17795229350047));
#99256=CARTESIAN_POINT('Ctrl Pts',(-4.59122576492328,3.074309666,-5.94531780892835));
#99257=CARTESIAN_POINT('Ctrl Pts',(-4.90173977734594,3.139297275,-5.67721840210349));
#99258=CARTESIAN_POINT('Origin',(0.0971190746813649,2.94646403943336,0.170671054066455));
#99259=CARTESIAN_POINT('Ctrl Pts',(-3.227710377,3.13930489,-6.491870741));
#99260=CARTESIAN_POINT('Ctrl Pts',(-3.580821789,3.07388663,-6.316306345));
#99261=CARTESIAN_POINT('Ctrl Pts',(-3.912807385,3.008559221,-6.103477563));
#99262=CARTESIAN_POINT('Ctrl Pts',(-3.116969508,3.13930489,-6.821620122));
#99263=CARTESIAN_POINT('Ctrl Pts',(-3.488016932,3.07388663,-6.652079238));
#99264=CARTESIAN_POINT('Ctrl Pts',(-3.838486062,3.008559221,-6.443293005));
#99265=CARTESIAN_POINT('',(-3.23191703699021,3.13852541864447,-6.48977751941203));
#99266=CARTESIAN_POINT('Origin',(0.0962436524403354,3.08928611387826,0.174935665362964));
#99267=CARTESIAN_POINT('Ctrl Pts',(-3.34225349900584,3.09925366545698,-6.7141150980915));
#99268=CARTESIAN_POINT('Ctrl Pts',(-3.3238092940059,3.10549653061459,-6.6767087602362));
#99269=CARTESIAN_POINT('Ctrl Pts',(-3.30538229912358,3.11188594216861,-6.63929325890792));
#99270=CARTESIAN_POINT('Ctrl Pts',(-3.26860772366043,3.12496645256281,-6.56452604360213));
#99271=CARTESIAN_POINT('Ctrl Pts',(-3.25024035225307,3.13166458640041,-6.52713410004394));
#99272=CARTESIAN_POINT('Ctrl Pts',(-3.23191703633812,3.13852541819882,-6.48977752054084));
#99273=CARTESIAN_POINT('Ctrl Pts',(-2.48360486417183,3.00402491773169,-6.8113841981799));
#99274=CARTESIAN_POINT('Ctrl Pts',(-2.49643286458595,3.00629206936588,-6.80665188708994));
#99275=CARTESIAN_POINT('Ctrl Pts',(-2.509260865,3.008559221,-6.801919576));
#99276=CARTESIAN_POINT('Ctrl Pts',(-2.881290121,3.074309666,-6.664676193));
#99277=CARTESIAN_POINT('Ctrl Pts',(-3.236131948,3.139297275,-6.487676781));
#99278=CARTESIAN_POINT('Ctrl Pts',(-2.79960031072545,3.00402491773169,-6.95851278007885));
#99279=CARTESIAN_POINT('Ctrl Pts',(-2.8127035348095,3.00629206936588,-6.95318348297372));
#99280=CARTESIAN_POINT('Ctrl Pts',(-2.82580675889353,3.008559221,-6.94785418586859));
#99281=CARTESIAN_POINT('Ctrl Pts',(-3.20581787129103,3.074309666,-6.79329740593167));
#99282=CARTESIAN_POINT('Ctrl Pts',(-3.5667056870988,3.139297275,-6.59821734858096));
#99283=CARTESIAN_POINT('Origin',(0.0581592152221827,2.94646401333924,0.18755850573811));
#99284=CARTESIAN_POINT('Ctrl Pts',(-1.756687991,3.13930489,-7.033956732));
#99285=CARTESIAN_POINT('Ctrl Pts',(-2.13928501,3.07388663,-6.93840544900001));
#99286=CARTESIAN_POINT('Ctrl Pts',(-2.509260865,3.008559221,-6.801919576));
#99287=CARTESIAN_POINT('Ctrl Pts',(-1.577649813,3.13930489,-7.332190741));
#99288=CARTESIAN_POINT('Ctrl Pts',(-1.976468632,3.07388663,-7.24637785700001));
#99289=CARTESIAN_POINT('Ctrl Pts',(-2.363626857,3.008559221,-7.11781343400001));
#99290=CARTESIAN_POINT('',(-1.76124628360345,3.13852541859317,-7.03281675504062));
#99291=CARTESIAN_POINT('Origin',(0.0563876163800928,3.08928612119298,0.191535565089408));
#99292=CARTESIAN_POINT('Ctrl Pts',(-1.82077719099447,3.09925366550455,-7.27562852393233));
#99293=CARTESIAN_POINT('Ctrl Pts',(-1.81080545823739,3.10549653066451,-7.23513176665341));
#99294=CARTESIAN_POINT('Ctrl Pts',(-1.80085250313915,3.11188594219304,-7.19462975998299));
#99295=CARTESIAN_POINT('Ctrl Pts',(-1.78101041491928,3.12496646786567,-7.11370501954715));
#99296=CARTESIAN_POINT('Ctrl Pts',(-1.7711106374316,3.13166459393754,-7.07323888725074));
#99297=CARTESIAN_POINT('Ctrl Pts',(-1.76124628168251,3.13852541820015,-7.03281675696655));
#99298=CARTESIAN_POINT('Ctrl Pts',(-0.961293304380143,3.00402491792402,
-7.18603945161995));
#99299=CARTESIAN_POINT('Ctrl Pts',(-0.974838699690071,3.00629206946205,
-7.18417542030998));
#99300=CARTESIAN_POINT('Ctrl Pts',(-0.988384095,3.008559221,-7.182311389));
#99301=CARTESIAN_POINT('Ctrl Pts',(-1.381218784,3.074309666,-7.128251973));
#99302=CARTESIAN_POINT('Ctrl Pts',(-1.765814248,3.139297275,-7.031671213));
#99303=CARTESIAN_POINT('Ctrl Pts',(-1.23827265637212,3.0040249179241,-7.39765792970278));
#99304=CARTESIAN_POINT('Ctrl Pts',(-1.25221517513604,3.00629206946205,-7.39527003453434));
#99305=CARTESIAN_POINT('Ctrl Pts',(-1.26615769389991,3.008559221,-7.39288213936585));
#99306=CARTESIAN_POINT('Ctrl Pts',(-1.67050949738474,3.074309666,-7.32362996662319));
#99307=CARTESIAN_POINT('Ctrl Pts',(-2.06489640124521,3.139297275,-7.2106909852025));
#99308=CARTESIAN_POINT('Origin',(0.0164799599938099,2.94646400269109,0.195676067964657));
#99309=CARTESIAN_POINT('Ctrl Pts',(-0.203524827,3.13930489,-7.24714272300001));
#99310=CARTESIAN_POINT('Ctrl Pts',(-0.597717642,3.07388663,-7.236072426));
#99311=CARTESIAN_POINT('Ctrl Pts',(-0.988384095,3.008559221,-7.182311389));
#99312=CARTESIAN_POINT('Ctrl Pts',(0.035439035,3.13930489,-7.499916271));
#99313=CARTESIAN_POINT('Ctrl Pts',(-0.372502856,3.07388663,-7.50184390200001));
#99314=CARTESIAN_POINT('Ctrl Pts',(-0.778247087,3.008559221,-7.459512817));
#99315=CARTESIAN_POINT('',(-0.20822160905804,3.13852541863702,-7.24700929639271));
#99316=CARTESIAN_POINT('Origin',(0.0138950876829804,3.08928569839221,0.19918167042057));
#99317=CARTESIAN_POINT('Ctrl Pts',(-0.214163364830849,3.09925366989869,
-7.4969416169044));
#99318=CARTESIAN_POINT('Ctrl Pts',(-0.213130371432416,3.10549653514307,
-7.45524802340234));
#99319=CARTESIAN_POINT('Ctrl Pts',(-0.212116845861233,3.11188594217775,
-7.41355336952049));
#99320=CARTESIAN_POINT('Ctrl Pts',(-0.210135086285302,3.1249664382743,-7.33025533037589));
#99321=CARTESIAN_POINT('Ctrl Pts',(-0.209165779932897,3.13166457940977,
-7.28860701383298));
#99322=CARTESIAN_POINT('Ctrl Pts',(-0.208221608534527,3.13852541825656,
-7.24700929713044));
#99323=CARTESIAN_POINT('Ctrl Pts',(0.589277982209245,3.00680105370404,-7.22601992003964));
#99324=CARTESIAN_POINT('Ctrl Pts',(0.583993199604623,3.00768013735202,-7.22644311151983));
#99325=CARTESIAN_POINT('Ctrl Pts',(0.578708417,3.008559221,-7.226866303));
#99326=CARTESIAN_POINT('Ctrl Pts',(0.183436808,3.074309666,-7.258518613));
#99327=CARTESIAN_POINT('Ctrl Pts',(-0.212929036,3.139297275,-7.246872513));
#99328=CARTESIAN_POINT('Ctrl Pts',(0.363937708262816,3.00680105370404,-7.49137623361797));
#99329=CARTESIAN_POINT('Ctrl Pts',(0.358459120241673,3.00768013735202,-7.4916343573119));
#99330=CARTESIAN_POINT('Ctrl Pts',(0.352980532220529,3.008559221,-7.49189248100584));
#99331=CARTESIAN_POINT('Ctrl Pts',(-0.0567866170036243,3.074309666,-7.51119866168644));
#99332=CARTESIAN_POINT('Ctrl Pts',(-0.466215022260595,3.139297275,-7.48569914997869));
#99333=CARTESIAN_POINT('Origin',(-0.0259698947464153,2.94646402789277,0.194643709377537));
#99334=CARTESIAN_POINT('Ctrl Pts',(1.359154932,3.13930489,-7.121460375));
#99335=CARTESIAN_POINT('Ctrl Pts',(0.971798339000001,3.07388663,-7.195388698));
#99336=CARTESIAN_POINT('Ctrl Pts',(0.578708417,3.008559221,-7.226866303));
#99337=CARTESIAN_POINT('Ctrl Pts',(1.646870792,3.13930489,-7.316954052));
#99338=CARTESIAN_POINT('Ctrl Pts',(1.24888074,3.07388663,-7.40653206300001));
#99339=CARTESIAN_POINT('Ctrl Pts',(0.843522651,3.008559221,-7.45241367199999));
#99340=CARTESIAN_POINT('',(1.3545392753172,3.13852541865081,-7.12233973722032));
#99341=CARTESIAN_POINT('Origin',(-0.0292476493493499,3.08928608977801,0.197509355480461));
#99342=CARTESIAN_POINT('Ctrl Pts',(1.40246450071478,3.0992536654408,-7.36770611019148));
#99343=CARTESIAN_POINT('Ctrl Pts',(1.39451038722841,3.10549658239958,-7.32676488706771));
#99344=CARTESIAN_POINT('Ctrl Pts',(1.3865371282657,3.11188596766313,-7.2858273040236));
#99345=CARTESIAN_POINT('Ctrl Pts',(1.37056594371818,3.12496646028372,-7.20405072874484));
#99346=CARTESIAN_POINT('Ctrl Pts',(1.36255944570165,3.13166459020175,-7.16316782787836));
#99347=CARTESIAN_POINT('Ctrl Pts',(1.35453927636302,3.13852541819903,-7.12233973829615));
#99348=CARTESIAN_POINT('Ctrl Pts',(2.14489347757516,3.00402491757735,-6.92550935161478));
#99349=CARTESIAN_POINT('Ctrl Pts',(2.13181732228758,3.00629206928867,-6.92950516680737));
#99350=CARTESIAN_POINT('Ctrl Pts',(2.118741167,3.008559221,-6.933500982));
#99351=CARTESIAN_POINT('Ctrl Pts',(1.739515099,3.074309666,-7.04938499));
#99352=CARTESIAN_POINT('Ctrl Pts',(1.349912501,3.139297275,-7.12321811));
#99353=CARTESIAN_POINT('Ctrl Pts',(1.9823701178637,3.00402491757735,-7.23386969212132));
#99354=CARTESIAN_POINT('Ctrl Pts',(1.96871357834968,3.00629206928867,-7.23755680916065));
#99355=CARTESIAN_POINT('Ctrl Pts',(1.95505703883561,3.008559221,-7.24124392619998));
#99356=CARTESIAN_POINT('Ctrl Pts',(1.55899904866107,3.074309666,-7.3481752730931));
#99357=CARTESIAN_POINT('Ctrl Pts',(1.15364134055402,3.139297275,-7.41127339163886));
#99358=CARTESIAN_POINT('Origin',(-0.0672054225525906,2.94646403236397,0.184510496212321));
#99359=CARTESIAN_POINT('Ctrl Pts',(2.858282117,3.13930489,-6.662786455));
#99360=CARTESIAN_POINT('Ctrl Pts',(2.49587411,3.07388663,-6.81825659200001));
#99361=CARTESIAN_POINT('Ctrl Pts',(2.118741167,3.008559221,-6.933500982));
#99362=CARTESIAN_POINT('Ctrl Pts',(3.181296702,3.13930489,-6.79185919300001));
#99363=CARTESIAN_POINT('Ctrl Pts',(2.81186806,3.07388663,-6.964899017));
#99364=CARTESIAN_POINT('Ctrl Pts',(2.425850208,3.008559221,-7.096847946));
#99365=CARTESIAN_POINT('',(2.85396340807885,3.13852541866625,-6.66463748776731));
#99366=CARTESIAN_POINT('Origin',(-0.0710225736237424,3.08928608316363,0.186604418638494));
#99367=CARTESIAN_POINT('Ctrl Pts',(2.9535146859888,3.0992536654475,-6.89396482448299));
#99368=CARTESIAN_POINT('Ctrl Pts',(2.93694538232829,3.10549658248996,-6.85569068315969));
#99369=CARTESIAN_POINT('Ctrl Pts',(2.92035816359901,3.11188596772589,-6.81742421322633));
#99370=CARTESIAN_POINT('Ctrl Pts',(2.8871808228278,3.12496646321178,-6.74099284469479));
#99371=CARTESIAN_POINT('Ctrl Pts',(2.87057290089434,3.13166459168363,-6.70278693262248));
#99372=CARTESIAN_POINT('Ctrl Pts',(2.85396340960551,3.13852541826454,-6.66463748835739));
#99373=CARTESIAN_POINT('Ctrl Pts',(3.58352685288815,3.00402491774724,-6.30250609728324));
#99374=CARTESIAN_POINT('Ctrl Pts',(3.5716153934441,3.00629206937366,-6.30921947914162));
#99375=CARTESIAN_POINT('Ctrl Pts',(3.559703934,3.008559221,-6.315932861));
#99376=CARTESIAN_POINT('Ctrl Pts',(3.214255597,3.074309666,-6.51062996));
#99377=CARTESIAN_POINT('Ctrl Pts',(2.84963363,3.139297275,-6.666489944));
#99378=CARTESIAN_POINT('Ctrl Pts',(3.49109155714461,3.00402491774723,-6.63859486252414));
#99379=CARTESIAN_POINT('Ctrl Pts',(3.47854692157417,3.00629206937366,-6.64513152886113));
#99380=CARTESIAN_POINT('Ctrl Pts',(3.46600228600367,3.008559221,-6.65166819519811));
#99381=CARTESIAN_POINT('Ctrl Pts',(3.10219099013011,3.074309666,-6.841240306511));
#99382=CARTESIAN_POINT('Ctrl Pts',(2.71987455123701,3.139297275,-6.9900031514952));
#99383=CARTESIAN_POINT('Origin',(-0.10529845987564,2.94646405132947,0.16574949656218));
#99384=CARTESIAN_POINT('Ctrl Pts',(4.223759206,3.13930489,-5.892568045));
#99385=CARTESIAN_POINT('Ctrl Pts',(3.903245582,3.07388663,-6.122310386));
#99386=CARTESIAN_POINT('Ctrl Pts',(3.559703934,3.008559221,-6.315932861));
#99387=CARTESIAN_POINT('Ctrl Pts',(4.566968713,3.13930489,-5.94918454700001));
#99388=CARTESIAN_POINT('Ctrl Pts',(4.243375555,3.07388663,-6.19759503400001));
#99389=CARTESIAN_POINT('Ctrl Pts',(3.894747705,3.008559221,-6.409441498));
#99390=CARTESIAN_POINT('',(4.21993938413285,3.13852541865766,-5.89530419657678));
#99391=CARTESIAN_POINT('Origin',(-0.109476389222967,3.08928612558317,0.166973696339344));
#99392=CARTESIAN_POINT('Ctrl Pts',(4.36646180685914,3.09925366547009,-6.09786940580673));
#99393=CARTESIAN_POINT('Ctrl Pts',(4.34205207570782,3.10549658240008,-6.06405200370254));
#99394=CARTESIAN_POINT('Ctrl Pts',(4.31762649685015,3.1118859676776,-6.0302459439873));
#99395=CARTESIAN_POINT('Ctrl Pts',(4.26879433194001,3.12496646502922,-5.96273363615785));
#99396=CARTESIAN_POINT('Ctrl Pts',(4.24436155596421,3.13166459254897,-5.92899117441959));
#99397=CARTESIAN_POINT('Ctrl Pts',(4.21993938576901,3.13852541822334,-5.89530419695904));
#99398=CARTESIAN_POINT('Ctrl Pts',(4.85459849685151,3.00402491777864,-5.38480466232962));
#99399=CARTESIAN_POINT('Ctrl Pts',(4.84440869942573,3.00629206938932,-5.3939217006648));
#99400=CARTESIAN_POINT('Ctrl Pts',(4.83421890200001,3.008559221,-5.403038739));
#99401=CARTESIAN_POINT('Ctrl Pts',(4.538701076,3.074309666,-5.66744510900001));
#99402=CARTESIAN_POINT('Ctrl Pts',(4.216109057,3.139297275,-5.898044118));
#99403=CARTESIAN_POINT('Ctrl Pts',(4.8365734368469,3.00402491777864,-5.73290671558476));
#99404=CARTESIAN_POINT('Ctrl Pts',(4.82572727799302,3.00629206938932,-5.74198728403669));
#99405=CARTESIAN_POINT('Ctrl Pts',(4.81488111913914,3.008559221,-5.75106785248864));
#99406=CARTESIAN_POINT('Ctrl Pts',(4.50032792921482,3.074309666,-6.01441654683934));
#99407=CARTESIAN_POINT('Ctrl Pts',(4.15892944979653,3.139297275,-6.24188813282856));
#99408=CARTESIAN_POINT('Origin',(-0.138467891961084,2.94646404519457,0.13923832246165));
#99409=CARTESIAN_POINT('Ctrl Pts',(5.39173801,3.13930489,-4.846819703));
#99410=CARTESIAN_POINT('Ctrl Pts',(5.128105628,3.07388663,-5.14009175));
#99411=CARTESIAN_POINT('Ctrl Pts',(4.834218902,3.008559221,-5.403038739));
#99412=CARTESIAN_POINT('Ctrl Pts',(5.739094344,3.13930489,-4.828332643));
#99413=CARTESIAN_POINT('Ctrl Pts',(5.476467525,3.07388663,-5.140498395));
#99414=CARTESIAN_POINT('Ctrl Pts',(5.181531129,3.008559221,-5.42233668900001));
#99415=CARTESIAN_POINT('',(5.38859568422891,3.13852541862581,-4.85031303434529));
#99416=CARTESIAN_POINT('Origin',(-0.142811494543745,3.08928612771913,0.139535953325501));
#99417=CARTESIAN_POINT('Ctrl Pts',(5.57523802689835,3.09925366543971,-5.0166443907419));
#99418=CARTESIAN_POINT('Ctrl Pts',(5.54412949788754,3.10549653059208,-4.9888652217637));
#99419=CARTESIAN_POINT('Ctrl Pts',(5.51300753522168,3.11188594214901,-4.96110018408167));
#99420=CARTESIAN_POINT('Ctrl Pts',(5.45080379357747,3.12496645952399,-4.90566366378266));
#99421=CARTESIAN_POINT('Ctrl Pts',(5.41968859661435,3.13166458985593,-4.87796239430588));
#99422=CARTESIAN_POINT('Ctrl Pts',(5.38859568661649,3.1385254182622,-4.85031303352164));
#99423=CARTESIAN_POINT('Ctrl Pts',(5.89867451036487,3.00402491759344,-4.21531574453703));
#99424=CARTESIAN_POINT('Ctrl Pts',(5.89068283818242,3.00629206929675,-4.22641013726852));
#99425=CARTESIAN_POINT('Ctrl Pts',(5.882691166,3.008559221,-4.23750453));
#99426=CARTESIAN_POINT('Ctrl Pts',(5.650921937,3.074309666,-4.559256823));
#99427=CARTESIAN_POINT('Ctrl Pts',(5.385443911,3.139297275,-4.853812304));
#99428=CARTESIAN_POINT('Ctrl Pts',(5.95590251824537,3.00402491759345,-4.55915422034929));
#99429=CARTESIAN_POINT('Ctrl Pts',(5.94726199003128,3.00629206929675,-4.57035409416915));
#99430=CARTESIAN_POINT('Ctrl Pts',(5.93862146181731,3.008559221,-4.58155396798899));
#99431=CARTESIAN_POINT('Ctrl Pts',(5.68803453625319,3.074309666,-4.90636535425118));
#99432=CARTESIAN_POINT('Ctrl Pts',(5.40351742967199,3.139297275,-5.20190936246538));
#99433=CARTESIAN_POINT('Origin',(-0.165164502112501,2.94646446502014,0.106218016553463));
#99434=CARTESIAN_POINT('Ctrl Pts',(6.307605137,3.13930489,-3.574439458));
#99435=CARTESIAN_POINT('Ctrl Pts',(6.113181154,3.07388663,-3.917528137));
#99436=CARTESIAN_POINT('Ctrl Pts',(5.882691166,3.008559221,-4.23750453));
#99437=CARTESIAN_POINT('Ctrl Pts',(6.64286630100001,3.13930489,-3.481713272));
#99438=CARTESIAN_POINT('Ctrl Pts',(6.453485961,3.07388663,-3.843037764));
#99439=CARTESIAN_POINT('Ctrl Pts',(6.226031915,3.008559221,-4.181689442));
#99440=CARTESIAN_POINT('',(6.30528723953085,3.13852541858252,-3.57852662505442));
#99441=CARTESIAN_POINT('Origin',(-0.169468734258327,3.08928610863066,0.105573437156782));
#99442=CARTESIAN_POINT('Ctrl Pts',(6.52332231319454,3.09925366544933,-3.70084665970846));
#99443=CARTESIAN_POINT('Ctrl Pts',(6.48696938400141,3.10549653060211,-3.68040436650827));
#99444=CARTESIAN_POINT('Ctrl Pts',(6.45060637303851,3.11188594215306,-3.65997876206266));
#99445=CARTESIAN_POINT('Ctrl Pts',(6.37793973874896,3.12496645377077,-3.61921030050866));
#99446=CARTESIAN_POINT('Ctrl Pts',(6.34159702665588,3.13166458699902,-3.59884550943043));
#99447=CARTESIAN_POINT('Ctrl Pts',(6.30528724135634,3.13852541819247,-3.5785266235761));
#99448=CARTESIAN_POINT('Ctrl Pts',(6.66693505965315,3.00402491762771,-2.84872334858325));
#99449=CARTESIAN_POINT('Ctrl Pts',(6.66151519482659,3.00629206931389,-2.8612763337916));
#99450=CARTESIAN_POINT('Ctrl Pts',(6.65609533,3.008559221,-2.873829319));
#99451=CARTESIAN_POINT('Ctrl Pts',(6.498911968,3.074309666,-3.237882756));
#99452=CARTESIAN_POINT('Ctrl Pts',(6.302961392,3.139297275,-3.582621622));
#99453=CARTESIAN_POINT('Ctrl Pts',(6.7967402167303,3.00402491762771,-3.17222074183296));
#99454=CARTESIAN_POINT('Ctrl Pts',(6.7907093411173,3.00629206931389,-3.18501622689353));
#99455=CARTESIAN_POINT('Ctrl Pts',(6.78467846550414,3.008559221,-3.19781171195412));
#99456=CARTESIAN_POINT('Ctrl Pts',(6.60977496975106,3.074309666,-3.56889797048598));
#99457=CARTESIAN_POINT('Ctrl Pts',(6.39544294078199,3.139297275,-3.91869509171463));
#99458=CARTESIAN_POINT('Origin',(-0.184134812493184,2.94646404232351,0.0682281691969916));
#99459=CARTESIAN_POINT('Ctrl Pts',(6.928535658,3.13930489,-2.134922397));
#99460=CARTESIAN_POINT('Ctrl Pts',(6.812411124,3.07388663,-2.511785262));
#99461=CARTESIAN_POINT('Ctrl Pts',(6.65609533,3.008559221,-2.873829319));
#99462=CARTESIAN_POINT('Ctrl Pts',(7.236025213,3.13930489,-1.972292858));
#99463=CARTESIAN_POINT('Ctrl Pts',(7.128746565,3.07388663,-2.365880959));
#99464=CARTESIAN_POINT('Ctrl Pts',(6.979410369,3.008559221,-2.745511045));
#99465=CARTESIAN_POINT('',(6.92715057170216,3.13852541858868,-2.13941228764284));
#99466=CARTESIAN_POINT('Origin',(-0.188201868409005,3.08928612478781,0.0666744331105723));
#99467=CARTESIAN_POINT('Ctrl Pts',(7.16638329785451,3.0992536654575,-2.21200145241879));
#99468=CARTESIAN_POINT('Ctrl Pts',(7.12648545168685,3.10549658374615,-2.1998517903871));
#99469=CARTESIAN_POINT('Ctrl Pts',(7.08658186675109,3.11188596832624,-2.18772075263819));
#99470=CARTESIAN_POINT('Ctrl Pts',(7.00685022097463,3.12496646406064,-2.16352664264606));
#99471=CARTESIAN_POINT('Ctrl Pts',(6.96697938663559,3.1316645920718,-2.1514505879326));
#99472=CARTESIAN_POINT('Ctrl Pts',(6.92715057360104,3.13852541822036,-2.13941228563729));
#99473=CARTESIAN_POINT('Ctrl Pts',(7.12345713528118,3.00402491764723,-1.34892781591291));
#99474=CARTESIAN_POINT('Ctrl Pts',(7.12086250464065,3.00629206932365,-1.36235242995646));
#99475=CARTESIAN_POINT('Ctrl Pts',(7.118267874,3.008559221,-1.375777044));
#99476=CARTESIAN_POINT('Ctrl Pts',(7.04302009900001,3.074309666,-1.76510889));
#99477=CARTESIAN_POINT('Ctrl Pts',(6.925759405,3.139297275,-2.143911534));
#99478=CARTESIAN_POINT('Ctrl Pts',(7.31976989663,3.00402491764723,-1.6369577478844));
#99479=CARTESIAN_POINT('Ctrl Pts',(7.3166306705952,3.00629206932366,-1.65075054153846));
#99480=CARTESIAN_POINT('Ctrl Pts',(7.3134914445603,3.008559221,-1.66454333519246));
#99481=CARTESIAN_POINT('Ctrl Pts',(7.22244967135065,3.074309666,-2.06455288462094));
#99482=CARTESIAN_POINT('Ctrl Pts',(7.08832464742211,3.139297275,-2.45224699367283));
#99483=CARTESIAN_POINT('Origin',(-0.194497013819791,2.94646404265204,0.0270495149303721));
#99484=CARTESIAN_POINT('Ctrl Pts',(7.225495552,3.13930489,-0.595578738));
#99485=CARTESIAN_POINT('Ctrl Pts',(7.193100321,3.07388663,-0.988594101));
#99486=CARTESIAN_POINT('Ctrl Pts',(7.118267874,3.008559221,-1.375777044));
#99487=CARTESIAN_POINT('Ctrl Pts',(7.490835629,3.13930489,-0.370650221));
#99488=CARTESIAN_POINT('Ctrl Pts',(7.47067490300001,3.07388663,-0.77809819));
#99489=CARTESIAN_POINT('Ctrl Pts',(7.406439351,3.008559221,-1.180955603));
#99490=CARTESIAN_POINT('',(7.22510804225623,3.13852541859739,-0.60026140928089));
#99491=CARTESIAN_POINT('Origin',(-0.198134895537586,3.08928611241096,0.0246577965307507));
#99492=CARTESIAN_POINT('Ctrl Pts',(7.47435216496847,3.0992536654315,-0.619725515399642));
#99493=CARTESIAN_POINT('Ctrl Pts',(7.43277529403877,3.10549658313059,-0.616436763639562));
#99494=CARTESIAN_POINT('Ctrl Pts',(7.39119681605539,3.11188596802581,-0.613167433926877));
#99495=CARTESIAN_POINT('Ctrl Pts',(7.30812831330693,3.12496645117645,-0.606678922198451));
#99496=CARTESIAN_POINT('Ctrl Pts',(7.26659359855861,3.13166458574274,-0.603456246411873));
#99497=CARTESIAN_POINT('Ctrl Pts',(7.22510804347203,3.13852541824124,-0.600261407597791));
#99498=CARTESIAN_POINT('Ctrl Pts',(7.2468942729035,3.00402491774289,0.213942082252785));
#99499=CARTESIAN_POINT('Ctrl Pts',(7.24724619845171,3.00629206937144,0.200273559626389));
#99500=CARTESIAN_POINT('Ctrl Pts',(7.247598124,3.008559221,0.186605037));
#99501=CARTESIAN_POINT('Ctrl Pts',(7.25780443800001,3.074309666,-0.209800494));
#99502=CARTESIAN_POINT('Ctrl Pts',(7.22471660500001,3.139297275,-0.604954526));
#99503=CARTESIAN_POINT('Ctrl Pts',(7.50053527194251,3.00402491774289,-0.0251524289314449));
#99504=CARTESIAN_POINT('Ctrl Pts',(7.50043448218546,3.00629206937144,-0.0392975952519484));
#99505=CARTESIAN_POINT('Ctrl Pts',(7.50033369242839,3.008559221,-0.0534427615724517));
#99506=CARTESIAN_POINT('Ctrl Pts',(7.49741065398017,3.074309666,-0.46367160046222));
#99507=CARTESIAN_POINT('Ctrl Pts',(7.4497641724016,3.139297275,-0.871134551944614));
#99508=CARTESIAN_POINT('Origin',(-0.195764717091161,2.94646402749331,-0.0153939945164652));
#99509=CARTESIAN_POINT('Ctrl Pts',(7.184599304,3.13930489,0.971613522));
#99510=CARTESIAN_POINT('Ctrl Pts',(7.237448142,3.07388663,0.580822623));
#99511=CARTESIAN_POINT('Ctrl Pts',(7.247598124,3.008559221,0.186605037));
#99512=CARTESIAN_POINT('Ctrl Pts',(7.395382895,3.13930489,1.248323608));
#99513=CARTESIAN_POINT('Ctrl Pts',(7.463282786,3.07388663,0.846067586));
#99514=CARTESIAN_POINT('Ctrl Pts',(7.487151461,3.008559221,0.43882001));
#99515=CARTESIAN_POINT('',(7.1852274901126,3.13852541864547,0.966957026736903));
#99516=CARTESIAN_POINT('Origin',(-0.198803195774695,3.08928614354635,-0.0185118389669156));
#99517=CARTESIAN_POINT('Ctrl Pts',(7.43282863154986,3.09925366549633,1.00152809855961));
#99518=CARTESIAN_POINT('Ctrl Pts',(7.39151716795886,3.10549653063858,0.995802211064652));
#99519=CARTESIAN_POINT('Ctrl Pts',(7.3502077780297,3.11188594216789,0.990056936559549));
#99520=CARTESIAN_POINT('Ctrl Pts',(7.2676863353547,3.12496645651863,0.978536450388539));
#99521=CARTESIAN_POINT('Ctrl Pts',(7.22642991707295,3.13166458834483,0.972755048399541));
#99522=CARTESIAN_POINT('Ctrl Pts',(7.18522749108296,3.13852541819917,0.966957027865251));
#99523=CARTESIAN_POINT('Ctrl Pts',(7.0314746878512,3.00402491773125,1.76680828720298));
#99524=CARTESIAN_POINT('Ctrl Pts',(7.03475671392561,3.00629206936566,1.75353498060149));
#99525=CARTESIAN_POINT('Ctrl Pts',(7.03803874,3.008559221,1.740261674));
#99526=CARTESIAN_POINT('Ctrl Pts',(7.133221908,3.074309666,1.35531794));
#99527=CARTESIAN_POINT('Ctrl Pts',(7.185854086,3.139297275,0.962289484));
#99528=CARTESIAN_POINT('Ctrl Pts',(7.3305839542102,3.00402491773132,1.5878289905596));
#99529=CARTESIAN_POINT('Ctrl Pts',(7.33352631350798,3.00629206936565,1.57399286353143));
#99530=CARTESIAN_POINT('Ctrl Pts',(7.33646867280563,3.008559221,1.5601567365032));
#99531=CARTESIAN_POINT('Ctrl Pts',(7.42180104768545,3.074309666,1.15889045356046));
#99532=CARTESIAN_POINT('Ctrl Pts',(7.46286100368629,3.139297275,0.750711174192357));
#99533=CARTESIAN_POINT('Origin',(-0.187878458688848,2.94646404251924,-0.0571176862107536));
#99534=CARTESIAN_POINT('Ctrl Pts',(6.807759179,3.13930489,2.493374213));
#99535=CARTESIAN_POINT('Ctrl Pts',(6.943380931,3.07388663,2.123080726));
#99536=CARTESIAN_POINT('Ctrl Pts',(7.03803874,3.008559221,1.740261674));
#99537=CARTESIAN_POINT('Ctrl Pts',(6.954130278,3.13930489,2.808927212));
#99538=CARTESIAN_POINT('Ctrl Pts',(7.10691586000001,3.07388663,2.430672182));
#99539=CARTESIAN_POINT('Ctrl Pts',(7.21777269,3.008559221,2.038076888));
#99540=CARTESIAN_POINT('',(6.80937368675612,3.13852541865695,2.48896162520118));
#99541=CARTESIAN_POINT('Origin',(-0.190175948613255,3.08928616020992,-0.0608158988611399));
#99542=CARTESIAN_POINT('Ctrl Pts',(7.0437542927345,3.09925366545663,2.57595137079219));
#99543=CARTESIAN_POINT('Ctrl Pts',(7.0046395647728,3.10549653061555,2.56147860792988));
#99544=CARTESIAN_POINT('Ctrl Pts',(6.96553102956378,3.11188594217194,2.54698735705091));
#99545=CARTESIAN_POINT('Ctrl Pts',(6.88741540061047,3.1249664658905,2.51799652197818));
#99546=CARTESIAN_POINT('Ctrl Pts',(6.84836639463171,3.13166459299201,2.50348138654226));
#99547=CARTESIAN_POINT('Ctrl Pts',(6.80937368765278,3.13852541825584,2.48896162659276));
#99548=CARTESIAN_POINT('Ctrl Pts',(6.4872711614844,3.00402491769784,3.23706050114662));
#99549=CARTESIAN_POINT('Ctrl Pts',(6.49332982424221,3.00629206934896,3.22480305557334));
#99550=CARTESIAN_POINT('Ctrl Pts',(6.499388487,3.008559221,3.21254561));
#99551=CARTESIAN_POINT('Ctrl Pts',(6.67509785,3.074309666,2.857063214));
#99552=CARTESIAN_POINT('Ctrl Pts',(6.810989017,3.139297275,2.484537907));
#99553=CARTESIAN_POINT('Ctrl Pts',(6.81786267768776,3.00402491769792,3.12656529035612));
#99554=CARTESIAN_POINT('Ctrl Pts',(6.82371060462596,3.00629206934896,3.11368516447345));
#99555=CARTESIAN_POINT('Ctrl Pts',(6.82955853156421,3.008559221,3.10080503859081));
#99556=CARTESIAN_POINT('Ctrl Pts',(6.99915627256187,3.074309666,2.72726407671965));
#99557=CARTESIAN_POINT('Ctrl Pts',(7.12700274973683,3.139297275,2.33745447873579));
#99558=CARTESIAN_POINT('Origin',(-0.171207237288136,2.94646404933259,-0.0961705711161648));
#99559=CARTESIAN_POINT('Ctrl Pts',(6.1125958,3.13930489,3.898547497));
#99560=CARTESIAN_POINT('Ctrl Pts',(6.324648946,3.07388663,3.566065933));
#99561=CARTESIAN_POINT('Ctrl Pts',(6.499388487,3.008559221,3.21254561));
#99562=CARTESIAN_POINT('Ctrl Pts',(6.18771025700001,3.13930489,4.238188502));
#99563=CARTESIAN_POINT('Ctrl Pts',(6.418237448,3.07388663,3.901621248));
#99564=CARTESIAN_POINT('Ctrl Pts',(6.61089889,3.008559221,3.542035555));
#99565=CARTESIAN_POINT('',(6.11512113789756,3.13852541863676,3.89458514483244));
#99566=CARTESIAN_POINT('Origin',(-0.172655948838892,3.08928607379705,-0.100276158918187));
#99567=CARTESIAN_POINT('Ctrl Pts',(6.32532183146937,3.09925366549066,4.02992602048575));
#99568=CARTESIAN_POINT('Ctrl Pts',(6.2902328002514,3.10549653065328,4.00738311236375));
#99569=CARTESIAN_POINT('Ctrl Pts',(6.25515379151119,3.1118859421876,3.98482347979379));
#99570=CARTESIAN_POINT('Ctrl Pts',(6.18509676441884,3.1249664417325,3.93971796624069));
#99571=CARTESIAN_POINT('Ctrl Pts',(6.15008095873197,3.13166458108201,3.91714776028921));
#99572=CARTESIAN_POINT('Ctrl Pts',(6.11512113813432,3.13852541820545,3.89458514567334));
#99573=CARTESIAN_POINT('Ctrl Pts',(5.63973004598923,3.00402491772892,4.55595136266774));
#99574=CARTESIAN_POINT('Ctrl Pts',(5.64828204899462,3.00629206936446,4.54528292283387));
#99575=CARTESIAN_POINT('Ctrl Pts',(5.656834052,3.008559221,4.534614483));
#99576=CARTESIAN_POINT('Ctrl Pts',(5.90485363500001,3.074309666,4.225215387));
#99577=CARTESIAN_POINT('Ctrl Pts',(6.117649671,3.139297275,3.890612098));
#99578=CARTESIAN_POINT('Ctrl Pts',(5.98634572077683,3.00402491772885,4.51910687246945));
#99579=CARTESIAN_POINT('Ctrl Pts',(5.99482577269543,3.00629206936446,4.5077850082868));
#99580=CARTESIAN_POINT('Ctrl Pts',(6.00330582461399,3.008559221,4.49646314410407));
#99581=CARTESIAN_POINT('Ctrl Pts',(6.24923872937746,3.074309666,4.16811386363588));
#99582=CARTESIAN_POINT('Ctrl Pts',(6.45789376755824,3.139297275,3.81490101079385));
#99583=CARTESIAN_POINT('Origin',(-0.146530587758711,2.94646404338753,-0.13072658550779));
#99584=CARTESIAN_POINT('Ctrl Pts',(5.131614236,3.13930489,5.121429033));
#99585=CARTESIAN_POINT('Ctrl Pts',(5.410183404,3.07388663,4.842305862));
#99586=CARTESIAN_POINT('Ctrl Pts',(5.65683405200001,3.008559221,4.534614483));
#99587=CARTESIAN_POINT('Ctrl Pts',(5.131959782,3.13930489,5.469276808));
#99588=CARTESIAN_POINT('Ctrl Pts',(5.429449386,3.07388663,5.190134841));
#99589=CARTESIAN_POINT('Ctrl Pts',(5.694906805,3.008559221,4.880372576));
#99590=CARTESIAN_POINT('',(5.13493232112406,3.13852541864172,5.11810219084313));
#99591=CARTESIAN_POINT('Origin',(-0.147063037517937,3.08928614843898,-0.135047780559689));
#99592=CARTESIAN_POINT('Ctrl Pts',(5.31112435157406,3.09925366548821,5.29546580809369));
#99593=CARTESIAN_POINT('Ctrl Pts',(5.28170174133006,3.105496530638,5.26590683617213));
#99594=CARTESIAN_POINT('Ctrl Pts',(5.25229251438716,3.11188594219092,5.23633368521849));
#99595=CARTESIAN_POINT('Ctrl Pts',(5.19356970549456,3.12496644806188,5.17722249498176));
#99596=CARTESIAN_POINT('Ctrl Pts',(5.16422449209147,3.13166458422919,5.14765261981693));
#99597=CARTESIAN_POINT('Ctrl Pts',(5.13493232125686,3.13852541826792,5.11810219192745));
#99598=CARTESIAN_POINT('Ctrl Pts',(4.52848142132521,3.00402491763025,5.66181100194064));
#99599=CARTESIAN_POINT('Ctrl Pts',(4.53912688266261,3.00629206931516,5.65323041197036));
#99600=CARTESIAN_POINT('Ctrl Pts',(4.549772344,3.008559221,5.644649822));
#99601=CARTESIAN_POINT('Ctrl Pts',(4.85850502600001,3.074309666,5.395801184));
#99602=CARTESIAN_POINT('Ctrl Pts',(5.138255826,3.139297275,5.114765592));
#99603=CARTESIAN_POINT('Ctrl Pts',(4.87491389009784,3.00402491763025,5.70034004019262));
#99604=CARTESIAN_POINT('Ctrl Pts',(4.88562954947645,3.00629206931516,5.69110583519945));
#99605=CARTESIAN_POINT('Ctrl Pts',(4.89634520885503,3.008559221,5.68187163020624));
#99606=CARTESIAN_POINT('Ctrl Pts',(5.20711372836752,3.074309666,5.41406727834801));
#99607=CARTESIAN_POINT('Ctrl Pts',(5.48682085039762,3.139297275,5.11396701104593));
#99608=CARTESIAN_POINT('Origin',(-0.11500256774619,2.94646401003658,-0.159170189428783));
#99609=CARTESIAN_POINT('Ctrl Pts',(3.910684093,3.13930489,6.104838239));
#99610=CARTESIAN_POINT('Ctrl Pts',(4.2427437,3.07388663,5.89212495));
#99611=CARTESIAN_POINT('Ctrl Pts',(4.549772344,3.008559221,5.644649822));
#99612=CARTESIAN_POINT('Ctrl Pts',(3.836244571,3.13930489,6.444627809));
#99613=CARTESIAN_POINT('Ctrl Pts',(4.186786305,3.07388663,6.235963497));
#99614=CARTESIAN_POINT('Ctrl Pts',(4.512627207,3.008559221,5.9905088));
#99615=CARTESIAN_POINT('',(3.91463977674163,3.1385254186077,6.10230246674704));
#99616=CARTESIAN_POINT('Origin',(-0.11459335387161,3.08928615979693,-0.163504429968793));
#99617=CARTESIAN_POINT('Ctrl Pts',(4.04858459986334,3.09925366545567,6.31339549972613));
#99618=CARTESIAN_POINT('Ctrl Pts',(4.02620398819062,3.10549658386035,6.27820230864598));
#99619=CARTESIAN_POINT('Ctrl Pts',(4.00383978723332,3.11188596840282,6.24299860631463));
#99620=CARTESIAN_POINT('Ctrl Pts',(3.95919710098266,3.12496645742458,6.17264582573996));
#99621=CARTESIAN_POINT('Ctrl Pts',(3.93689462839475,3.13166458883223,6.13745895129201));
#99622=CARTESIAN_POINT('Ctrl Pts',(3.91463977556472,3.1385254182671,6.10230246879974));
#99623=CARTESIAN_POINT('Ctrl Pts',(3.20548603911016,3.00402491768037,6.50293065189639));
#99624=CARTESIAN_POINT('Ctrl Pts',(3.21772718855505,3.00629206934018,6.49683913094818));
#99625=CARTESIAN_POINT('Ctrl Pts',(3.229968338,3.008559221,6.49074761));
#99626=CARTESIAN_POINT('Ctrl Pts',(3.584978123,3.074309666,6.31408531600001));
#99627=CARTESIAN_POINT('Ctrl Pts',(3.918602849,3.139297275,6.099758332));
#99628=CARTESIAN_POINT('Ctrl Pts',(3.53553650510488,3.00402491768037,6.61503164296334));
#99629=CARTESIAN_POINT('Ctrl Pts',(3.54798671931566,3.00629206934018,6.60831687860393));
#99630=CARTESIAN_POINT('Ctrl Pts',(3.56043693352648,3.008559221,6.60160211424467));
#99631=CARTESIAN_POINT('Ctrl Pts',(3.92150987770271,3.074309666,6.40686492373528));
#99632=CARTESIAN_POINT('Ctrl Pts',(4.25919028778872,3.139297275,6.17390959721214));
#99633=CARTESIAN_POINT('Origin',(-0.0780968644948271,2.94646402648455,-0.180170798700373));
#99634=CARTESIAN_POINT('Ctrl Pts',(2.506894708,3.13930489,6.802791995));
#99635=CARTESIAN_POINT('Ctrl Pts',(2.876918016,3.07388663,6.666434823));
#99636=CARTESIAN_POINT('Ctrl Pts',(3.229968338,3.008559221,6.49074761));
#99637=CARTESIAN_POINT('Ctrl Pts',(2.361150828,3.13930489,7.118635176));
#99638=CARTESIAN_POINT('Ctrl Pts',(2.748353749,3.07388663,6.990205431));
#99639=CARTESIAN_POINT('Ctrl Pts',(3.119342177,3.008559221,6.820535491));
#99640=CARTESIAN_POINT('',(2.51130302525059,3.13852541863486,6.8011658629826));
#99641=CARTESIAN_POINT('Origin',(-0.0767657578311959,3.0892861107107,-0.184316315789026));
#99642=CARTESIAN_POINT('Ctrl Pts',(2.59673753170469,3.09925366545958,7.03611783518109));
#99643=CARTESIAN_POINT('Ctrl Pts',(2.58244578398988,3.10549653063277,6.99693660543637));
#99644=CARTESIAN_POINT('Ctrl Pts',(2.56817213627037,3.11188594218907,6.95774812676784));
#99645=CARTESIAN_POINT('Ctrl Pts',(2.53969691770555,3.12496644121774,6.87944323712604));
#99646=CARTESIAN_POINT('Ctrl Pts',(2.52547998361091,3.13166458086886,6.84028458819026));
#99647=CARTESIAN_POINT('Ctrl Pts',(2.51130302490646,3.13852541827308,6.80116586366728));
#99648=CARTESIAN_POINT('Ctrl Pts',(1.73260569247021,3.00402491780393,7.0399804913979));
#99649=CARTESIAN_POINT('Ctrl Pts',(1.74587014723511,3.00629206940196,7.03666287219902));
#99650=CARTESIAN_POINT('Ctrl Pts',(1.759134602,3.008559221,7.033345253));
#99651=CARTESIAN_POINT('Ctrl Pts',(2.143821627,3.074309666,6.93712983500001));
#99652=CARTESIAN_POINT('Ctrl Pts',(2.515720358,3.139297275,6.79953315100001));
#99653=CARTESIAN_POINT('Ctrl Pts',(2.03084136254015,3.00402491780392,7.22041171771373));
#99654=CARTESIAN_POINT('Ctrl Pts',(2.04444397313732,3.00629206940197,7.21653036895605));
#99655=CARTESIAN_POINT('Ctrl Pts',(2.05804658373455,3.008559221,7.21264902019841));
#99656=CARTESIAN_POINT('Ctrl Pts',(2.4525405825932,3.074309666,7.1000846869461));
#99657=CARTESIAN_POINT('Ctrl Pts',(2.83240472211033,3.139297275,6.94516703341138));
#99658=CARTESIAN_POINT('Origin',(-0.0375396041755813,2.94646404903966,-0.192746987544548));
#99659=CARTESIAN_POINT('Ctrl Pts',(0.985885713,3.13930489,7.182654757));
#99660=CARTESIAN_POINT('Ctrl Pts',(1.376570843,3.07388663,7.129029614));
#99661=CARTESIAN_POINT('Ctrl Pts',(1.759134602,3.008559221,7.033345253));
#99662=CARTESIAN_POINT('Ctrl Pts',(0.775652296,3.13930489,7.459783074));
#99663=CARTESIAN_POINT('Ctrl Pts',(1.181411227,3.07388663,7.417593128));
#99664=CARTESIAN_POINT('Ctrl Pts',(1.580200173,3.008559221,7.331641522));
#99665=CARTESIAN_POINT('',(0.990540537957797,3.13852541858696,7.18201430105442));
#99666=CARTESIAN_POINT('Origin',(-0.0353484116042134,3.08928611100659,-0.196509256625923));
#99667=CARTESIAN_POINT('Ctrl Pts',(1.02346990277173,3.09925366544172,7.42983912041204));
#99668=CARTESIAN_POINT('Ctrl Pts',(1.01793509438376,3.10549653059944,7.38850162286539));
#99669=CARTESIAN_POINT('Ctrl Pts',(1.01241952112971,3.11188594212621,7.34716093692004));
#99670=CARTESIAN_POINT('Ctrl Pts',(1.00144325721373,3.12496646100666,7.26456531650114));
#99671=CARTESIAN_POINT('Ctrl Pts',(0.995976668043184,3.13166459052523,7.22326602139092));
#99672=CARTESIAN_POINT('Ctrl Pts',(0.99054053586425,3.13852541814021,7.18201430276513));
#99673=CARTESIAN_POINT('Ctrl Pts',(0.178710629076645,3.00402491789854,7.24784866891218));
#99674=CARTESIAN_POINT('Ctrl Pts',(0.192378158038323,3.0062920694493,7.24746007945602));
#99675=CARTESIAN_POINT('Ctrl Pts',(0.206045687,3.008559221,7.24707149000001));
#99676=CARTESIAN_POINT('Ctrl Pts',(0.602422414,3.074309666,7.235801873));
#99677=CARTESIAN_POINT('Ctrl Pts',(0.99520558,3.139297275,7.181369358));
#99678=CARTESIAN_POINT('Ctrl Pts',(0.431186334731839,3.00402491789854,7.48817336586714));
#99679=CARTESIAN_POINT('Ctrl Pts',(0.445305298819396,3.0062920694493,7.48730692008476));
#99680=CARTESIAN_POINT('Ctrl Pts',(0.45942426290696,3.008559221,7.48644047430236));
#99681=CARTESIAN_POINT('Ctrl Pts',(0.868893215879408,3.074309666,7.461312380972));
#99682=CARTESIAN_POINT('Ctrl Pts',(1.27317905962692,3.139297275,7.3916761777119));
#99683=CARTESIAN_POINT('Origin',(0.00477268321224331,2.94646447851623,-0.196313054001395));
#99684=CARTESIAN_POINT('Ctrl Pts',(-0.581222202,3.13930489,7.226664566));
#99685=CARTESIAN_POINT('Ctrl Pts',(-0.188143253,3.07388663,7.258278904));
#99686=CARTESIAN_POINT('Ctrl Pts',(0.206045687,3.008559221,7.24707149000001));
#99687=CARTESIAN_POINT('Ctrl Pts',(-0.846114875,3.13930489,7.452119807));
#99688=CARTESIAN_POINT('Ctrl Pts',(-0.440772771,3.07388663,7.498142414));
#99689=CARTESIAN_POINT('Ctrl Pts',(-0.032830234,3.008559221,7.499928145));
#99690=CARTESIAN_POINT('Origin',(0.0077217778851673,3.08928625812933,-0.199516394736223));
#99691=CARTESIAN_POINT('Ctrl Pts',(0.214081497,2.75,7.24683856));
#99692=CARTESIAN_POINT('Ctrl Pts',(0.606773411,2.81435393,7.235237905));
#99693=CARTESIAN_POINT('Ctrl Pts',(0.995912368,2.879481221,7.181271375));
#99694=CARTESIAN_POINT('Ctrl Pts',(0.467202875,2.75,7.485433954));
#99695=CARTESIAN_POINT('Ctrl Pts',(0.872823804,2.81435393,7.46011715000001));
#99696=CARTESIAN_POINT('Ctrl Pts',(1.27333392,2.879481221,7.391117691));
#99697=CARTESIAN_POINT('',(0.467202886311634,2.75,7.48543395315807));
#99698=CARTESIAN_POINT('',(1.02739270828442,2.83963938427222,7.42929769337341));
#99699=CARTESIAN_POINT('Origin',(-0.0426544601547765,2.94636923496794,-0.183656325683895));
#99700=CARTESIAN_POINT('Ctrl Pts',(0.991263375807224,2.87870320272917,7.181914572441));
#99701=CARTESIAN_POINT('Ctrl Pts',(0.997239354637858,2.87185457193071,7.22308853581347));
#99702=CARTESIAN_POINT('Ctrl Pts',(1.00324258046769,2.86518067056541,7.26431437598536));
#99703=CARTESIAN_POINT('Ctrl Pts',(1.01528456492317,2.8521708113185,7.34676107373081));
#99704=CARTESIAN_POINT('Ctrl Pts',(1.02133053850809,2.84582706798436,7.38803131637516));
#99705=CARTESIAN_POINT('Ctrl Pts',(1.02739270989943,2.8396393842762,7.42929769313675));
#99706=CARTESIAN_POINT('',(0.340642197483777,2.74999999814853,7.36613625646894));
#99707=CARTESIAN_POINT('Origin',(1.68756068147369E-13,2.84071505699956,
1.43158054854986E-12));
#99708=CARTESIAN_POINT('',(1.02739270828441,2.66036061572777,7.42929769337331));
#99709=CARTESIAN_POINT('Origin',(-0.0426544601514964,2.55363076502388,-0.183656325612771));
#99710=CARTESIAN_POINT('',(1.58832892548214,2.75,7.32988480226283));
#99711=CARTESIAN_POINT('Ctrl Pts',(1.58832892514213,2.75000000173941,7.32988480199432));
#99712=CARTESIAN_POINT('Ctrl Pts',(1.44013430592371,2.72598918212329,7.36199742168401));
#99713=CARTESIAN_POINT('Ctrl Pts',(1.29133537739194,2.70215892392441,7.3895315483916));
#99714=CARTESIAN_POINT('Ctrl Pts',(1.14235084253717,2.6785714288812,7.41249179069507));
#99715=CARTESIAN_POINT('Ctrl Pts',(1.1041082303364,2.67251679083289,7.41838542008151));
#99716=CARTESIAN_POINT('Ctrl Pts',(1.06578665338603,2.66644617724574,7.42398821998536));
#99717=CARTESIAN_POINT('Ctrl Pts',(1.02739270835229,2.66036061551156,7.42929769361639));
#99718=CARTESIAN_POINT('Ctrl Pts',(1.0273927083523,2.83963938448845,7.42929769361639));
#99719=CARTESIAN_POINT('Ctrl Pts',(1.06578665338584,2.83355382275425,7.42398821998572));
#99720=CARTESIAN_POINT('Ctrl Pts',(1.10410823026581,2.82748320916963,7.41838542016399));
#99721=CARTESIAN_POINT('Ctrl Pts',(1.14235084253684,2.8214285711188,7.41249179069551));
#99722=CARTESIAN_POINT('Ctrl Pts',(1.2913353776657,2.79784107606577,7.38953154807236));
#99723=CARTESIAN_POINT('Ctrl Pts',(1.44013430592352,2.77401081787668,7.36199742168431));
#99724=CARTESIAN_POINT('Ctrl Pts',(1.58832892514213,2.74999999826059,7.32988480199431));
#99725=CARTESIAN_POINT('Ctrl Pts',(0.986554849,2.879480225,7.18256288));
#99726=CARTESIAN_POINT('Ctrl Pts',(1.163317088,2.85030975,7.158283853));
#99727=CARTESIAN_POINT('Ctrl Pts',(1.338671059,2.821428571,7.125339276));
#99728=CARTESIAN_POINT('Ctrl Pts',(1.554222808,2.785926731,7.08484255300001));
#99729=CARTESIAN_POINT('Ctrl Pts',(1.766932466,2.75,7.031390308));
#99730=CARTESIAN_POINT('Ctrl Pts',(1.77080069057172,2.74934665560115,7.03041825393595));
#99731=CARTESIAN_POINT('Ctrl Pts',(1.77466891514343,2.7486933112023,7.02944619987189));
#99732=CARTESIAN_POINT('Ctrl Pts',(0.77634725,2.879480225,7.459710782));
#99733=CARTESIAN_POINT('Ctrl Pts',(0.959930074,2.85030975,7.440604944));
#99734=CARTESIAN_POINT('Ctrl Pts',(1.142350843,2.821428571,7.412491791));
#99735=CARTESIAN_POINT('Ctrl Pts',(1.366589369,2.785926731,7.377934037));
#99736=CARTESIAN_POINT('Ctrl Pts',(1.588328914,2.75,7.329884805));
#99737=CARTESIAN_POINT('Ctrl Pts',(1.59236135128825,2.74934665560115,7.32901100725324));
#99738=CARTESIAN_POINT('Ctrl Pts',(1.5963937885765,2.7486933112023,7.32813720950648));
#99739=CARTESIAN_POINT('',(1.67763070119454,2.75000000185147,7.18063755388459));
#99740=CARTESIAN_POINT('Ctrl Pts',(1.766932466,2.75,7.031390308));
#99741=CARTESIAN_POINT('Ctrl Pts',(2.147949663,2.81435393,6.935643716));
#99742=CARTESIAN_POINT('Ctrl Pts',(2.516389559,2.879481221,6.79928552));
#99743=CARTESIAN_POINT('Ctrl Pts',(2.065426964,2.75,7.20999386));
#99744=CARTESIAN_POINT('Ctrl Pts',(2.456122336,2.81435393,7.098072439));
#99745=CARTESIAN_POINT('Ctrl Pts',(2.832435904,2.879481221,6.944588314));
#99746=CARTESIAN_POINT('',(2.06542697487382,2.75,7.20999385677276));
#99747=CARTESIAN_POINT('',(2.60045223338147,2.83963938432456,7.03474577907832));
#99748=CARTESIAN_POINT('Origin',(-0.0811379622534811,2.94636923733788,-0.170193277971202));
#99749=CARTESIAN_POINT('Ctrl Pts',(2.51198752654408,2.87870320280854,6.80091307558165));
#99750=CARTESIAN_POINT('Ctrl Pts',(2.52667497498449,2.87185457194135,6.8398397562541));
#99751=CARTESIAN_POINT('Ctrl Pts',(2.54140018575414,2.86518067050631,6.8788112436685));
#99752=CARTESIAN_POINT('Ctrl Pts',(2.57088423815875,2.85217081128638,6.95674171291582));
#99753=CARTESIAN_POINT('Ctrl Pts',(2.58566074252707,2.84582706798929,6.99574737455167));
#99754=CARTESIAN_POINT('Ctrl Pts',(2.60045223490396,2.83963938432854,7.03474577850149));
#99755=CARTESIAN_POINT('',(1.91617972610113,2.74999999814853,7.12069208101268));
#99756=CARTESIAN_POINT('Origin',(3.25043811311154E-13,2.84071505699967,
9.72312508285E-13));
#99757=CARTESIAN_POINT('',(2.60045223338141,2.66036061567541,7.03474577907809));
#99758=CARTESIAN_POINT('Origin',(-0.081137962209949,2.55363076264363,-0.170193277808389));
#99759=CARTESIAN_POINT('',(3.12690324058091,2.75,6.81707240076085));
#99760=CARTESIAN_POINT('Ctrl Pts',(3.12690324023566,2.7500000017394,6.81707240066876));
#99761=CARTESIAN_POINT('Ctrl Pts',(2.98907659225498,2.72598918212324,6.88029170751296));
#99762=CARTESIAN_POINT('Ctrl Pts',(2.84967552346095,2.70215892392428,6.93916947253795));
#99763=CARTESIAN_POINT('Ctrl Pts',(2.7091099382986,2.67857142886255,6.99362018802513));
#99764=CARTESIAN_POINT('Ctrl Pts',(2.67302837304287,2.67251679079023,7.00759705909646));
#99765=CARTESIAN_POINT('Ctrl Pts',(2.63680716970682,2.66644617720861,7.02130687482412));
#99766=CARTESIAN_POINT('Ctrl Pts',(2.60045223349521,2.66036061545778,7.03474577928741));
#99767=CARTESIAN_POINT('Ctrl Pts',(2.6004522334952,2.83963938454222,7.03474577928741));
#99768=CARTESIAN_POINT('Ctrl Pts',(2.63680716970653,2.83355382279137,7.02130687482507));
#99769=CARTESIAN_POINT('Ctrl Pts',(2.67302837322312,2.82748320918882,7.00759705891095));
#99770=CARTESIAN_POINT('Ctrl Pts',(2.70910993830944,2.82142857113746,6.99362018799814));
#99771=CARTESIAN_POINT('Ctrl Pts',(2.84967552281257,2.79784107615723,6.93916947312821));
#99772=CARTESIAN_POINT('Ctrl Pts',(2.9890765922547,2.77401081787686,6.88029170751378));
#99773=CARTESIAN_POINT('Ctrl Pts',(3.12690324023566,2.7499999982606,6.81707240066876));
#99774=CARTESIAN_POINT('Ctrl Pts',(2.507528449,2.879480225,6.802558422));
#99775=CARTESIAN_POINT('Ctrl Pts',(2.674938811,2.85030975,6.740848368));
#99776=CARTESIAN_POINT('Ctrl Pts',(2.839110994,2.821428571,6.670978097));
#99777=CARTESIAN_POINT('Ctrl Pts',(3.040917665,2.785926731,6.58509091));
#99778=CARTESIAN_POINT('Ctrl Pts',(3.237163637,2.75,6.48716206));
#99779=CARTESIAN_POINT('Ctrl Pts',(3.24073246174509,2.74934665560115,6.48538117808137));
#99780=CARTESIAN_POINT('Ctrl Pts',(3.24430128649018,2.7486933112023,6.48360029616274));
#99781=CARTESIAN_POINT('Ctrl Pts',(2.361813993,2.879480225,7.118415179));
#99782=CARTESIAN_POINT('Ctrl Pts',(2.536997563,2.85030975,7.060291145));
#99783=CARTESIAN_POINT('Ctrl Pts',(2.709109939,2.821428571,6.993620188));
#99784=CARTESIAN_POINT('Ctrl Pts',(2.920676996,2.785926731,6.911665721));
#99785=CARTESIAN_POINT('Ctrl Pts',(3.12690323,2.75,6.817072406));
#99786=CARTESIAN_POINT('Ctrl Pts',(3.1306535504753,2.74934665560115,6.8153521823447));
#99787=CARTESIAN_POINT('Ctrl Pts',(3.13440387095059,2.7486933112023,6.8136319586894));
#99788=CARTESIAN_POINT('',(3.18203344387054,2.75000000185146,6.65211722803926));
#99789=CARTESIAN_POINT('Ctrl Pts',(3.237163637,2.75,6.48716206));
#99790=CARTESIAN_POINT('Ctrl Pts',(3.588690177,2.81435393,6.311746536));
#99791=CARTESIAN_POINT('Ctrl Pts',(3.919203171,2.879481221,6.099372632));
#99792=CARTESIAN_POINT('Ctrl Pts',(3.567073983,2.75,6.597422466));
#99793=CARTESIAN_POINT('Ctrl Pts',(3.924575317,2.81435393,6.40412975));
#99794=CARTESIAN_POINT('Ctrl Pts',(4.259096333,2.879481221,6.173337705));
#99795=CARTESIAN_POINT('',(3.56707399302919,2.75,6.59742246070181));
#99796=CARTESIAN_POINT('',(4.05191750198777,2.83963938428845,6.31125697077989));
#99797=CARTESIAN_POINT('Origin',(-0.115827529813538,2.94636920761577,-0.148772020898219));
#99798=CARTESIAN_POINT('Ctrl Pts',(3.9152539318276,2.87870320278185,6.10190844318095));
#99799=CARTESIAN_POINT('Ctrl Pts',(3.93796608157822,2.87185457197069,6.1367676721412));
#99800=CARTESIAN_POINT('Ctrl Pts',(3.96072474276779,2.86518067058185,6.17166254250291));
#99801=CARTESIAN_POINT('Ctrl Pts',(4.00627222155147,2.85217081136344,6.24143284080794));
#99802=CARTESIAN_POINT('Ctrl Pts',(4.02908832386645,2.84582706798215,6.27635006047718));
#99803=CARTESIAN_POINT('Ctrl Pts',(4.05191750339012,2.83963938429247,6.31125696986346));
#99804=CARTESIAN_POINT('',(3.40211882019941,2.74999999814853,6.54229225769611));
#99805=CARTESIAN_POINT('Origin',(1.66750294128271E-13,2.84071505700011,
1.39645239816133E-13));
#99806=CARTESIAN_POINT('',(4.05191750198764,2.66036061571151,6.31125697077964));
#99807=CARTESIAN_POINT('Origin',(-0.115827529770104,2.55363079237376,-0.14877202081415));
#99808=CARTESIAN_POINT('',(4.51926703516983,2.75,5.98550127055907));
#99809=CARTESIAN_POINT('Ctrl Pts',(4.51926703485033,2.75000000173941,5.98550127059301));
#99810=CARTESIAN_POINT('Ctrl Pts',(4.39825297998733,2.72598918212333,6.07687120025204));
#99811=CARTESIAN_POINT('Ctrl Pts',(4.27476800964676,2.70215892392453,6.16433954508843));
#99812=CARTESIAN_POINT('Ctrl Pts',(4.14919406351116,2.67857142889851,6.24773467905231));
#99813=CARTESIAN_POINT('Ctrl Pts',(4.11696067960482,2.67251679086577,6.26914124840894));
#99814=CARTESIAN_POINT('Ctrl Pts',(4.08453351292944,2.66644617725385,6.29031702417241));
#99815=CARTESIAN_POINT('Ctrl Pts',(4.05191750219905,2.66036061550164,6.31125697104795));
#99816=CARTESIAN_POINT('Ctrl Pts',(4.05191750219919,2.83963938449833,6.3112569710482));
#99817=CARTESIAN_POINT('Ctrl Pts',(4.08453351292954,2.83355382274611,6.29031702417293));
#99818=CARTESIAN_POINT('Ctrl Pts',(4.11696067950133,2.82748320915847,6.26914124834338));
#99819=CARTESIAN_POINT('Ctrl Pts',(4.14919406351669,2.82142857110149,6.24773467901926));
#99820=CARTESIAN_POINT('Ctrl Pts',(4.27476801007775,2.79784107598091,6.16433954518152));
#99821=CARTESIAN_POINT('Ctrl Pts',(4.39825297998724,2.77401081787664,6.07687120025258));
#99822=CARTESIAN_POINT('Ctrl Pts',(4.51926703485033,2.74999999826059,5.98550127059301));
#99823=CARTESIAN_POINT('Ctrl Pts',(3.911252806,2.879480225,6.104473891));
#99824=CARTESIAN_POINT('Ctrl Pts',(4.06148337,2.85030975,6.00821830500001));
#99825=CARTESIAN_POINT('Ctrl Pts',(4.206797255,2.821428571,5.904689396));
#99826=CARTESIAN_POINT('Ctrl Pts',(4.385422592,2.785926731,5.777427735));
#99827=CARTESIAN_POINT('Ctrl Pts',(4.556028634,2.75,5.63960132400001));
#99828=CARTESIAN_POINT('Ctrl Pts',(4.55913118463147,2.74934665560115,5.63709488628262));
#99829=CARTESIAN_POINT('Ctrl Pts',(4.56223373526293,2.7486933112023,5.63458844856525));
#99830=CARTESIAN_POINT('Ctrl Pts',(3.836844939,2.879480225,6.444270394));
#99831=CARTESIAN_POINT('Ctrl Pts',(3.995437865,2.85030975,6.349845979));
#99832=CARTESIAN_POINT('Ctrl Pts',(4.149194064,2.821428571,6.247734679));
#99833=CARTESIAN_POINT('Ctrl Pts',(4.338197014,2.785926731,6.122215598));
#99834=CARTESIAN_POINT('Ctrl Pts',(4.519267026,2.75,5.98550127800001));
#99835=CARTESIAN_POINT('Ctrl Pts',(4.52255986881779,2.74934665560115,5.98301506417736));
#99836=CARTESIAN_POINT('Ctrl Pts',(4.52585271163557,2.7486933112023,5.98052885035472));
#99837=CARTESIAN_POINT('',(4.53764783906171,2.75000000185146,5.81255129392586));
#99838=CARTESIAN_POINT('Ctrl Pts',(4.556028634,2.75,5.63960132400001));
#99839=CARTESIAN_POINT('Ctrl Pts',(4.861627526,2.81435393,5.392719102));
#99840=CARTESIAN_POINT('Ctrl Pts',(5.138759199,2.879481221,5.114259858));
#99841=CARTESIAN_POINT('Ctrl Pts',(4.901928588,2.75,5.676362931));
#99842=CARTESIAN_POINT('Ctrl Pts',(5.209519519,2.81435393,5.41073707200001));
#99843=CARTESIAN_POINT('Ctrl Pts',(5.486606152,2.879481221,5.113428687));
#99844=CARTESIAN_POINT('',(4.90192859649301,2.75,5.67636292348124));
#99845=CARTESIAN_POINT('',(5.31391961162131,2.83963938432021,5.29266080113455));
#99846=CARTESIAN_POINT('Origin',(-0.1451010862056,2.94636923250028,-0.120394251048356));
#99847=CARTESIAN_POINT('Ctrl Pts',(5.13544741478264,2.87870320266467,5.11758535350932));
#99848=CARTESIAN_POINT('Ctrl Pts',(5.16512227092593,2.87185457185746,5.14674715239094));
#99849=CARTESIAN_POINT('Ctrl Pts',(5.1948502129185,2.86518067047536,5.17593376078539));
#99850=CARTESIAN_POINT('Ctrl Pts',(5.25433136878464,2.85217081127113,5.23428150693977));
#99851=CARTESIAN_POINT('Ctrl Pts',(5.28412021299232,2.84582706799665,5.26347759348871));
#99852=CARTESIAN_POINT('Ctrl Pts',(5.31391961274871,2.83963938432419,5.29266079998418));
#99853=CARTESIAN_POINT('',(4.72897861982077,2.74999999814853,5.65798212012754));
#99854=CARTESIAN_POINT('Origin',(-4.38017677684144E-14,2.84071505699989,
6.50521303491303E-14));
#99855=CARTESIAN_POINT('',(5.31391961162116,2.66036061567976,5.29266080113437));
#99856=CARTESIAN_POINT('Origin',(-0.145101086098398,2.55363076748073,-0.120394250919469));
#99857=CARTESIAN_POINT('',(5.70031492639775,2.75,4.87405475279786));
#99858=CARTESIAN_POINT('Ctrl Pts',(5.70031492605116,2.75000000173941,4.8740547528639));
#99859=CARTESIAN_POINT('Ctrl Pts',(5.60177194666881,2.72598918212334,4.98930294874716));
#99860=CARTESIAN_POINT('Ctrl Pts',(5.49997709495883,2.70215892392439,5.10127195060386));
#99861=CARTESIAN_POINT('Ctrl Pts',(5.39526648644324,2.67857142887792,5.20971203926714));
#99862=CARTESIAN_POINT('Ctrl Pts',(5.36838848047096,2.67251679080437,5.23754735998662));
#99863=CARTESIAN_POINT('Ctrl Pts',(5.34127160873142,2.66644617720303,5.2651989404272));
#99864=CARTESIAN_POINT('Ctrl Pts',(5.31391961177441,2.66036061545698,5.29266080123764));
#99865=CARTESIAN_POINT('Ctrl Pts',(5.3139196117744,2.83963938454303,5.29266080123765));
#99866=CARTESIAN_POINT('Ctrl Pts',(5.34127160873155,2.83355382279695,5.26519894042819));
#99867=CARTESIAN_POINT('Ctrl Pts',(5.36838848046974,2.827483209194,5.23754735980595));
#99868=CARTESIAN_POINT('Ctrl Pts',(5.3952664864407,2.82142857112209,5.20971203921784));
#99869=CARTESIAN_POINT('Ctrl Pts',(5.49997709495177,2.79784107608189,5.10127195106572));
#99870=CARTESIAN_POINT('Ctrl Pts',(5.60177194666888,2.77401081787662,4.98930294874803));
#99871=CARTESIAN_POINT('Ctrl Pts',(5.70031492605117,2.74999999826059,4.87405475286389));
#99872=CARTESIAN_POINT('Ctrl Pts',(5.132091328,2.879480225,5.120950947));
#99873=CARTESIAN_POINT('Ctrl Pts',(5.258117479,2.85030975,4.994650632));
#99874=CARTESIAN_POINT('Ctrl Pts',(5.377778351,2.821428571,4.862303981));
#99875=CARTESIAN_POINT('Ctrl Pts',(5.524870032,2.785926731,4.69961846));
#99876=CARTESIAN_POINT('Ctrl Pts',(5.661858795,2.75,4.528339098));
#99877=CARTESIAN_POINT('Ctrl Pts',(5.6643499996969,2.74934665560115,4.52522430272956));
#99878=CARTESIAN_POINT('Ctrl Pts',(5.6668412043938,2.7486933112023,4.52210950745911));
#99879=CARTESIAN_POINT('Ctrl Pts',(5.13246928,2.879480225,5.468798688));
#99880=CARTESIAN_POINT('Ctrl Pts',(5.267055933,2.85030975,5.342489072));
#99881=CARTESIAN_POINT('Ctrl Pts',(5.395266487,2.821428571,5.209712039));
#99882=CARTESIAN_POINT('Ctrl Pts',(5.552867761,2.785926731,5.046497477));
#99883=CARTESIAN_POINT('Ctrl Pts',(5.700314919,2.75,4.874054762));
#99884=CARTESIAN_POINT('Ctrl Pts',(5.70299631449924,2.74934665560115,4.87091881061139));
#99885=CARTESIAN_POINT('Ctrl Pts',(5.70567770999847,2.7486933112023,4.86778285922278));
#99886=CARTESIAN_POINT('',(5.68108686432912,2.75000000185146,4.70119692114325));
#99887=CARTESIAN_POINT('Ctrl Pts',(5.661858795,2.75,4.528339098));
#99888=CARTESIAN_POINT('Ctrl Pts',(5.907240575,2.81435393,4.221534117));
#99889=CARTESIAN_POINT('Ctrl Pts',(6.118032557,2.879481221,3.890009978));
#99890=CARTESIAN_POINT('Ctrl Pts',(6.007574459,2.75,4.489882974));
#99891=CARTESIAN_POINT('Ctrl Pts',(6.250872378,2.81435393,4.164344342));
#99892=CARTESIAN_POINT('Ctrl Pts',(6.457568365,2.879481221,3.814421426));
#99893=CARTESIAN_POINT('',(6.0075744657785,2.75,4.48988296490629));
#99894=CARTESIAN_POINT('',(6.32744874633466,2.83963938435354,4.0265856945531));
#99895=CARTESIAN_POINT('Origin',(-0.167589759079224,2.9463692414211,-0.0863869564722602));
#99896=CARTESIAN_POINT('Ctrl Pts',(6.11551308399302,2.87870320275711,3.89396966050874));
#99897=CARTESIAN_POINT('Ctrl Pts',(6.15076308335111,2.87185457194778,3.91607045570484));
#99898=CARTESIAN_POINT('Ctrl Pts',(6.1860702606457,2.86518067056699,3.93818406853816));
#99899=CARTESIAN_POINT('Ctrl Pts',(6.256703820957,2.85217081132701,3.98238098655727));
#99900=CARTESIAN_POINT('Ctrl Pts',(6.29207251402559,2.84582706805614,4.00449076384202));
#99901=CARTESIAN_POINT('Ctrl Pts',(6.32744874717936,2.83963938435753,4.02658569320178));
#99902=CARTESIAN_POINT('',(5.83471663402968,2.74999999814853,4.5091110269037));
#99903=CARTESIAN_POINT('Origin',(1.65752828129584E-12,2.84071505699922,
1.06338549077378E-12));
#99904=CARTESIAN_POINT('',(6.32744874633445,2.66036061564643,4.02658569455294));
#99905=CARTESIAN_POINT('Origin',(-0.167589758930268,2.55363075855824,-0.0863869563564529));
#99906=CARTESIAN_POINT('',(6.61482242727647,2.75,3.53470285143859));
#99907=CARTESIAN_POINT('Ctrl Pts',(6.61482242692228,2.75000000173941,3.53470285156161));
#99908=CARTESIAN_POINT('Ctrl Pts',(6.54335828239023,2.72598918212333,3.6684404372531));
#99909=CARTESIAN_POINT('Ctrl Pts',(6.46801336322534,2.70215892392438,3.79967455044767));
#99910=CARTESIAN_POINT('Ctrl Pts',(6.38906224448245,2.67857142887702,3.9280890552822));
#99911=CARTESIAN_POINT('Ctrl Pts',(6.36879640248986,2.67251679078551,3.96105157831173));
#99912=CARTESIAN_POINT('Ctrl Pts',(6.34825778061731,2.66644617717233,3.99388600610648));
#99913=CARTESIAN_POINT('Ctrl Pts',(6.32744874646083,2.66036061541843,4.02658569459093));
#99914=CARTESIAN_POINT('Ctrl Pts',(6.32744874646082,2.83963938458158,4.02658569459094));
#99915=CARTESIAN_POINT('Ctrl Pts',(6.34825778061771,2.83355382282764,3.99388600610754));
#99916=CARTESIAN_POINT('Ctrl Pts',(6.36879640248882,2.82748320921173,3.96105157825919));
#99917=CARTESIAN_POINT('Ctrl Pts',(6.38906224448281,2.82142857112299,3.92808905528369));
#99918=CARTESIAN_POINT('Ctrl Pts',(6.46801336323162,2.79784107608627,3.79967455065886));
#99919=CARTESIAN_POINT('Ctrl Pts',(6.54335828239052,2.77401081787664,3.66844043725405));
#99920=CARTESIAN_POINT('Ctrl Pts',(6.61482242692228,2.74999999826059,3.53470285156161));
#99921=CARTESIAN_POINT('Ctrl Pts',(6.112958964,2.879480225,3.897978027));
#99922=CARTESIAN_POINT('Ctrl Pts',(6.20888786,2.85030975,3.747538647));
#99923=CARTESIAN_POINT('Ctrl Pts',(6.297300509,2.821428571,3.592562637));
#99924=CARTESIAN_POINT('Ctrl Pts',(6.40598069,2.785926731,3.402060249));
#99925=CARTESIAN_POINT('Ctrl Pts',(6.502946732,2.75,3.205336768));
#99926=CARTESIAN_POINT('Ctrl Pts',(6.50471010480504,2.74934665560115,3.20175925953051));
#99927=CARTESIAN_POINT('Ctrl Pts',(6.50647347761008,2.7486933112023,3.19818175106102));
#99928=CARTESIAN_POINT('Ctrl Pts',(6.188105062,2.879480225,4.237612033));
#99929=CARTESIAN_POINT('Ctrl Pts',(6.29239232,2.85030975,4.085323313));
#99930=CARTESIAN_POINT('Ctrl Pts',(6.389062245,2.821428571,3.928089055));
#99931=CARTESIAN_POINT('Ctrl Pts',(6.50789258200001,2.785926731,3.734810744));
#99932=CARTESIAN_POINT('Ctrl Pts',(6.614822422,2.75,3.534702862));
#99933=CARTESIAN_POINT('Ctrl Pts',(6.61676699112971,2.74934665560115,3.53106380661613));
#99934=CARTESIAN_POINT('Ctrl Pts',(6.61871156025942,2.7486933112023,3.52742475123226));
#99935=CARTESIAN_POINT('',(6.55888458225382,2.75000000185146,3.37001980477476));
#99936=CARTESIAN_POINT('Ctrl Pts',(6.502946732,2.75,3.205336768));
#99937=CARTESIAN_POINT('Ctrl Pts',(6.676637621,2.81435393,2.852954888));
#99938=CARTESIAN_POINT('Ctrl Pts',(6.81123351300001,2.879481221,2.483867554));
#99939=CARTESIAN_POINT('Ctrl Pts',(6.832312826,2.75,3.093461079));
#99940=CARTESIAN_POINT('Ctrl Pts',(6.999941392,2.81435393,2.723231498));
#99941=CARTESIAN_POINT('Ctrl Pts',(7.126581858,2.879481221,2.337056058));
#99942=CARTESIAN_POINT('',(6.83231283068604,2.75,3.09346106867118));
#99943=CARTESIAN_POINT('',(7.04511341073837,2.8396393842543,2.57223191590152));
#99944=CARTESIAN_POINT('Origin',(-0.182242366147894,2.94636923907614,-0.0483404868385445));
#99945=CARTESIAN_POINT('Ctrl Pts',(6.80962415850719,2.87870320272689,2.48827627372443));
#99946=CARTESIAN_POINT('Ctrl Pts',(6.84880105018254,2.87185457190863,2.50228265672233));
#99947=CARTESIAN_POINT('Ctrl Pts',(6.88803653853397,2.86518067051122,2.51628926610237));
#99948=CARTESIAN_POINT('Ctrl Pts',(6.96651975635637,2.85217081129629,2.54426875701519));
#99949=CARTESIAN_POINT('Ctrl Pts',(7.0058144982252,2.84582706793473,2.55825839662235));
#99950=CARTESIAN_POINT('Ctrl Pts',(7.04511341129873,2.8396393842583,2.57223191432735));
#99951=CARTESIAN_POINT('',(6.6676297839099,2.74999999814853,3.14939891310519));
#99952=CARTESIAN_POINT('Origin',(-2.03613167992778E-12,2.84071505700056,
-7.66314095512755E-13));
#99953=CARTESIAN_POINT('',(7.04511341073833,2.66036061574569,2.57223191590147));
#99954=CARTESIAN_POINT('Origin',(-0.182242366131465,2.55363076092139,-0.0483404868305065));
#99955=CARTESIAN_POINT('',(7.22002818281552,2.75,2.03007217453226));
#99956=CARTESIAN_POINT('Ctrl Pts',(7.22002818256322,2.75000000173941,2.03007217474743));
#99957=CARTESIAN_POINT('Ctrl Pts',(7.17898445787291,2.72598918212316,2.17604572814847));
#99958=CARTESIAN_POINT('Ctrl Pts',(7.13361251627696,2.70215892392443,2.32040859113163));
#99959=CARTESIAN_POINT('Ctrl Pts',(7.08411255356873,2.67857142888421,2.46279299334046));
#99960=CARTESIAN_POINT('Ctrl Pts',(7.07140648396715,2.67251679085757,2.49934142753215));
#99961=CARTESIAN_POINT('Ctrl Pts',(7.05840647505362,2.66644617727519,2.53582340086089));
#99962=CARTESIAN_POINT('Ctrl Pts',(7.04511341106862,2.66036061553643,2.57223191598709));
#99963=CARTESIAN_POINT('Ctrl Pts',(7.04511341106867,2.83963938446356,2.57223191598713));
#99964=CARTESIAN_POINT('Ctrl Pts',(7.05840647505371,2.8335538227248,2.53582340086099));
#99965=CARTESIAN_POINT('Ctrl Pts',(7.07140648393755,2.82748320914873,2.499341427539));
#99966=CARTESIAN_POINT('Ctrl Pts',(7.0841125535688,2.82142857111579,2.46279299334067));
#99967=CARTESIAN_POINT('Ctrl Pts',(7.13361251639273,2.79784107605103,2.32040859110585));
#99968=CARTESIAN_POINT('Ctrl Pts',(7.17898445787293,2.77401081787663,2.1760457281486));
#99969=CARTESIAN_POINT('Ctrl Pts',(7.22002818256322,2.74999999826059,2.03007217474743));
#99970=CARTESIAN_POINT('Ctrl Pts',(6.807991433,2.879480225,2.492739988));
#99971=CARTESIAN_POINT('Ctrl Pts',(6.869337544,2.85030975,2.325195919));
#99972=CARTESIAN_POINT('Ctrl Pts',(6.922367894,2.821428571,2.154837056));
#99973=CARTESIAN_POINT('Ctrl Pts',(6.987554811,2.785926731,1.945425482));
#99974=CARTESIAN_POINT('Ctrl Pts',(7.039964107,2.75,1.732456454));
#99975=CARTESIAN_POINT('Ctrl Pts',(7.04091719454892,2.74934665560115,1.72858351266358));
#99976=CARTESIAN_POINT('Ctrl Pts',(7.04187028209783,2.7486933112023,1.72471057132716));
#99977=CARTESIAN_POINT('Ctrl Pts',(6.954391929,2.879480225,2.808279349));
#99978=CARTESIAN_POINT('Ctrl Pts',(7.023503436,2.85030975,2.637132378));
#99979=CARTESIAN_POINT('Ctrl Pts',(7.084112554,2.821428571,2.462792993));
#99980=CARTESIAN_POINT('Ctrl Pts',(7.15861558,2.785926731,2.248488411));
#99981=CARTESIAN_POINT('Ctrl Pts',(7.22002818,2.75,2.030072186));
#99982=CARTESIAN_POINT('Ctrl Pts',(7.22114499684117,2.74934665560115,2.02610018483959));
#99983=CARTESIAN_POINT('Ctrl Pts',(7.22226181368234,2.7486933112023,2.02212818367918));
#99984=CARTESIAN_POINT('',(7.12999614643287,2.75000000185147,1.88126430888441));
#99985=CARTESIAN_POINT('Ctrl Pts',(7.039964107,2.75,1.732456454));
#99986=CARTESIAN_POINT('Ctrl Pts',(7.133842512,2.81435393,1.35097466));
#99987=CARTESIAN_POINT('Ctrl Pts',(7.18594876,2.879481221,0.961582244));
#99988=CARTESIAN_POINT('Ctrl Pts',(7.337579839,2.75,1.552392382));
#99989=CARTESIAN_POINT('Ctrl Pts',(7.421700926,2.81435393,1.154783377));
#99990=CARTESIAN_POINT('Ctrl Pts',(7.46236430400001,2.879481221,0.750412547000001));
#99991=CARTESIAN_POINT('',(7.33757984131742,2.75,1.55239237089712));
#99992=CARTESIAN_POINT('',(7.43335640120693,2.83963938428037,0.997603432181168));
#99993=CARTESIAN_POINT('Origin',(-0.188373354874297,2.94636921314844,-0.00803358028075435));
#99994=CARTESIAN_POINT('Ctrl Pts',(7.18532477572594,2.8787032027058,0.966233854084377));
#99995=CARTESIAN_POINT('Ctrl Pts',(7.22659669178231,2.87185457188186,0.971490902133333));
#99996=CARTESIAN_POINT('Ctrl Pts',(7.26792588317493,2.86518067048678,0.976735574680769));
#99997=CARTESIAN_POINT('Ctrl Pts',(7.35058897048162,2.85217081126976,0.9871893489177));
#99998=CARTESIAN_POINT('Ctrl Pts',(7.39197238182782,2.8458270679546,0.992404710569672));
#99999=CARTESIAN_POINT('Ctrl Pts',(7.43335640141232,2.83963938428435,0.997603430550835));
#100000=CARTESIAN_POINT('',(7.18877197556053,2.74999999814853,1.64242440679273));
#100001=CARTESIAN_POINT('Origin',(-4.66640615037761E-13,2.840715057,-5.7516925250356E-14));
#100002=CARTESIAN_POINT('',(7.43335640120675,2.66036061571961,0.997603432181095));
#100003=CARTESIAN_POINT('Origin',(-0.188373354749872,2.55363078683776,-0.00803358025205148));
#100004=CARTESIAN_POINT('',(7.48763344524873,2.75,0.430517578193262));
#100005=CARTESIAN_POINT('Ctrl Pts',(7.48763344508452,2.75000000173941,0.430517578459702));
#100006=CARTESIAN_POINT('Ctrl Pts',(7.4789292985699,2.72598918212316,0.581901539071339));
#100007=CARTESIAN_POINT('Ctrl Pts',(7.46565187590449,2.70215892392418,0.732642904818717));
#100008=CARTESIAN_POINT('Ctrl Pts',(7.44791763247454,2.67857142884723,0.882339467482308));
#100009=CARTESIAN_POINT('Ctrl Pts',(7.44336545647058,2.67251679079159,0.920764849139752));
#100010=CARTESIAN_POINT('Ctrl Pts',(7.43851192655382,2.66644617724562,0.959188511968675));
#100011=CARTESIAN_POINT('Ctrl Pts',(7.43335640149295,2.66036061550664,0.997603432185768));
#100012=CARTESIAN_POINT('Ctrl Pts',(7.43335640149294,2.83963938449337,0.997603432185807));
#100013=CARTESIAN_POINT('Ctrl Pts',(7.43851192655439,2.83355382275437,0.959188511969271));
#100014=CARTESIAN_POINT('Ctrl Pts',(7.4433654566666,2.82748320916823,0.92076484908148));
#100015=CARTESIAN_POINT('Ctrl Pts',(7.4479176324752,2.82142857115279,0.882339467483236));
#100016=CARTESIAN_POINT('Ctrl Pts',(7.46565187514419,2.79784107623236,0.732642905049655));
#100017=CARTESIAN_POINT('Ctrl Pts',(7.47892929857034,2.77401081787663,0.5819015390719));
#100018=CARTESIAN_POINT('Ctrl Pts',(7.48763344508452,2.74999999826059,0.430517578459712));
#100019=CARTESIAN_POINT('Ctrl Pts',(7.184689789,2.879480225,0.970944197));
#100020=CARTESIAN_POINT('Ctrl Pts',(7.20858464,2.85030975,0.794129615));
#100021=CARTESIAN_POINT('Ctrl Pts',(7.22375305,2.821428571,0.616353689));
#100022=CARTESIAN_POINT('Ctrl Pts',(7.24239863499999,2.785926731,0.397824782));
#100023=CARTESIAN_POINT('Ctrl Pts',(7.247800585,2.75,0.178568402));
#100024=CARTESIAN_POINT('Ctrl Pts',(7.24789882198614,2.74934665560115,0.174581122228147));
#100025=CARTESIAN_POINT('Ctrl Pts',(7.24799705897229,2.7486933112023,0.170593842456293));
#100026=CARTESIAN_POINT('Ctrl Pts',(7.395499158,2.879480225,1.247634645));
#100027=CARTESIAN_POINT('Ctrl Pts',(7.426203336,2.85030975,1.065632063));
#100028=CARTESIAN_POINT('Ctrl Pts',(7.447917633,2.821428571,0.882339467));
#100029=CARTESIAN_POINT('Ctrl Pts',(7.474609669,2.785926731,0.657029259));
#100030=CARTESIAN_POINT('Ctrl Pts',(7.487633445,2.75,0.43051759));
#100031=CARTESIAN_POINT('Ctrl Pts',(7.48787028845513,2.74934665560115,0.426398369405861));
#100032=CARTESIAN_POINT('Ctrl Pts',(7.48810713191026,2.7486933112023,0.422279148811721));
#100033=CARTESIAN_POINT('',(7.36771701547478,2.75000000185146,0.304542984513805));
#100034=CARTESIAN_POINT('Ctrl Pts',(7.247800585,2.75,0.178568402));
#100035=CARTESIAN_POINT('Ctrl Pts',(7.257476856,2.81435393,-0.214175642));
#100036=CARTESIAN_POINT('Ctrl Pts',(7.22465703,2.879481221,-0.605665581999999));
#100037=CARTESIAN_POINT('Ctrl Pts',(7.499749774,2.75,-0.061264458));
#100038=CARTESIAN_POINT('Ctrl Pts',(7.49642997300001,2.81435393,-0.467661132000001));
#100039=CARTESIAN_POINT('Ctrl Pts',(7.449214889,2.879481221,-0.871319421));
#100040=CARTESIAN_POINT('',(7.49974977376454,2.75,-0.061264469340567));
#100041=CARTESIAN_POINT('',(7.47402390826455,2.83963938428077,-0.623671879939793));
#100042=CARTESIAN_POINT('Origin',(-0.185696566482395,2.94636920236734,0.0326489605617519));
#100043=CARTESIAN_POINT('Ctrl Pts',(7.22504759274717,2.87870320280466,-0.60098858640385));
#100044=CARTESIAN_POINT('Ctrl Pts',(7.26648470406984,2.87185457197965,-0.604726687300666));
#100045=CARTESIAN_POINT('Ctrl Pts',(7.30797509130833,2.8651806705829,-0.608489186847638));
#100046=CARTESIAN_POINT('Ctrl Pts',(7.39095281381384,2.85217081134085,-0.616049936504215));
#100047=CARTESIAN_POINT('Ctrl Pts',(7.43248985279003,2.84582706797145,-0.619852717380044));
#100048=CARTESIAN_POINT('Ctrl Pts',(7.47402390811265,2.83963938428477,-0.623671881598194));
#100049=CARTESIAN_POINT('',(7.37377517959144,2.74999999814853,0.0586519605043138));
#100050=CARTESIAN_POINT('Origin',(5.5944832100252E-14,2.84071505699989,
9.62873173120798E-14));
#100051=CARTESIAN_POINT('',(7.47402390826407,2.66036061571915,-0.623671879939818));
#100052=CARTESIAN_POINT('Origin',(-0.185696566312097,2.5536307976139,0.0326489605633622));
#100053=CARTESIAN_POINT('',(7.40512528964675,2.75,-1.18916754157494));
#100054=CARTESIAN_POINT('Ctrl Pts',(7.4051252896016,2.75000000173941,-1.18916754128873));
#100055=CARTESIAN_POINT('Ctrl Pts',(7.42916771795374,2.72598918212316,-1.03945171928497));
#100056=CARTESIAN_POINT('Ctrl Pts',(7.44860565166737,2.7021589239243,-0.889380349572321));
#100057=CARTESIAN_POINT('Ctrl Pts',(7.46346636079052,2.67857142886505,-0.739371271367419));
#100058=CARTESIAN_POINT('Ctrl Pts',(7.46728093354585,2.67251679082236,-0.700865670528982));
#100059=CARTESIAN_POINT('Ctrl Pts',(7.47080082797672,2.66644617725542,-0.662296966240046));
#100060=CARTESIAN_POINT('Ctrl Pts',(7.47402390859826,2.66036061551054,-0.623671880000571));
#100061=CARTESIAN_POINT('Ctrl Pts',(7.47402390859875,2.8396393844894,-0.623671880000552));
#100062=CARTESIAN_POINT('Ctrl Pts',(7.47080082797757,2.83355382274451,-0.662296966239768));
#100063=CARTESIAN_POINT('Ctrl Pts',(7.46728093347334,2.82748320915981,-0.700865670689327));
#100064=CARTESIAN_POINT('Ctrl Pts',(7.4634663607916,2.82142857113497,-0.73937127136646));
#100065=CARTESIAN_POINT('Ctrl Pts',(7.44860565195505,2.79784107614504,-0.889380348944392));
#100066=CARTESIAN_POINT('Ctrl Pts',(7.42916771795445,2.77401081787664,-1.03945171928441));
#100067=CARTESIAN_POINT('Ctrl Pts',(7.4051252896016,2.74999999826059,-1.18916754128874));
#100068=CARTESIAN_POINT('Ctrl Pts',(7.22574379878017,2.880540329927,-0.589982327261686));
#100069=CARTESIAN_POINT('Ctrl Pts',(7.21096041357039,2.85083482787434,-0.771040212929628));
#100070=CARTESIAN_POINT('Ctrl Pts',(7.18712761817257,2.821428571,-0.951130479136298));
#100071=CARTESIAN_POINT('Ctrl Pts',(7.15835455504156,2.785926731,-1.16855141510238));
#100072=CARTESIAN_POINT('Ctrl Pts',(7.11649154232713,2.75,-1.38383550852302));
#100073=CARTESIAN_POINT('Ctrl Pts',(7.11541813743386,2.74907880665164,-1.3893555842256));
#100074=CARTESIAN_POINT('Ctrl Pts',(7.11434473254058,2.74815761330328,-1.39487565992819));
#100075=CARTESIAN_POINT('Ctrl Pts',(7.49113016545384,2.880540329927,-0.36464893196537));
#100076=CARTESIAN_POINT('Ctrl Pts',(7.48199303513689,2.85083482787434,-0.552356692243661));
#100077=CARTESIAN_POINT('Ctrl Pts',(7.463466361,2.821428571,-0.739371272));
#100078=CARTESIAN_POINT('Ctrl Pts',(7.441099318,2.785926731,-0.965151851));
#100079=CARTESIAN_POINT('Ctrl Pts',(7.405125292,2.75,-1.18916753));
#100080=CARTESIAN_POINT('Ctrl Pts',(7.40420288596577,2.74907880665164,-1.1949114913257));
#100081=CARTESIAN_POINT('Ctrl Pts',(7.40328047993151,2.74815761330329,-1.2006554526514));
#100082=CARTESIAN_POINT('',(7.26093162549449,2.75000000185147,-1.28641843181972));
#100083=CARTESIAN_POINT('Ctrl Pts',(7.11673796300001,2.75,-1.383669311));
#100084=CARTESIAN_POINT('Ctrl Pts',(7.041759648,2.81435393,-1.769311329));
#100085=CARTESIAN_POINT('Ctrl Pts',(6.925548367,2.879481221,-2.14459316));
#100086=CARTESIAN_POINT('Ctrl Pts',(7.311239744,2.75,-1.672056639));
#100087=CARTESIAN_POINT('Ctrl Pts',(7.220634287,2.81435393,-2.068238326));
#100088=CARTESIAN_POINT('Ctrl Pts',(7.087748465,2.879481221,-2.452309461));
#100089=CARTESIAN_POINT('',(7.31123974150887,2.75,-1.67205665006523));
#100090=CARTESIAN_POINT('',(7.1652143640651,2.83963938426122,-2.21578498726053));
#100091=CARTESIAN_POINT('Origin',(-0.174336251871083,2.94636921029586,0.0718048408766353));
#100092=CARTESIAN_POINT('Ctrl Pts',(6.92693521455026,2.87870320272253,-2.14010946892607));
#100093=CARTESIAN_POINT('Ctrl Pts',(6.96659996794133,2.87185457192133,-2.15266792919406));
#100094=CARTESIAN_POINT('Ctrl Pts',(7.00631150668629,2.8651806705447,-2.16526167034536));
#100095=CARTESIAN_POINT('Ctrl Pts',(7.08572391840278,2.85217081130674,-2.1904834112367));
#100096=CARTESIAN_POINT('Ctrl Pts',(7.12547235876744,2.84582706796812,-2.20312652055182));
#100097=CARTESIAN_POINT('Ctrl Pts',(7.16521436356818,2.8396393842652,-2.2157849888226));
#100098=CARTESIAN_POINT('',(7.21398885111807,2.74999999814853,-1.52786298624658));
#100099=CARTESIAN_POINT('Origin',(-1.04083408558608E-14,2.84071505699967,
-1.3238108526048E-13));
#100100=CARTESIAN_POINT('',(7.16521436406483,2.66036061573874,-2.21578498726049));
#100101=CARTESIAN_POINT('Origin',(-0.174336251676337,2.55363078968169,0.0718048408357719));
#100102=CARTESIAN_POINT('',(6.97636170529881,2.75,-2.75324850883221));
#100103=CARTESIAN_POINT('Ctrl Pts',(6.97636170523082,2.75000000173941,-2.75324850850928));
#100104=CARTESIAN_POINT('Ctrl Pts',(7.03202651153764,2.72598918212314,-2.61220137043643));
#100105=CARTESIAN_POINT('Ctrl Pts',(7.08327090563027,2.70215892392449,-2.46981716683914));
#100106=CARTESIAN_POINT('Ctrl Pts',(7.13003169698747,2.67857142889278,-2.32650983045378));
#100107=CARTESIAN_POINT('Ctrl Pts',(7.14203465313809,2.6725167908538,-2.28972448961772));
#100108=CARTESIAN_POINT('Ctrl Pts',(7.15376338573902,2.6664461772565,-2.25281417336172));
#100109=CARTESIAN_POINT('Ctrl Pts',(7.16521436431504,2.66036061552466,-2.21578498737305));
#100110=CARTESIAN_POINT('Ctrl Pts',(7.16521436431505,2.83963938447534,-2.21578498737302));
#100111=CARTESIAN_POINT('Ctrl Pts',(7.15376338574019,2.83355382274348,-2.25281417336128));
#100112=CARTESIAN_POINT('Ctrl Pts',(7.14203465296253,2.82748320916324,-2.28972448961258));
#100113=CARTESIAN_POINT('Ctrl Pts',(7.13003169690104,2.82142857110724,-2.32650983049405));
#100114=CARTESIAN_POINT('Ctrl Pts',(7.08327090589077,2.79784107600908,-2.46981716705734));
#100115=CARTESIAN_POINT('Ctrl Pts',(7.03202651153861,2.77401081787666,-2.61220137043596));
#100116=CARTESIAN_POINT('Ctrl Pts',(6.97636170523082,2.74999999826059,-2.75324850850928));
#100117=CARTESIAN_POINT('Ctrl Pts',(6.928336737,2.879480225,-2.135567854));
#100118=CARTESIAN_POINT('Ctrl Pts',(6.87578060099999,2.85030975,-2.30607361));
#100119=CARTESIAN_POINT('Ctrl Pts',(6.814900903,2.821428571,-2.47378772));
#100120=CARTESIAN_POINT('Ctrl Pts',(6.740065271,2.785926731,-2.679948262));
#100121=CARTESIAN_POINT('Ctrl Pts',(6.652904584,2.75,-2.881208184));
#100122=CARTESIAN_POINT('Ctrl Pts',(6.6513195261596,2.74934665560115,-2.88486818976984));
#100123=CARTESIAN_POINT('Ctrl Pts',(6.64973446831921,2.7486933112023,-2.88852819553969));
#100124=CARTESIAN_POINT('Ctrl Pts',(7.23584144200001,2.879480225,-1.972966961));
#100125=CARTESIAN_POINT('Ctrl Pts',(7.187286899,2.85030975,-2.15104038));
#100126=CARTESIAN_POINT('Ctrl Pts',(7.130031697,2.821428571,-2.326509831));
#100127=CARTESIAN_POINT('Ctrl Pts',(7.059651433,2.785926731,-2.542203533));
#100128=CARTESIAN_POINT('Ctrl Pts',(6.97636171000001,2.75,-2.753248498));
#100129=CARTESIAN_POINT('Ctrl Pts',(6.9748470474496,2.74934665560115,-2.75708644935127));
#100130=CARTESIAN_POINT('Ctrl Pts',(6.97333238489921,2.7486933112023,-2.76092440070255));
#100131=CARTESIAN_POINT('',(6.81463314260797,2.75000000185147,-2.81722835162395));
#100132=CARTESIAN_POINT('Ctrl Pts',(6.652904584,2.75,-2.881208184));
#100133=CARTESIAN_POINT('Ctrl Pts',(6.49677758500001,2.81435393,-3.241715985));
#100134=CARTESIAN_POINT('Ctrl Pts',(6.302608759,2.879481221,-3.583241945));
#100135=CARTESIAN_POINT('Ctrl Pts',(6.78086427000001,2.75,-3.20466531));
#100136=CARTESIAN_POINT('Ctrl Pts',(6.607209766,2.81435393,-3.572106995));
#100137=CARTESIAN_POINT('Ctrl Pts',(6.394866801,2.879481221,-3.918632236));
#100138=CARTESIAN_POINT('',(6.78086426520829,2.75,-3.20466532028041));
#100139=CARTESIAN_POINT('',(6.5213673600565,2.83963938426449,-3.70429045185705));
#100140=CARTESIAN_POINT('Origin',(-0.154824635565474,2.94636926992071,0.107603327694034));
#100141=CARTESIAN_POINT('Ctrl Pts',(6.30492704407009,2.8787032026541,-3.57916121100237));
#100142=CARTESIAN_POINT('Ctrl Pts',(6.34096475976856,2.87185457189683,-3.59995281093015));
#100143=CARTESIAN_POINT('Ctrl Pts',(6.37704058264914,2.86518067055398,-3.62078892438102));
#100144=CARTESIAN_POINT('Ctrl Pts',(6.44917444755483,2.8521708113417,-3.66249231621842));
#100145=CARTESIAN_POINT('Ctrl Pts',(6.48527569685389,2.84582706798045,-3.68338457656364));
#100146=CARTESIAN_POINT('Ctrl Pts',(6.52136735922969,2.83963938426847,-3.70429045328561));
#100147=CARTESIAN_POINT('',(6.71688442225607,2.74999999814853,-3.04293675747159));
#100148=CARTESIAN_POINT('Origin',(-6.65266453037106E-13,2.84071505699989,
3.67761376907083E-13));
#100149=CARTESIAN_POINT('',(6.52136736005646,2.6603606157355,-3.70429045185702));
#100150=CARTESIAN_POINT('Origin',(-0.15482463553375,2.55363073007556,0.107603327679747));
#100151=CARTESIAN_POINT('',(6.2213912019492,2.75,-4.18859063547911));
#100152=CARTESIAN_POINT('Ctrl Pts',(6.22139120208406,2.75000000173934,-4.18859063523788));
#100153=CARTESIAN_POINT('Ctrl Pts',(6.30607556111986,2.72598918212307,-4.06280738917551));
#100154=CARTESIAN_POINT('Ctrl Pts',(6.38673028461759,2.70215892392445,-3.93476807920542));
#100155=CARTESIAN_POINT('Ctrl Pts',(6.46320467600042,2.67857142888631,-3.8048633764564));
#100156=CARTESIAN_POINT('Ctrl Pts',(6.48283477051439,2.67251679084892,-3.77151833718257));
#100157=CARTESIAN_POINT('Ctrl Pts',(6.50222391884417,2.66644617725987,-3.73799229439273));
#100158=CARTESIAN_POINT('Ctrl Pts',(6.52136736030762,2.66036061552477,-3.70429045203774));
#100159=CARTESIAN_POINT('Ctrl Pts',(6.52136736030762,2.83963938447523,-3.70429045203774));
#100160=CARTESIAN_POINT('Ctrl Pts',(6.50222391884436,2.83355382274013,-3.7379922943927));
#100161=CARTESIAN_POINT('Ctrl Pts',(6.482834770476,2.82748320916001,-3.77151833714848));
#100162=CARTESIAN_POINT('Ctrl Pts',(6.46320467600067,2.82142857111369,-3.80486337645633));
#100163=CARTESIAN_POINT('Ctrl Pts',(6.38673028476825,2.79784107604075,-3.93476807933803));
#100164=CARTESIAN_POINT('Ctrl Pts',(6.30607556112001,2.77401081787675,-4.06280738917544));
#100165=CARTESIAN_POINT('Ctrl Pts',(6.22139120208405,2.74999999826065,-4.18859063523787));
#100166=CARTESIAN_POINT('Ctrl Pts',(6.307272113,2.879480225,-3.575027062));
#100167=CARTESIAN_POINT('Ctrl Pts',(6.219291012,2.85030975,-3.730248473));
#100168=CARTESIAN_POINT('Ctrl Pts',(6.123781072,2.821428571,-3.880954185));
#100169=CARTESIAN_POINT('Ctrl Pts',(6.006376632,2.785926731,-4.06620736));
#100170=CARTESIAN_POINT('Ctrl Pts',(5.87798878,2.75,-4.244024965));
#100171=CARTESIAN_POINT('Ctrl Pts',(5.87565398689053,2.74934665560115,-4.247258661276));
#100172=CARTESIAN_POINT('Ctrl Pts',(5.87331919378106,2.7486933112023,-4.25049235755201));
#100173=CARTESIAN_POINT('Ctrl Pts',(6.64254191400001,2.879480225,-3.48233211));
#100174=CARTESIAN_POINT('Ctrl Pts',(6.556842028,2.85030975,-3.64580448));
#100175=CARTESIAN_POINT('Ctrl Pts',(6.463204676,2.821428571,-3.804863377));
#100176=CARTESIAN_POINT('Ctrl Pts',(6.348102093,2.785926731,-4.000384604));
#100177=CARTESIAN_POINT('Ctrl Pts',(6.221391209,2.75,-4.188590626));
#100178=CARTESIAN_POINT('Ctrl Pts',(6.21908691233759,2.74934665560115,-4.19201324049569));
#100179=CARTESIAN_POINT('Ctrl Pts',(6.21678261567518,2.7486933112023,-4.19543585499139));
#100180=CARTESIAN_POINT('',(6.04968998792708,2.75000000185138,-4.21630780493103));
#100181=CARTESIAN_POINT('Ctrl Pts',(5.87798878,2.75,-4.244024965));
#100182=CARTESIAN_POINT('Ctrl Pts',(5.648013423,2.81435393,-4.562541604));
#100183=CARTESIAN_POINT('Ctrl Pts',(5.38496617,2.879481221,-4.854342319));
#100184=CARTESIAN_POINT('Ctrl Pts',(5.933423119,2.75,-4.587427393));
#100185=CARTESIAN_POINT('Ctrl Pts',(5.684839461,2.81435393,-4.90894791));
#100186=CARTESIAN_POINT('Ctrl Pts',(5.402968272,2.879481221,-5.201724123));
#100187=CARTESIAN_POINT('',(5.93342311214813,2.75,-4.58742740203919));
#100188=CARTESIAN_POINT('',(5.5725884661497,2.83963938431518,-5.01958741169361));
#100189=CARTESIAN_POINT('Origin',(-0.128073249550485,2.9463692159568,0.138370213108596));
#100190=CARTESIAN_POINT('Ctrl Pts',(5.38810749189843,2.87870320268935,-4.85085535321375));
#100191=CARTESIAN_POINT('Ctrl Pts',(5.41883308675611,2.871854571875,-4.87890790060259));
#100192=CARTESIAN_POINT('Ctrl Pts',(5.4495863287704,2.86518067048863,-4.90701211292848));
#100193=CARTESIAN_POINT('Ctrl Pts',(5.5110687475944,2.852170811308,-4.96324715123295));
#100194=CARTESIAN_POINT('Ctrl Pts',(5.5418347513048,2.84582706798285,-4.99141166354931));
#100195=CARTESIAN_POINT('Ctrl Pts',(5.57258846503531,2.83963938431916,-5.01958741291084));
#100196=CARTESIAN_POINT('',(5.9057059426159,2.74999999814853,-4.41572618820698));
#100197=CARTESIAN_POINT('Origin',(-5.20850723662036E-13,2.84071505700067,
4.48426018540005E-13));
#100198=CARTESIAN_POINT('',(5.57258846614968,2.66036061568482,-5.01958741169357));
#100199=CARTESIAN_POINT('Origin',(-0.128073249529073,2.55363078404042,0.138370213093019));
#100200=CARTESIAN_POINT('',(5.17551536021189,2.75,-5.42807891888395));
#100201=CARTESIAN_POINT('Ctrl Pts',(5.1755153602599,2.75000000173934,-5.42807891853518));
#100202=CARTESIAN_POINT('Ctrl Pts',(5.28525952558719,2.7259891821231,-5.32344104899518));
#100203=CARTESIAN_POINT('Ctrl Pts',(5.39155325324616,2.7021589239245,-5.21573360859195));
#100204=CARTESIAN_POINT('Ctrl Pts',(5.49416538711631,2.67857142889486,-5.1053057395091));
#100205=CARTESIAN_POINT('Ctrl Pts',(5.52050473880592,2.67251679084257,-5.07696017883811));
#100206=CARTESIAN_POINT('Ctrl Pts',(5.54664768791324,2.66644617722575,-5.04838604997926));
#100207=CARTESIAN_POINT('Ctrl Pts',(5.57258846635438,2.66036061547379,-5.01958741192256));
#100208=CARTESIAN_POINT('Ctrl Pts',(5.57258846635438,2.83963938452621,-5.01958741192256));
#100209=CARTESIAN_POINT('Ctrl Pts',(5.54664768791338,2.83355382277425,-5.04838604997928));
#100210=CARTESIAN_POINT('Ctrl Pts',(5.52050473877698,2.82748320917711,-5.07696017874644));
#100211=CARTESIAN_POINT('Ctrl Pts',(5.49416538711348,2.82142857110514,-5.1053057395091));
#100212=CARTESIAN_POINT('Ctrl Pts',(5.39155325334494,2.79784107599881,-5.21573360894922));
#100213=CARTESIAN_POINT('Ctrl Pts',(5.28525952558731,2.77401081787672,-5.32344104899515));
#100214=CARTESIAN_POINT('Ctrl Pts',(5.1755153602599,2.74999999826065,-5.42807891853518));
#100215=CARTESIAN_POINT('Ctrl Pts',(5.391286454,2.879480225,-4.84732197900001));
#100216=CARTESIAN_POINT('Ctrl Pts',(5.271994288,2.85030975,-4.980001063));
#100217=CARTESIAN_POINT('Ctrl Pts',(5.146320044,2.821428571,-5.106651545));
#100218=CARTESIAN_POINT('Ctrl Pts',(4.991836498,2.785926731,-5.26233512));
#100219=CARTESIAN_POINT('Ctrl Pts',(4.828224754,2.75,-5.408395855));
#100220=CARTESIAN_POINT('Ctrl Pts',(4.82524939794747,2.74934665560115,-5.41105203774884));
#100221=CARTESIAN_POINT('Ctrl Pts',(4.82227404189494,2.7486933112023,-5.41370822049767));
#100222=CARTESIAN_POINT('Ctrl Pts',(5.73864450900001,2.879480225,-4.828867279));
#100223=CARTESIAN_POINT('Ctrl Pts',(5.619806511,2.85030975,-4.970094815));
#100224=CARTESIAN_POINT('Ctrl Pts',(5.494165387,2.821428571,-5.10530574));
#100225=CARTESIAN_POINT('Ctrl Pts',(5.33972255400001,2.785926731,-5.271512136));
#100226=CARTESIAN_POINT('Ctrl Pts',(5.175515369,2.75,-5.428078911));
#100227=CARTESIAN_POINT('Ctrl Pts',(5.17252918457452,2.74934665560115,-5.43092615099776));
#100228=CARTESIAN_POINT('Ctrl Pts',(5.16954300014905,2.7486933112023,-5.43377339099553));
#100229=CARTESIAN_POINT('',(5.00187005305336,2.75000000185138,-5.41823739079755));
#100230=CARTESIAN_POINT('Ctrl Pts',(4.828224754,2.75,-5.408395855));
#100231=CARTESIAN_POINT('Ctrl Pts',(4.535154431,2.81435393,-5.670027848));
#100232=CARTESIAN_POINT('Ctrl Pts',(4.215528549,2.879481221,-5.898459041));
#100233=CARTESIAN_POINT('Ctrl Pts',(4.808541698,2.75,-5.75568647));
#100234=CARTESIAN_POINT('Ctrl Pts',(4.49665238,2.81435393,-6.016251877));
#100235=CARTESIAN_POINT('Ctrl Pts',(4.158432951,2.879481221,-6.241589172));
#100236=CARTESIAN_POINT('',(4.80854168926236,2.75,-5.75568647723186));
#100237=CARTESIAN_POINT('',(4.36324152879854,2.83963938426255,-6.10017404315626));
#100238=CARTESIAN_POINT('Origin',(-0.0953336098313168,2.94636920711836,
0.162667358570282));
#100239=CARTESIAN_POINT('Ctrl Pts',(4.21934602295708,2.87870320271879,-5.89572888998683));
#100240=CARTESIAN_POINT('Ctrl Pts',(4.24332280172585,2.87185457190337,-5.92973067904311));
#100241=CARTESIAN_POINT('Ctrl Pts',(4.2673154748862,2.86518067052144,-5.9637888683585));
#100242=CARTESIAN_POINT('Ctrl Pts',(4.31527159774156,2.85217081130269,-6.03192606541324));
#100243=CARTESIAN_POINT('Ctrl Pts',(4.33926377175047,2.84582706794485,-6.06604588857911));
#100244=CARTESIAN_POINT('Ctrl Pts',(4.36324152744183,2.83963938426654,-6.10017404411018));
#100245=CARTESIAN_POINT('',(4.81838321729762,2.74999999814853,-5.58204117001184));
#100246=CARTESIAN_POINT('Origin',(-1.45283091113058E-13,2.84071505700011,
1.50920942409982E-13));
#100247=CARTESIAN_POINT('',(4.36324152879854,2.66036061573744,-6.10017404315625));
#100248=CARTESIAN_POINT('Origin',(-0.0953336098246177,2.55363079288176,
0.162667358561808));
#100249=CARTESIAN_POINT('',(3.88763817265509,2.75,-6.41375626569998));
#100250=CARTESIAN_POINT('Ctrl Pts',(3.88763817284382,2.75000000173934,-6.41375626547999));
#100251=CARTESIAN_POINT('Ctrl Pts',(4.01731062957616,2.72598918212306,-6.33515652268646));
#100252=CARTESIAN_POINT('Ctrl Pts',(4.14427318472604,2.70215892392422,-6.25281723181124));
#100253=CARTESIAN_POINT('Ctrl Pts',(4.26822503138358,2.67857142885272,-6.16702968037998));
#100254=CARTESIAN_POINT('Ctrl Pts',(4.30004204137926,2.67251679081034,-6.14500900501089));
#100255=CARTESIAN_POINT('Ctrl Pts',(4.33171637566225,2.66644617726505,-6.122722884807));
#100256=CARTESIAN_POINT('Ctrl Pts',(4.36324152896542,2.66036061552908,-6.10017404344581));
#100257=CARTESIAN_POINT('Ctrl Pts',(4.36324152896542,2.83963938447092,-6.10017404344581));
#100258=CARTESIAN_POINT('Ctrl Pts',(4.33171637566227,2.83355382273495,-6.12272288480701));
#100259=CARTESIAN_POINT('Ctrl Pts',(4.30004204116324,2.82748320915638,-6.14500900512305));
#100260=CARTESIAN_POINT('Ctrl Pts',(4.26822503138362,2.82142857114729,-6.16702968037998));
#100261=CARTESIAN_POINT('Ctrl Pts',(4.14427318556775,2.79784107620545,-6.25281723137432));
#100262=CARTESIAN_POINT('Ctrl Pts',(4.01731062957619,2.77401081787675,-6.33515652268643));
#100263=CARTESIAN_POINT('Ctrl Pts',(3.88763817284382,2.74999999826065,-6.41375626547999));
#100264=CARTESIAN_POINT('Ctrl Pts',(4.223210233,2.879480225,-5.892961507));
#100265=CARTESIAN_POINT('Ctrl Pts',(4.07818497,2.85030975,-5.996894338));
#100266=CARTESIAN_POINT('Ctrl Pts',(3.928222811,2.821428571,-6.093567555));
#100267=CARTESIAN_POINT('Ctrl Pts',(3.743883638,2.785926731,-6.212401939));
#100268=CARTESIAN_POINT('Ctrl Pts',(3.552698305,2.75,-6.319876166));
#100269=CARTESIAN_POINT('Ctrl Pts',(3.54922151034096,2.74934665560115,-6.3218306350618));
#100270=CARTESIAN_POINT('Ctrl Pts',(3.54574471568191,2.7486933112023,-6.3237851041236));
#100271=CARTESIAN_POINT('Ctrl Pts',(4.566414464,2.879480225,-5.949609982));
#100272=CARTESIAN_POINT('Ctrl Pts',(4.419995088,2.85030975,-6.061989039));
#100273=CARTESIAN_POINT('Ctrl Pts',(4.268225031,2.821428571,-6.167029681));
#100274=CARTESIAN_POINT('Ctrl Pts',(4.081663524,2.785926731,-6.29614962));
#100275=CARTESIAN_POINT('Ctrl Pts',(3.887638183,2.75,-6.41375626));
#100276=CARTESIAN_POINT('Ctrl Pts',(3.88410974146778,2.74934665560115,-6.41589499172907));
#100277=CARTESIAN_POINT('Ctrl Pts',(3.88058129993557,2.7486933112023,-6.41803372345814));
#100278=CARTESIAN_POINT('',(3.7201682340746,2.75000000185138,-6.36681621879948));
#100279=CARTESIAN_POINT('Ctrl Pts',(3.552698305,2.75,-6.319876166));
#100280=CARTESIAN_POINT('Ctrl Pts',(3.210236658,2.81435393,-6.512389893));
#100281=CARTESIAN_POINT('Ctrl Pts',(2.848977497,2.879481221,-6.666770374));
#100282=CARTESIAN_POINT('Ctrl Pts',(3.458818211,2.75,-6.654816044));
#100283=CARTESIAN_POINT('Ctrl Pts',(3.098206832,2.81435393,-6.84224259300001));
#100284=CARTESIAN_POINT('Ctrl Pts',(2.719453928,2.879481221,-6.989604448));
#100285=CARTESIAN_POINT('',(3.45881820097473,2.75,-6.65481604930514));
#100286=CARTESIAN_POINT('',(2.94987426729199,2.83963938428779,-6.89552331626262));
#100287=CARTESIAN_POINT('Origin',(-0.0581360810472636,2.94636920663246,
0.179358157749951));
#100288=CARTESIAN_POINT('Ctrl Pts',(2.85329262215939,2.87870320274543,-6.66492469653363));
#100289=CARTESIAN_POINT('Ctrl Pts',(2.86939945776764,2.87185457193515,-6.70328584159086));
#100290=CARTESIAN_POINT('Ctrl Pts',(2.88550969177699,2.86518067054803,-6.74170548506837));
#100291=CARTESIAN_POINT('Ctrl Pts',(2.91769714417173,2.85217081132374,-6.81855882132505));
#100292=CARTESIAN_POINT('Ctrl Pts',(2.93379364116285,2.84582706797916,-6.85703855007138));
#100293=CARTESIAN_POINT('Ctrl Pts',(2.9498742657648,2.83963938429177,-6.89552331690139));
#100294=CARTESIAN_POINT('',(3.50575824788625,2.74999999814853,-6.48734611046546));
#100295=CARTESIAN_POINT('Origin',(2.43511807940244E-13,2.84071505700011,
-7.83227649403528E-13));
#100296=CARTESIAN_POINT('',(2.949874267292,2.66036061571221,-6.89552331626262));
#100297=CARTESIAN_POINT('Origin',(-0.0581360810464882,2.55363079336866,
0.179358157747066));
#100298=CARTESIAN_POINT('',(2.41797934471617,2.75,-7.09953349747217));
#100299=CARTESIAN_POINT('Ctrl Pts',(2.41797934490384,2.75000000173934,-7.09953349716892));
#100300=CARTESIAN_POINT('Ctrl Pts',(2.56151675261816,2.72598918212304,-7.05064711788722));
#100301=CARTESIAN_POINT('Ctrl Pts',(2.70321150762957,2.70215892392445,-6.99752607038529));
#100302=CARTESIAN_POINT('Ctrl Pts',(2.84270721710102,2.67857142888649,-6.94039016746389));
#100303=CARTESIAN_POINT('Ctrl Pts',(2.87851415700855,2.67251679084317,-6.92572403990961));
#100304=CARTESIAN_POINT('Ctrl Pts',(2.91423882038528,2.6664461772466,-6.91076800243955));
#100305=CARTESIAN_POINT('Ctrl Pts',(2.94987426738843,2.66036061550281,-6.89552331657164));
#100306=CARTESIAN_POINT('Ctrl Pts',(2.94987426738843,2.83963938449719,-6.89552331657164));
#100307=CARTESIAN_POINT('Ctrl Pts',(2.91423882038527,2.8335538227534,-6.91076800243956));
#100308=CARTESIAN_POINT('Ctrl Pts',(2.87851415728558,2.82748320916599,-6.92572403998946));
#100309=CARTESIAN_POINT('Ctrl Pts',(2.84270721710102,2.82142857111351,-6.94039016746388));
#100310=CARTESIAN_POINT('Ctrl Pts',(2.70321150655026,2.79784107603985,-6.99752607007421));
#100311=CARTESIAN_POINT('Ctrl Pts',(2.56151675261817,2.77401081787678,-7.05064711788719));
#100312=CARTESIAN_POINT('Ctrl Pts',(2.41797934490384,2.74999999826065,-7.09953349716892));
#100313=CARTESIAN_POINT('Ctrl Pts',(2.86334288997134,2.88054032922091,-6.66038437985894));
#100314=CARTESIAN_POINT('Ctrl Pts',(2.69645140622961,2.85083482752464,-6.7321321221731));
#100315=CARTESIAN_POINT('Ctrl Pts',(2.52617600579015,2.821428571,-6.79543136056091));
#100316=CARTESIAN_POINT('Ctrl Pts',(2.32060444466131,2.785926731,-6.87185181346664));
#100317=CARTESIAN_POINT('Ctrl Pts',(2.11078936785013,2.75,-6.93570622463011));
#100318=CARTESIAN_POINT('Ctrl Pts',(2.10540952396099,2.74907880688478,-6.93734350813192));
#100319=CARTESIAN_POINT('Ctrl Pts',(2.10002968007185,2.74815761376957,-6.93898079163371));
#100320=CARTESIAN_POINT('Ctrl Pts',(3.18673687309472,2.88054032922091,-6.78930836744132));
#100321=CARTESIAN_POINT('Ctrl Pts',(3.01661489805259,2.85083482752464,-6.86915950063725));
#100322=CARTESIAN_POINT('Ctrl Pts',(2.842707217,2.821428571,-6.940390168));
#100323=CARTESIAN_POINT('Ctrl Pts',(2.632750443,2.785926731,-7.026386145));
#100324=CARTESIAN_POINT('Ctrl Pts',(2.417979356,2.75,-7.099533494));
#100325=CARTESIAN_POINT('Ctrl Pts',(2.41247243563221,2.74907880688478,-7.10140905663594));
#100326=CARTESIAN_POINT('Ctrl Pts',(2.40696551526442,2.74815761376956,-7.10328461927189));
#100327=CARTESIAN_POINT('',(2.26451548255993,2.75000000185138,-7.01768979653022));
#100328=CARTESIAN_POINT('Ctrl Pts',(2.111051631,2.75,-6.93584609200001));
#100329=CARTESIAN_POINT('Ctrl Pts',(1.735211787,2.81435393,-7.050239824));
#100330=CARTESIAN_POINT('Ctrl Pts',(1.349211424,2.879481221,-7.12335093400001));
#100331=CARTESIAN_POINT('Ctrl Pts',(1.947364229,2.75,-7.242773817));
#100332=CARTESIAN_POINT('Ctrl Pts',(1.554892575,2.81435393,-7.34829765));
#100333=CARTESIAN_POINT('Ctrl Pts',(1.153316261,2.879481221,-7.410793588));
#100334=CARTESIAN_POINT('',(1.94736421802029,2.75,-7.24277381984604));
#100335=CARTESIAN_POINT('',(1.39857416315072,2.83963938425915,-7.36844558274882));
#100336=CARTESIAN_POINT('Origin',(-0.0182202012778113,2.94636924245329,
0.187662522287977));
#100337=CARTESIAN_POINT('Ctrl Pts',(1.35382242975619,2.87870320279233,-7.12247603185831));
#100338=CARTESIAN_POINT('Ctrl Pts',(1.36130618454109,2.8718545719451,-7.1634028081296));
#100339=CARTESIAN_POINT('Ctrl Pts',(1.36878068266059,2.8651806705191,-7.20438744592115));
#100340=CARTESIAN_POINT('Ctrl Pts',(1.38369441476349,2.85217081129476,-7.28636334460521));
#100341=CARTESIAN_POINT('Ctrl Pts',(1.39114258031019,2.84582706794182,-7.32740370979372));
#100342=CARTESIAN_POINT('Ctrl Pts',(1.39857416152078,2.83963938426313,-7.36844558304456));
#100343=CARTESIAN_POINT('',(2.02920791894779,2.74999999814853,-7.08930995766353));
#100344=CARTESIAN_POINT('Origin',(-2.39825520553794E-13,2.84071505700044,
1.3240276930393E-12));
#100345=CARTESIAN_POINT('',(1.39857416315073,2.66036061574086,-7.36844558274881));
#100346=CARTESIAN_POINT('Origin',(-0.0182202012776395,2.5536307575481,0.187662522285998));
#100347=CARTESIAN_POINT('',(0.835258490224588,2.75,-7.45334443388523));
#100348=CARTESIAN_POINT('Ctrl Pts',(0.835258490482039,2.75000000173934,
-7.45334443370948));
#100349=CARTESIAN_POINT('Ctrl Pts',(0.985949199742631,2.72598918212304,
-7.43645729020576));
#100350=CARTESIAN_POINT('Ctrl Pts',(1.13575066492352,2.70215892392457,-7.41503836687994));
#100351=CARTESIAN_POINT('Ctrl Pts',(1.28426757234363,2.67857142890408,-7.38922572369872));
#100352=CARTESIAN_POINT('Ctrl Pts',(1.32239014986553,2.67251679087538,-7.38259991596011));
#100353=CARTESIAN_POINT('Ctrl Pts',(1.36049469628082,2.66644617726638,-7.37567328884459));
#100354=CARTESIAN_POINT('Ctrl Pts',(1.39857416317938,2.66036061553191,-7.36844558307566));
#100355=CARTESIAN_POINT('Ctrl Pts',(1.39857416317937,2.83963938446809,-7.36844558307567));
#100356=CARTESIAN_POINT('Ctrl Pts',(1.36049469628082,2.83355382273362,-7.37567328884459));
#100357=CARTESIAN_POINT('Ctrl Pts',(1.32239014995584,2.82748320915589,-7.38259991584564));
#100358=CARTESIAN_POINT('Ctrl Pts',(1.28426757232936,2.82142857109592,-7.38922572368795));
#100359=CARTESIAN_POINT('Ctrl Pts',(1.1357506645018,2.79784107595362,-7.4150383672732));
#100360=CARTESIAN_POINT('Ctrl Pts',(0.985949199742657,2.77401081787678,
-7.43645729020573));
#100361=CARTESIAN_POINT('Ctrl Pts',(0.835258490482038,2.74999999826065,
-7.45334443370947));
#100362=CARTESIAN_POINT('Ctrl Pts',(1.36461376391627,2.88054032957737,-7.12020237567227));
#100363=CARTESIAN_POINT('Ctrl Pts',(1.18620046619936,2.85083482770118,-7.15439595949493));
#100364=CARTESIAN_POINT('Ctrl Pts',(1.00629854418785,2.821428571,-7.17961111971661));
#100365=CARTESIAN_POINT('Ctrl Pts',(0.789104992932871,2.785926731,-7.21005309657259));
#100366=CARTESIAN_POINT('Ctrl Pts',(0.570468464739401,2.75,-7.22731058680332));
#100367=CARTESIAN_POINT('Ctrl Pts',(0.564862430624157,2.74907880681559,
-7.22775308412879));
#100368=CARTESIAN_POINT('Ctrl Pts',(0.559256396508915,2.74815761363118,
-7.22819558145427));
#100369=CARTESIAN_POINT('Ctrl Pts',(1.65273212970456,2.88054032957737,-7.31563233797624));
#100370=CARTESIAN_POINT('Ctrl Pts',(1.46942187764671,2.85083482770118,-7.35704540162157));
#100371=CARTESIAN_POINT('Ctrl Pts',(1.284267572,2.821428571,-7.389225724));
#100372=CARTESIAN_POINT('Ctrl Pts',(1.060732878,2.785926731,-7.428076663));
#100373=CARTESIAN_POINT('Ctrl Pts',(0.835258502,2.75,-7.453344433));
#100374=CARTESIAN_POINT('Ctrl Pts',(0.829477139414281,2.74907880681559,
-7.45399232098928));
#100375=CARTESIAN_POINT('Ctrl Pts',(0.823695776828564,2.74815761363118,
-7.45464020897858));
#100376=CARTESIAN_POINT('',(0.702976504056814,2.75000000185138,-7.34042399909589));
#100377=CARTESIAN_POINT('Ctrl Pts',(0.570694529,2.75,-7.227503563));
#100378=CARTESIAN_POINT('Ctrl Pts',(0.179050341,2.81435393,-7.258428376));
#100379=CARTESIAN_POINT('Ctrl Pts',(-0.213642275,2.879481221,-7.246851522));
#100380=CARTESIAN_POINT('Ctrl Pts',(0.344853659,2.75,-7.492067535));
#100381=CARTESIAN_POINT('Ctrl Pts',(-0.06112673,2.81435393,-7.510754476));
#100382=CARTESIAN_POINT('Ctrl Pts',(-0.466749192,2.879481221,-7.485462256));
#100383=CARTESIAN_POINT('Ctrl Pts',(-0.208950993846245,2.8787032027828,
-7.24698830451023));
#100384=CARTESIAN_POINT('Ctrl Pts',(-0.210440252485708,2.87185457196389,
-7.28856702129115));
#100385=CARTESIAN_POINT('Ctrl Pts',(-0.211950989736505,2.86518067057272,
-7.33020025685042));
#100386=CARTESIAN_POINT('Ctrl Pts',(-0.215008327563085,2.85217081134745,
-7.41346561591905));
#100387=CARTESIAN_POINT('Ctrl Pts',(-0.216556761366686,2.84582706794544,
-7.45514761582421));
#100388=CARTESIAN_POINT('Ctrl Pts',(-0.21812171594292,2.83963938424759,
-7.49682752321784));
#100389=CARTESIAN_POINT('',(0.457774082526124,2.74999999814853,-7.35978554971367));
#100390=CARTESIAN_POINT('Ctrl Pts',(-0.204199974,2.879480225,-7.247123731));
#100391=CARTESIAN_POINT('Ctrl Pts',(-0.382551049,2.85030975,-7.242098388));
#100392=CARTESIAN_POINT('Ctrl Pts',(-0.560439023,2.821428571,-7.228306033));
#100393=CARTESIAN_POINT('Ctrl Pts',(-0.779105665,2.785926731,-7.211351947));
#100394=CARTESIAN_POINT('Ctrl Pts',(-0.996347613999999,2.75,-7.181211));
#100395=CARTESIAN_POINT('Ctrl Pts',(-1.00029826040238,2.74934665560115,
-7.18066287278802));
#100396=CARTESIAN_POINT('Ctrl Pts',(-1.00424890680475,2.7486933112023,-7.18011474557605));
#100397=CARTESIAN_POINT('Ctrl Pts',(0.034740338,2.879480225,-7.49991954));
#100398=CARTESIAN_POINT('Ctrl Pts',(-0.14983202,2.85030975,-7.500774497));
#100399=CARTESIAN_POINT('Ctrl Pts',(-0.334222997,2.821428571,-7.492549298));
#100400=CARTESIAN_POINT('Ctrl Pts',(-0.560883377,2.785926731,-7.482438573));
#100401=CARTESIAN_POINT('Ctrl Pts',(-0.786518112,2.75,-7.45864527));
#100402=CARTESIAN_POINT('Ctrl Pts',(-0.790621385139384,2.74934665560115,
-7.45821257766166));
#100403=CARTESIAN_POINT('Ctrl Pts',(-0.794724658278769,2.7486933112023,
-7.45777988532332));
#100404=CARTESIAN_POINT('',(-0.891432874411234,2.75000000185138,-7.31992813361032));
#100405=CARTESIAN_POINT('Ctrl Pts',(-0.996347614,2.75,-7.181211));
#100406=CARTESIAN_POINT('Ctrl Pts',(-1.3854833,2.81435393,-7.127220885));
#100407=CARTESIAN_POINT('Ctrl Pts',(-1.766506299,2.879481221,-7.031497386));
#100408=CARTESIAN_POINT('Ctrl Pts',(-1.273781884,2.75,-7.391040503));
#100409=CARTESIAN_POINT('Ctrl Pts',(-1.674287817,2.81435393,-7.32201677));
#100410=CARTESIAN_POINT('Ctrl Pts',(-2.064989971,2.879481221,-7.210119029));
#100411=CARTESIAN_POINT('',(-1.27378189515849,2.75,-7.39104050096434));
#100412=CARTESIAN_POINT('',(-1.82461846250296,2.83963938428032,-7.27466614086713));
#100413=CARTESIAN_POINT('Origin',(0.0622612227616864,2.94636923860537,0.177968265673633));
#100414=CARTESIAN_POINT('Ctrl Pts',(-1.76195410140001,2.87870320274956,
-7.03263945744517));
#100415=CARTESIAN_POINT('Ctrl Pts',(-1.77234673711184,2.87185457193404,
-7.07292594060115));
#100416=CARTESIAN_POINT('Ctrl Pts',(-1.78277206917022,2.86518067054195,
-7.11326105058591));
#100417=CARTESIAN_POINT('Ctrl Pts',(-1.80365751908978,2.85217081132598,
-7.19392247482129));
#100418=CARTESIAN_POINT('Ctrl Pts',(-1.8141301492228,2.84582706796081,-7.23429710511575));
#100419=CARTESIAN_POINT('Ctrl Pts',(-1.82461846412333,2.83963938428433,
-7.27466614044675));
#100420=CARTESIAN_POINT('',(-1.13506476035904,2.74999999814853,-7.28612574973044));
#100421=CARTESIAN_POINT('Origin',(1.92337465398928E-13,2.84071505700033,
8.8557633448616E-13));
#100422=CARTESIAN_POINT('',(-1.82461846250295,2.66036061571968,-7.27466614086712));
#100423=CARTESIAN_POINT('Origin',(0.0622612227626687,2.55363076139464,0.177968265676951));
#100424=CARTESIAN_POINT('',(-2.3715180240997,2.75,-7.11518813898183));
#100425=CARTESIAN_POINT('Ctrl Pts',(-2.37151802375132,2.75000000173934,
-7.11518813880764));
#100426=CARTESIAN_POINT('Ctrl Pts',(-2.22766411164902,2.7259891821231,-7.16313516951371));
#100427=CARTESIAN_POINT('Ctrl Pts',(-2.08271441129929,2.70215892392426,
-7.20659588422854));
#100428=CARTESIAN_POINT('Ctrl Pts',(-1.93708566943587,2.67857142885868,
-7.24552959465705));
#100429=CARTESIAN_POINT('Ctrl Pts',(-1.89970445058239,2.67251679081792,
-7.25552342898784));
#100430=CARTESIAN_POINT('Ctrl Pts',(-1.86221328573061,2.66644617725889,
-7.26523667630949));
#100431=CARTESIAN_POINT('Ctrl Pts',(-1.82461846261757,2.66036061550997,
-7.27466614118873));
#100432=CARTESIAN_POINT('Ctrl Pts',(-1.82461846261757,2.83963938449003,
-7.27466614118873));
#100433=CARTESIAN_POINT('Ctrl Pts',(-1.86221328573062,2.83355382274111,
-7.2652366763095));
#100434=CARTESIAN_POINT('Ctrl Pts',(-1.89970445061032,2.8274832091563,-7.25552342919053));
#100435=CARTESIAN_POINT('Ctrl Pts',(-1.93708566943587,2.82142857114132,
-7.24552959465706));
#100436=CARTESIAN_POINT('Ctrl Pts',(-2.0827144111905,2.79784107617617,-7.20659588343893));
#100437=CARTESIAN_POINT('Ctrl Pts',(-2.22766411164898,2.77401081787672,
-7.16313516951369));
#100438=CARTESIAN_POINT('Ctrl Pts',(-2.37151802375131,2.74999999826065,
-7.11518813880763));
#100439=CARTESIAN_POINT('Ctrl Pts',(-1.75734327,2.879480225,-7.033793047));
#100440=CARTESIAN_POINT('Ctrl Pts',(-1.930444297,2.85030975,-6.990544984));
#100441=CARTESIAN_POINT('Ctrl Pts',(-2.1012084,2.821428571,-6.938834431));
#100442=CARTESIAN_POINT('Ctrl Pts',(-2.31111811,2.785926731,-6.875269858));
#100443=CARTESIAN_POINT('Ctrl Pts',(-2.516801651,2.75,-6.799132993));
#100444=CARTESIAN_POINT('Ctrl Pts',(-2.52054210234939,2.74934665560115,
-6.79774840851628));
#100445=CARTESIAN_POINT('Ctrl Pts',(-2.52428255369877,2.7486933112023,-6.79636382403254));
#100446=CARTESIAN_POINT('Ctrl Pts',(-1.578332876,2.879480225,-7.332043735));
#100447=CARTESIAN_POINT('Ctrl Pts',(-1.758773826,2.85030975,-7.29320110200001));
#100448=CARTESIAN_POINT('Ctrl Pts',(-1.93708567,2.821428571,-7.245529595));
#100449=CARTESIAN_POINT('Ctrl Pts',(-2.156273349,2.785926731,-7.18692997));
#100450=CARTESIAN_POINT('Ctrl Pts',(-2.371518013,2.75,-7.115188143));
#100451=CARTESIAN_POINT('Ctrl Pts',(-2.37543233784093,2.74934665560115,
-7.11388348433696));
#100452=CARTESIAN_POINT('Ctrl Pts',(-2.37934666268186,2.7486933112023,-7.11257882567393));
#100453=CARTESIAN_POINT('',(-2.44415984284571,2.75000000185138,-6.95716056418973));
#100454=CARTESIAN_POINT('Ctrl Pts',(-2.516801651,2.75,-6.799132993));
#100455=CARTESIAN_POINT('Ctrl Pts',(-2.885233281,2.81435393,-6.662752466));
#100456=CARTESIAN_POINT('Ctrl Pts',(-3.236770452,2.879481221,-6.487358248));
#100457=CARTESIAN_POINT('Ctrl Pts',(-2.832856802,2.75,-6.944416631));
#100458=CARTESIAN_POINT('Ctrl Pts',(-3.209161066,2.81435393,-6.79090969800001));
#100459=CARTESIAN_POINT('Ctrl Pts',(-3.566674115,2.879481221,-6.59763865));
#100460=CARTESIAN_POINT('',(-2.83285681245535,2.75,-6.94441662660179));
#100461=CARTESIAN_POINT('',(-3.34579807948844,2.83963938429423,-6.71234945516635));
#100462=CARTESIAN_POINT('Origin',(0.0990635273127888,2.94636920486568,0.16042320697258));
#100463=CARTESIAN_POINT('Ctrl Pts',(-3.23257019394498,2.8787032027684,-6.4894522063135));
#100464=CARTESIAN_POINT('Ctrl Pts',(-3.25138025846878,2.87185457193376,
-6.52656270441233));
#100465=CARTESIAN_POINT('Ctrl Pts',(-3.27023270836533,2.86518067053059,
-6.56371366377399));
#100466=CARTESIAN_POINT('Ctrl Pts',(-3.30796968985539,2.85217081132906,
-6.63799951434366));
#100467=CARTESIAN_POINT('Ctrl Pts',(-3.32687682777823,2.84582706796692,
-6.67517890235472));
#100468=CARTESIAN_POINT('Ctrl Pts',(-3.34579808097769,2.83963938429823,
-6.71234945440893));
#100469=CARTESIAN_POINT('',(-2.67482923721307,2.74999999814853,-6.87177480782995));
#100470=CARTESIAN_POINT('Origin',(-8.69530142333375E-14,2.84071505699933,
-1.02348685082632E-13));
#100471=CARTESIAN_POINT('',(-3.34579807948842,2.66036061570577,-6.71234945516632));
#100472=CARTESIAN_POINT('Origin',(0.0990635273070517,2.55363079513323,0.160423206958388));
#100473=CARTESIAN_POINT('',(-3.84562837697436,2.75,-6.43903272068618));
#100474=CARTESIAN_POINT('Ctrl Pts',(-3.84562837659874,2.75000000173934,
-6.43903272059439));
#100475=CARTESIAN_POINT('Ctrl Pts',(-3.71544488347682,2.72598918212305,
-6.51678311509396));
#100476=CARTESIAN_POINT('Ctrl Pts',(-3.58322679552254,2.70215892392445,
-6.5903876432404));
#100477=CARTESIAN_POINT('Ctrl Pts',(-3.44937236946746,2.67857142888618,
-6.6597169799323));
#100478=CARTESIAN_POINT('Ctrl Pts',(-3.41501348176197,2.67251679084659,
-6.67751302125371));
#100479=CARTESIAN_POINT('Ctrl Pts',(-3.38048690047503,2.66644617724843,
-6.69505867042727));
#100480=CARTESIAN_POINT('Ctrl Pts',(-3.34579807966921,2.66036061549648,
-6.71234945545536));
#100481=CARTESIAN_POINT('Ctrl Pts',(-3.34579807966923,2.83963938450351,
-6.7123494554554));
#100482=CARTESIAN_POINT('Ctrl Pts',(-3.38048690047503,2.83355382275157,
-6.69505867042736));
#100483=CARTESIAN_POINT('Ctrl Pts',(-3.41501348171708,2.82748320916218,
-6.67751302126219));
#100484=CARTESIAN_POINT('Ctrl Pts',(-3.44937236946741,2.82142857111382,
-6.65971697993242));
#100485=CARTESIAN_POINT('Ctrl Pts',(-3.58322679569734,2.79784107604138,
-6.59038764320792));
#100486=CARTESIAN_POINT('Ctrl Pts',(-3.71544488347676,2.77401081787677,
-6.51678311509403));
#100487=CARTESIAN_POINT('Ctrl Pts',(-3.84562837659873,2.74999999826065,
-6.43903272059438));
#100488=CARTESIAN_POINT('Ctrl Pts',(-3.22260332935241,2.88054032962933,
-6.49417280112119));
#100489=CARTESIAN_POINT('Ctrl Pts',(-3.38532999374888,2.85083482772692,
-6.41342294922764));
#100490=CARTESIAN_POINT('Ctrl Pts',(-3.54380823152172,2.821428571,-6.32462455818216));
#100491=CARTESIAN_POINT('Ctrl Pts',(-3.73513721104557,2.785926731,-6.21741926817495));
#100492=CARTESIAN_POINT('Ctrl Pts',(-3.91963602296178,2.75,-6.09884464776978));
#100493=CARTESIAN_POINT('Ctrl Pts',(-3.92436673545407,2.74907880688562,
-6.09580428977402));
#100494=CARTESIAN_POINT('Ctrl Pts',(-3.92909744794634,2.74815761377124,
-6.09276393177824));
#100495=CARTESIAN_POINT('Ctrl Pts',(-3.11150347067144,2.88054032962933,
-6.82411504555695));
#100496=CARTESIAN_POINT('Ctrl Pts',(-3.28249760950799,2.85083482772692,
-6.74614906006595));
#100497=CARTESIAN_POINT('Ctrl Pts',(-3.44937237,2.821428571,-6.65971698));
#100498=CARTESIAN_POINT('Ctrl Pts',(-3.650838376,2.785926731,-6.55536851));
#100499=CARTESIAN_POINT('Ctrl Pts',(-3.845628367,2.75,-6.439032727));
#100500=CARTESIAN_POINT('Ctrl Pts',(-3.85062295441346,2.74907880688562,
-6.43604977477271));
#100501=CARTESIAN_POINT('Ctrl Pts',(-3.85561754182692,2.74815761377124,
-6.43306682254543));
#100502=CARTESIAN_POINT('',(-3.88260061277304,2.75000000185138,-6.26908389894731));
#100503=CARTESIAN_POINT('Ctrl Pts',(-3.919572839,2.75,-6.099135083));
#100504=CARTESIAN_POINT('Ctrl Pts',(-4.250072961,2.81435393,-5.886741148));
#100505=CARTESIAN_POINT('Ctrl Pts',(-4.555686816,2.879481221,-5.63987744800001));
#100506=CARTESIAN_POINT('Ctrl Pts',(-4.259470484,2.75,-6.173079555));
#100507=CARTESIAN_POINT('Ctrl Pts',(-4.593977511,2.81435393,-5.942267236));
#100508=CARTESIAN_POINT('Ctrl Pts',(-4.901584541,2.879481221,-5.67666002));
#100509=CARTESIAN_POINT('',(-4.25947049338054,2.75,-6.17307954862385));
#100510=CARTESIAN_POINT('',(-4.71053189666572,2.83963938430234,-5.83617076883909));
#100511=CARTESIAN_POINT('Origin',(0.131233580395995,2.94636921249293,0.135376684318178));
#100512=CARTESIAN_POINT('Ctrl Pts',(-4.55203489665337,2.87870320274035,
-5.64282538217238));
#100513=CARTESIAN_POINT('Ctrl Pts',(-4.57838285257828,2.87185457192953,
-5.67502464964238));
#100514=CARTESIAN_POINT('Ctrl Pts',(-4.60478090062114,2.86518067054936,
-5.70725432072026));
#100515=CARTESIAN_POINT('Ctrl Pts',(-4.65760487443965,2.85217081131047,
-5.77169107409159));
#100516=CARTESIAN_POINT('Ctrl Pts',(-4.68406244312412,2.84582706798356,
-5.80393675270542));
#100517=CARTESIAN_POINT('Ctrl Pts',(-4.71053189794207,2.83963938430632,
-5.83617076779177));
#100518=CARTESIAN_POINT('',(-4.08952167106617,2.74999999814853,-6.13610731262445));
#100519=CARTESIAN_POINT('Origin',(-3.57786716920216E-13,2.84071505699989,
-4.45823933326039E-13));
#100520=CARTESIAN_POINT('',(-4.71053189666556,2.66036061569762,-5.83617076883885));
#100521=CARTESIAN_POINT('Origin',(0.131233580279342,2.55363078748444,0.135376684142551));
#100522=CARTESIAN_POINT('',(-5.1399214203484,2.75,-5.4617952896511));
#100523=CARTESIAN_POINT('Ctrl Pts',(-5.1399214199973,2.75000000173934,-5.46179528967991));
#100524=CARTESIAN_POINT('Ctrl Pts',(-5.02949558164935,2.72598918212305,
-5.56571352588234));
#100525=CARTESIAN_POINT('Ctrl Pts',(-4.91619147725867,2.70215892392415,
-5.66602020133334));
#100526=CARTESIAN_POINT('Ctrl Pts',(-4.80037025126701,2.67857142884375,
-5.76250340104977));
#100527=CARTESIAN_POINT('Ctrl Pts',(-4.77064027777155,2.67251679078282,
-5.78726952594611));
#100528=CARTESIAN_POINT('Ctrl Pts',(-4.74069270475776,2.66644617723471,
-5.81182716194082));
#100529=CARTESIAN_POINT('Ctrl Pts',(-4.71053189688486,2.66036061548689,
-5.83617076905788));
#100530=CARTESIAN_POINT('Ctrl Pts',(-4.71053189688485,2.83963938451312,
-5.83617076905789));
#100531=CARTESIAN_POINT('Ctrl Pts',(-4.7406927047578,2.83355382276527,-5.8118271619421));
#100532=CARTESIAN_POINT('Ctrl Pts',(-4.77064027797896,2.82748320917259,
-5.78726952596174));
#100533=CARTESIAN_POINT('Ctrl Pts',(-4.80037025126685,2.82142857115626,
-5.7625034010515));
#100534=CARTESIAN_POINT('Ctrl Pts',(-4.91619147645074,2.79784107624942,
-5.66602020128021));
#100535=CARTESIAN_POINT('Ctrl Pts',(-5.02949558164928,2.77401081787677,
-5.56571352588347));
#100536=CARTESIAN_POINT('Ctrl Pts',(-5.13992141999731,2.74999999826065,
-5.46179528967991));
#100537=CARTESIAN_POINT('Ctrl Pts',(-4.548334599,2.879480225,-5.64580839));
#100538=CARTESIAN_POINT('Ctrl Pts',(-4.687277446,2.85030975,-5.533874277));
#100539=CARTESIAN_POINT('Ctrl Pts',(-4.82054605,2.821428571,-5.415241063));
#100540=CARTESIAN_POINT('Ctrl Pts',(-4.984364872,2.785926731,-5.26941262000001));
#100541=CARTESIAN_POINT('Ctrl Pts',(-5.139069158,2.75,-5.113948395));
#100542=CARTESIAN_POINT('Ctrl Pts',(-5.14188252776459,2.74934665560115,
-5.11112120538942));
#100543=CARTESIAN_POINT('Ctrl Pts',(-5.14469589752919,2.7486933112023,-5.10829401577884));
#100544=CARTESIAN_POINT('Ctrl Pts',(-4.511101379,2.879480225,-5.991657896));
#100545=CARTESIAN_POINT('Ctrl Pts',(-4.658555551,2.85030975,-5.880640089));
#100546=CARTESIAN_POINT('Ctrl Pts',(-4.800370252,2.821428571,-5.762503401));
#100547=CARTESIAN_POINT('Ctrl Pts',(-4.974694258,2.785926731,-5.617285305));
#100548=CARTESIAN_POINT('Ctrl Pts',(-5.139921412,2.75,-5.461795298));
#100549=CARTESIAN_POINT('Ctrl Pts',(-5.14292614503858,2.74934665560115,
-5.4589676395317));
#100550=CARTESIAN_POINT('Ctrl Pts',(-5.14593087807715,2.7486933112023,-5.4561399810634));
#100551=CARTESIAN_POINT('',(-5.13949529324341,2.75000000185138,-5.2878718384879));
#100552=CARTESIAN_POINT('Ctrl Pts',(-5.139069158,2.75,-5.113948395));
#100553=CARTESIAN_POINT('Ctrl Pts',(-5.416183953,2.81435393,-4.83547235600001));
#100554=CARTESIAN_POINT('Ctrl Pts',(-5.661584328,2.879481221,-4.528682248));
#100555=CARTESIAN_POINT('Ctrl Pts',(-5.48691606,2.75,-5.113096141));
#100556=CARTESIAN_POINT('Ctrl Pts',(-5.763984674,2.81435393,-4.815770962));
#100557=CARTESIAN_POINT('Ctrl Pts',(-6.007302322,2.879481221,-4.490247077));
#100558=CARTESIAN_POINT('',(-5.48691606779505,2.75000000000002,-5.11309613274603));
#100559=CARTESIAN_POINT('',(-5.85500647817754,2.83963938428039,-4.68709922414167));
#100560=CARTESIAN_POINT('Origin',(0.157267369836855,2.94636927201175,0.104000280378761));
#100561=CARTESIAN_POINT('Ctrl Pts',(-5.6586515072673,2.87870320275799,-4.53234631572629));
#100562=CARTESIAN_POINT('Ctrl Pts',(-5.69130535301401,2.87185457194846,
-4.55812875035173));
#100563=CARTESIAN_POINT('Ctrl Pts',(-5.72401465585923,2.86518067057082,
-4.58393010943499));
#100564=CARTESIAN_POINT('Ctrl Pts',(-5.7894556316736,2.85217081134139,-4.63550477407209));
#100565=CARTESIAN_POINT('Ctrl Pts',(-5.82222650503423,2.84582706798315,
-4.66130897145861));
#100566=CARTESIAN_POINT('Ctrl Pts',(-5.85500647919594,2.83963938428437,
-4.68709922284821));
#100567=CARTESIAN_POINT('',(-5.31299261697924,2.74999999814684,-5.11352225970951));
#100568=CARTESIAN_POINT('Origin',(-2.55871712706579E-14,2.84071505700033,
2.47198095326695E-14));
#100569=CARTESIAN_POINT('',(-5.85500647817749,2.66036061571961,-4.68709922414165));
#100570=CARTESIAN_POINT('Origin',(0.157267369807963,2.55363072798491,0.104000280351224));
#100571=CARTESIAN_POINT('',(-6.19387745226799,2.75,-4.22917037999045));
#100572=CARTESIAN_POINT('Ctrl Pts',(-6.19387745202191,2.75000000173934,
-4.22917038015593));
#100573=CARTESIAN_POINT('Ctrl Pts',(-6.10837265719485,2.72598918212311,
-4.35439735677576));
#100574=CARTESIAN_POINT('Ctrl Pts',(-6.01928050973812,2.70215892392435,
-4.47671595142935));
#100575=CARTESIAN_POINT('Ctrl Pts',(-5.92690815539044,2.67857142887217,
-4.59584156796461));
#100576=CARTESIAN_POINT('Ctrl Pts',(-5.90319723703065,2.67251679082422,
-4.62641973990005));
#100577=CARTESIAN_POINT('Ctrl Pts',(-5.8792289873938,2.66644617724722,-4.65684107515696));
#100578=CARTESIAN_POINT('Ctrl Pts',(-5.85500647842804,2.66036061550761,
-4.68709922429958));
#100579=CARTESIAN_POINT('Ctrl Pts',(-5.85500647842804,2.83963938449239,
-4.68709922429957));
#100580=CARTESIAN_POINT('Ctrl Pts',(-5.87922898739386,2.83355382275278,
-4.65684107515717));
#100581=CARTESIAN_POINT('Ctrl Pts',(-5.90319723711639,2.82748320916694,
-4.6264197401748));
#100582=CARTESIAN_POINT('Ctrl Pts',(-5.92690815539048,2.82142857112784,
-4.59584156796493));
#100583=CARTESIAN_POINT('Ctrl Pts',(-6.01928050940444,2.79784107611009,
-4.47671595036035));
#100584=CARTESIAN_POINT('Ctrl Pts',(-6.10837265719485,2.77401081787671,
-4.35439735677597));
#100585=CARTESIAN_POINT('Ctrl Pts',(-6.1938774520219,2.74999999826065,-4.22917038015593));
#100586=CARTESIAN_POINT('Ctrl Pts',(-5.655678979,2.879480225,-4.536055036));
#100587=CARTESIAN_POINT('Ctrl Pts',(-5.767310893,2.85030975,-4.396869275));
#100588=CARTESIAN_POINT('Ctrl Pts',(-5.871961118,2.821428571,-4.25236083));
#100589=CARTESIAN_POINT('Ctrl Pts',(-6.000601142,2.785926731,-4.074725571));
#100590=CARTESIAN_POINT('Ctrl Pts',(-6.118268315,2.75,-3.889639164));
#100591=CARTESIAN_POINT('Ctrl Pts',(-6.12040814754998,2.74934665560115,
-3.88627328116149));
#100592=CARTESIAN_POINT('Ctrl Pts',(-6.12254798009995,2.7486933112023,-3.88290739832298));
#100593=CARTESIAN_POINT('Ctrl Pts',(-5.693663671,2.879480225,-4.881822815));
#100594=CARTESIAN_POINT('Ctrl Pts',(-5.8138049,2.85030975,-4.741702254));
#100595=CARTESIAN_POINT('Ctrl Pts',(-5.926908156,2.821428571,-4.595841568));
#100596=CARTESIAN_POINT('Ctrl Pts',(-6.06593896600001,2.785926731,-4.416544081));
#100597=CARTESIAN_POINT('Ctrl Pts',(-6.193877446,2.75,-4.22917039));
#100598=CARTESIAN_POINT('Ctrl Pts',(-6.19620406706957,2.74934665560115,
-4.22576291183265));
#100599=CARTESIAN_POINT('Ctrl Pts',(-6.19853068813914,2.7486933112023,-4.22235543366531));
#100600=CARTESIAN_POINT('',(-6.15607288682832,2.75000000185138,-4.05940476740313));
#100601=CARTESIAN_POINT('Ctrl Pts',(-6.118268315,2.75,-3.889639164));
#100602=CARTESIAN_POINT('Ctrl Pts',(-6.32904020300001,2.81435393,-3.55810225));
#100603=CARTESIAN_POINT('Ctrl Pts',(-6.502752449,2.879481221,-3.205730898));
#100604=CARTESIAN_POINT('Ctrl Pts',(-6.45779954,2.75,-3.814030034));
#100605=CARTESIAN_POINT('Ctrl Pts',(-6.664474319,2.81435393,-3.464094591));
#100606=CARTESIAN_POINT('Ctrl Pts',(-6.832125323,2.879481221,-3.093875171));
#100607=CARTESIAN_POINT('',(-6.45779954578553,2.75,-3.81403002424441));
#100608=CARTESIAN_POINT('',(-6.72570746383011,2.83963938432043,-3.31886412904555));
#100609=CARTESIAN_POINT('Origin',(0.175947461605686,2.94636924508285,0.067760940793829));
#100610=CARTESIAN_POINT('Ctrl Pts',(-6.50067586214128,2.8787032027215,-3.20993977181558));
#100611=CARTESIAN_POINT('Ctrl Pts',(-6.53810874055978,2.87185457190171,
-3.22809981590397));
#100612=CARTESIAN_POINT('Ctrl Pts',(-6.57559984766339,2.86518067052256,
-3.24626642040999));
#100613=CARTESIAN_POINT('Ctrl Pts',(-6.65059787826818,2.85217081130526,
-3.28256742285789));
#100614=CARTESIAN_POINT('Ctrl Pts',(-6.68814972626432,2.84582706800102,
-3.30072356335558));
#100615=CARTESIAN_POINT('Ctrl Pts',(-6.72570746453642,2.83963938432441,
-3.31886412758459));
#100616=CARTESIAN_POINT('',(-6.288033933505,2.74999999814853,-3.85183458919698));
#100617=CARTESIAN_POINT('Origin',(-1.03302782994419E-12,2.84071505699978,
-5.41450564939261E-13));
#100618=CARTESIAN_POINT('',(-6.7257074638301,2.66036061567957,-3.31886412904556));
#100619=CARTESIAN_POINT('Origin',(0.175947461606183,2.55363075491703,0.0677609407940782));
#100620=CARTESIAN_POINT('',(-6.95821465711167,2.75,-2.79879416493425));
#100621=CARTESIAN_POINT('Ctrl Pts',(-6.958214656765,2.75000000173934,-2.79879416509168));
#100622=CARTESIAN_POINT('Ctrl Pts',(-6.9016290152138,2.72598918212306,-2.93947440757433));
#100623=CARTESIAN_POINT('Ctrl Pts',(-6.84091467506888,2.70215892392413,
-3.07808543914549));
#100624=CARTESIAN_POINT('Ctrl Pts',(-6.77631042134925,2.67857142884028,
-3.21428329038083));
#100625=CARTESIAN_POINT('Ctrl Pts',(-6.7597272540588,2.67251679076156,-3.24924370862982));
#100626=CARTESIAN_POINT('Ctrl Pts',(-6.74285905662865,2.66644617720877,
-3.28410627512915));
#100627=CARTESIAN_POINT('Ctrl Pts',(-6.72570746404163,2.66036061546033,
-3.31886412911155));
#100628=CARTESIAN_POINT('Ctrl Pts',(-6.72570746404163,2.83963938453967,
-3.31886412911154));
#100629=CARTESIAN_POINT('Ctrl Pts',(-6.74285905662865,2.83355382279123,
-3.28410627512915));
#100630=CARTESIAN_POINT('Ctrl Pts',(-6.75972725426173,2.82748320918954,
-3.24924370852248));
#100631=CARTESIAN_POINT('Ctrl Pts',(-6.77631042134924,2.82142857115972,
-3.21428329038083));
#100632=CARTESIAN_POINT('Ctrl Pts',(-6.84091467427833,2.79784107626641,
-3.07808543956365));
#100633=CARTESIAN_POINT('Ctrl Pts',(-6.90162901521376,2.77401081787676,
-2.93947440757435));
#100634=CARTESIAN_POINT('Ctrl Pts',(-6.958214656765,2.74999999826065,-2.79879416509168));
#100635=CARTESIAN_POINT('Ctrl Pts',(-6.498570095,2.879480225,-3.21420079));
#100636=CARTESIAN_POINT('Ctrl Pts',(-6.577671293,2.85030975,-3.054271554));
#100637=CARTESIAN_POINT('Ctrl Pts',(-6.64880981,2.821428571,-2.890644931));
#100638=CARTESIAN_POINT('Ctrl Pts',(-6.736255972,2.785926731,-2.689508882));
#100639=CARTESIAN_POINT('Ctrl Pts',(-6.811384045,2.75,-2.483454729));
#100640=CARTESIAN_POINT('Ctrl Pts',(-6.81275028412961,2.74934665560115,
-2.47970753789814));
#100641=CARTESIAN_POINT('Ctrl Pts',(-6.81411652325921,2.7486933112023,-2.47596034679627));
#100642=CARTESIAN_POINT('Ctrl Pts',(-6.609996578,2.879480225,-3.543719125));
#100643=CARTESIAN_POINT('Ctrl Pts',(-6.69720719300001,2.85030975,-3.381047692));
#100644=CARTESIAN_POINT('Ctrl Pts',(-6.776310422,2.821428571,-3.21428329));
#100645=CARTESIAN_POINT('Ctrl Pts',(-6.87354710900001,2.785926731,-3.009290165));
#100646=CARTESIAN_POINT('Ctrl Pts',(-6.958214653,2.75,-2.798794176));
#100647=CARTESIAN_POINT('Ctrl Pts',(-6.9597543718694,2.74934665560115,-2.79496620803394));
#100648=CARTESIAN_POINT('Ctrl Pts',(-6.96129409073881,2.7486933112023,-2.79113824006787));
#100649=CARTESIAN_POINT('',(-6.88479935311732,2.75000000185138,-2.6411244417671));
#100650=CARTESIAN_POINT('Ctrl Pts',(-6.811384045,2.75,-2.483454729));
#100651=CARTESIAN_POINT('Ctrl Pts',(-6.945957567,2.81435393,-2.114359238));
#100652=CARTESIAN_POINT('Ctrl Pts',(-7.039859092,2.879481221,-1.732883135));
#100653=CARTESIAN_POINT('Ctrl Pts',(-7.12672349100001,2.75,-2.336624121));
#100654=CARTESIAN_POINT('Ctrl Pts',(-7.253340552,2.81435393,-1.950441006));
#100655=CARTESIAN_POINT('Ctrl Pts',(-7.33748573700001,2.879481221,-1.5528371));
#100656=CARTESIAN_POINT('',(-7.12672349453342,2.75,-2.33662411022232));
#100657=CARTESIAN_POINT('',(-7.28192184370656,2.83963938427376,-1.79544263556377));
#100658=CARTESIAN_POINT('Origin',(0.186400573970105,2.94636923522301,0.0283532430203706));
#100659=CARTESIAN_POINT('Ctrl Pts',(-7.03873583813264,2.87870320277747,
-1.73744001214091));
#100660=CARTESIAN_POINT('Ctrl Pts',(-7.07919742953855,2.87185457196145,
-1.74712852185622));
#100661=CARTESIAN_POINT('Ctrl Pts',(-7.11971729855279,2.86518067056953,
-1.75681092128746));
#100662=CARTESIAN_POINT('Ctrl Pts',(-7.20076555952284,2.85217081132604,
-1.7761408666784));
#100663=CARTESIAN_POINT('Ctrl Pts',(-7.24134249982081,2.84582706798385,
-1.78579998946225));
#100664=CARTESIAN_POINT('Ctrl Pts',(-7.28192184408587,2.83963938427774,
-1.79544263397008));
#100665=CARTESIAN_POINT('',(-6.96905377175724,2.74999999814853,-2.41003941413528));
#100666=CARTESIAN_POINT('Origin',(2.18575157973078E-13,2.84071505699989,
8.64109131470947E-14));
#100667=CARTESIAN_POINT('',(-7.28192184370656,2.66036061572624,-1.79544263556378));
#100668=CARTESIAN_POINT('Origin',(0.18640057397059,2.55363076477878,0.0283532430206035));
#100669=CARTESIAN_POINT('',(-7.3971934794137,2.75,-1.23754944427177));
#100670=CARTESIAN_POINT('Ctrl Pts',(-7.39719347933202,2.75000000173934,
-1.23754944453735));
#100671=CARTESIAN_POINT('Ctrl Pts',(-7.37217287192558,2.72598918212305,
-1.38710490209901));
#100672=CARTESIAN_POINT('Ctrl Pts',(-7.34267527326005,2.70215892392471,
-1.53552707352338));
#100673=CARTESIAN_POINT('Ctrl Pts',(-7.30885994283025,2.67857142892459,
-1.682428699378));
#100674=CARTESIAN_POINT('Ctrl Pts',(-7.30017993773283,2.67251679088925,
-1.7201366528899));
#100675=CARTESIAN_POINT('Ctrl Pts',(-7.29120053043776,2.66644617724762,
-1.75781031566047));
#100676=CARTESIAN_POINT('Ctrl Pts',(-7.28192184397542,2.66036061551178,
-1.79544263559539));
#100677=CARTESIAN_POINT('Ctrl Pts',(-7.28192184397542,2.83963938448822,
-1.79544263559538));
#100678=CARTESIAN_POINT('Ctrl Pts',(-7.29120053043776,2.83355382275238,
-1.75781031566047));
#100679=CARTESIAN_POINT('Ctrl Pts',(-7.30017993742646,2.82748320916779,
-1.72013665290894));
#100680=CARTESIAN_POINT('Ctrl Pts',(-7.30885994269999,2.82142857107541,
-1.68242869918427));
#100681=CARTESIAN_POINT('Ctrl Pts',(-7.34267527381588,2.79784107585308,
-1.53552707250072));
#100682=CARTESIAN_POINT('Ctrl Pts',(-7.37217287192555,2.77401081787677,
-1.38710490209903));
#100683=CARTESIAN_POINT('Ctrl Pts',(-7.39719347933202,2.74999999826065,
-1.23754944453735));
#100684=CARTESIAN_POINT('Ctrl Pts',(-7.037595296,2.879480225,-1.742054088));
#100685=CARTESIAN_POINT('Ctrl Pts',(-7.080467094,2.85030975,-1.568859488));
#100686=CARTESIAN_POINT('Ctrl Pts',(-7.114767544,2.821428571,-1.393765687));
#100687=CARTESIAN_POINT('Ctrl Pts',(-7.156930959,2.785926731,-1.178533747));
#100688=CARTESIAN_POINT('Ctrl Pts',(-7.186007028,2.75,-0.961146711));
#100689=CARTESIAN_POINT('Ctrl Pts',(-7.18653578990772,2.74934665560115,
-0.9571934261227));
#100690=CARTESIAN_POINT('Ctrl Pts',(-7.18706455181544,2.7486933112023,-0.953240141245399));
#100691=CARTESIAN_POINT('Ctrl Pts',(-7.217253392,2.879480225,-2.039915067));
#100692=CARTESIAN_POINT('Ctrl Pts',(-7.26745552200001,2.85030975,-1.862299097));
#100693=CARTESIAN_POINT('Ctrl Pts',(-7.308859943,2.821428571,-1.682428699));
#100694=CARTESIAN_POINT('Ctrl Pts',(-7.359755829,2.785926731,-1.461325186));
#100695=CARTESIAN_POINT('Ctrl Pts',(-7.39719347800001,2.75,-1.237549456));
#100696=CARTESIAN_POINT('Ctrl Pts',(-7.39787429914903,2.74934665560115,
-1.23347998973562));
#100697=CARTESIAN_POINT('Ctrl Pts',(-7.39855512029806,2.7486933112023,-1.22941052347124));
#100698=CARTESIAN_POINT('',(-7.2916002547138,2.75000000185138,-1.09934807213293));
#100699=CARTESIAN_POINT('Ctrl Pts',(-7.186007028,2.75,-0.961146711));
#100700=CARTESIAN_POINT('Ctrl Pts',(-7.238089675,2.81435393,-0.571751139));
#100701=CARTESIAN_POINT('Ctrl Pts',(-7.247789749,2.879481221,-0.179007682));
#100702=CARTESIAN_POINT('Ctrl Pts',(-7.462409772,2.75,-0.749960261));
#100703=CARTESIAN_POINT('Ctrl Pts',(-7.503048642,2.81435393,-0.345586968));
#100704=CARTESIAN_POINT('Ctrl Pts',(-7.499753473,2.879481221,0.060809907));
#100705=CARTESIAN_POINT('',(-7.46240977317129,2.75,-0.749960249718469));
#100706=CARTESIAN_POINT('',(-7.49764165152831,2.83963938428599,-0.188068240164113));
#100707=CARTESIAN_POINT('Origin',(0.18813789085566,2.94636921308583,-0.0123802379614946));
#100708=CARTESIAN_POINT('Ctrl Pts',(-7.24767235005792,2.87870320272657,
-0.183699488584397));
#100709=CARTESIAN_POINT('Ctrl Pts',(-7.28927071525243,2.87185457192322,
-0.184463440225009));
#100710=CARTESIAN_POINT('Ctrl Pts',(-7.33092468187684,2.86518067054497,
-0.185208896527471));
#100711=CARTESIAN_POINT('Ctrl Pts',(-7.41423344644177,2.85217081131025,
-0.186663938230128));
#100712=CARTESIAN_POINT('Ctrl Pts',(-7.45593814635207,2.84582706796522,
-0.187374393336462));
#100713=CARTESIAN_POINT('Ctrl Pts',(-7.49764165155662,2.83963938428999,
-0.188068238498512));
#100714=CARTESIAN_POINT('',(-7.32420840133381,2.74999999814853,-0.855553474581588));
#100715=CARTESIAN_POINT('Origin',(6.61363325216158E-13,2.84071505700056,
8.93111539584934E-14));
#100716=CARTESIAN_POINT('',(-7.49764165152831,2.66036061571401,-0.188068240164119));
#100717=CARTESIAN_POINT('Origin',(0.188137890860158,2.55363078691417,-0.0123802379614915));
#100718=CARTESIAN_POINT('',(-7.49028775502938,2.75,0.381561712766595));
#100719=CARTESIAN_POINT('Ctrl Pts',(-7.49028775483674,2.75000000173934,
0.381561712481001));
#100720=CARTESIAN_POINT('Ctrl Pts',(-7.49800211813204,2.72598918212311,
0.230124087868946));
#100721=CARTESIAN_POINT('Ctrl Pts',(-7.50110053690817,2.70215892392423,
0.0788308326963932));
#100722=CARTESIAN_POINT('Ctrl Pts',(-7.49965529763164,2.67857142885476,
-0.0719056115850236));
#100723=CARTESIAN_POINT('Ctrl Pts',(-7.49928432131415,2.67251679080789,
-0.110597918899535));
#100724=CARTESIAN_POINT('Ctrl Pts',(-7.4986135715597,2.66644617725217,-0.149321099433654));
#100725=CARTESIAN_POINT('Ctrl Pts',(-7.49764165186744,2.66036061550535,
-0.188068240139857));
#100726=CARTESIAN_POINT('Ctrl Pts',(-7.49764165186744,2.83963938449465,
-0.188068240139847));
#100727=CARTESIAN_POINT('Ctrl Pts',(-7.49861357155971,2.83355382274783,
-0.149321099433649));
#100728=CARTESIAN_POINT('Ctrl Pts',(-7.4992843213749,2.8274832091614,-0.110597918759457));
#100729=CARTESIAN_POINT('Ctrl Pts',(-7.49965529763164,2.82142857114524,
-0.0719056115850307));
#100730=CARTESIAN_POINT('Ctrl Pts',(-7.50110053667153,2.79784107619542,
0.0788308321506787));
#100731=CARTESIAN_POINT('Ctrl Pts',(-7.49800211813201,2.77401081787671,
0.230124087868916));
#100732=CARTESIAN_POINT('Ctrl Pts',(-7.49028775483674,2.74999999826065,
0.381561712481007));
#100733=CARTESIAN_POINT('Ctrl Pts',(-7.247550363,2.879480225,-0.188450873));
#100734=CARTESIAN_POINT('Ctrl Pts',(-7.252188123,2.85030975,-0.010089297));
#100735=CARTESIAN_POINT('Ctrl Pts',(-7.248046656,2.821428571,0.168284491));
#100736=CARTESIAN_POINT('Ctrl Pts',(-7.242955809,2.785926731,0.387548315));
#100737=CARTESIAN_POINT('Ctrl Pts',(-7.224620308,2.75,0.606103459));
#100738=CARTESIAN_POINT('Ctrl Pts',(-7.22428686834254,2.74934665560115,
0.610077986467366));
#100739=CARTESIAN_POINT('Ctrl Pts',(-7.22395342868507,2.7486933112023,0.614052513934733));
#100740=CARTESIAN_POINT('Ctrl Pts',(-7.487039458,2.879480225,-0.440726847));
#100741=CARTESIAN_POINT('Ctrl Pts',(-7.497885707,2.85030975,-0.256471467));
#100742=CARTESIAN_POINT('Ctrl Pts',(-7.499655298,2.821428571,-0.071905611));
#100743=CARTESIAN_POINT('Ctrl Pts',(-7.501830546,2.785926731,0.154969736));
#100744=CARTESIAN_POINT('Ctrl Pts',(-7.490287756,2.75,0.381561701));
#100745=CARTESIAN_POINT('Ctrl Pts',(-7.49007784496764,2.74934665560115,
0.385682381814436));
#100746=CARTESIAN_POINT('Ctrl Pts',(-7.48986793393528,2.7486933112023,0.389803062628871));
#100747=CARTESIAN_POINT('',(-7.35745403123015,2.75000000185138,0.493832591469735));
#100748=CARTESIAN_POINT('Ctrl Pts',(-7.224620308,2.75,0.606103459));
#100749=CARTESIAN_POINT('Ctrl Pts',(-7.19177675500001,2.81435393,0.997591409));
#100750=CARTESIAN_POINT('Ctrl Pts',(-7.116821813,2.879481221,1.383237971));
#100751=CARTESIAN_POINT('Ctrl Pts',(-7.44916206600001,2.75,0.871770907));
#100752=CARTESIAN_POINT('Ctrl Pts',(-7.401922517,2.81435393,1.275426333));
#100753=CARTESIAN_POINT('Ctrl Pts',(-7.311341072,2.879481221,1.671613511));
#100754=CARTESIAN_POINT('',(-7.4491620646855,2.75,0.871770918265686));
#100755=CARTESIAN_POINT('',(-7.36278006843227,2.83963938429796,1.4281000172255));
#100756=CARTESIAN_POINT('Origin',(0.181077865154473,2.94636922108518,-0.052534871448249));
#100757=CARTESIAN_POINT('Ctrl Pts',(-7.11771575851598,2.87870320271664,
1.37863061888998));
#100758=CARTESIAN_POINT('Ctrl Pts',(-7.15850580391357,2.87185457189991,
1.38682694679702));
#100759=CARTESIAN_POINT('Ctrl Pts',(-7.1993461750297,2.86518067050694,1.39505329048376));
#100760=CARTESIAN_POINT('Ctrl Pts',(-7.28102001766141,2.85217081130069,
1.41154118876166));
#100761=CARTESIAN_POINT('Ctrl Pts',(-7.32190241154598,2.84582706797934,
1.41981262145295));
#100762=CARTESIAN_POINT('Ctrl Pts',(-7.36278006810718,2.83963938430194,
1.428100018832));
#100763=CARTESIAN_POINT('',(-7.33689118584801,2.74999999814853,0.738937194438185));
#100764=CARTESIAN_POINT('Origin',(1.19479079407903E-12,2.84071505700056,
-3.3957212042246E-13));
#100765=CARTESIAN_POINT('',(-7.36278006843227,2.66036061570204,1.4281000172255));
#100766=CARTESIAN_POINT('Origin',(0.181077865154028,2.5536307789163,-0.0525348714478818));
#100767=CARTESIAN_POINT('',(-7.23314450045272,2.75,1.98283146826368));
#100768=CARTESIAN_POINT('Ctrl Pts',(-7.23314450039587,2.75000000173934,
1.98283146796251));
#100769=CARTESIAN_POINT('Ctrl Pts',(-7.27323311869183,2.72598918212307,
1.83659273035069));
#100770=CARTESIAN_POINT('Ctrl Pts',(-7.30878267557167,2.70215892392438,
1.68950269573436));
#100771=CARTESIAN_POINT('Ctrl Pts',(-7.33977510491094,2.67857142887669,
1.54197970238118));
#100772=CARTESIAN_POINT('Ctrl Pts',(-7.34773050433874,2.67251679082118,
1.50411225081318));
#100773=CARTESIAN_POINT('Ctrl Pts',(-7.35539977549778,2.66644617723181,
1.46615020532329));
#100774=CARTESIAN_POINT('Ctrl Pts',(-7.36278006869151,2.66036061548774,
1.42810001731005));
#100775=CARTESIAN_POINT('Ctrl Pts',(-7.36278006869151,2.83963938451226,
1.42810001731005));
#100776=CARTESIAN_POINT('Ctrl Pts',(-7.35539977549778,2.83355382276819,
1.4661502053233));
#100777=CARTESIAN_POINT('Ctrl Pts',(-7.34773050418597,2.82748320917567,
1.50411225092341));
#100778=CARTESIAN_POINT('Ctrl Pts',(-7.33977510486803,2.82142857112331,
1.54197970240722));
#100779=CARTESIAN_POINT('Ctrl Pts',(-7.30878267595674,2.7978410760879,1.68950269543247));
#100780=CARTESIAN_POINT('Ctrl Pts',(-7.27323311869181,2.77401081787675,
1.83659273035066));
#100781=CARTESIAN_POINT('Ctrl Pts',(-7.23314450039587,2.74999999826065,
1.98283146796251));
#100782=CARTESIAN_POINT('Ctrl Pts',(-7.11959786607701,2.88054032779396,
1.36776416485828));
#100783=CARTESIAN_POINT('Ctrl Pts',(-7.08532534214618,2.8508348268179,1.54616231001887));
#100784=CARTESIAN_POINT('Ctrl Pts',(-7.04216107449507,2.821428571,1.72262009544759));
#100785=CARTESIAN_POINT('Ctrl Pts',(-6.99004934207468,2.785926731,1.93565558493594));
#100786=CARTESIAN_POINT('Ctrl Pts',(-6.92515542781633,2.75,2.145151485466));
#100787=CARTESIAN_POINT('Ctrl Pts',(-6.92349149172195,2.74907880754079,
2.15052314156808));
#100788=CARTESIAN_POINT('Ctrl Pts',(-6.92182755562759,2.74815761508157,
2.15589479767016));
#100789=CARTESIAN_POINT('Ctrl Pts',(-7.40779135236163,2.88054032779396,
1.17244499782585));
#100790=CARTESIAN_POINT('Ctrl Pts',(-7.37841300668275,2.8508348268179,1.35806450323592));
#100791=CARTESIAN_POINT('Ctrl Pts',(-7.339775105,2.821428571,1.541979703));
#100792=CARTESIAN_POINT('Ctrl Pts',(-7.293128004,2.785926731,1.764018444));
#100793=CARTESIAN_POINT('Ctrl Pts',(-7.233144504,2.75,1.982831457));
#100794=CARTESIAN_POINT('Ctrl Pts',(-7.23160647517469,2.74907880754079,
1.98844201192505));
#100795=CARTESIAN_POINT('Ctrl Pts',(-7.23006844634938,2.74815761508157,
1.9940525668501));
#100796=CARTESIAN_POINT('',(-7.0792814352825,2.75000000185138,2.06392219203608));
#100797=CARTESIAN_POINT('Ctrl Pts',(-6.925418373,2.75,2.145012905));
#100798=CARTESIAN_POINT('Ctrl Pts',(-6.809184347,2.81435393,2.520287691));
#100799=CARTESIAN_POINT('Ctrl Pts',(-6.653079198,2.879481221,2.880804954));
#100800=CARTESIAN_POINT('Ctrl Pts',(-7.087599821,2.75,2.452739036));
#100801=CARTESIAN_POINT('Ctrl Pts',(-6.954690722,2.81435393,2.836802116));
#100802=CARTESIAN_POINT('Ctrl Pts',(-6.781058488,2.879481221,3.204254325));
#100803=CARTESIAN_POINT('',(-7.08759981726226,2.75,2.45273904670858));
#100804=CARTESIAN_POINT('',(-6.88364307283612,2.83963938426474,2.97749190505679));
#100805=CARTESIAN_POINT('Origin',(0.165550829136227,2.94636919898514,-0.0902329832633514));
#100806=CARTESIAN_POINT('Ctrl Pts',(-6.65494268792754,2.8787032027829,2.87649749144771));
#100807=CARTESIAN_POINT('Ctrl Pts',(-6.69301711670703,2.87185457193056,
2.89327084769831));
#100808=CARTESIAN_POINT('Ctrl Pts',(-6.73113424203585,2.86518067051512,
2.91008433647982));
#100809=CARTESIAN_POINT('Ctrl Pts',(-6.8073541850895,2.85217081127456,2.94374421864197));
#100810=CARTESIAN_POINT('Ctrl Pts',(-6.84550265796655,2.84582706793118,
2.96061077606773));
#100811=CARTESIAN_POINT('Ctrl Pts',(-6.8836430721632,2.83963938426872,2.97749190657861));
#100812=CARTESIAN_POINT('',(-7.00650909341606,2.74999999814853,2.29887598142312));
#100813=CARTESIAN_POINT('Origin',(-1.346145417358E-12,2.84071505700011,
5.42317926677249E-13));
#100814=CARTESIAN_POINT('',(-6.88364307283612,2.66036061573526,2.97749190505678));
#100815=CARTESIAN_POINT('Origin',(0.165550829137875,2.55363080101485,-0.090232983264088));
#100816=CARTESIAN_POINT('',(-6.63778744815122,2.75,3.49138622725718));
#100817=CARTESIAN_POINT('Ctrl Pts',(-6.63778744812353,2.75000000173934,
3.49138622693142));
#100818=CARTESIAN_POINT('Ctrl Pts',(-6.708375822714,2.72598918212332,3.35718433829753));
#100819=CARTESIAN_POINT('Ctrl Pts',(-6.77471426039344,2.70215892392423,
3.22117529108411));
#100820=CARTESIAN_POINT('Ctrl Pts',(-6.83669518688489,2.67857142885406,
3.08376375931997));
#100821=CARTESIAN_POINT('Ctrl Pts',(-6.85260497599632,2.67251679081341,
3.04849180343724));
#100822=CARTESIAN_POINT('Ctrl Pts',(-6.86825566148464,2.66644617726573,
3.0130659561535));
#100823=CARTESIAN_POINT('Ctrl Pts',(-6.8836430731335,2.66036061552687,2.97749190522106));
#100824=CARTESIAN_POINT('Ctrl Pts',(-6.8836430731335,2.83963938447313,2.97749190522107));
#100825=CARTESIAN_POINT('Ctrl Pts',(-6.86825566148464,2.83355382273427,
3.01306595615351));
#100826=CARTESIAN_POINT('Ctrl Pts',(-6.85260497602587,2.82748320915501,
3.04849180358285));
#100827=CARTESIAN_POINT('Ctrl Pts',(-6.83669518688489,2.82142857114594,
3.08376375931997));
#100828=CARTESIAN_POINT('Ctrl Pts',(-6.77471426027832,2.79784107619884,
3.22117529051684));
#100829=CARTESIAN_POINT('Ctrl Pts',(-6.708375822714,2.77401081787672,3.35718433829754));
#100830=CARTESIAN_POINT('Ctrl Pts',(-6.63778744812352,2.74999999826066,
3.49138622693142));
#100831=CARTESIAN_POINT('Ctrl Pts',(-6.65911676148846,2.88054032844669,
2.86628968296735));
#100832=CARTESIAN_POINT('Ctrl Pts',(-6.58729518161321,2.85083482714118,
3.03314940069317));
#100833=CARTESIAN_POINT('Ctrl Pts',(-6.50720686179461,2.821428571,3.19620266055702));
#100834=CARTESIAN_POINT('Ctrl Pts',(-6.41051713982161,2.785926731,3.39305501682207));
#100835=CARTESIAN_POINT('Ctrl Pts',(-6.30210498255076,2.75,3.58370274611001));
#100836=CARTESIAN_POINT('Ctrl Pts',(-6.2993252004271,2.7490788073302,3.58859111991541));
#100837=CARTESIAN_POINT('Ctrl Pts',(-6.29654541830346,2.7481576146604,3.59347949372081));
#100838=CARTESIAN_POINT('Ctrl Pts',(-6.98256029174724,2.88054032844669,
2.73749004926488));
#100839=CARTESIAN_POINT('Ctrl Pts',(-6.91396608765727,2.85083482714118,
2.91245439970453));
#100840=CARTESIAN_POINT('Ctrl Pts',(-6.836695187,2.821428571,3.08376376));
#100841=CARTESIAN_POINT('Ctrl Pts',(-6.74340690300001,2.785926731,3.290583611));
#100842=CARTESIAN_POINT('Ctrl Pts',(-6.637787454,2.75,3.491386217));
#100843=CARTESIAN_POINT('Ctrl Pts',(-6.63507927934845,2.7490788073302,3.49653497068772));
#100844=CARTESIAN_POINT('Ctrl Pts',(-6.63237110469693,2.7481576146604,3.50168372437542));
#100845=CARTESIAN_POINT('',(-6.47008950698529,2.75000000185139,3.53750508408639));
#100846=CARTESIAN_POINT('Ctrl Pts',(-6.302391571,2.75,3.583623931));
#100847=CARTESIAN_POINT('Ctrl Pts',(-6.108202046,2.81435393,3.925138122));
#100848=CARTESIAN_POINT('Ctrl Pts',(-5.878245994,2.879481221,4.243668699));
#100849=CARTESIAN_POINT('Ctrl Pts',(-6.39462928600001,2.75,3.919019814));
#100850=CARTESIAN_POINT('Ctrl Pts',(-6.182265318,2.81435393,4.265532185));
#100851=CARTESIAN_POINT('Ctrl Pts',(-5.933701147,2.879481221,4.587067767));
#100852=CARTESIAN_POINT('',(-6.39462927992378,2.75,3.91901982357883));
#100853=CARTESIAN_POINT('',(-6.0826345771943,2.8396393843766,4.38765957983895));
#100854=CARTESIAN_POINT('Origin',(0.142282719380422,2.94636928188172,-0.123711824272659));
#100855=CARTESIAN_POINT('Ctrl Pts',(-5.88099189386276,2.87870320273351,
4.23986253753841));
#100856=CARTESIAN_POINT('Ctrl Pts',(-5.91457038781333,2.87185457194718,
4.2644286186552));
#100857=CARTESIAN_POINT('Ctrl Pts',(-5.94818195278064,2.86518067058278,
4.2890430724903));
#100858=CARTESIAN_POINT('Ctrl Pts',(-6.01538403650056,2.85217081134544,
4.33830103996495));
#100859=CARTESIAN_POINT('Ctrl Pts',(-6.04901480760903,2.84582706809447,
4.36297406019775));
#100860=CARTESIAN_POINT('Ctrl Pts',(-6.08263457640376,2.83963938437968,
4.38765958091638));
#100861=CARTESIAN_POINT('',(-6.34851042265171,2.74999999814853,3.75132188239731));
#100862=CARTESIAN_POINT('Ctrl Pts',(-5.8872627585203,2.8805403289085,4.23079068185782));
#100863=CARTESIAN_POINT('Ctrl Pts',(-5.78125041957623,2.85083482736991,
4.37830979712559));
#100864=CARTESIAN_POINT('Ctrl Pts',(-5.66798288841052,2.821428571,4.52033434203316));
#100865=CARTESIAN_POINT('Ctrl Pts',(-5.53123628067281,2.785926731,4.69179896798155));
#100866=CARTESIAN_POINT('Ctrl Pts',(-5.38437511387682,2.75,4.85468405041332));
#100867=CARTESIAN_POINT('Ctrl Pts',(-5.38060946525645,2.74907880723015,
4.85886056622971));
#100868=CARTESIAN_POINT('Ctrl Pts',(-5.37684381663609,2.7481576144603,4.8630370820461));
#100869=CARTESIAN_POINT('Ctrl Pts',(-6.23083247311669,2.8805403289085,4.17453311033498));
#100870=CARTESIAN_POINT('Ctrl Pts',(-6.12622979866047,2.85083482736991,
4.33066116654239));
#100871=CARTESIAN_POINT('Ctrl Pts',(-6.013939,2.821428571,4.48135445));
#100872=CARTESIAN_POINT('Ctrl Pts',(-5.87837158900001,2.785926731,4.663284745));
#100873=CARTESIAN_POINT('Ctrl Pts',(-5.73205484,2.75,4.836687639));
#100874=CARTESIAN_POINT('Ctrl Pts',(-5.72830315072755,2.74907880723015,
4.84113384069378));
#100875=CARTESIAN_POINT('Ctrl Pts',(-5.72455146145511,2.7481576144603,4.84558004238754));
#100876=CARTESIAN_POINT('',(-5.73205483199695,2.75,4.83668764768363));
#100877=CARTESIAN_POINT('Ctrl Pts',(-6.08263457751693,2.83963938452334,
4.38765958010009));
#100878=CARTESIAN_POINT('Ctrl Pts',(-6.05995954582765,2.83355382275396,
4.41909409084215));
#100879=CARTESIAN_POINT('Ctrl Pts',(-6.03705925485745,2.82748320915825,
4.45032726682969));
#100880=CARTESIAN_POINT('Ctrl Pts',(-6.01393899979816,2.82142857110512,
4.4813544495293));
#100881=CARTESIAN_POINT('Ctrl Pts',(-5.92386773399068,2.79784107599885,
4.60222930969558));
#100882=CARTESIAN_POINT('Ctrl Pts',(-5.82984232843352,2.77401081787658,
4.72079773781478));
#100883=CARTESIAN_POINT('Ctrl Pts',(-5.73205483213063,2.74999999826059,
4.83668764743604));
#100884=CARTESIAN_POINT('',(-5.55836338494564,2.75000000185147,4.84567817116543));
#100885=CARTESIAN_POINT('Origin',(6.31439345255558E-13,2.84071505699967,
-5.21718085400025E-13));
#100886=CARTESIAN_POINT('',(-6.08263457777298,2.66036061569962,4.38765957990834));
#100887=CARTESIAN_POINT('Origin',(0.142282947892951,2.55363074788761,-0.123711959058361));
#100888=CARTESIAN_POINT('Ctrl Pts',(-5.73205483213063,2.75000000173941,
4.83668764743604));
#100889=CARTESIAN_POINT('Ctrl Pts',(-5.82984232843352,2.72598918212338,
4.72079773781479));
#100890=CARTESIAN_POINT('Ctrl Pts',(-5.9238677351341,2.7021589239245,4.60222930920695));
#100891=CARTESIAN_POINT('Ctrl Pts',(-6.01393899979815,2.67857142889489,
4.48135444952932));
#100892=CARTESIAN_POINT('Ctrl Pts',(-6.0370592546571,2.67251679083703,4.45032726683011));
#100893=CARTESIAN_POINT('Ctrl Pts',(-6.0599595461582,2.66644617722229,4.4190940906906));
#100894=CARTESIAN_POINT('Ctrl Pts',(-6.08263457793126,2.66036061548051,
4.38765958006493));
#100895=CARTESIAN_POINT('Ctrl Pts',(-5.384671945,2.75,4.854668686));
#100896=CARTESIAN_POINT('Ctrl Pts',(-5.121607007,2.81435393,5.14645345700001));
#100897=CARTESIAN_POINT('Ctrl Pts',(-4.828552541,2.879481221,5.408103212));
#100898=CARTESIAN_POINT('Ctrl Pts',(-5.40265299200001,2.75,5.202051581));
#100899=CARTESIAN_POINT('Ctrl Pts',(-5.120764059,2.81435393,5.49481071));
#100900=CARTESIAN_POINT('Ctrl Pts',(-4.808890534,2.879481221,5.75539502));
#100901=CARTESIAN_POINT('',(-5.40265298407939,2.75,5.20205158911868));
#100902=CARTESIAN_POINT('',(-5.39366246066081,2.74999999814853,5.0283601419087));
#100903=CARTESIAN_POINT('',(-4.99720885004651,2.83963938428276,5.59266517060532));
#100904=CARTESIAN_POINT('Origin',(0.112362020446343,2.94636922241594,-0.151406233933549));
#100905=CARTESIAN_POINT('Ctrl Pts',(-4.83205245537769,2.87870320275158,
5.40497632385788));
#100906=CARTESIAN_POINT('Ctrl Pts',(-4.8595649216461,2.87185457192515,5.43618644745341));
#100907=CARTESIAN_POINT('Ctrl Pts',(-4.88709928706816,2.86518067051737,
5.46745092225138));
#100908=CARTESIAN_POINT('Ctrl Pts',(-4.94214121631759,2.85217081129803,
5.53000372745823));
#100909=CARTESIAN_POINT('Ctrl Pts',(-4.96968174897597,2.84582706796719,
5.5613295283599));
#100910=CARTESIAN_POINT('Ctrl Pts',(-4.99720884880956,2.83963938428673,
5.59266517169271));
#100911=CARTESIAN_POINT('Origin',(-2.57172755313562E-13,2.84071505700022,
2.98806118737005E-13));
#100912=CARTESIAN_POINT('',(-4.55829770235788,2.75,5.95583092881941));
#100913=CARTESIAN_POINT('Ctrl Pts',(-4.99720885021896,2.8396393844946,5.59266517084824));
#100914=CARTESIAN_POINT('Ctrl Pts',(-4.96830645736748,2.83355382275415,
5.61849029850888));
#100915=CARTESIAN_POINT('Ctrl Pts',(-4.93922735261419,2.82748320916757,
5.64407037449145));
#100916=CARTESIAN_POINT('Ctrl Pts',(-4.90997770917938,2.82142857112666,
5.66940198742473));
#100917=CARTESIAN_POINT('Ctrl Pts',(-4.79602773926675,2.79784107610431,
5.76808820007588));
#100918=CARTESIAN_POINT('Ctrl Pts',(-4.67871188691834,2.77401081787663,
5.86367188157641));
#100919=CARTESIAN_POINT('Ctrl Pts',(-4.55829770249563,2.74999999826059,
5.95583092854622));
#100920=CARTESIAN_POINT('',(-4.99720885004652,2.66036061571725,5.59266517060532));
#100921=CARTESIAN_POINT('Origin',(0.112362020508088,2.55363077759231,-0.151406233995569));
#100922=CARTESIAN_POINT('Ctrl Pts',(-4.55829770249563,2.75000000173941,
5.95583092854622));
#100923=CARTESIAN_POINT('Ctrl Pts',(-4.67871188691833,2.72598918212333,
5.86367188157641));
#100924=CARTESIAN_POINT('Ctrl Pts',(-4.7960277391387,2.70215892392436,5.76808820019688));
#100925=CARTESIAN_POINT('Ctrl Pts',(-4.90997770917935,2.67857142887334,
5.66940198742472));
#100926=CARTESIAN_POINT('Ctrl Pts',(-4.93922735264703,2.67251679082507,
5.64407037446037));
#100927=CARTESIAN_POINT('Ctrl Pts',(-4.96830645736746,2.66644617724585,
5.61849029850887));
#100928=CARTESIAN_POINT('Ctrl Pts',(-4.99720885021896,2.66036061550539,
5.59266517084823));
#100929=CARTESIAN_POINT('Ctrl Pts',(-4.83559480800001,2.879480225,5.401807369));
#100930=CARTESIAN_POINT('Ctrl Pts',(-4.702656805,2.85030975,5.520810931));
#100931=CARTESIAN_POINT('Ctrl Pts',(-4.564025943,2.821428571,5.633131207));
#100932=CARTESIAN_POINT('Ctrl Pts',(-4.393615631,2.785926731,5.771199548));
#100933=CARTESIAN_POINT('Ctrl Pts',(-4.215171043,2.75,5.89871452800001));
#100934=CARTESIAN_POINT('Ctrl Pts',(-4.21192594474503,2.74934665560115,
5.90103344752409));
#100935=CARTESIAN_POINT('Ctrl Pts',(-4.20868084649006,2.7486933112023,5.90335236704817));
#100936=CARTESIAN_POINT('Ctrl Pts',(-5.182911938,2.879480225,5.421016864));
#100937=CARTESIAN_POINT('Ctrl Pts',(-5.049501192,2.85030975,5.54856787));
#100938=CARTESIAN_POINT('Ctrl Pts',(-4.909977709,2.821428571,5.669401988));
#100939=CARTESIAN_POINT('Ctrl Pts',(-4.738470154,2.785926731,5.817935867));
#100940=CARTESIAN_POINT('Ctrl Pts',(-4.558297712,2.75,5.955830922));
#100941=CARTESIAN_POINT('Ctrl Pts',(-4.55502119191227,2.74934665560115,
5.95833860804061));
#100942=CARTESIAN_POINT('Ctrl Pts',(-4.55174467182455,2.7486933112023,5.96084629408121));
#100943=CARTESIAN_POINT('',(-4.38673436825944,2.75000000185146,5.92727273183888));
#100944=CARTESIAN_POINT('Ctrl Pts',(-4.215171043,2.75,5.89871452800001));
#100945=CARTESIAN_POINT('Ctrl Pts',(-3.895531316,2.81435393,6.127126348));
#100946=CARTESIAN_POINT('Ctrl Pts',(-3.553081338,2.879481221,6.31966083));
#100947=CARTESIAN_POINT('Ctrl Pts',(-4.158054649,2.75,6.241841198));
#100948=CARTESIAN_POINT('Ctrl Pts',(-3.819821564,2.81435393,6.467157993));
#100949=CARTESIAN_POINT('Ctrl Pts',(-3.459221545,2.879481221,6.654606397));
#100950=CARTESIAN_POINT('',(-4.15805463949679,2.75,6.24184120419392));
#100951=CARTESIAN_POINT('',(-3.67811919046932,2.83963938434862,6.53616395242618));
#100952=CARTESIAN_POINT('Origin',(0.077187090066142,2.9463692329547,-0.172020802380906));
#100953=CARTESIAN_POINT('Ctrl Pts',(-3.55717161501909,2.87870320271742,
6.31735942479319));
#100954=CARTESIAN_POINT('Ctrl Pts',(-3.57733160092653,2.87185457192173,
6.35375423980345));
#100955=CARTESIAN_POINT('Ctrl Pts',(-3.5975012901241,2.86518067055048,6.39020684292654));
#100956=CARTESIAN_POINT('Ctrl Pts',(-3.63780936552281,2.85217081133915,
6.46312958584068));
#100957=CARTESIAN_POINT('Ctrl Pts',(-3.65797189449222,2.84582706805202,
6.49964340700815));
#100958=CARTESIAN_POINT('Ctrl Pts',(-3.67811918906675,2.83963938435261,
6.53616395320061));
#100959=CARTESIAN_POINT('',(-4.18661283653578,2.7499999981484,6.07027786952739));
#100960=CARTESIAN_POINT('Origin',(8.23993651088983E-15,2.840715057,-8.23993651088983E-14));
#100961=CARTESIAN_POINT('',(-3.67811919046927,2.66036061565136,6.5361639524261));
#100962=CARTESIAN_POINT('Origin',(0.0771870900262217,2.55363076703895,-0.172020802323091));
#100963=CARTESIAN_POINT('',(-3.17139963915191,2.75,6.79648617466084));
#100964=CARTESIAN_POINT('Ctrl Pts',(-3.17139963931085,2.75000000173941,
6.79648617435012));
#100965=CARTESIAN_POINT('Ctrl Pts',(-3.30881007717435,2.72598918212335,
6.73236724563488));
#100966=CARTESIAN_POINT('Ctrl Pts',(-3.44393081564739,2.70215892392454,
6.66423769797584));
#100967=CARTESIAN_POINT('Ctrl Pts',(-3.57643131729758,2.67857142890089,
6.59235458861174));
#100968=CARTESIAN_POINT('Ctrl Pts',(-3.6104426685576,2.6725167908205,6.57390302330991));
#100969=CARTESIAN_POINT('Ctrl Pts',(-3.64434088045567,2.66644617717984,
6.55517214304717));
#100970=CARTESIAN_POINT('Ctrl Pts',(-3.67811919051385,2.66036061542591,
6.53616395257749));
#100971=CARTESIAN_POINT('Ctrl Pts',(-3.67811919051385,2.8396393845741,6.53616395257749));
#100972=CARTESIAN_POINT('Ctrl Pts',(-3.64434088045605,2.83355382282015,
6.55517214304733));
#100973=CARTESIAN_POINT('Ctrl Pts',(-3.61044266852075,2.82748320920675,
6.57390302316407));
#100974=CARTESIAN_POINT('Ctrl Pts',(-3.57643131723044,2.82142857109912,
6.59235458858938));
#100975=CARTESIAN_POINT('Ctrl Pts',(-3.44393081546194,2.79784107596927,
6.6642376984347));
#100976=CARTESIAN_POINT('Ctrl Pts',(-3.30881007717469,2.77401081787661,
6.732367245635));
#100977=CARTESIAN_POINT('Ctrl Pts',(-3.17139963931086,2.74999999826059,
6.79648617435011));
#100978=CARTESIAN_POINT('Ctrl Pts',(-3.56131238,2.879480225,6.315026059));
#100979=CARTESIAN_POINT('Ctrl Pts',(-3.405900146,2.85030975,6.402669643));
#100980=CARTESIAN_POINT('Ctrl Pts',(-3.246364857,2.821428571,6.482562396));
#100981=CARTESIAN_POINT('Ctrl Pts',(-3.050258032,2.785926731,6.580769596));
#100982=CARTESIAN_POINT('Ctrl Pts',(-2.848573427,2.75,6.666943035));
#100983=CARTESIAN_POINT('Ctrl Pts',(-2.84490569817126,2.74934665560115,
6.66851013927399));
#100984=CARTESIAN_POINT('Ctrl Pts',(-2.84123796934252,2.7486933112023,6.67007724354796));
#100985=CARTESIAN_POINT('Ctrl Pts',(-3.896379956,2.879480225,6.408449363));
#100986=CARTESIAN_POINT('Ctrl Pts',(-3.738668582,2.85030975,6.50433893));
#100987=CARTESIAN_POINT('Ctrl Pts',(-3.576431317,2.821428571,6.592354589));
#100988=CARTESIAN_POINT('Ctrl Pts',(-3.37700312,2.785926731,6.700546775));
#100989=CARTESIAN_POINT('Ctrl Pts',(-3.17139965,2.75,6.79648617));
#100990=CARTESIAN_POINT('Ctrl Pts',(-3.16766065477918,2.74934665560115,
6.7982308727494));
#100991=CARTESIAN_POINT('Ctrl Pts',(-3.16392165955837,2.7486933112023,6.79997557549878));
#100992=CARTESIAN_POINT('',(-3.00998652800533,2.75000000185147,6.73171460719254));
#100993=CARTESIAN_POINT('Ctrl Pts',(-2.848573427,2.75,6.666943035));
#100994=CARTESIAN_POINT('Ctrl Pts',(-2.48730491,2.81435393,6.82130162));
#100995=CARTESIAN_POINT('Ctrl Pts',(-2.111472,2.879481221,6.93571813100001));
#100996=CARTESIAN_POINT('Ctrl Pts',(-2.719030292,2.75,6.989769257));
#100997=CARTESIAN_POINT('Ctrl Pts',(-2.340268458,2.81435393,7.137108156));
#100998=CARTESIAN_POINT('Ctrl Pts',(-1.947803201,2.879481221,7.242655776));
#100999=CARTESIAN_POINT('',(-2.71903028147046,2.75,6.98976926121724));
#101000=CARTESIAN_POINT('',(-2.18704476574115,2.83963938432791,7.17403897303378));
#101001=CARTESIAN_POINT('Origin',(0.0384031144212466,2.94636922736759,-0.18459196964046));
#101002=CARTESIAN_POINT('Ctrl Pts',(-2.11596138231835,2.87870320278422,
6.9343498201285));
#101003=CARTESIAN_POINT('Ctrl Pts',(-2.12782622978281,2.87185457194067,
6.97422754562859));
#101004=CARTESIAN_POINT('Ctrl Pts',(-2.13968813088101,2.86518067053237,
7.01416379420402));
#101005=CARTESIAN_POINT('Ctrl Pts',(-2.1633775919085,2.85217081131246,7.09404668855678));
#101006=CARTESIAN_POINT('Ctrl Pts',(-2.17521934002718,2.84582706801463,
7.13404118468278));
#101007=CARTESIAN_POINT('Ctrl Pts',(-2.18704476419215,2.83963938433189,
7.17403897349237));
#101008=CARTESIAN_POINT('',(-2.78380184885462,2.74999999814853,6.82835615033994));
#101009=CARTESIAN_POINT('Origin',(4.54822811357669E-13,2.840715057,-1.85745516190217E-12));
#101010=CARTESIAN_POINT('',(-2.18704476574113,2.66036061567209,7.17403897303371));
#101011=CARTESIAN_POINT('Origin',(0.0384031144027247,2.55363077262798,-0.184591969595875));
#101012=CARTESIAN_POINT('',(-1.63621045241957,2.75,7.31934528129139));
#101013=CARTESIAN_POINT('Ctrl Pts',(-1.63621045262561,2.75000000173941,
7.31934528095056));
#101014=CARTESIAN_POINT('Ctrl Pts',(-1.78419198574281,2.72598918212331,
7.28626459934368));
#101015=CARTESIAN_POINT('Ctrl Pts',(-1.93079951578136,2.70215892392453,
7.24877484738345));
#101016=CARTESIAN_POINT('Ctrl Pts',(-2.0756549731527,2.67857142889793,7.2070560165367));
#101017=CARTESIAN_POINT('Ctrl Pts',(-2.11283769872407,2.67251679082882,
7.19634727361592));
#101018=CARTESIAN_POINT('Ctrl Pts',(-2.14996997488054,2.6664461772002,7.18534142458151));
#101019=CARTESIAN_POINT('Ctrl Pts',(-2.18704476576501,2.66036061545065,
7.17403897323128));
#101020=CARTESIAN_POINT('Ctrl Pts',(-2.18704476576502,2.83963938454935,
7.17403897323128));
#101021=CARTESIAN_POINT('Ctrl Pts',(-2.1499699748808,2.83355382279979,7.1853414245817));
#101022=CARTESIAN_POINT('Ctrl Pts',(-2.1128376989978,2.82748320919473,7.19634727365132));
#101023=CARTESIAN_POINT('Ctrl Pts',(-2.07565497315309,2.82142857110207,
7.20705601653691));
#101024=CARTESIAN_POINT('Ctrl Pts',(-1.93079951471658,2.79784107598374,
7.24877484724666));
#101025=CARTESIAN_POINT('Ctrl Pts',(-1.78419198574305,2.77401081787665,
7.28626459934383));
#101026=CARTESIAN_POINT('Ctrl Pts',(-1.63621045262561,2.74999999826059,
7.31934528095056));
#101027=CARTESIAN_POINT('Ctrl Pts',(-2.120506944,2.879480225,6.93296115));
#101028=CARTESIAN_POINT('Ctrl Pts',(-1.949887382,2.85030975,6.98514663800001));
#101029=CARTESIAN_POINT('Ctrl Pts',(-1.776907359,2.821428571,7.028876172));
#101030=CARTESIAN_POINT('Ctrl Pts',(-1.564273757,2.785926731,7.082630172));
#101031=CARTESIAN_POINT('Ctrl Pts',(-1.348779684,2.75,7.123432695));
#101032=CARTESIAN_POINT('Ctrl Pts',(-1.34486082353981,2.74934665560115,
7.12417470795578));
#101033=CARTESIAN_POINT('Ctrl Pts',(-1.34094196307961,2.7486933112023,7.12491672091157));
#101034=CARTESIAN_POINT('Ctrl Pts',(-2.427657577,2.879480225,7.096229893));
#101035=CARTESIAN_POINT('Ctrl Pts',(-2.253019985,2.85030975,7.155974331));
#101036=CARTESIAN_POINT('Ctrl Pts',(-2.075654973,2.821428571,7.207056017));
#101037=CARTESIAN_POINT('Ctrl Pts',(-1.857631174,2.785926731,7.269847562));
#101038=CARTESIAN_POINT('Ctrl Pts',(-1.636210464,2.75,7.319345279));
#101039=CARTESIAN_POINT('Ctrl Pts',(-1.63218382487528,2.74934665560115,
7.32024541812365));
#101040=CARTESIAN_POINT('Ctrl Pts',(-1.62815718575056,2.7486933112023,7.3211455572473));
#101041=CARTESIAN_POINT('',(-1.49249506274193,2.75000000185147,7.22138898932679));
#101042=CARTESIAN_POINT('Ctrl Pts',(-1.348779684,2.75,7.123432695));
#101043=CARTESIAN_POINT('Ctrl Pts',(-0.962774892000001,2.81435393,7.196520411));
#101044=CARTESIAN_POINT('Ctrl Pts',(-0.571132578,2.879481221,7.227468961));
#101045=CARTESIAN_POINT('Ctrl Pts',(-1.1528671,2.75,7.41086347500001));
#101046=CARTESIAN_POINT('Ctrl Pts',(-0.751286999,2.81435393,7.473335074));
#101047=CARTESIAN_POINT('Ctrl Pts',(-0.345307744,2.879481221,7.49204662));
#101048=CARTESIAN_POINT('',(-1.15286708880857,2.75,7.41086347684554));
#101049=CARTESIAN_POINT('',(-0.593706557887295,2.83963938429001,7.47646390471328));
#101050=CARTESIAN_POINT('Origin',(-0.00217653894457756,2.94636924407997,
-0.188531935449823));
#101051=CARTESIAN_POINT('Ctrl Pts',(-0.575811147992967,2.87870320269475,
7.22709772493196));
#101052=CARTESIAN_POINT('Ctrl Pts',(-0.578826069595871,2.87185457189305,
7.26859372276947));
#101053=CARTESIAN_POINT('Ctrl Pts',(-0.581825533002033,2.86518067051596,
7.31014624196717));
#101054=CARTESIAN_POINT('Ctrl Pts',(-0.587788686380652,2.85217081130779,
7.39325405240357));
#101055=CARTESIAN_POINT('Ctrl Pts',(-0.590755946430203,2.84582706796969,
7.43485912546498));
#101056=CARTESIAN_POINT('Ctrl Pts',(-0.593706556239983,2.83963938429398,
7.47646390483069));
#101057=CARTESIAN_POINT('',(-1.25082338067054,2.74999999814853,7.26714808695003));
#101058=CARTESIAN_POINT('Origin',(7.34360624610533E-14,2.84071505699978,
-7.24680732089311E-13));
#101059=CARTESIAN_POINT('',(-0.593706557887282,2.66036061570999,7.47646390471321));
#101060=CARTESIAN_POINT('Origin',(-0.00217653895281604,2.55363075591576,
-0.188531935399019));
#101061=CARTESIAN_POINT('',(-0.0245138841973356,2.75,7.49995993759332));
#101062=CARTESIAN_POINT('Ctrl Pts',(-0.0245138844723349,2.7500000017394,
7.49995993745986));
#101063=CARTESIAN_POINT('Ctrl Pts',(-0.176147060361898,2.72598918212328,
7.49946431871023));
#101064=CARTESIAN_POINT('Ctrl Pts',(-0.327386176079984,2.70215892392418,
7.49436734156413));
#101065=CARTESIAN_POINT('Ctrl Pts',(-0.477823308499627,2.67857142884758,
7.48476351549384));
#101066=CARTESIAN_POINT('Ctrl Pts',(-0.516438785871464,2.67251679079197,
7.48229832387388));
#101067=CARTESIAN_POINT('Ctrl Pts',(-0.555068861913598,2.66644617724321,
7.4795321272271));
#101068=CARTESIAN_POINT('Ctrl Pts',(-0.593706557878843,2.66036061549942,
7.47646390502461));
#101069=CARTESIAN_POINT('Ctrl Pts',(-0.593706557878851,2.83963938450059,
7.47646390502461));
#101070=CARTESIAN_POINT('Ctrl Pts',(-0.555068861913804,2.83355382275679,
7.47953212722733));
#101071=CARTESIAN_POINT('Ctrl Pts',(-0.516438785815961,2.82748320916829,
7.4822983240761));
#101072=CARTESIAN_POINT('Ctrl Pts',(-0.477823308499939,2.82142857115242,
7.48476351549411));
#101073=CARTESIAN_POINT('Ctrl Pts',(-0.327386176297452,2.7978410762306,
7.49436734077764));
#101074=CARTESIAN_POINT('Ctrl Pts',(-0.176147060362065,2.77401081787682,
7.49946431871042));
#101075=CARTESIAN_POINT('Ctrl Pts',(-0.0245138844723352,2.7499999982606,
7.49995993745986));
#101076=CARTESIAN_POINT('Ctrl Pts',(-0.586785048244814,2.88054032958409,
7.22600414473736));
#101077=CARTESIAN_POINT('Ctrl Pts',(-0.405720639388154,2.85083482770451,
7.24070741365988));
#101078=CARTESIAN_POINT('Ctrl Pts',(-0.224147072116056,2.821428571,7.24632394240433));
#101079=CARTESIAN_POINT('Ctrl Pts',(-0.00493536232790208,2.785926731,7.25310471367341));
#101080=CARTESIAN_POINT('Ctrl Pts',(0.214285371684215,2.75,7.24662227317082));
#101081=CARTESIAN_POINT('Ctrl Pts',(0.219906386668887,2.74907880660006,
7.24645605761933));
#101082=CARTESIAN_POINT('Ctrl Pts',(0.225527401653559,2.74815761320013,
7.24628984206785));
#101083=CARTESIAN_POINT('Ctrl Pts',(-0.852084755314493,2.88054032958409,
7.45143956339864));
#101084=CARTESIAN_POINT('Ctrl Pts',(-0.665371536520333,2.85083482770451,
7.47279053664977));
#101085=CARTESIAN_POINT('Ctrl Pts',(-0.477823308,2.821428571,7.484763516));
#101086=CARTESIAN_POINT('Ctrl Pts',(-0.251398459,2.785926731,7.499218357));
#101087=CARTESIAN_POINT('Ctrl Pts',(-0.024513896,2.75,7.499959938));
#101088=CARTESIAN_POINT('Ctrl Pts',(-0.0186963736102467,2.74907880660006,
7.49997895279773));
#101089=CARTESIAN_POINT('Ctrl Pts',(-0.0128788512204935,2.74815761320013,
7.49999796759543));
#101090=CARTESIAN_POINT('',(0.0947838119950076,2.75000000185146,7.37339924885223));
#101091=CARTESIAN_POINT('Ctrl Pts',(-1.649106096,3.007773793,7.31645058));
#101092=CARTESIAN_POINT('Ctrl Pts',(-1.248920843,3.07352872,7.40665114));
#101093=CARTESIAN_POINT('Ctrl Pts',(-0.841285031000001,3.138525418,7.452666603));
#101094=CARTESIAN_POINT('Ctrl Pts',(-0.837226499918957,3.13917254249503,
7.45312474524682));
#101095=CARTESIAN_POINT('Ctrl Pts',(-0.833167968837915,3.13981966699007,
7.45358288749364));
#101096=CARTESIAN_POINT('Ctrl Pts',(-1.361330525,3.007773793,7.121044811));
#101097=CARTESIAN_POINT('Ctrl Pts',(-0.971833309999999,3.07352872,7.195505015));
#101098=CARTESIAN_POINT('Ctrl Pts',(-0.576538529,3.138525418,7.22703973500001));
#101099=CARTESIAN_POINT('Ctrl Pts',(-0.572602868521616,3.13917254249503,
7.22735370309967));
#101100=CARTESIAN_POINT('Ctrl Pts',(-0.568667208043231,3.13981966699007,
7.22766767119934));
#101101=CARTESIAN_POINT('',(-0.841285032614871,3.13852541850725,7.45266660087849));
#101102=CARTESIAN_POINT('',(-0.708911788726928,3.13852541943002,7.33985316815712));
#101103=CARTESIAN_POINT('',(-1.40333520077077,3.04797057326662,7.36754032226984));
#101104=CARTESIAN_POINT('Origin',(0.0511750932729073,2.9464821042826,-0.1817606101355));
#101105=CARTESIAN_POINT('Ctrl Pts',(-1.35667769724235,3.00855922358375,
7.12193272858185));
#101106=CARTESIAN_POINT('Ctrl Pts',(-1.36448211669332,3.01545478679876,
7.16280006053993));
#101107=CARTESIAN_POINT('Ctrl Pts',(-1.37227545237948,3.02218156071882,
7.20372368936741));
#101108=CARTESIAN_POINT('Ctrl Pts',(-1.387824204079,3.03530792012134,7.28557967537735));
#101109=CARTESIAN_POINT('Ctrl Pts',(-1.39558848094672,3.04171498175703,
7.32655869520993));
#101110=CARTESIAN_POINT('Ctrl Pts',(-1.4033352045952,3.04797057332674,7.36754031585559));
#101111=CARTESIAN_POINT('Ctrl Pts',(-1.96108872313986,3.13983235804358,
7.23907434966038));
#101112=CARTESIAN_POINT('Ctrl Pts',(-1.95715442456993,3.13917888802179,
7.2401355763302));
#101113=CARTESIAN_POINT('Ctrl Pts',(-1.953220126,3.138525418,7.241196803));
#101114=CARTESIAN_POINT('Ctrl Pts',(-1.559352402,3.073105688,7.347437579));
#101115=CARTESIAN_POINT('Ctrl Pts',(-1.156285027,3.007781414,7.41033096));
#101116=CARTESIAN_POINT('Ctrl Pts',(-2.12419422451127,3.13983235804358,
6.93183676660003));
#101117=CARTESIAN_POINT('Ctrl Pts',(-2.12042675825564,3.13917888802179,
6.93298679330002));
#101118=CARTESIAN_POINT('Ctrl Pts',(-2.116659292,3.138525418,6.93413682));
#101119=CARTESIAN_POINT('Ctrl Pts',(-1.739493367,3.073105688,7.04926748200001));
#101120=CARTESIAN_POINT('Ctrl Pts',(-1.352065021,3.007781414,7.122809851));
#101121=CARTESIAN_POINT('',(-1.95322012318267,3.13852541980573,7.24119677028181));
#101122=CARTESIAN_POINT('Origin',(0.0426114486941837,3.08928602504253,-0.188292761037378));
#101123=CARTESIAN_POINT('',(-2.03493969893267,3.13852541968788,7.08766681439043));
#101124=CARTESIAN_POINT('Origin',(1.51788304147971E-15,3.22948687199989,
-4.08527378592538E-13));
#101125=CARTESIAN_POINT('',(-1.39671107502148,3.22840427021682,7.36879896407947));
#101126=CARTESIAN_POINT('Origin',(0.0135835823359337,3.08929955170748,-0.190873985323708));
#101127=CARTESIAN_POINT('Ctrl Pts',(-1.95322012332207,3.13852541968788,
7.24119679148189));
#101128=CARTESIAN_POINT('Ctrl Pts',(-1.72094870099522,3.176642188,7.30384904600832));
#101129=CARTESIAN_POINT('Ctrl Pts',(-1.48513956599495,3.214285714,7.35148695600817));
#101130=CARTESIAN_POINT('Ctrl Pts',(-1.44097732348694,3.22133557899821,
7.36040856533142));
#101131=CARTESIAN_POINT('Ctrl Pts',(-1.39671108389569,3.22840426981341,
7.36879896225412));
#101132=CARTESIAN_POINT('Ctrl Pts',(-3.183371514,3.007773793,6.790886967));
#101133=CARTESIAN_POINT('Ctrl Pts',(-2.811932824,3.07352872,6.965006689));
#101134=CARTESIAN_POINT('Ctrl Pts',(-2.423719275,3.138525418,7.097575986));
#101135=CARTESIAN_POINT('Ctrl Pts',(-2.4198541171598,3.13917254249503,7.09889588134881));
#101136=CARTESIAN_POINT('Ctrl Pts',(-2.4159889593196,3.13981966699007,7.10021577669762));
#101137=CARTESIAN_POINT('Ctrl Pts',(-2.860317511,3.007773793,6.661912919));
#101138=CARTESIAN_POINT('Ctrl Pts',(-2.495933268,3.07352872,6.818362672));
#101139=CARTESIAN_POINT('Ctrl Pts',(-2.116659292,3.138525418,6.93413682000001));
#101140=CARTESIAN_POINT('Ctrl Pts',(-2.1128831389376,3.13917254249503,6.93528949835702));
#101141=CARTESIAN_POINT('Ctrl Pts',(-2.10910698587521,3.13981966699007,
6.93644217671404));
#101142=CARTESIAN_POINT('',(-2.42371927611826,3.13852541850768,7.09757598357859));
#101143=CARTESIAN_POINT('',(-2.27018929184914,3.1385254194313,7.01585640029839));
#101144=CARTESIAN_POINT('',(-2.95432939001173,3.0479705733085,6.89361573776188));
#101145=CARTESIAN_POINT('Origin',(0.0890517505241159,2.94648211656367,-0.166509866620262));
#101146=CARTESIAN_POINT('Ctrl Pts',(-2.85596434015128,3.00855922361461,
6.66378029826412));
#101147=CARTESIAN_POINT('Ctrl Pts',(-2.87237156518513,3.0154547868692,6.702014455108));
#101148=CARTESIAN_POINT('Ctrl Pts',(-2.8887800676319,3.02218156079834,6.74030597523103));
#101149=CARTESIAN_POINT('Ctrl Pts',(-2.92156191564258,3.0353079202082,6.81690569145188));
#101150=CARTESIAN_POINT('Ctrl Pts',(-2.9379539459452,3.04171498182537,6.85525755432722));
#101151=CARTESIAN_POINT('Ctrl Pts',(-2.95432939247112,3.04797057336922,
6.89361573063811));
#101152=CARTESIAN_POINT('Ctrl Pts',(-3.47142655900055,3.13983235804358,
6.64825270764319));
#101153=CARTESIAN_POINT('Ctrl Pts',(-3.46781237450027,3.13917888802179,
6.6501348813216));
#101154=CARTESIAN_POINT('Ctrl Pts',(-3.46419819,3.138525418,6.652017055));
#101155=CARTESIAN_POINT('Ctrl Pts',(-3.1023775,3.073105688,6.840443899));
#101156=CARTESIAN_POINT('Ctrl Pts',(-2.722253834,3.007781414,6.988514439));
#101157=CARTESIAN_POINT('Ctrl Pts',(-3.56467174548097,3.13983235804358,
6.31313530783206));
#101158=CARTESIAN_POINT('Ctrl Pts',(-3.56123958224049,3.13917888802179,
6.31506834141603));
#101159=CARTESIAN_POINT('Ctrl Pts',(-3.557807419,3.138525418,6.317001375));
#101160=CARTESIAN_POINT('Ctrl Pts',(-3.214209113,3.073105688,6.51051987000001));
#101161=CARTESIAN_POINT('Ctrl Pts',(-2.851648061,3.007781414,6.665628503));
#101162=CARTESIAN_POINT('',(-3.46419818021678,3.13852541980584,6.65201702365357));
#101163=CARTESIAN_POINT('Origin',(0.0820926261211432,3.08928600358673,-0.174730455447152));
#101164=CARTESIAN_POINT('',(-3.51100279528937,3.13852541968789,6.48450921998705));
#101165=CARTESIAN_POINT('Origin',(-3.64725610824124E-13,3.22948687200033,
8.43509290193722E-13));
#101166=CARTESIAN_POINT('',(-2.94813070307675,3.22840427021118,6.89626894456007));
#101167=CARTESIAN_POINT('Origin',(0.0542983013444376,3.08929950335629,-0.183491481227457));
#101168=CARTESIAN_POINT('Ctrl Pts',(-3.46419818490878,3.13852541968789,
6.65201704432619));
#101169=CARTESIAN_POINT('Ctrl Pts',(-3.25082552099696,3.176642188,6.76313601400966));
#101170=CARTESIAN_POINT('Ctrl Pts',(-3.03077021499666,3.214285714,6.86035217000956));
#101171=CARTESIAN_POINT('Ctrl Pts',(-2.98955834350168,3.22133557899461,
6.87855877362988));
#101172=CARTESIAN_POINT('Ctrl Pts',(-2.94813071139113,3.22840426981375,
6.89626894081897));
#101173=CARTESIAN_POINT('Ctrl Pts',(-4.568786018,3.007773793,5.947789028));
#101174=CARTESIAN_POINT('Ctrl Pts',(-4.243461951,3.07352872,6.197686266));
#101175=CARTESIAN_POINT('Ctrl Pts',(-3.892823099,3.138525418,6.41061060400001));
#101176=CARTESIAN_POINT('Ctrl Pts',(-3.88933204488461,3.13917254249503,
6.41273053561112));
#101177=CARTESIAN_POINT('Ctrl Pts',(-3.88584099076922,3.13981966699007,
6.41485046722225));
#101178=CARTESIAN_POINT('Ctrl Pts',(-4.22555923,3.007773793,5.891277382));
#101179=CARTESIAN_POINT('Ctrl Pts',(-3.90332616,3.07352872,6.122401268));
#101180=CARTESIAN_POINT('Ctrl Pts',(-3.557807419,3.138525418,6.317001375));
#101181=CARTESIAN_POINT('Ctrl Pts',(-3.55436734207803,3.13917254249503,
6.31893886567032));
#101182=CARTESIAN_POINT('Ctrl Pts',(-3.55092726515605,3.13981966699007,
6.32087635634062));
#101183=CARTESIAN_POINT('',(-3.89282309958503,3.13852541850725,6.41061060139456));
#101184=CARTESIAN_POINT('',(-3.72531526656647,3.13852541943003,6.36380598507066));
#101185=CARTESIAN_POINT('',(-4.36718242045613,3.0479705733016,6.09735334318613));
#101186=CARTESIAN_POINT('Origin',(0.122764508923577,2.94648211407493,-0.143473532378355));
#101187=CARTESIAN_POINT('Ctrl Pts',(-4.22170926527457,3.00855922354818,
5.89403690575471));
#101188=CARTESIAN_POINT('Ctrl Pts',(-4.24595211177457,3.01545478679473,
5.92785010094362));
#101189=CARTESIAN_POINT('Ctrl Pts',(-4.27020853745607,3.02218156074601,
5.96171904382587));
#101190=CARTESIAN_POINT('Ctrl Pts',(-4.3186906387285,3.03530792016112,6.02948077315774));
#101191=CARTESIAN_POINT('Ctrl Pts',(-4.34294394943307,3.04171498180012,
6.06341218901963));
#101192=CARTESIAN_POINT('Ctrl Pts',(-4.36718242130857,3.04797057336225,
6.09735333570621));
#101193=CARTESIAN_POINT('Ctrl Pts',(-4.81944434632715,3.13983235804358,
5.74656615832854));
#101194=CARTESIAN_POINT('Ctrl Pts',(-4.81631927116357,3.13917888802179,
5.74918127066428));
#101195=CARTESIAN_POINT('Ctrl Pts',(-4.813194196,3.138525418,5.751796383));
#101196=CARTESIAN_POINT('Ctrl Pts',(-4.500338875,3.073105688,6.01359866500001));
#101197=CARTESIAN_POINT('Ctrl Pts',(-4.160933077,3.007781414,6.23992275));
#101198=CARTESIAN_POINT('Ctrl Pts',(-4.83846917719169,3.13983235804358,
5.39923865803316));
#101199=CARTESIAN_POINT('Ctrl Pts',(-4.83553280109584,3.13917888802179,
5.40186431201658));
#101200=CARTESIAN_POINT('Ctrl Pts',(-4.83259642500001,3.138525418,5.404489966));
#101201=CARTESIAN_POINT('Ctrl Pts',(-4.538632012,3.073105688,5.667347586));
#101202=CARTESIAN_POINT('Ctrl Pts',(-4.217891208,3.007781414,5.896769773));
#101203=CARTESIAN_POINT('',(-4.81319417970427,3.13852541980591,5.7517963544844));
#101204=CARTESIAN_POINT('Origin',(0.117735124629917,3.08928604967561,-0.152997718666201));
#101205=CARTESIAN_POINT('',(-4.82289530257677,3.13852541968789,5.57814318135047));
#101206=CARTESIAN_POINT('Origin',(5.61833565781988E-13,3.22948687200044,
-9.40653804848424E-13));
#101207=CARTESIAN_POINT('',(-4.36169901671411,3.22840427023201,6.10127705377287));
#101208=CARTESIAN_POINT('Origin',(0.0924741257385808,3.08929953180407,-0.167529084643822));
#101209=CARTESIAN_POINT('Ctrl Pts',(-4.81319418873319,3.13852541968789,
5.7517963736712));
#101210=CARTESIAN_POINT('Ctrl Pts',(-4.62869735299911,3.176642188,5.9061862590101));
#101211=CARTESIAN_POINT('Ctrl Pts',(-4.43468541799878,3.214285714,6.04843494201006));
#101212=CARTESIAN_POINT('Ctrl Pts',(-4.39835093887207,3.22133557899724,
6.0750752195256));
#101213=CARTESIAN_POINT('Ctrl Pts',(-4.36169902396167,3.22840426981355,
6.10127704866005));
#101214=CARTESIAN_POINT('Ctrl Pts',(-5.740569165,3.007773793,4.826579084));
#101215=CARTESIAN_POINT('Ctrl Pts',(-5.476571513,3.07352872,5.140568922));
#101216=CARTESIAN_POINT('Ctrl Pts',(-5.179902842,3.138525418,5.423892195));
#101217=CARTESIAN_POINT('Ctrl Pts',(-5.17694912942966,3.13917254249503,
5.42671303722142));
#101218=CARTESIAN_POINT('Ctrl Pts',(-5.17399541685932,3.13981966699007,
5.42953387944285));
#101219=CARTESIAN_POINT('Ctrl Pts',(-5.393218496,3.007773793,4.845172263));
#101220=CARTESIAN_POINT('Ctrl Pts',(-5.12820386,3.07352872,5.140163186));
#101221=CARTESIAN_POINT('Ctrl Pts',(-4.832596425,3.138525418,5.404489966));
#101222=CARTESIAN_POINT('Ctrl Pts',(-4.82965327837888,3.13917254249503,
5.40712167406049));
#101223=CARTESIAN_POINT('Ctrl Pts',(-4.82671013175777,3.13981966699007,
5.40975338212096));
#101224=CARTESIAN_POINT('',(-5.17990284201368,3.13852541850726,5.42389219232864));
#101225=CARTESIAN_POINT('',(-5.00624963993739,3.13852541943003,5.41419107454764));
#101226=CARTESIAN_POINT('',(-5.57583085480616,3.04797057328096,5.01598548285496));
#101227=CARTESIAN_POINT('Origin',(0.150736866359442,2.94648216097497,-0.113728428632556));
#101228=CARTESIAN_POINT('Ctrl Pts',(-5.39005175674981,3.00855922359023,
4.84869489944727));
#101229=CARTESIAN_POINT('Ctrl Pts',(-5.42099665668092,3.01545478682458,
4.87650606540874));
#101230=CARTESIAN_POINT('Ctrl Pts',(-5.45196680211484,3.02218156072737,
4.90436875647179));
#101231=CARTESIAN_POINT('Ctrl Pts',(-5.51388218774758,3.03530792014147,
4.96012403551547));
#101232=CARTESIAN_POINT('Ctrl Pts',(-5.54486272091281,3.04171498177744,
4.98804840882984));
#101233=CARTESIAN_POINT('Ctrl Pts',(-5.57583085399527,3.04797057334128,
5.01598547540733));
#101234=CARTESIAN_POINT('Ctrl Pts',(-5.9421102725929,3.13983235804358,4.57617656251187));
#101235=CARTESIAN_POINT('Ctrl Pts',(-5.93962043179645,3.13917888802179,
4.57940233375594));
#101236=CARTESIAN_POINT('Ctrl Pts',(-5.93713059100001,3.138525418,4.582628105));
#101237=CARTESIAN_POINT('Ctrl Pts',(-5.687869405,3.073105688,4.905564241));
#101238=CARTESIAN_POINT('Ctrl Pts',(-5.405051715,3.007781414,5.199559208));
#101239=CARTESIAN_POINT('Ctrl Pts',(-5.88602516750172,3.13983235804358,
4.23287960957504));
#101240=CARTESIAN_POINT('Ctrl Pts',(-5.88372188025086,3.13917888802179,
4.23607511128751));
#101241=CARTESIAN_POINT('Ctrl Pts',(-5.881418593,3.138525418,4.239270613));
#101242=CARTESIAN_POINT('Ctrl Pts',(-5.650833524,3.073105688,4.559176427));
#101243=CARTESIAN_POINT('Ctrl Pts',(-5.386910449,3.007781414,4.852184643));
#101244=CARTESIAN_POINT('',(-5.93713056884798,3.13852541976328,4.5826280811928));
#101245=CARTESIAN_POINT('Origin',(0.147872621769565,3.08928602335869,-0.124111231483713));
#101246=CARTESIAN_POINT('',(-5.90927458573466,3.13852541968789,4.41094936739357));
#101247=CARTESIAN_POINT('Origin',(-6.52689707836274E-13,3.22948687199956,
5.54677831443584E-13));
#101248=CARTESIAN_POINT('',(-5.57131913161687,3.22840427018799,5.02099622948482));
#101249=CARTESIAN_POINT('Origin',(0.126325665212076,3.08929953797125,-0.143732892740396));
#101250=CARTESIAN_POINT('Ctrl Pts',(-5.93713058189749,3.13852541968789,
4.58262809745036));
#101251=CARTESIAN_POINT('Ctrl Pts',(-5.79013644100131,3.176642188,4.77306979901004));
#101252=CARTESIAN_POINT('Ctrl Pts',(-5.63123965900098,3.214285714,4.95369961801008));
#101253=CARTESIAN_POINT('Ctrl Pts',(-5.60148153190861,3.2213355789788,4.98752789928355));
#101254=CARTESIAN_POINT('Ctrl Pts',(-5.57131913758477,3.22840426981253,
5.02099622261143));
#101255=CARTESIAN_POINT('Ctrl Pts',(-6.643929679,3.007773793,3.479683667));
#101256=CARTESIAN_POINT('Ctrl Pts',(-6.453602679,3.07352872,3.843084288));
#101257=CARTESIAN_POINT('Ctrl Pts',(-6.224776085,3.138525418,4.183558616));
#101258=CARTESIAN_POINT('Ctrl Pts',(-6.22249782627842,3.13917254249503,
4.18694846939808));
#101259=CARTESIAN_POINT('Ctrl Pts',(-6.22021956755684,3.13981966699007,
4.19033832279615));
#101260=CARTESIAN_POINT('Ctrl Pts',(-6.308696859,3.007773793,3.572512274));
#101261=CARTESIAN_POINT('Ctrl Pts',(-6.113292446,3.07352872,3.917576786));
#101262=CARTESIAN_POINT('Ctrl Pts',(-5.881418593,3.138525418,4.239270613));
#101263=CARTESIAN_POINT('Ctrl Pts',(-5.87910999495346,3.13917254249503,
4.24247348271121));
#101264=CARTESIAN_POINT('Ctrl Pts',(-5.87680139690693,3.13981966699007,
4.24567635242242));
#101265=CARTESIAN_POINT('',(-6.22477608441923,3.13852541850725,4.18355861340267));
#101266=CARTESIAN_POINT('',(-6.05309734400731,3.13852541943003,4.21141460730296));
#101267=CARTESIAN_POINT('',(-6.52375963486162,3.04797057325993,3.70007571645805));
#101268=CARTESIAN_POINT('Origin',(0.17166106789941,2.9464821192333,-0.0786655901702615));
#101269=CARTESIAN_POINT('Ctrl Pts',(-6.30636141922387,3.00855922362562,
3.57663330860406));
#101270=CARTESIAN_POINT('Ctrl Pts',(-6.34256142316941,3.01545478687365,
3.59714202626727));
#101271=CARTESIAN_POINT('Ctrl Pts',(-6.37879715852299,3.02218156074315,
3.61769563720488));
#101272=CARTESIAN_POINT('Ctrl Pts',(-6.45125073357316,3.03530792015397,
3.65883741109778));
#101273=CARTESIAN_POINT('Ctrl Pts',(-6.48750987375242,3.04171498177261,
3.67944902917069));
#101274=CARTESIAN_POINT('Ctrl Pts',(-6.52375963243751,3.04797057331986,
3.70007570940484));
#101275=CARTESIAN_POINT('Ctrl Pts',(-6.78692972648235,3.13983235804358,
3.19181003665553));
#101276=CARTESIAN_POINT('Ctrl Pts',(-6.78519154224117,3.13917888802179,
3.19549563332777));
#101277=CARTESIAN_POINT('Ctrl Pts',(-6.783453358,3.138525418,3.19918123));
#101278=CARTESIAN_POINT('Ctrl Pts',(-6.609441483,3.073105688,3.568151085));
#101279=CARTESIAN_POINT('Ctrl Pts',(-6.396436141,3.007781414,3.916070057));
#101280=CARTESIAN_POINT('Ctrl Pts',(-6.65835716353885,3.13983235804358,
2.86859581532773));
#101281=CARTESIAN_POINT('Ctrl Pts',(-6.65679466426943,3.13917888802179,
2.87221174666387));
#101282=CARTESIAN_POINT('Ctrl Pts',(-6.655232165,3.138525418,2.875827678));
#101283=CARTESIAN_POINT('Ctrl Pts',(-6.49880834,3.073105688,3.237823246));
#101284=CARTESIAN_POINT('Ctrl Pts',(-6.304043745,3.007781414,3.580716752));
#101285=CARTESIAN_POINT('',(-6.78345333124599,3.13852541976318,3.19918121151157));
#101286=CARTESIAN_POINT('Origin',(0.171095824460236,3.08928604518906,-0.0894214078364035));
#101287=CARTESIAN_POINT('',(-6.71934275718553,3.13852541968788,3.03750446354416));
#101288=CARTESIAN_POINT('Origin',(-4.65773253299773E-13,3.22948687199922,
2.87530416143156E-13));
#101289=CARTESIAN_POINT('',(-6.52043055618455,3.22840427020818,3.70593920108148));
#101290=CARTESIAN_POINT('Origin',(0.154270784387071,3.08929955107671,-0.113216334442104));
#101291=CARTESIAN_POINT('Ctrl Pts',(-6.78345334748772,3.13852541968788,
3.19918122458446));
#101292=CARTESIAN_POINT('Ctrl Pts',(-6.68083518500339,3.176642188,3.41676990000944));
#101293=CARTESIAN_POINT('Ctrl Pts',(-6.56448339300309,3.214285714,3.62733480500954));
#101294=CARTESIAN_POINT('Ctrl Pts',(-6.54269307504985,3.22133557898338,
3.66676931770777));
#101295=CARTESIAN_POINT('Ctrl Pts',(-6.52043056059152,3.22840426981355,
3.70593919332983));
#101296=CARTESIAN_POINT('Ctrl Pts',(-7.236627425,3.007773793,1.970082109));
#101297=CARTESIAN_POINT('Ctrl Pts',(-7.128870556,3.07352872,2.365901304));
#101298=CARTESIAN_POINT('Ctrl Pts',(-6.978585717,3.138525418,2.747606485));
#101299=CARTESIAN_POINT('Ctrl Pts',(-6.97708944098073,3.13917254249503,
2.75140684378909));
#101300=CARTESIAN_POINT('Ctrl Pts',(-6.97559316496146,3.13981966699007,
2.75520720257818));
#101301=CARTESIAN_POINT('Ctrl Pts',(-6.929187568,3.007773793,2.132805581));
#101302=CARTESIAN_POINT('Ctrl Pts',(-6.812530272,3.07352872,2.511808849));
#101303=CARTESIAN_POINT('Ctrl Pts',(-6.655232165,3.138525418,2.875827678));
#101304=CARTESIAN_POINT('Ctrl Pts',(-6.65366606301029,3.13917254249503,
2.87945194674207));
#101305=CARTESIAN_POINT('Ctrl Pts',(-6.65209996102059,3.13981966699007,
2.88307621548415));
#101306=CARTESIAN_POINT('',(-6.97858571586415,3.13852541850724,2.74760648259996));
#101307=CARTESIAN_POINT('',(-6.81690894434307,3.13852541943002,2.81171707339485));
#101308=CARTESIAN_POINT('',(-7.16664466580176,3.04797057323609,2.21115452164468));
#101309=CARTESIAN_POINT('Origin',(0.18455854297556,2.9464821110578,-0.0399243888134687));
#101310=CARTESIAN_POINT('Ctrl Pts',(-6.92779263031792,3.00855922359982,
2.13733231839922));
#101311=CARTESIAN_POINT('Ctrl Pts',(-6.96755506624603,3.01545478682721,
2.1495796229758));
#101312=CARTESIAN_POINT('Ctrl Pts',(-7.00736204937631,3.02218156074204,
2.16186309011969));
#101313=CARTESIAN_POINT('Ctrl Pts',(-7.08696596538827,3.03530792012699,
2.18646761537362));
#101314=CARTESIAN_POINT('Ctrl Pts',(-7.12680827576463,3.04171498174729,
2.19880270198573));
#101315=CARTESIAN_POINT('Ctrl Pts',(-7.16664466189622,3.04797057329574,
2.21115451533576));
#101316=CARTESIAN_POINT('Ctrl Pts',(-7.31439988922279,3.13983235804358,
1.65819802060071));
#101317=CARTESIAN_POINT('Ctrl Pts',(-7.31349463711139,3.13917888802179,
1.66217110830035));
#101318=CARTESIAN_POINT('Ctrl Pts',(-7.312589385,3.138525418,1.666144196));
#101319=CARTESIAN_POINT('Ctrl Pts',(-7.221963424,3.073105688,2.06389515));
#101320=CARTESIAN_POINT('Ctrl Pts',(-7.088730323,3.007781414,2.449469822));
#101321=CARTESIAN_POINT('Ctrl Pts',(-7.11935177812158,3.13983235804358,
1.37017966895271));
#101322=CARTESIAN_POINT('Ctrl Pts',(-7.11860312756079,3.13917888802179,
1.37404695297636));
#101323=CARTESIAN_POINT('Ctrl Pts',(-7.117854477,3.138525418,1.377914237));
#101324=CARTESIAN_POINT('Ctrl Pts',(-7.0429061,3.073105688,1.765073048));
#101325=CARTESIAN_POINT('Ctrl Pts',(-6.926406962,3.007781414,2.141818525));
#101326=CARTESIAN_POINT('',(-7.31258935489774,3.13852541976228,1.6661441837052));
#101327=CARTESIAN_POINT('Origin',(0.186318504438061,3.08928605858041,-0.0505501868150156));
#101328=CARTESIAN_POINT('',(-7.21522192883811,3.13852541968788,1.5220292267485));
#101329=CARTESIAN_POINT('Origin',(4.38017677684144E-14,3.22948687199956,
-7.3075226425523E-14));
#101330=CARTESIAN_POINT('',(-7.16465389455188,3.2284042702292,2.21759657501191));
#101331=CARTESIAN_POINT('Origin',(0.175002196689876,3.08929950069257,-0.0774057478759155));
#101332=CARTESIAN_POINT('Ctrl Pts',(-7.31258937356945,3.13852541968788,
1.6661441929711));
#101333=CARTESIAN_POINT('Ctrl Pts',(-7.25914550000535,3.176642188,1.90070563800849));
#101334=CARTESIAN_POINT('Ctrl Pts',(-7.19077917900507,3.214285714,2.13135984800866));
#101335=CARTESIAN_POINT('Ctrl Pts',(-7.17797556110879,3.22133557899793,
2.17455667813255));
#101336=CARTESIAN_POINT('Ctrl Pts',(-7.16465389719845,3.22840426981355,
2.21759656650944));
#101337=CARTESIAN_POINT('Ctrl Pts',(-7.490948515,3.007773793,0.368361701));
#101338=CARTESIAN_POINT('Ctrl Pts',(-7.470800368,3.07352872,0.778091405));
#101339=CARTESIAN_POINT('Ctrl Pts',(-7.406084436,3.138525418,1.183179329));
#101340=CARTESIAN_POINT('Ctrl Pts',(-7.4054401068863,3.13917254249503,1.18721249262722));
#101341=CARTESIAN_POINT('Ctrl Pts',(-7.40479577777259,3.13981966699007,
1.19124565625443));
#101342=CARTESIAN_POINT('Ctrl Pts',(-7.225677168,3.007773793,0.59337127));
#101343=CARTESIAN_POINT('Ctrl Pts',(-7.193221754,3.07352872,0.988591523));
#101344=CARTESIAN_POINT('Ctrl Pts',(-7.117854477,3.138525418,1.377914237));
#101345=CARTESIAN_POINT('Ctrl Pts',(-7.117104100249,3.13917254249503,1.38179043798336));
#101346=CARTESIAN_POINT('Ctrl Pts',(-7.11635372349801,3.13981966699007,
1.38566663896671));
#101347=CARTESIAN_POINT('',(-7.4060844343901,3.13852541850726,1.18317932687253));
#101348=CARTESIAN_POINT('',(-7.26196945802254,3.13852541943002,1.28054677436567));
#101349=CARTESIAN_POINT('',(-7.47442535668232,3.0479705732519,0.618842199152955));
#101350=CARTESIAN_POINT('Origin',(0.188826312889078,2.94648211665553,0.000683638074364806));
#101351=CARTESIAN_POINT('Ctrl Pts',(-7.22528795810141,3.00855922362978,
0.598092045178342));
#101352=CARTESIAN_POINT('Ctrl Pts',(-7.26675357867071,3.01545478683311,
0.601505266195231));
#101353=CARTESIAN_POINT('Ctrl Pts',(-7.30827047911143,3.02218156077703,
0.604944228025243));
#101354=CARTESIAN_POINT('Ctrl Pts',(-7.39130254515032,3.03530792014544,
0.611861024277268));
#101355=CARTESIAN_POINT('Ctrl Pts',(-7.43286504331963,3.04171498176303,
0.615342804424618));
#101356=CARTESIAN_POINT('Ctrl Pts',(-7.47442535151781,3.0479705733117,0.618842193790382));
#101357=CARTESIAN_POINT('Ctrl Pts',(-7.49985684282223,3.13983235804358,
0.0470505078652194));
#101358=CARTESIAN_POINT('Ctrl Pts',(-7.49982685141112,3.13917888802179,
0.0511253094326098));
#101359=CARTESIAN_POINT('Ctrl Pts',(-7.49979686,3.138525418,0.055200111));
#101360=CARTESIAN_POINT('Ctrl Pts',(-7.496794381,3.073105688,0.463133772));
#101361=CARTESIAN_POINT('Ctrl Pts',(-7.449563353,3.007781414,0.868335101));
#101362=CARTESIAN_POINT('Ctrl Pts',(-7.24745341654421,3.13983235804358,
-0.192304556630875));
#101363=CARTESIAN_POINT('Ctrl Pts',(-7.2475536207721,3.13917888802179,-0.188366749815437));
#101364=CARTESIAN_POINT('Ctrl Pts',(-7.247653825,3.138525418,-0.184428943));
#101365=CARTESIAN_POINT('Ctrl Pts',(-7.25768540000001,3.073105688,0.209789996));
#101366=CARTESIAN_POINT('Ctrl Pts',(-7.224899088,3.007781414,0.602771245));
#101367=CARTESIAN_POINT('',(-7.49979682771917,3.13852541980542,0.0552001049644113));
#101368=CARTESIAN_POINT('Origin',(0.192829366040071,3.08928604866555,-0.00931538846567845));
#101369=CARTESIAN_POINT('',(-7.37372534259178,3.13852541968788,-0.0646144055263606));
#101370=CARTESIAN_POINT('Origin',(-4.03323208164608E-14,3.22948687200056,
9.69378386155711E-14));
#101371=CARTESIAN_POINT('',(-7.47386597982596,3.22840427019247,0.625561598002911));
#101372=CARTESIAN_POINT('Origin',(0.187550563655007,3.08929957882852,-0.0379757253992395));
#101373=CARTESIAN_POINT('Ctrl Pts',(-7.49979684818555,3.13852541968788,
0.0552001104991303));
#101374=CARTESIAN_POINT('Ctrl Pts',(-7.49802624000704,3.176642188,0.295766492007143));
#101375=CARTESIAN_POINT('Ctrl Pts',(-7.48084212200681,3.214285714,0.535724874007362));
#101376=CARTESIAN_POINT('Ctrl Pts',(-7.47762388722127,3.22133557897867,
0.580664185511631));
#101377=CARTESIAN_POINT('Ctrl Pts',(-7.47386598048774,3.22840426981254,
0.625561589035954));
#101378=CARTESIAN_POINT('Ctrl Pts',(-7.395001179,3.007773793,-1.250582891));
#101379=CARTESIAN_POINT('Ctrl Pts',(-7.463403859,3.07352872,-0.846101184));
#101380=CARTESIAN_POINT('Ctrl Pts',(-7.487282879,3.138525418,-0.436571978));
#101381=CARTESIAN_POINT('Ctrl Pts',(-7.48752062490456,3.13917254249503,
-0.432494595782302));
#101382=CARTESIAN_POINT('Ctrl Pts',(-7.48775837080912,3.13981966699007,
-0.428417213564603));
#101383=CARTESIAN_POINT('Ctrl Pts',(-7.184302134,3.007773793,-0.973808422));
#101384=CARTESIAN_POINT('Ctrl Pts',(-7.237566182,3.07352872,-0.580851245));
#101385=CARTESIAN_POINT('Ctrl Pts',(-7.247653825,3.138525418,-0.184428943));
#101386=CARTESIAN_POINT('Ctrl Pts',(-7.24775426026954,3.13917254249503,
-0.180482056621221));
#101387=CARTESIAN_POINT('Ctrl Pts',(-7.24785469553907,3.13981966699007,
-0.176535170242441));
#101388=CARTESIAN_POINT('',(-7.48728287696554,3.13852541850724,-0.436571979715327));
#101389=CARTESIAN_POINT('',(-7.36746835163082,3.13852541943002,-0.310500469259762));
#101390=CARTESIAN_POINT('',(-7.43271022601071,3.0479705733026,-1.0024064970043));
#101391=CARTESIAN_POINT('Origin',(0.184264765153066,2.94648210271064,0.0412597353598802));
#101392=CARTESIAN_POINT('Ctrl Pts',(-7.18493685111983,3.00855922368414,
-0.969114347424904));
#101393=CARTESIAN_POINT('Ctrl Pts',(-7.22616677032159,3.01545478688936,
-0.974694808421183));
#101394=CARTESIAN_POINT('Ctrl Pts',(-7.26745230375002,3.02218156080068,
-0.980261154022604));
#101395=CARTESIAN_POINT('Ctrl Pts',(-7.35003003322002,3.03530792018507,
-0.991355508549004));
#101396=CARTESIAN_POINT('Ctrl Pts',(-7.39136930315834,3.04171498180619,
-0.996889839063651));
#101397=CARTESIAN_POINT('Ctrl Pts',(-7.43271021980434,3.04797057336331,
-1.00240650126442));
#101398=CARTESIAN_POINT('Ctrl Pts',(-7.33462882668321,3.13983235804358,
-1.56629703347738));
#101399=CARTESIAN_POINT('Ctrl Pts',(-7.33547549834161,3.13917888802179,
-1.56231105123869));
#101400=CARTESIAN_POINT('Ctrl Pts',(-7.33632217,3.138525418,-1.558325069));
#101401=CARTESIAN_POINT('Ctrl Pts',(-7.421083566,3.073105688,-1.159283226));
#101402=CARTESIAN_POINT('Ctrl Pts',(-7.462063081,3.007781414,-0.753402005));
#101403=CARTESIAN_POINT('Ctrl Pts',(-7.03667218785752,3.13983235804358,
-1.74579683426311));
#101404=CARTESIAN_POINT('Ctrl Pts',(-7.03761656142876,3.13917888802179,
-1.74197263213155));
#101405=CARTESIAN_POINT('Ctrl Pts',(-7.038560935,3.138525418,-1.73814843));
#101406=CARTESIAN_POINT('Ctrl Pts',(-7.133103396,3.073105688,-1.355302603));
#101407=CARTESIAN_POINT('Ctrl Pts',(-7.185562962,3.007781414,-0.964460949));
#101408=CARTESIAN_POINT('',(-7.33632213717586,3.13852541980608,-1.55832506796128));
#101409=CARTESIAN_POINT('Origin',(0.190323629021206,3.08928601948903,0.0323550041314696));
#101410=CARTESIAN_POINT('',(-7.18744155484115,3.13852541968788,-1.64823673929096));
#101411=CARTESIAN_POINT('Origin',(-6.5746019739521E-13,3.22948687199956,
-2.0491421059976E-14));
#101412=CARTESIAN_POINT('',(-7.43360839863754,3.2284042701966,-0.995723944406123));
#101413=CARTESIAN_POINT('Origin',(0.191329551313522,3.08929953639508,0.00322996651958354));
#101414=CARTESIAN_POINT('Ctrl Pts',(-7.33632215835401,3.13852541968788,
-1.55832506694945));
#101415=CARTESIAN_POINT('Ctrl Pts',(-7.38630760700842,3.176642188,-1.32300236499454));
#101416=CARTESIAN_POINT('Ctrl Pts',(-7.42110920300824,3.214285714,-1.08495999999427));
#101417=CARTESIAN_POINT('Ctrl Pts',(-7.42762683215621,3.22133557897501,
-1.04037951929082));
#101418=CARTESIAN_POINT('Ctrl Pts',(-7.43360839747068,3.22840426981253,
-0.995723953228806));
#101419=CARTESIAN_POINT('Ctrl Pts',(-6.953271806,3.007773793,-2.811051617));
#101420=CARTESIAN_POINT('Ctrl Pts',(-7.10702688,3.07352872,-2.430731022));
#101421=CARTESIAN_POINT('Ctrl Pts',(-7.218384296,3.138525418,-2.035909664));
#101422=CARTESIAN_POINT('Ctrl Pts',(-7.2194930001929,3.13917254249503,-2.03197871704752));
#101423=CARTESIAN_POINT('Ctrl Pts',(-7.2206017043858,3.13981966699007,-2.02804777009504));
#101424=CARTESIAN_POINT('Ctrl Pts',(-6.806997118,3.007773793,-2.495453915));
#101425=CARTESIAN_POINT('Ctrl Pts',(-6.943490059,3.07352872,-2.123134053));
#101426=CARTESIAN_POINT('Ctrl Pts',(-7.038560935,3.138525418,-1.73814843));
#101427=CARTESIAN_POINT('Ctrl Pts',(-7.03950748604824,3.13917254249503,
-1.73431541025369));
#101428=CARTESIAN_POINT('Ctrl Pts',(-7.04045403709647,3.13981966699007,
-1.73048239050737));
#101429=CARTESIAN_POINT('',(-7.21838429364368,3.13852541850724,-2.03590966522802));
#101430=CARTESIAN_POINT('',(-7.12847261325636,3.13852541943002,-1.8870290554756));
#101431=CARTESIAN_POINT('',(-7.04344982493227,3.04797057330757,-2.57678377911017));
#101432=CARTESIAN_POINT('Origin',(0.17108717423595,2.94648207320262,0.0799066117954211));
#101433=CARTESIAN_POINT('Ctrl Pts',(-6.8086260823428,3.00855922361795,-2.49100602981249));
#101434=CARTESIAN_POINT('Ctrl Pts',(-6.84769243471522,3.01545478683609,
-2.5053192366488));
#101435=CARTESIAN_POINT('Ctrl Pts',(-6.886816135416,3.02218156075082,-2.51963061349986));
#101436=CARTESIAN_POINT('Ctrl Pts',(-6.96507828505715,3.03530792016389,
-2.54821735912404));
#101437=CARTESIAN_POINT('Ctrl Pts',(-7.00426134831103,3.04171498179865,
-2.56250902116351));
#101438=CARTESIAN_POINT('Ctrl Pts',(-7.04344981795141,3.04797057336821,
-2.57678378194846));
#101439=CARTESIAN_POINT('Ctrl Pts',(-6.82644171740222,3.13983235804358,
-3.10640626662274));
#101440=CARTESIAN_POINT('Ctrl Pts',(-6.82812546270111,3.13917888802179,
-3.10269548381137));
#101441=CARTESIAN_POINT('Ctrl Pts',(-6.829809208,3.138525418,-3.098984701));
#101442=CARTESIAN_POINT('Ctrl Pts',(-6.99837113000001,3.073105688,-2.727493429));
#101443=CARTESIAN_POINT('Ctrl Pts',(-7.125645032,3.007781414,-2.33991087));
#101444=CARTESIAN_POINT('Ctrl Pts',(-6.49686398890001,3.13983235804358,
-3.21765759201994));
#101445=CARTESIAN_POINT('Ctrl Pts',(-6.49860837395001,3.13917888802179,
-3.21412581000997));
#101446=CARTESIAN_POINT('Ctrl Pts',(-6.50035275900001,3.138525418,-3.210594028));
#101447=CARTESIAN_POINT('Ctrl Pts',(-6.674985405,3.073105688,-2.857022758));
#101448=CARTESIAN_POINT('Ctrl Pts',(-6.81023789800001,3.007781414,-2.486596021));
#101449=CARTESIAN_POINT('',(-6.82980917617189,3.13852541980549,-3.09898469292473));
#101450=CARTESIAN_POINT('Origin',(0.178918748265815,3.08928601856382,0.0725125769354081));
#101451=CARTESIAN_POINT('',(-6.66508098798106,3.13852541968788,-3.15478935503292));
#101452=CARTESIAN_POINT('Origin',(-6.49653941753314E-13,3.22948687199978,
-2.65846372693446E-13));
#101453=CARTESIAN_POINT('',(-7.04576355038251,3.22840427021457,-2.5704505416214));
#101454=CARTESIAN_POINT('Origin',(0.186162053929123,3.08929956872846,0.0442846701300559));
#101455=CARTESIAN_POINT('Ctrl Pts',(-6.82980919706723,3.13852541968788,
-3.09898469649379));
#101456=CARTESIAN_POINT('Ctrl Pts',(-6.92921343900949,3.176642188,-2.87990910299644));
#101457=CARTESIAN_POINT('Ctrl Pts',(-7.01437346500937,3.214285714,-2.65491334999614));
#101458=CARTESIAN_POINT('Ctrl Pts',(-7.03032220117711,3.2213355789857,-2.61277623396586));
#101459=CARTESIAN_POINT('Ctrl Pts',(-7.04576354739409,3.22840426981256,
-2.57045054996743));
#101460=CARTESIAN_POINT('Ctrl Pts',(-6.18641517199999,3.007773793,-4.240078693));
#101461=CARTESIAN_POINT('Ctrl Pts',(-6.418333224,3.07352872,-3.901702578));
#101462=CARTESIAN_POINT('Ctrl Pts',(-6.611962085,3.138525418,-3.540050477));
#101463=CARTESIAN_POINT('Ctrl Pts',(-6.61388990568557,3.13917254249503,
-3.53644977203438));
#101464=CARTESIAN_POINT('Ctrl Pts',(-6.61581772637116,3.13981966699007,
-3.53284906706876));
#101465=CARTESIAN_POINT('Ctrl Pts',(-6.111404481,3.007773793,-3.900414756));
#101466=CARTESIAN_POINT('Ctrl Pts',(-6.324744057,3.07352872,-3.566141474));
#101467=CARTESIAN_POINT('Ctrl Pts',(-6.50035275900001,3.138525418,-3.210594028));
#101468=CARTESIAN_POINT('Ctrl Pts',(-6.50210116616686,3.13917254249503,
-3.20705410261097));
#101469=CARTESIAN_POINT('Ctrl Pts',(-6.50384957333372,3.13981966699007,
-3.20351417722194));
#101470=CARTESIAN_POINT('',(-6.61196208242836,3.13852541850727,-3.54005047773679));
#101471=CARTESIAN_POINT('',(-6.55615741798682,3.13852541943002,-3.37532226029513));
#101472=CARTESIAN_POINT('',(-6.32484553890956,3.04797057324976,-4.030673515416));
#101473=CARTESIAN_POINT('Origin',(0.149909447659728,2.94648211908025,0.114816963127455));
#101474=CARTESIAN_POINT('Ctrl Pts',(-6.11395152485902,3.00855922359023,
-3.89642103948571));
#101475=CARTESIAN_POINT('Ctrl Pts',(-6.14902761123259,3.01545478679443,
-3.91879772231694));
#101476=CARTESIAN_POINT('Ctrl Pts',(-6.18416009886821,3.02218156074056,
-3.94118494628396));
#101477=CARTESIAN_POINT('Ctrl Pts',(-6.2544472177817,3.0353079201198,-3.98592739811759));
#101478=CARTESIAN_POINT('Ctrl Pts',(-6.28964191806543,3.04171498174985,
-4.00830812928556));
#101479=CARTESIAN_POINT('Ctrl Pts',(-6.32484553155734,3.0479705733095,-4.03067351655581));
#101480=CARTESIAN_POINT('Ctrl Pts',(-5.9990577812363,3.13983235804358,-4.50126339560797));
#101481=CARTESIAN_POINT('Ctrl Pts',(-6.00149987011815,3.13917888802179,
-4.49800132430398));
#101482=CARTESIAN_POINT('Ctrl Pts',(-6.003941959,3.138525418,-4.494739253));
#101483=CARTESIAN_POINT('Ctrl Pts',(-6.248422639,3.073105688,-4.168169071));
#101484=CARTESIAN_POINT('Ctrl Pts',(-6.456039741,3.007781414,-3.817008103));
#101485=CARTESIAN_POINT('Ctrl Pts',(-5.65326964992618,3.13983235804358,
-4.53906425736617));
#101486=CARTESIAN_POINT('Ctrl Pts',(-5.6557324809631,3.13917888802179,-4.53599003768308));
#101487=CARTESIAN_POINT('Ctrl Pts',(-5.658195312,3.138525418,-4.532915818));
#101488=CARTESIAN_POINT('Ctrl Pts',(-5.904752516,3.073105688,-4.225151705));
#101489=CARTESIAN_POINT('Ctrl Pts',(-6.11647367900001,3.007781414,-3.892460627));
#101490=CARTESIAN_POINT('',(-6.00394192964676,3.13852541980585,-4.49473923827281));
#101491=CARTESIAN_POINT('Origin',(0.159147628181055,3.08928603080669,0.10927948382582));
#101492=CARTESIAN_POINT('',(-5.83106864191144,3.13852541968788,-4.51382752721755));
#101493=CARTESIAN_POINT('Origin',(-2.86663054405167E-13,3.22948687200044,
-1.5330618718945E-13));
#101494=CARTESIAN_POINT('',(-6.32846662957753,3.22840427021542,-4.02498572848737));
#101495=CARTESIAN_POINT('Origin',(0.172289535163268,3.08929953212073,0.0832684844022252));
#101496=CARTESIAN_POINT('Ctrl Pts',(-6.00394194929151,3.13852541968788,
-4.49473924624893));
#101497=CARTESIAN_POINT('Ctrl Pts',(-6.14811695100994,3.176642188,-4.30215449199858));
#101498=CARTESIAN_POINT('Ctrl Pts',(-6.27965341900987,3.214285714,-4.10072590299827));
#101499=CARTESIAN_POINT('Ctrl Pts',(-6.30428751723109,3.22133557899334,
-4.0630024360247));
#101500=CARTESIAN_POINT('Ctrl Pts',(-6.32846662470299,3.22840426981355,
-4.02498573602417));
#101501=CARTESIAN_POINT('Ctrl Pts',(-5.13028864,3.007773793,-5.47084440199999));
#101502=CARTESIAN_POINT('Ctrl Pts',(-5.429525439,3.07352872,-5.190234859));
#101503=CARTESIAN_POINT('Ctrl Pts',(-5.696371877,3.138525418,-4.878662465));
#101504=CARTESIAN_POINT('Ctrl Pts',(-5.69902867144889,3.13917254249503,
-4.8755603669806));
#101505=CARTESIAN_POINT('Ctrl Pts',(-5.70168546589777,3.13981966699007,
-4.87245826896118));
#101506=CARTESIAN_POINT('Ctrl Pts',(-5.130049363,3.007773793,-5.122996538));
#101507=CARTESIAN_POINT('Ctrl Pts',(-5.410260054,3.07352872,-4.842400082));
#101508=CARTESIAN_POINT('Ctrl Pts',(-5.658195312,3.138525418,-4.532915818));
#101509=CARTESIAN_POINT('Ctrl Pts',(-5.66066382168697,3.13917254249503,
-4.5298345099609));
#101510=CARTESIAN_POINT('Ctrl Pts',(-5.66313233137395,3.13981966699007,
-4.52675320192181));
#101511=CARTESIAN_POINT('',(-5.69637187435097,3.13852541850723,-4.8786624651115));
#101512=CARTESIAN_POINT('',(-5.67728358890492,3.13852541943002,-4.70578914825017));
#101513=CARTESIAN_POINT('',(-5.31049850488852,3.04797057322864,-5.29609343840933));
#101514=CARTESIAN_POINT('Origin',(0.121722443726788,2.9464820914821,0.144358776216413));
#101515=CARTESIAN_POINT('Ctrl Pts',(-5.13339538944628,3.00855922360106,
-5.11964373170498));
#101516=CARTESIAN_POINT('Ctrl Pts',(-5.16284109107939,3.01545478677039,
-5.14903758173383));
#101517=CARTESIAN_POINT('Ctrl Pts',(-5.1923396093951,3.02218156072343,-5.17845385122894));
#101518=CARTESIAN_POINT('Ctrl Pts',(-5.25136514995679,3.03530792008805,
-5.23725990226701));
#101519=CARTESIAN_POINT('Ctrl Pts',(-5.28092582206647,3.04171498172015,
-5.26668320461477));
#101520=CARTESIAN_POINT('Ctrl Pts',(-5.31049849750202,3.04797057328804,
-5.29609343790255));
#101521=CARTESIAN_POINT('Ctrl Pts',(-4.89116456977673,3.13983235804358,
-5.68564645093098));
#101522=CARTESIAN_POINT('Ctrl Pts',(-4.89425081288837,3.13917888802179,
-5.68298562196549));
#101523=CARTESIAN_POINT('Ctrl Pts',(-4.897337056,3.138525418,-5.68032479300001));
#101524=CARTESIAN_POINT('Ctrl Pts',(-5.20630485,3.073105688,-5.41394576));
#101525=CARTESIAN_POINT('Ctrl Pts',(-5.484557207,3.007781414,-5.11562628));
#101526=CARTESIAN_POINT('Ctrl Pts',(-4.54533470543984,3.13983235804358,
-5.64822932251851));
#101527=CARTESIAN_POINT('Ctrl Pts',(-4.54840082321992,3.13917888802179,
-5.64575641225926));
#101528=CARTESIAN_POINT('Ctrl Pts',(-4.551466941,3.138525418,-5.643283502));
#101529=CARTESIAN_POINT('Ctrl Pts',(-4.85841996200001,3.073105688,-5.395717254));
#101530=CARTESIAN_POINT('Ctrl Pts',(-5.136709949,3.007781414,-5.1163181));
#101531=CARTESIAN_POINT('',(-4.8973370310442,3.13852541976208,-5.68032477216621));
#101532=CARTESIAN_POINT('Origin',(0.131934875247602,3.08928601505222,0.140936509631236));
#101533=CARTESIAN_POINT('',(-4.72440200654202,3.13852541968788,-5.66180414078946));
#101534=CARTESIAN_POINT('Origin',(8.46978737145676E-13,3.22948687200067,
8.92515228390067E-13));
#101535=CARTESIAN_POINT('',(-5.31525764263672,3.22840427020599,-5.29131705602687));
#101536=CARTESIAN_POINT('Origin',(0.150361561841226,3.08929951791396,0.118359186089775));
#101537=CARTESIAN_POINT('Ctrl Pts',(-4.89733704796982,3.13852541968788,
-5.68032478431973));
#101538=CARTESIAN_POINT('Ctrl Pts',(-5.07954134901011,3.176642188,-5.52323591800075));
#101539=CARTESIAN_POINT('Ctrl Pts',(-5.25130375901012,3.214285714,-5.35479307000043));
#101540=CARTESIAN_POINT('Ctrl Pts',(-5.28347135607228,3.22133557898738,
-5.32324715960407));
#101541=CARTESIAN_POINT('Ctrl Pts',(-5.3152576362352,3.22840426981355,-5.291317062339));
#101542=CARTESIAN_POINT('Ctrl Pts',(-3.834275513,3.007773793,-6.445799508));
#101543=CARTESIAN_POINT('Ctrl Pts',(-4.186839079,3.07352872,-6.236077526));
#101544=CARTESIAN_POINT('Ctrl Pts',(-4.51442565,3.138525418,-5.989153617));
#101545=CARTESIAN_POINT('Ctrl Pts',(-4.51768718944525,3.13917254249503,
-5.98669517657394));
#101546=CARTESIAN_POINT('Ctrl Pts',(-4.52094872889051,3.13981966699007,
-5.98423673614789));
#101547=CARTESIAN_POINT('Ctrl Pts',(-3.908818839,3.007773793,-6.106032696));
#101548=CARTESIAN_POINT('Ctrl Pts',(-4.242798303,3.07352872,-5.892233444));
#101549=CARTESIAN_POINT('Ctrl Pts',(-4.551466941,3.138525418,-5.643283502));
#101550=CARTESIAN_POINT('Ctrl Pts',(-4.55454012844867,3.13917254249503,
-5.64080488984796));
#101551=CARTESIAN_POINT('Ctrl Pts',(-4.55761331589734,3.13981966699007,
-5.63832627769592));
#101552=CARTESIAN_POINT('',(-4.51442564736557,3.13852541850725,-5.98915361657509));
#101553=CARTESIAN_POINT('',(-4.53294628858464,3.13852541943002,-5.81621856488957));
#101554=CARTESIAN_POINT('',(-4.04783846321783,3.04797057326586,-6.3138739184838));
#101555=CARTESIAN_POINT('Origin',(0.0878437618876299,2.94648209802678,0.167150436905271));
#101556=CARTESIAN_POINT('Ctrl Pts',(-3.91280739158268,3.008559223625,-6.10347757308111));
#101557=CARTESIAN_POINT('Ctrl Pts',(-3.93524586011906,3.01545478681085,
-6.138514166815));
#101558=CARTESIAN_POINT('Ctrl Pts',(-3.95773109096271,3.0221815607577,-6.17358400974169));
#101559=CARTESIAN_POINT('Ctrl Pts',(-4.00273508442949,3.03530792013278,
-6.24370395450373));
#101560=CARTESIAN_POINT('Ctrl Pts',(-4.02527950415133,3.04171498176201,
-6.27879402706656));
#101561=CARTESIAN_POINT('Ctrl Pts',(-4.04783845603459,3.04797057332588,
-6.31387391645986));
#101562=CARTESIAN_POINT('Ctrl Pts',(-3.55456593991965,3.13983235804358,
-6.60417499745422));
#101563=CARTESIAN_POINT('Ctrl Pts',(-3.55815202795982,3.13917888802179,
-6.60223982822711));
#101564=CARTESIAN_POINT('Ctrl Pts',(-3.561738116,3.138525418,-6.600304659));
#101565=CARTESIAN_POINT('Ctrl Pts',(-3.920746033,3.073105688,-6.406572362));
#101566=CARTESIAN_POINT('Ctrl Pts',(-4.256622874,3.007781414,-6.175043458));
#101567=CARTESIAN_POINT('Ctrl Pts',(-3.22486496249061,3.13983235804358,
-6.49328946261242));
#101568=CARTESIAN_POINT('Ctrl Pts',(-3.2283909987453,3.13917888802179,-6.49153349230621));
#101569=CARTESIAN_POINT('Ctrl Pts',(-3.231917035,3.138525418,-6.48977752200001));
#101570=CARTESIAN_POINT('Ctrl Pts',(-3.58491309,3.073105688,-6.313985061));
#101571=CARTESIAN_POINT('Ctrl Pts',(-3.916759371,3.007781414,-6.100942225));
#101572=CARTESIAN_POINT('',(-3.56173809610214,3.13852541976265,-6.60030463329241));
#101573=CARTESIAN_POINT('Origin',(0.0985531836936841,3.08928598123718,0.166003673652068));
#101574=CARTESIAN_POINT('',(-3.39682758479658,3.13852541968788,-6.54504108567515));
#101575=CARTESIAN_POINT('Origin',(5.42101086242752E-13,3.22948687200056,
8.91647866652079E-13));
#101576=CARTESIAN_POINT('',(-4.05351311580907,3.22840427022695,-6.31023227897596));
#101577=CARTESIAN_POINT('Origin',(0.121402364643847,3.08929956194483,0.147915157976117));
#101578=CARTESIAN_POINT('Ctrl Pts',(-3.56173811002333,3.13852541968788,
-6.60030464879634));
#101579=CARTESIAN_POINT('Ctrl Pts',(-3.7734520380093,3.176642188,-6.4860569710028));
#101580=CARTESIAN_POINT('Ctrl Pts',(-3.97740897200938,3.214285714,-6.35847606500249));
#101581=CARTESIAN_POINT('Ctrl Pts',(-4.01560594677838,3.22133557899676,
-6.33458276279003));
#101582=CARTESIAN_POINT('Ctrl Pts',(-4.05351310833931,3.22840426981258,
-6.31023228380055));
#101583=CARTESIAN_POINT('Ctrl Pts',(-2.358975924,3.007773793,-7.11935619199999));
#101584=CARTESIAN_POINT('Ctrl Pts',(-2.748380777,3.07352872,-6.990328138));
#101585=CARTESIAN_POINT('Ctrl Pts',(-3.121389897,3.138525418,-6.819598603));
#101586=CARTESIAN_POINT('Ctrl Pts',(-3.12510367548184,3.13917254249503,
-6.8178987741237));
#101587=CARTESIAN_POINT('Ctrl Pts',(-3.12881745396368,3.13981966699007,
-6.81619894524741));
#101588=CARTESIAN_POINT('Ctrl Pts',(-2.50481629,3.007773793,-6.803557551));
#101589=CARTESIAN_POINT('Ctrl Pts',(-2.876948019,3.07352872,-6.66655252));
#101590=CARTESIAN_POINT('Ctrl Pts',(-3.231917035,3.138525418,-6.489777522));
#101591=CARTESIAN_POINT('Ctrl Pts',(-3.23545120138537,3.13917254249503,
-6.48801750287848));
#101592=CARTESIAN_POINT('Ctrl Pts',(-3.23898536777074,3.13981966699007,
-6.48625748375697));
#101593=CARTESIAN_POINT('',(-3.12138989451244,3.13852541850726,-6.81959860202427));
#101594=CARTESIAN_POINT('',(-3.17665345808772,3.13852541943002,-6.65468806627697));
#101595=CARTESIAN_POINT('',(-2.59590599360655,3.0479705733211,-7.03642467113093));
#101596=CARTESIAN_POINT('Origin',(0.0498576734522127,2.94648212933595,0.182126481435873));
#101597=CARTESIAN_POINT('Ctrl Pts',(-2.50926086840672,3.00855922369567,
-6.80191958692094));
#101598=CARTESIAN_POINT('Ctrl Pts',(-2.52364290616179,3.01545478692602,
-6.84096065214121));
#101599=CARTESIAN_POINT('Ctrl Pts',(-2.53806346503707,3.02218156078119,
-6.88004424097906));
#101600=CARTESIAN_POINT('Ctrl Pts',(-2.56694157478864,3.03530792019364,
-6.95819934879997));
#101601=CARTESIAN_POINT('Ctrl Pts',(-2.58141559011017,3.04171498182181,
-6.99731541877659));
#101602=CARTESIAN_POINT('Ctrl Pts',(-2.59590598689054,3.04797057338195,
-7.03642466765963));
#101603=CARTESIAN_POINT('Ctrl Pts',(-2.05175975706096,3.13983235804358,
-7.2138996612507));
#101604=CARTESIAN_POINT('Ctrl Pts',(-2.05567800853048,3.13917888802179,
-7.21278063812536));
#101605=CARTESIAN_POINT('Ctrl Pts',(-2.05959626,3.138525418,-7.211661615));
#101606=CARTESIAN_POINT('Ctrl Pts',(-2.451857488,3.073105688,-7.099634761));
#101607=CARTESIAN_POINT('Ctrl Pts',(-2.829653587,3.007781414,-6.945722466));
#101608=CARTESIAN_POINT('Ctrl Pts',(-1.75360411761002,3.13983235804358,
-7.03473060324848));
#101609=CARTESIAN_POINT('Ctrl Pts',(-1.75742519880501,3.13917888802179,
-7.03377368012423));
#101610=CARTESIAN_POINT('Ctrl Pts',(-1.76124628,3.138525418,-7.032816757));
#101611=CARTESIAN_POINT('Ctrl Pts',(-2.143779666,3.073105688,-6.937017944));
#101612=CARTESIAN_POINT('Ctrl Pts',(-2.513665477,3.007781414,-6.800293072));
#101613=CARTESIAN_POINT('',(-2.05959624554176,3.13852541980597,-7.21166158551047));
#101614=CARTESIAN_POINT('Origin',(0.0605632130569449,3.08928603561543,0.183308723200907));
#101615=CARTESIAN_POINT('',(-1.91042128011643,3.13852541968788,-7.12223918328643));
#101616=CARTESIAN_POINT('Origin',(-1.12106504635001E-13,3.22948687199956,
-3.78603398631938E-13));
#101617=CARTESIAN_POINT('',(-2.60223082099891,3.22840427021944,-7.03408805428349));
#101618=CARTESIAN_POINT('Origin',(0.0867666093238001,3.0892995251928,0.170554746126368));
#101619=CARTESIAN_POINT('Ctrl Pts',(-2.05959625635551,3.13852541968788,
-7.21166160374947));
#101620=CARTESIAN_POINT('Ctrl Pts',(-2.29092030400738,3.176642188,-7.14559720900411));
#101621=CARTESIAN_POINT('Ctrl Pts',(-2.5175349620075,3.214285714,-7.06484378600387));
#101622=CARTESIAN_POINT('Ctrl Pts',(-2.55997526625953,3.2213355789953,-7.04972031639188));
#101623=CARTESIAN_POINT('Ctrl Pts',(-2.60223081258653,3.22840426981265,
-7.03408805734967));
#101624=CARTESIAN_POINT('Ctrl Pts',(-0.773373243,3.007773793,-7.460019693));
#101625=CARTESIAN_POINT('Ctrl Pts',(-1.181411245,3.07352872,-7.417718777));
#101626=CARTESIAN_POINT('Ctrl Pts',(-1.582401422,3.138525418,-7.331166738));
#101627=CARTESIAN_POINT('Ctrl Pts',(-1.586393787363,3.13917254249503,-7.33030500276951));
#101628=CARTESIAN_POINT('Ctrl Pts',(-1.590386152726,3.13981966699007,-7.32944326753902));
#101629=CARTESIAN_POINT('Ctrl Pts',(-0.983691316,3.007773793,-7.18295561700001));
#101630=CARTESIAN_POINT('Ctrl Pts',(-1.376574843,3.07352872,-7.12915100900001));
#101631=CARTESIAN_POINT('Ctrl Pts',(-1.76124628,3.138525418,-7.032816757));
#101632=CARTESIAN_POINT('Ctrl Pts',(-1.76507617162653,3.13917254249503,
-7.03185762744268));
#101633=CARTESIAN_POINT('Ctrl Pts',(-1.76890606325307,3.13981966699007,
-7.03089849788536));
#101634=CARTESIAN_POINT('',(-1.58240141979824,3.13852541850725,-7.33116673650153));
#101635=CARTESIAN_POINT('',(-1.67182384246077,3.13852541943002,-7.18199174948777));
#101636=CARTESIAN_POINT('',(-1.02259184491922,3.04797057332665,-7.42996002711352));
#101637=CARTESIAN_POINT('Origin',(0.00954017391375017,2.94648215635932,
0.188586111446705));
#101638=CARTESIAN_POINT('Ctrl Pts',(-0.98838409649014,3.00855922368921,
-7.18231140053146));
#101639=CARTESIAN_POINT('Ctrl Pts',(-0.994037214996654,3.0154547869579,
-7.22353142049163));
#101640=CARTESIAN_POINT('Ctrl Pts',(-0.999718812719134,3.02218156078833,
-7.26480125048925));
#101641=CARTESIAN_POINT('Ctrl Pts',(-1.01112073015354,3.0353079202144,-7.34733707545125));
#101642=CARTESIAN_POINT('Ctrl Pts',(-1.01684755219726,3.04171498183755,
-7.38865011893273));
#101643=CARTESIAN_POINT('Ctrl Pts',(-1.02259183909231,3.04797057338766,
-7.42996002228574));
#101644=CARTESIAN_POINT('Ctrl Pts',(-0.453015568348983,3.13983235804358,
-7.48631039345565));
#101645=CARTESIAN_POINT('Ctrl Pts',(-0.457082770174492,3.13917888802179,
-7.48605984072783));
#101646=CARTESIAN_POINT('Ctrl Pts',(-0.461149972,3.138525418,-7.485809288));
#101647=CARTESIAN_POINT('Ctrl Pts',(-0.868322813,3.073105688,-7.46072613));
#101648=CARTESIAN_POINT('Ctrl Pts',(-1.270372842,3.007781414,-7.391627212));
#101649=CARTESIAN_POINT('Ctrl Pts',(-0.200346692749638,3.13983235804358,
-7.24723556060148));
#101650=CARTESIAN_POINT('Ctrl Pts',(-0.204284149374819,3.13917888802179,
-7.24712242930074));
#101651=CARTESIAN_POINT('Ctrl Pts',(-0.208221606,3.138525418,-7.24700929800001));
#101652=CARTESIAN_POINT('Ctrl Pts',(-0.602405487000001,3.073105688,-7.235683577));
#101653=CARTESIAN_POINT('Ctrl Pts',(-0.99303538,3.007781414,-7.181669773));
#101654=CARTESIAN_POINT('',(-0.461149964227287,3.13852541980534,-7.48580925609884));
#101655=CARTESIAN_POINT('Origin',(0.0197412726344003,3.08928600276568,0.192041965304161));
#101656=CARTESIAN_POINT('',(-0.334685799463248,3.13852541968788,-7.36640929252461));
#101657=CARTESIAN_POINT('Origin',(-3.29326409892472E-14,3.22948687200011,
3.54750950837257E-13));
#101658=CARTESIAN_POINT('',(-1.02927110501602,3.2284042702107,-7.42903768943116));
#101659=CARTESIAN_POINT('Origin',(0.0480737921300024,3.08929955132135,0.185219410294131));
#101660=CARTESIAN_POINT('Ctrl Pts',(-0.461149970859381,3.13852541968788,
-7.48580927622917));
#101661=CARTESIAN_POINT('Ctrl Pts',(-0.701267683007476,3.176642188,-7.47101726400662));
#101662=CARTESIAN_POINT('Ctrl Pts',(-0.93994381500768,3.214285714,-7.44086726300637));
#101663=CARTESIAN_POINT('Ctrl Pts',(-0.984642987471772,3.2213355789848,
-7.43522078275191));
#101664=CARTESIAN_POINT('Ctrl Pts',(-1.02927109619218,3.22840426981355,
-7.42903769066228));
#101665=CARTESIAN_POINT('Ctrl Pts',(0.848391511,3.007773793,-7.451860965));
#101666=CARTESIAN_POINT('Ctrl Pts',(0.440799764,3.07352872,-7.498265129));
#101667=CARTESIAN_POINT('Ctrl Pts',(0.030578384,3.138525418,-7.499937664));
#101668=CARTESIAN_POINT('Ctrl Pts',(0.0264941103129808,3.13917254249503,
-7.49995431620543));
#101669=CARTESIAN_POINT('Ctrl Pts',(0.0224098366259617,3.13981966699007,
-7.49997096841086));
#101670=CARTESIAN_POINT('Ctrl Pts',(0.583429972,3.007773793,-7.226486661));
#101671=CARTESIAN_POINT('Ctrl Pts',(0.188165442,3.07352872,-7.25839832));
#101672=CARTESIAN_POINT('Ctrl Pts',(-0.208221606,3.138525418,-7.247009298));
#101673=CARTESIAN_POINT('Ctrl Pts',(-0.212168141380535,3.13917254249503,
-7.24689590585336));
#101674=CARTESIAN_POINT('Ctrl Pts',(-0.216114676761069,3.13981966699007,
-7.24678251370672));
#101675=CARTESIAN_POINT('',(0.0305783858254823,3.13852541850725,-7.49993766206233));
#101676=CARTESIAN_POINT('',(-0.0888216022330979,3.13852541943002,-7.37347348110561));
#101677=CARTESIAN_POINT('',(0.598537562247386,3.04797057329688,-7.47607870979874));
#101678=CARTESIAN_POINT('Origin',(-0.0312233212322582,2.94648213638327,
0.186228177115241));
#101679=CARTESIAN_POINT('Ctrl Pts',(0.57870841876267,3.00855922356026,-7.22686631446595));
#101680=CARTESIAN_POINT('Ctrl Pts',(0.58204855259275,3.01545478674394,-7.26833788632441));
#101681=CARTESIAN_POINT('Ctrl Pts',(0.585371580930391,3.02218156076013,
-7.30986422746823));
#101682=CARTESIAN_POINT('Ctrl Pts',(0.591978996394136,3.03530792013989,
-7.39292148582055));
#101683=CARTESIAN_POINT('Ctrl Pts',(0.595267147374943,3.04171498178307,
-7.43449975095489));
#101684=CARTESIAN_POINT('Ctrl Pts',(0.59853756682197,3.04797057335751,-7.47607870383028));
#101685=CARTESIAN_POINT('Ctrl Pts',(1.16691112465914,3.13983235804358,-7.40866957357816));
#101686=CARTESIAN_POINT('Ctrl Pts',(1.16288515032957,3.13917888802179,-7.40929920678909));
#101687=CARTESIAN_POINT('Ctrl Pts',(1.158859176,3.138525418,-7.40992884));
#101688=CARTESIAN_POINT('Ctrl Pts',(0.755813673,3.073105688,-7.472962236));
#101689=CARTESIAN_POINT('Ctrl Pts',(0.348309125,3.007781414,-7.491907685));
#101690=CARTESIAN_POINT('Ctrl Pts',(1.36227871992292,3.13983235804358,-7.12086783712926));
#101691=CARTESIAN_POINT('Ctrl Pts',(1.35840899896146,3.13917888802179,-7.12160378756463));
#101692=CARTESIAN_POINT('Ctrl Pts',(1.354539278,3.138525418,-7.122339738));
#101693=CARTESIAN_POINT('Ctrl Pts',(0.967136502,3.073105688,-7.19601668900001));
#101694=CARTESIAN_POINT('Ctrl Pts',(0.574027948,3.007781414,-7.227239578));
#101695=CARTESIAN_POINT('',(1.15885917628989,3.13852541976333,-7.40992880748018));
#101696=CARTESIAN_POINT('Origin',(-0.0220036510827664,3.08928604246497,
0.191796247293505));
#101697=CARTESIAN_POINT('',(1.25669921667914,3.13852541968789,-7.26613429078503));
#101698=CARTESIAN_POINT('Origin',(1.20100801591187E-13,3.22948687200011,
-1.8028113724089E-12));
#101699=CARTESIAN_POINT('',(0.591816183700481,3.22840427021323,-7.47661377888631));
#101700=CARTESIAN_POINT('Origin',(0.00713314255942156,3.08929953360765,
0.191223796675345));
#101701=CARTESIAN_POINT('Ctrl Pts',(1.15885917458283,3.13852541968788,-7.4099288282602));
#101702=CARTESIAN_POINT('Ctrl Pts',(0.921175435994036,3.176642188,-7.44710085400819));
#101703=CARTESIAN_POINT('Ctrl Pts',(0.681598059993781,3.214285714,-7.46896405700799));
#101704=CARTESIAN_POINT('Ctrl Pts',(0.636730102971802,3.22133557898984,
-7.47305858888712));
#101705=CARTESIAN_POINT('Ctrl Pts',(0.591816192611198,3.22840426981315,
-7.47661377814827));
#101706=CARTESIAN_POINT('Ctrl Pts',(2.430486421,3.007773793,-7.0952615));
#101707=CARTESIAN_POINT('Ctrl Pts',(2.042399466,3.07352872,-7.228200938));
#101708=CARTESIAN_POINT('Ctrl Pts',(1.64212838,3.138525418,-7.31801984));
#101709=CARTESIAN_POINT('Ctrl Pts',(1.63814317409917,3.13917254249503,-7.31891410099156));
#101710=CARTESIAN_POINT('Ctrl Pts',(1.63415796819833,3.13981966699007,-7.31980836198311));
#101711=CARTESIAN_POINT('Ctrl Pts',(2.123270722,3.007773793,-6.932115221));
#101712=CARTESIAN_POINT('Ctrl Pts',(1.744107321,3.07352872,-7.048250993));
#101713=CARTESIAN_POINT('Ctrl Pts',(1.354539278,3.138525418,-7.12233973800001));
#101714=CARTESIAN_POINT('Ctrl Pts',(1.35066063445556,3.13917254249503,-7.12307738534472));
#101715=CARTESIAN_POINT('Ctrl Pts',(1.34678199091112,3.13981966699007,-7.12381503268945));
#101716=CARTESIAN_POINT('',(1.64212838139077,3.13852541850725,-7.31801983771826));
#101717=CARTESIAN_POINT('',(1.49833383758464,3.13852541943002,-7.22017978721851));
#101718=CARTESIAN_POINT('',(2.19168001780487,3.04797057328338,-7.1726242606184));
#101719=CARTESIAN_POINT('Origin',(-0.0705268460826172,2.9464821631811,0.175162031611241));
#101720=CARTESIAN_POINT('Ctrl Pts',(2.11874117040445,3.00855922370958,-6.93350099351421));
#101721=CARTESIAN_POINT('Ctrl Pts',(2.13091837590938,3.01545478694813,-6.97328495323188));
#101722=CARTESIAN_POINT('Ctrl Pts',(2.1430906492882,3.02218156082002,-7.01312607782696));
#101723=CARTESIAN_POINT('Ctrl Pts',(2.16739844252111,3.03530792020108,-7.09282110458575));
#101724=CARTESIAN_POINT('Ctrl Pts',(2.1795478163059,3.04171498180817,-7.13272043750306));
#101725=CARTESIAN_POINT('Ctrl Pts',(2.19168002095519,3.04797057334374,-7.17262425381494));
#101726=CARTESIAN_POINT('Ctrl Pts',(2.7322743505124,3.13983235804358,-6.98460759756821));
#101727=CARTESIAN_POINT('Ctrl Pts',(2.7284778537562,3.13917888802179,-6.98608797578411));
#101728=CARTESIAN_POINT('Ctrl Pts',(2.724681357,3.138525418,-6.987568354));
#101729=CARTESIAN_POINT('Ctrl Pts',(2.344609151,3.073105688,-7.135770934));
#101730=CARTESIAN_POINT('Ctrl Pts',(1.950704544,3.007781414,-7.24187488));
#101731=CARTESIAN_POINT('Ctrl Pts',(2.86120549389769,3.13983235804358,-6.661536248119));
#101732=CARTESIAN_POINT('Ctrl Pts',(2.85758445244885,3.13917888802179,-6.6630868680595));
#101733=CARTESIAN_POINT('Ctrl Pts',(2.853963411,3.138525418,-6.664637488));
#101734=CARTESIAN_POINT('Ctrl Pts',(2.491456263,3.073105688,-6.819872058));
#101735=CARTESIAN_POINT('Ctrl Pts',(2.114250367,3.007781414,-6.934871692));
#101736=CARTESIAN_POINT('',(2.72468135066201,3.13852541980582,-6.98756832177496));
#101737=CARTESIAN_POINT('Origin',(-0.0627196471463952,3.08928604481397,
0.182581748066019));
#101738=CARTESIAN_POINT('',(2.78932237430421,3.13852541968788,-6.82610292496196));
#101739=CARTESIAN_POINT('Origin',(-2.31043482956661E-13,3.22948687200044,
7.12971348626468E-13));
#101740=CARTESIAN_POINT('',(2.18523080594797,3.22840427023862,-7.17459171825009));
#101741=CARTESIAN_POINT('Origin',(-0.0341410904281592,3.08929951162922,
0.188286562003838));
#101742=CARTESIAN_POINT('Ctrl Pts',(2.72468135309239,3.13852541968788,-6.98756834283909));
#101743=CARTESIAN_POINT('Ctrl Pts',(2.50054541499605,3.176642188,-7.07496628600903));
#101744=CARTESIAN_POINT('Ctrl Pts',(2.27126916799576,3.214285714,-7.14782039300889));
#101745=CARTESIAN_POINT('Ctrl Pts',(2.22833040210814,3.22133557900871,-7.16146448151981));
#101746=CARTESIAN_POINT('Ctrl Pts',(2.18523081450453,3.22840426981356,-7.17459171559583));
#101747=CARTESIAN_POINT('Ctrl Pts',(3.898934487,3.007773793,-6.406895494));
#101748=CARTESIAN_POINT('Ctrl Pts',(3.548498839,3.07352872,-6.620154104));
#101749=CARTESIAN_POINT('Ctrl Pts',(3.176894277,3.138525418,-6.79391954300001));
#101750=CARTESIAN_POINT('Ctrl Pts',(3.17319448267296,3.13917254249503,-6.79564959814783));
#101751=CARTESIAN_POINT('Ctrl Pts',(3.16949468834593,3.13981966699007,-6.79737965329567));
#101752=CARTESIAN_POINT('Ctrl Pts',(3.563829693,3.007773793,-6.313605778));
#101753=CARTESIAN_POINT('Ctrl Pts',(3.21849668,3.07352872,-6.508535283));
#101754=CARTESIAN_POINT('Ctrl Pts',(2.853963411,3.138525418,-6.664637488));
#101755=CARTESIAN_POINT('Ctrl Pts',(2.85033402035581,3.13917254249503,-6.66619168326981));
#101756=CARTESIAN_POINT('Ctrl Pts',(2.84670462971162,3.13981966699007,-6.6677458785396));
#101757=CARTESIAN_POINT('',(3.17689427783338,3.13852541850723,-6.7939195404758));
#101758=CARTESIAN_POINT('',(3.01542885200097,3.13852541943002,-6.72927851191472));
#101759=CARTESIAN_POINT('',(3.68234195126533,3.04797057322359,-6.53378587281428));
#101760=CARTESIAN_POINT('Origin',(-0.106532830040017,2.9464820989943,0.155905996139329));
#101761=CARTESIAN_POINT('Ctrl Pts',(3.55970394000874,3.00855922362529,-6.31593287126577));
#101762=CARTESIAN_POINT('Ctrl Pts',(3.58014882442165,3.01545478682465,-6.35216896468786));
#101763=CARTESIAN_POINT('Ctrl Pts',(3.60060118097571,3.0221815607465,-6.38846194717738));
#101764=CARTESIAN_POINT('Ctrl Pts',(3.64147274623553,3.03530792011833,-6.4610682912835));
#101765=CARTESIAN_POINT('Ctrl Pts',(3.66191525145192,3.04171498173437,-6.49742304369186));
#101766=CARTESIAN_POINT('Ctrl Pts',(3.68234195274149,3.0479705732829,-6.53378586556781));
#101767=CARTESIAN_POINT('Ctrl Pts',(4.16987946444665,3.13983235804358,-6.23395313325984));
#101768=CARTESIAN_POINT('Ctrl Pts',(4.16648996522332,3.13917888802179,-6.23621503562992));
#101769=CARTESIAN_POINT('Ctrl Pts',(4.163100466,3.138525418,-6.238476938));
#101770=CARTESIAN_POINT('Ctrl Pts',(3.82377331,3.073105688,-6.46491891300001));
#101771=CARTESIAN_POINT('Ctrl Pts',(3.461887187,3.007781414,-6.653220055));
#101772=CARTESIAN_POINT('Ctrl Pts',(4.22634547911204,3.13983235804358,-5.89071862761956));
#101773=CARTESIAN_POINT('Ctrl Pts',(4.22314243305602,3.13917888802179,-5.89301141180978));
#101774=CARTESIAN_POINT('Ctrl Pts',(4.219939387,3.138525418,-5.895304196));
#101775=CARTESIAN_POINT('Ctrl Pts',(3.899278299,3.073105688,-6.12483779));
#101776=CARTESIAN_POINT('Ctrl Pts',(3.555612789,3.007781414,-6.318236914));
#101777=CARTESIAN_POINT('',(4.16310045288277,3.13852541980557,-6.23847690789766));
#101778=CARTESIAN_POINT('Origin',(-0.10050314211654,3.08928601196563,0.164830506409255));
#101779=CARTESIAN_POINT('',(4.19151991788259,3.13852541968788,-6.06689057295364));
#101780=CARTESIAN_POINT('Origin',(-8.87744738831131E-13,3.22948687200044,
1.49229587020905E-12));
#101781=CARTESIAN_POINT('',(3.67646646406889,3.22840427021341,-6.53709372269269));
#101782=CARTESIAN_POINT('Origin',(-0.073818884042236,3.08929956416316,0.176545072854689));
#101783=CARTESIAN_POINT('Ctrl Pts',(4.16310045978442,3.13852541968788,-6.23847692794034));
#101784=CARTESIAN_POINT('Ctrl Pts',(3.96299266999802,3.176642188,-6.37201415700994));
#101785=CARTESIAN_POINT('Ctrl Pts',(3.75473825299771,3.214285714,-6.49245259100987));
#101786=CARTESIAN_POINT('Ctrl Pts',(3.71573644753807,3.22133557899732,-6.51500825378087));
#101787=CARTESIAN_POINT('Ctrl Pts',(3.67646647191127,3.22840426981354,-6.53709371808503));
#101788=CARTESIAN_POINT('Ctrl Pts',(5.18507271,3.007773793,-5.418950174));
#101789=CARTESIAN_POINT('Ctrl Pts',(4.888674351,3.07352872,-5.702556223));
#101790=CARTESIAN_POINT('Ctrl Pts',(4.563112129,3.138525418,-5.952143118));
#101791=CARTESIAN_POINT('Ctrl Pts',(4.55987074451438,3.13917254249503,-5.95462807182634));
#101792=CARTESIAN_POINT('Ctrl Pts',(4.55662936002876,3.13981966699007,-5.95711302565267));
#101793=CARTESIAN_POINT('Ctrl Pts',(4.837747949,3.007773793,-5.399879145));
#101794=CARTESIAN_POINT('Ctrl Pts',(4.542392711,3.07352872,-5.664487697));
#101795=CARTESIAN_POINT('Ctrl Pts',(4.219939387,3.138525418,-5.895304196));
#101796=CARTESIAN_POINT('Ctrl Pts',(4.21672895553369,3.13917254249503,-5.89760226674754));
#101797=CARTESIAN_POINT('Ctrl Pts',(4.21351852406738,3.13981966699007,-5.89990033749508));
#101798=CARTESIAN_POINT('',(4.5631121292891,3.13852541850725,-5.95214311534969));
#101799=CARTESIAN_POINT('',(4.39152576504318,3.13852541943002,-5.92372365177857));
#101800=CARTESIAN_POINT('',(5.00082166817462,3.04797057327088,-5.58943491989446));
#101801=CARTESIAN_POINT('Origin',(-0.137557002453182,2.94648211136749,0.12935920701272));
#101802=CARTESIAN_POINT('Ctrl Pts',(4.8342189097993,3.00855922380044,-5.40303874779572));
#101803=CARTESIAN_POINT('Ctrl Pts',(4.86197549338503,3.01545478703697,-5.43403261591302));
#101804=CARTESIAN_POINT('Ctrl Pts',(4.88975160317973,3.02218156082008,-5.46508043598458));
#101805=CARTESIAN_POINT('Ctrl Pts',(4.94527583198523,3.03530792020206,-5.52720310594268));
#101806=CARTESIAN_POINT('Ctrl Pts',(4.97305559995048,3.04171498179997,-5.5583133700908));
#101807=CARTESIAN_POINT('Ctrl Pts',(5.00082166815137,3.04797057333098,-5.58943491241765));
#101808=CARTESIAN_POINT('Ctrl Pts',(5.41250564892147,3.13983235804358,-5.19180595003168));
#101809=CARTESIAN_POINT('Ctrl Pts',(5.40968163646074,3.13917888802179,-5.19474361251584));
#101810=CARTESIAN_POINT('Ctrl Pts',(5.40685762400001,3.138525418,-5.197681275));
#101811=CARTESIAN_POINT('Ctrl Pts',(5.12414208000001,3.073105688,-5.49177447));
#101812=CARTESIAN_POINT('Ctrl Pts',(4.81119583200001,3.007781414,-5.753468055));
#101813=CARTESIAN_POINT('Ctrl Pts',(5.39386624760078,3.13983235804358,-4.84445755122613));
#101814=CARTESIAN_POINT('Ctrl Pts',(5.39123096780039,3.13917888802179,-4.84738529161306));
#101815=CARTESIAN_POINT('Ctrl Pts',(5.388595688,3.138525418,-4.850313032));
#101816=CARTESIAN_POINT('Ctrl Pts',(5.124774415,3.073105688,-5.143412913));
#101817=CARTESIAN_POINT('Ctrl Pts',(4.830718708,3.007781414,-5.406168399));
#101818=CARTESIAN_POINT('',(5.40685760454955,3.1385254197632,-5.19768124893519));
#101819=CARTESIAN_POINT('Origin',(-0.133587032587033,3.08928604981775,0.139371560321166));
#101820=CARTESIAN_POINT('',(5.39772664886391,3.13852541968788,-5.02399716116693));
#101821=CARTESIAN_POINT('Origin',(1.1067535776732E-12,3.22948687199922,
-1.24639881748934E-12));
#101822=CARTESIAN_POINT('',(4.9957946363652,3.22840427022511,-5.5939284900372));
#101823=CARTESIAN_POINT('Origin',(-0.110044981485926,3.08929957773932,0.15654863207421));
#101824=CARTESIAN_POINT('Ctrl Pts',(5.40685761576715,3.13852541968788,-5.19768126651046));
#101825=CARTESIAN_POINT('Ctrl Pts',(5.24013479200018,3.176642188,-5.37111372800878));
#101826=CARTESIAN_POINT('Ctrl Pts',(5.0626399509999,3.214285714,-5.53350492300877));
#101827=CARTESIAN_POINT('Ctrl Pts',(5.02939878672657,3.22133557899626,-5.56391748211061));
#101828=CARTESIAN_POINT('Ctrl Pts',(4.99579464301703,3.22840426981362,-5.59392848408735));
#101829=CARTESIAN_POINT('Ctrl Pts',(6.228762696,3.007773793,-4.177620768));
#101830=CARTESIAN_POINT('Ctrl Pts',(6.000260882,3.07352872,-4.51831315));
#101831=CARTESIAN_POINT('Ctrl Pts',(5.73596393,3.138525418,-4.832051096));
#101832=CARTESIAN_POINT('Ctrl Pts',(5.73333251891506,3.13917254249503,-4.83517475483384));
#101833=CARTESIAN_POINT('Ctrl Pts',(5.73070110783012,3.13981966699007,-4.83829841366768));
#101834=CARTESIAN_POINT('Ctrl Pts',(5.885458487,3.007773793,-4.233660165));
#101835=CARTESIAN_POINT('Ctrl Pts',(5.653891507,3.07352872,-4.555574961));
#101836=CARTESIAN_POINT('Ctrl Pts',(5.388595688,3.138525418,-4.850313032));
#101837=CARTESIAN_POINT('Ctrl Pts',(5.38595433192827,3.13917254249503,-4.8532475230008));
#101838=CARTESIAN_POINT('Ctrl Pts',(5.38331297585654,3.13981966699007,-4.85618201400161));
#101839=CARTESIAN_POINT('',(5.73596392970722,3.13852541850725,-4.83205109335266));
#101840=CARTESIAN_POINT('',(5.56227981475606,3.13852541943002,-4.84118205738657));
#101841=CARTESIAN_POINT('',(6.08546852191175,3.04797057323436,-4.3837282020756));
#101842=CARTESIAN_POINT('Origin',(-0.162149709194065,2.94648212629685,0.0967644123793421));
#101843=CARTESIAN_POINT('Ctrl Pts',(5.88269117573789,3.00855922365084,-4.23750453653349));
#101844=CARTESIAN_POINT('Ctrl Pts',(5.91646159104702,3.01545478684441,-4.26180694017313));
#101845=CARTESIAN_POINT('Ctrl Pts',(5.95026267506045,3.02218156076831,-4.28615783749173));
#101846=CARTESIAN_POINT('Ctrl Pts',(6.01784331581345,3.03530792012776,-4.33489204606716));
#101847=CARTESIAN_POINT('Ctrl Pts',(6.05166139551355,3.04171498174435,-4.35930314069436));
#101848=CARTESIAN_POINT('Ctrl Pts',(6.08546852022469,3.0479705732939,-4.38372819485558));
#101849=CARTESIAN_POINT('Ctrl Pts',(6.40204908504071,3.13983235804358,-3.90689568945038));
#101850=CARTESIAN_POINT('Ctrl Pts',(6.39992260702036,3.13917888802179,-3.91037175022519));
#101851=CARTESIAN_POINT('Ctrl Pts',(6.397796129,3.138525418,-3.913847811));
#101852=CARTESIAN_POINT('Ctrl Pts',(6.18491166100001,3.073105688,-4.261840756));
#101853=CARTESIAN_POINT('Ctrl Pts',(5.93553830800001,3.007781414,-4.584690283));
#101854=CARTESIAN_POINT('Ctrl Pts',(6.30917582457058,3.13983235804358,-3.57167502459223));
#101855=CARTESIAN_POINT('Ctrl Pts',(6.30723153378529,3.13917888802179,-3.57510082329612));
#101856=CARTESIAN_POINT('Ctrl Pts',(6.305287243,3.138525418,-3.578526622));
#101857=CARTESIAN_POINT('Ctrl Pts',(6.110641775,3.073105688,-3.921487766));
#101858=CARTESIAN_POINT('Ctrl Pts',(5.87994559000001,3.007781414,-4.241313459));
#101859=CARTESIAN_POINT('',(6.397796104402,3.13852541976232,-3.91384778973847));
#101860=CARTESIAN_POINT('Origin',(-0.160424606371967,3.08928602904207,0.10739586321264));
#101861=CARTESIAN_POINT('',(6.35154168067892,3.13852541968788,-3.74618722552173));
#101862=CARTESIAN_POINT('Origin',(4.10695782937509E-13,3.22948687199889,
-4.39752401160121E-13));
#101863=CARTESIAN_POINT('',(6.08152500365499,3.22840427021624,-4.38919737818779));
#101864=CARTESIAN_POINT('Origin',(-0.141125708614549,3.08929954404176,0.129232339770062));
#101865=CARTESIAN_POINT('Ctrl Pts',(6.39779611913472,3.13852541968788,-3.91384780447908));
#101866=CARTESIAN_POINT('Ctrl Pts',(6.27225403500211,3.176642188,-4.11906599100872));
#101867=CARTESIAN_POINT('Ctrl Pts',(6.13381823100183,3.214285714,-4.31581671400877));
#101868=CARTESIAN_POINT('Ctrl Pts',(6.10789202802801,3.22133557898932,-4.35266411204301));
#101869=CARTESIAN_POINT('Ctrl Pts',(6.08152500887293,3.2284042698136,-4.38919737096436));
#101870=CARTESIAN_POINT('Ctrl Pts',(6.981202661,3.007773793,-2.740950457));
#101871=CARTESIAN_POINT('Ctrl Pts',(6.831281884,3.07352872,-3.122798776));
#101872=CARTESIAN_POINT('Ctrl Pts',(6.640608432,3.138525418,-3.486017736));
#101873=CARTESIAN_POINT('Ctrl Pts',(6.63871003615623,3.13917254249503,-3.48963404103255));
#101874=CARTESIAN_POINT('Ctrl Pts',(6.63681164031246,3.13981966699007,-3.4932503460651));
#101875=CARTESIAN_POINT('Ctrl Pts',(6.657971528,3.007773793,-2.869479942));
#101876=CARTESIAN_POINT('Ctrl Pts',(6.50102062000001,3.07352872,-3.233648604));
#101877=CARTESIAN_POINT('Ctrl Pts',(6.30528724300001,3.138525418,-3.578526622));
#101878=CARTESIAN_POINT('Ctrl Pts',(6.30333846919071,3.13917254249503,-3.58196031971256));
#101879=CARTESIAN_POINT('Ctrl Pts',(6.30138969538143,3.13981966699007,-3.58539401742512));
#101880=CARTESIAN_POINT('',(6.64060843113851,3.13852541850724,-3.48601773348335));
#101881=CARTESIAN_POINT('',(6.4729478416998,3.13852541943002,-3.5322721713038));
#101882=CARTESIAN_POINT('',(6.88556563105117,3.04797057325362,-2.97304322568093));
#101883=CARTESIAN_POINT('Origin',(-0.179160225268817,2.94648210547569,0.0596447132767219));
#101884=CARTESIAN_POINT('Ctrl Pts',(6.65609534086921,3.00855922359392,-2.87382932423474));
#101885=CARTESIAN_POINT('Ctrl Pts',(6.6943005212506,3.01545478683807,-2.89030390998496));
#101886=CARTESIAN_POINT('Ctrl Pts',(6.73254607753589,3.02218156072765,-2.90681926266647));
#101887=CARTESIAN_POINT('Ctrl Pts',(6.8090231348598,3.03530792013855,-2.93988625227469));
#101888=CARTESIAN_POINT('Ctrl Pts',(6.84729823036446,3.04171498176221,-2.95645674151876));
#101889=CARTESIAN_POINT('Ctrl Pts',(6.88556562787249,3.04797057331347,-2.97304321894631));
#101890=CARTESIAN_POINT('Ctrl Pts',(7.09223982166471,3.13983235804358,-2.43930332935916));
#101891=CARTESIAN_POINT('Ctrl Pts',(7.09091030983235,3.13917888802179,-2.44315525167958));
#101892=CARTESIAN_POINT('Ctrl Pts',(7.089580798,3.138525418,-2.447007174));
#101893=CARTESIAN_POINT('Ctrl Pts',(6.956481647,3.073105688,-2.832628105));
#101894=CARTESIAN_POINT('Ctrl Pts',(6.782341609,3.007781414,-3.201537489));
#101895=CARTESIAN_POINT('Ctrl Pts',(6.92947535176304,3.13983235804358,-2.1318849430597));
#101896=CARTESIAN_POINT('Ctrl Pts',(6.92831296288152,3.13917888802179,-2.13564861352985));
#101897=CARTESIAN_POINT('Ctrl Pts',(6.927150574,3.138525418,-2.139412284));
#101898=CARTESIAN_POINT('Ctrl Pts',(6.81078231800001,3.073105688,-2.516198208));
#101899=CARTESIAN_POINT('Ctrl Pts',(6.654232751,3.007781414,-2.878139415));
#101900=CARTESIAN_POINT('',(7.0895807693367,3.13852541980578,-2.44700715796875));
#101901=CARTESIAN_POINT('Origin',(-0.179760882835231,3.08928603680601,0.0703984541554009));
#101902=CARTESIAN_POINT('',(7.00836568274272,3.13852541968788,-2.29320973895468));
#101903=CARTESIAN_POINT('Origin',(3.20923843055709E-13,3.22948687200022,
5.42101086242752E-15));
#101904=CARTESIAN_POINT('',(6.88289002147178,3.2284042702058,-2.97923227547513));
#101905=CARTESIAN_POINT('Origin',(-0.165607402433887,3.08929956023117,0.0958731051008638));
#101906=CARTESIAN_POINT('Ctrl Pts',(7.08958078696342,3.13852541968788,-2.44700716975202));
#101907=CARTESIAN_POINT('Ctrl Pts',(7.01108965100386,3.176642188,-2.67441530600791));
#101908=CARTESIAN_POINT('Ctrl Pts',(6.9181859880036,3.214285714,-2.89632571200803));
#101909=CARTESIAN_POINT('Ctrl Pts',(6.90078702682232,3.22133557898884,-2.93788500570877));
#101910=CARTESIAN_POINT('Ctrl Pts',(6.88289002496,3.22840426981237,-2.97923226718436));
#101911=CARTESIAN_POINT('Ctrl Pts',(7.407209349,3.007773793,-1.176116349));
#101912=CARTESIAN_POINT('Ctrl Pts',(7.342879738,3.07352872,-1.581265802));
#101913=CARTESIAN_POINT('Ctrl Pts',(7.234745464,3.138525418,-1.97698206));
#101914=CARTESIAN_POINT('Ctrl Pts',(7.23366885027021,3.13917254249503,-1.98092191681603));
#101915=CARTESIAN_POINT('Ctrl Pts',(7.23259223654041,3.13981966699007,-1.98486177363207));
#101916=CARTESIAN_POINT('Ctrl Pts',(7.11916522,3.007773793,-1.371126025));
#101917=CARTESIAN_POINT('Ctrl Pts',(7.044169235,3.07352872,-1.760520432));
#101918=CARTESIAN_POINT('Ctrl Pts',(6.927150574,3.138525418,-2.139412284));
#101919=CARTESIAN_POINT('Ctrl Pts',(6.92598550493897,3.13917254249503,-2.14318463253374));
#101920=CARTESIAN_POINT('Ctrl Pts',(6.92482043587793,3.13981966699007,-2.14695698106747));
#101921=CARTESIAN_POINT('',(7.23474546263686,3.13852541850726,-1.97698205770052));
#101922=CARTESIAN_POINT('',(7.08094802144716,3.13852541943002,-2.05819716358091));
#101923=CARTESIAN_POINT('',(7.36370134438744,3.04797057330458,-1.42334205253659));
#101924=CARTESIAN_POINT('Origin',(-0.187793154152902,2.94648211929427,0.019736057114943));
#101925=CARTESIAN_POINT('Ctrl Pts',(7.11826788532725,3.00855922357092,-1.37577704600417));
#101926=CARTESIAN_POINT('Ctrl Pts',(7.15912139880288,3.01545478681724,-1.38365348071187));
#101927=CARTESIAN_POINT('Ctrl Pts',(7.20002310803504,3.02218156072704,-1.39156104960523));
#101928=CARTESIAN_POINT('Ctrl Pts',(7.28182059976212,3.03530792015462,-1.40741464472073));
#101929=CARTESIAN_POINT('Ctrl Pts',(7.32276301033261,3.04171498179586,-1.41536971100774));
#101930=CARTESIAN_POINT('Ctrl Pts',(7.36370133986324,3.04797057336533,-1.42334204651203));
#101931=CARTESIAN_POINT('Ctrl Pts',(7.45080530628486,3.13983235804358,-0.8576518564782));
#101932=CARTESIAN_POINT('Ctrl Pts',(7.45033492714243,3.13917888802179,-0.8616995287391));
#101933=CARTESIAN_POINT('Ctrl Pts',(7.449864548,3.138525418,-0.865747201));
#101934=CARTESIAN_POINT('Ctrl Pts',(7.402774283,3.073105688,-1.270964912));
#101935=CARTESIAN_POINT('Ctrl Pts',(7.312010155,3.007781414,-1.668684361));
#101936=CARTESIAN_POINT('Ctrl Pts',(7.2257603139574,3.13983235804358,-0.592410290582772));
#101937=CARTESIAN_POINT('Ctrl Pts',(7.2254341789787,3.13917888802179,-0.596335847791386));
#101938=CARTESIAN_POINT('Ctrl Pts',(7.225108044,3.138525418,-0.600261405));
#101939=CARTESIAN_POINT('Ctrl Pts',(7.192458249,3.073105688,-0.99325402));
#101940=CARTESIAN_POINT('Ctrl Pts',(7.11737538400001,3.007781414,-1.380386771));
#101941=CARTESIAN_POINT('',(7.44986451655801,3.13852541980588,-0.865747191503968));
#101942=CARTESIAN_POINT('Origin',(-0.190691700192834,3.0892860583674,0.0301092810209785));
#101943=CARTESIAN_POINT('',(7.33748629495884,3.13852541968788,-0.733004313422165));
#101944=CARTESIAN_POINT('Origin',(-5.10008701937181E-13,3.22948687200011,
7.92551788086904E-14));
#101945=CARTESIAN_POINT('',(7.36241875121879,3.22840427023676,-1.42996158253138));
#101946=CARTESIAN_POINT('Origin',(-0.182345328124276,3.08929952089793,0.0580309238824359));
#101947=CARTESIAN_POINT('Ctrl Pts',(7.4498645363088,3.13852541968788,-0.865747199224515));
#101948=CARTESIAN_POINT('Ctrl Pts',(7.42209450600614,3.176642188,-1.10471193400775));
#101949=CARTESIAN_POINT('Ctrl Pts',(7.37906705800589,3.214285714,-1.34140573900794));
#101950=CARTESIAN_POINT('Ctrl Pts',(7.3710088942515,3.22133557900333,-1.38573366195178));
#101951=CARTESIAN_POINT('Ctrl Pts',(7.36241875294202,3.22840426981265,-1.42996157381253));
#101952=CARTESIAN_POINT('Ctrl Pts',(7.48686316,3.007773793,0.443711652));
#101953=CARTESIAN_POINT('Ctrl Pts',(7.511132695,3.07352872,0.034205403));
#101954=CARTESIAN_POINT('Ctrl Pts',(7.49059384,3.138525418,-0.375504901));
#101955=CARTESIAN_POINT('Ctrl Pts',(7.49038934967081,3.13917254249503,-0.379584086277783));
#101956=CARTESIAN_POINT('Ctrl Pts',(7.49018485934161,3.13981966699007,-0.383663271555565));
#101957=CARTESIAN_POINT('Ctrl Pts',(7.247474658,3.007773793,0.191340221));
#101958=CARTESIAN_POINT('Ctrl Pts',(7.257940325,3.07352872,-0.205072282));
#101959=CARTESIAN_POINT('Ctrl Pts',(7.225108044,3.138525418,-0.600261405));
#101960=CARTESIAN_POINT('Ctrl Pts',(7.22478115703625,3.13917254249503,-0.6041960135191));
#101961=CARTESIAN_POINT('Ctrl Pts',(7.2244542700725,3.13981966699007,-0.6081306220382));
#101962=CARTESIAN_POINT('',(7.35785094258044,3.1385254194309,-0.487883144246335));
#101963=CARTESIAN_POINT('Ctrl Pts',(7.24759813528023,3.00855922363686,0.186605038200589));
#101964=CARTESIAN_POINT('Ctrl Pts',(7.28918971675842,3.01545478684859,0.187695047633154));
#101965=CARTESIAN_POINT('Ctrl Pts',(7.33083506030774,3.02218156075999,0.188765011538209));
#101966=CARTESIAN_POINT('Ctrl Pts',(7.41412822615322,3.03530792015269,0.19086610716728));
#101967=CARTESIAN_POINT('Ctrl Pts',(7.45582352988066,3.04171498178109,0.191898433839794));
#101968=CARTESIAN_POINT('Ctrl Pts',(7.49751856038283,3.0479705733412,0.192913017772022));
#101969=CARTESIAN_POINT('Ctrl Pts',(7.46097941612226,3.13983235804358,0.764102464106214));
#101970=CARTESIAN_POINT('Ctrl Pts',(7.46139016406113,3.13917888802179,0.760048306553106));
#101971=CARTESIAN_POINT('Ctrl Pts',(7.461800912,3.138525418,0.755994149));
#101972=CARTESIAN_POINT('Ctrl Pts',(7.50292141999999,3.073105688,0.350127187));
#101973=CARTESIAN_POINT('Ctrl Pts',(7.499777232,3.007781414,-0.057805406));
#101974=CARTESIAN_POINT('Ctrl Pts',(7.18417675373603,3.13983235804358,0.974764808487867));
#101975=CARTESIAN_POINT('Ctrl Pts',(7.18470212236801,3.13917888802179,0.970860919243934));
#101976=CARTESIAN_POINT('Ctrl Pts',(7.185227491,3.138525418,0.96695703));
#101977=CARTESIAN_POINT('Ctrl Pts',(7.237822825,3.073105688,0.576133623));
#101978=CARTESIAN_POINT('Ctrl Pts',(7.247717455,3.007781414,0.181911224));
#101979=CARTESIAN_POINT('',(7.32351420272364,3.13852541968788,0.86147557909768));
#101980=CARTESIAN_POINT('Ctrl Pts',(7.21643957,3.007773793,2.042792189));
#101981=CARTESIAN_POINT('Ctrl Pts',(7.328173436,3.07352872,1.648077202));
#101982=CARTESIAN_POINT('Ctrl Pts',(7.396190372,3.138525418,1.24353045));
#101983=CARTESIAN_POINT('Ctrl Pts',(7.39686756679169,3.13917254249503,1.23950267442584));
#101984=CARTESIAN_POINT('Ctrl Pts',(7.39754476158338,3.13981966699007,1.23547489885168));
#101985=CARTESIAN_POINT('Ctrl Pts',(7.036900237,3.007773793,1.74485961));
#101986=CARTESIAN_POINT('Ctrl Pts',(7.132338192,3.07352872,1.359964821));
#101987=CARTESIAN_POINT('Ctrl Pts',(7.18522749100001,3.138525418,0.96695703));
#101988=CARTESIAN_POINT('Ctrl Pts',(7.185754070995,3.13917254249503,0.963044139405232));
#101989=CARTESIAN_POINT('Ctrl Pts',(7.18628065099001,3.13981966699007,0.959131248810464));
#101990=CARTESIAN_POINT('',(7.39619036979386,3.13852541850725,1.243530451497));
#101991=CARTESIAN_POINT('',(7.29070893018589,3.13852541943002,1.1052437486685));
#101992=CARTESIAN_POINT('',(7.28076015326005,3.04797057328962,1.80014768114074));
#101993=CARTESIAN_POINT('Origin',(-0.178723583592237,2.94648210035276,-0.0609403866795913));
#101994=CARTESIAN_POINT('Ctrl Pts',(7.03803875139297,3.00855922357189,1.74026167702851));
#101995=CARTESIAN_POINT('Ctrl Pts',(7.07842362489373,3.01545478679328,1.75026716357868));
#101996=CARTESIAN_POINT('Ctrl Pts',(7.11886531302015,3.02218156075358,1.76026463048229));
#101997=CARTESIAN_POINT('Ctrl Pts',(7.19975945737551,3.03530792015482,1.78022217259254));
#101998=CARTESIAN_POINT('Ctrl Pts',(7.24025802834496,3.04171498178902,1.79019362198331));
#101999=CARTESIAN_POINT('Ctrl Pts',(7.28076014663648,3.04797057335003,1.80014768467118));
#102000=CARTESIAN_POINT('Ctrl Pts',(7.12228642016887,3.13983235804358,2.35012820286911));
#102001=CARTESIAN_POINT('Ctrl Pts',(7.12355908908444,3.13917888802179,2.34625712793456));
#102002=CARTESIAN_POINT('Ctrl Pts',(7.124831758,3.138525418,2.342386053));
#102003=CARTESIAN_POINT('Ctrl Pts',(7.252240291,3.073105688,1.954847729));
#102004=CARTESIAN_POINT('Ctrl Pts',(7.336863062,3.007781414,1.555776466));
#102005=CARTESIAN_POINT('Ctrl Pts',(6.80666907381407,3.13983235804358,2.496360987497));
#102006=CARTESIAN_POINT('Ctrl Pts',(6.80802138040703,3.13917888802179,2.4926613077485));
#102007=CARTESIAN_POINT('Ctrl Pts',(6.809373687,3.138525418,2.488961628));
#102008=CARTESIAN_POINT('Ctrl Pts',(6.944754851,3.073105688,2.118581898));
#102009=CARTESIAN_POINT('Ctrl Pts',(7.039164313,3.007781414,1.735703252));
#102010=CARTESIAN_POINT('',(7.12483172548045,3.13852541980596,2.34238604841789));
#102011=CARTESIAN_POINT('Origin',(-0.185709916198784,3.08928601941837,-0.0527429847199418));
#102012=CARTESIAN_POINT('',(6.96710272593122,3.13852541968788,2.41567383060393));
#102013=CARTESIAN_POINT('Origin',(1.19609183668601E-12,3.22948687199989,
2.5652223401007E-13));
#102014=CARTESIAN_POINT('',(7.28237557194861,3.22840427022627,1.79360141154214));
#102015=CARTESIAN_POINT('Origin',(-0.189858677544151,3.08929957468348,-0.0238973877759271));
#102016=CARTESIAN_POINT('Ctrl Pts',(7.12483174664295,3.13852541968788,2.3423860497028));
#102017=CARTESIAN_POINT('Ctrl Pts',(7.19996703800783,3.176642188,2.11384719699605));
#102018=CARTESIAN_POINT('Ctrl Pts',(7.2603015320077,3.214285714,1.8809629609958));
#102019=CARTESIAN_POINT('Ctrl Pts',(7.27160095263314,3.22133557899429,1.83734849258618));
#102020=CARTESIAN_POINT('Ctrl Pts',(7.28237556986395,3.22840426981362,1.79360142017328));
#102021=CARTESIAN_POINT('Ctrl Pts',(6.60858328699999,3.007773793,3.546354034));
#102022=CARTESIAN_POINT('Ctrl Pts',(6.802556932,3.07352872,3.184886742));
#102023=CARTESIAN_POINT('Ctrl Pts',(6.955949263,3.138525418,2.804419699));
#102024=CARTESIAN_POINT('Ctrl Pts',(6.95747647804007,3.13917254249503,2.80063166744372));
#102025=CARTESIAN_POINT('Ctrl Pts',(6.95900369308013,3.13981966699007,2.79684363588743));
#102026=CARTESIAN_POINT('Ctrl Pts',(6.497288181,3.007773793,3.216791304));
#102027=CARTESIAN_POINT('Ctrl Pts',(6.67323585300001,3.07352872,2.86141148));
#102028=CARTESIAN_POINT('Ctrl Pts',(6.809373687,3.138525418,2.488961628));
#102029=CARTESIAN_POINT('Ctrl Pts',(6.81072911165684,3.13917254249503,2.48525341773983));
#102030=CARTESIAN_POINT('Ctrl Pts',(6.81208453631367,3.13981966699007,2.48154520747966));
#102031=CARTESIAN_POINT('',(6.9559492605235,3.13852541850726,2.80441969999317));
#102032=CARTESIAN_POINT('',(6.88266147185314,3.13852541943002,2.64669067168334));
#102033=CARTESIAN_POINT('',(6.7235614876778,3.04797057331005,3.3232094438561));
#102034=CARTESIAN_POINT('Origin',(-0.161444725667562,2.94648211734716,-0.0979359062490287));
#102035=CARTESIAN_POINT('Ctrl Pts',(6.49938849766569,3.00855922363798,3.21254561543738));
#102036=CARTESIAN_POINT('Ctrl Pts',(6.53667831154149,3.01545478684796,3.23099873311303));
#102037=CARTESIAN_POINT('Ctrl Pts',(6.57402533564303,3.02218156079055,3.24945623212677));
#102038=CARTESIAN_POINT('Ctrl Pts',(6.64873793835688,3.0353079201812,3.28633702758897));
#102039=CARTESIAN_POINT('Ctrl Pts',(6.68614610838593,3.04171498180963,3.3047813455693));
#102040=CARTESIAN_POINT('Ctrl Pts',(6.72356148043066,3.04797057337082,3.32320944593047));
#102041=CARTESIAN_POINT('Ctrl Pts',(6.45056322737556,3.13983235804358,3.82626455831516));
#102042=CARTESIAN_POINT('Ctrl Pts',(6.45263830868778,3.13917888802179,3.82275757315758));
#102043=CARTESIAN_POINT('Ctrl Pts',(6.45471339,3.138525418,3.819250588));
#102044=CARTESIAN_POINT('Ctrl Pts',(6.662452467,3.073105688,3.468161763));
#102045=CARTESIAN_POINT('Ctrl Pts',(6.830885329,3.007781414,3.096611959));
#102046=CARTESIAN_POINT('Ctrl Pts',(6.11088911360346,3.13983235804358,3.90123010271037));
#102047=CARTESIAN_POINT('Ctrl Pts',(6.11300512580173,3.13917888802179,3.89790762535519));
#102048=CARTESIAN_POINT('Ctrl Pts',(6.115121138,3.138525418,3.894585148));
#102049=CARTESIAN_POINT('Ctrl Pts',(6.326957859,3.073105688,3.561967638));
#102050=CARTESIAN_POINT('Ctrl Pts',(6.50146767100001,3.007781414,3.208335726));
#102051=CARTESIAN_POINT('',(6.45471335922989,3.13852541980593,3.81925057653514));
#102052=CARTESIAN_POINT('Origin',(-0.170029793294556,3.0892859931606,-0.0914319448838835));
#102053=CARTESIAN_POINT('',(6.28491726947836,3.13852541968788,3.85691785907291));
#102054=CARTESIAN_POINT('Origin',(-3.28730098697605E-13,3.22948687200044,
-1.06902334207071E-13));
#102055=CARTESIAN_POINT('',(6.72654639328731,3.2284042702405,3.31716348977603));
#102056=CARTESIAN_POINT('Origin',(-0.180282775615583,3.08929951594535,-0.0641527183463853));
#102057=CARTESIAN_POINT('Ctrl Pts',(6.45471337961771,3.13852541968788,3.81925058233835));
#102058=CARTESIAN_POINT('Ctrl Pts',(6.57722114700879,3.176642188,3.61220670799775));
#102059=CARTESIAN_POINT('Ctrl Pts',(6.68620828100871,3.214285714,3.39773730899748));
#102060=CARTESIAN_POINT('Ctrl Pts',(6.70661934883691,3.22133557901279,3.35757156380995));
#102061=CARTESIAN_POINT('Ctrl Pts',(6.72654638920165,3.2284042698136,3.31716349782817));
#102062=CARTESIAN_POINT('Ctrl Pts',(5.69171699500001,3.007773793,4.884092306));
#102063=CARTESIAN_POINT('Ctrl Pts',(5.958860426,3.07352872,4.572774518));
#102064=CARTESIAN_POINT('Ctrl Pts',(6.190455698,3.138525418,4.2341774));
#102065=CARTESIAN_POINT('Ctrl Pts',(6.19276152241965,3.13917254249503,4.23080623660635));
#102066=CARTESIAN_POINT('Ctrl Pts',(6.1950673468393,3.13981966699007,4.2274350732127));
#102067=CARTESIAN_POINT('Ctrl Pts',(5.653870151,3.007773793,4.538309411));
#102068=CARTESIAN_POINT('Ctrl Pts',(5.902100421,3.07352872,4.229061719));
#102069=CARTESIAN_POINT('Ctrl Pts',(6.115121138,3.138525418,3.894585148));
#102070=CARTESIAN_POINT('Ctrl Pts',(6.11724202918621,3.13917254249503,3.89125500987346));
#102071=CARTESIAN_POINT('Ctrl Pts',(6.1193629203724,3.13981966699007,3.88792487174692));
#102072=CARTESIAN_POINT('',(6.19045569537371,3.13852541850724,4.23417740041519));
#102073=CARTESIAN_POINT('',(6.15278841316754,3.13852541943002,4.06438128131554));
#102074=CARTESIAN_POINT('',(5.8519765592091,3.04797057325383,4.69088162618691));
#102075=CARTESIAN_POINT('Origin',(-0.136617110471591,2.94648208787109,-0.130352228523811));
#102076=CARTESIAN_POINT('Ctrl Pts',(5.65683406098952,3.0085592236328,4.53461449072007));
#102077=CARTESIAN_POINT('Ctrl Pts',(5.68928518494542,3.01545478683192,4.56065239240518));
#102078=CARTESIAN_POINT('Ctrl Pts',(5.72179123963888,3.02218156074882,4.58670687140468));
#102079=CARTESIAN_POINT('Ctrl Pts',(5.78682882246822,3.03530792013085,4.63878641527706));
#102080=CARTESIAN_POINT('Ctrl Pts',(5.8193974271448,3.04171498175484,4.66484116602169));
#102081=CARTESIAN_POINT('Ctrl Pts',(5.85197655176899,3.04797057331367,4.69088162653268));
#102082=CARTESIAN_POINT('Ctrl Pts',(5.47721886760685,3.13983235804358,5.12348903528974));
#102083=CARTESIAN_POINT('Ctrl Pts',(5.47999933280343,3.13917888802179,5.12051012264487));
#102084=CARTESIAN_POINT('Ctrl Pts',(5.482779798,3.138525418,5.11753121));
#102085=CARTESIAN_POINT('Ctrl Pts',(5.761135769,3.073105688,4.819308408));
#102086=CARTESIAN_POINT('Ctrl Pts',(6.00550299000001,3.007781414,4.492653318));
#102087=CARTESIAN_POINT('Ctrl Pts',(5.12937076913739,3.13983235804358,5.12368203318865));
#102088=CARTESIAN_POINT('Ctrl Pts',(5.1321515445687,3.13917888802179,5.12089211359433));
#102089=CARTESIAN_POINT('Ctrl Pts',(5.13493232,3.138525418,5.118102194));
#102090=CARTESIAN_POINT('Ctrl Pts',(5.413319349,3.073105688,4.838799731));
#102091=CARTESIAN_POINT('Ctrl Pts',(5.659769626,3.007781414,4.530949987));
#102092=CARTESIAN_POINT('',(5.48277977040895,3.1385254198058,5.11753119218416));
#102093=CARTESIAN_POINT('Origin',(-0.146399510967205,3.08928604665587,-0.125845777516614));
#102094=CARTESIAN_POINT('',(5.30885606626935,3.13852541968788,5.1178166944593));
#102095=CARTESIAN_POINT('Origin',(-8.60856524953491E-13,3.22948687200056,
-7.23813370351323E-13));
#102096=CARTESIAN_POINT('',(5.8561913810091,3.2284042702163,4.68561868987122));
#102097=CARTESIAN_POINT('Origin',(-0.162276638324688,3.08929955310546,-0.101408132844909));
#102098=CARTESIAN_POINT('Ctrl Pts',(5.4827797890775,3.13852541968788,5.11753120223883));
#102099=CARTESIAN_POINT('Ctrl Pts',(5.64693170600921,3.176642188,4.94166344799969));
#102100=CARTESIAN_POINT('Ctrl Pts',(5.7994753620092,3.214285714,4.75563723599939));
#102101=CARTESIAN_POINT('Ctrl Pts',(5.82804367834116,3.22133557899689,4.72079831996769));
#102102=CARTESIAN_POINT('Ctrl Pts',(5.85619137527324,3.2284042698127,4.68561869685597));
#102103=CARTESIAN_POINT('Ctrl Pts',(4.508712341,3.007773793,5.99345585));
#102104=CARTESIAN_POINT('Ctrl Pts',(4.83653423,3.07352872,5.74684444));
#102105=CARTESIAN_POINT('Ctrl Pts',(5.135503304,3.138525418,5.465949672));
#102106=CARTESIAN_POINT('Ctrl Pts',(5.13847991999737,3.13917254249504,5.46315300862336));
#102107=CARTESIAN_POINT('Ctrl Pts',(5.14145653599473,3.13981966699007,5.4603563452467));
#102108=CARTESIAN_POINT('Ctrl Pts',(4.546083437,3.007773793,5.647621215));
#102109=CARTESIAN_POINT('Ctrl Pts',(4.854989334,3.07352872,5.398965732));
#102110=CARTESIAN_POINT('Ctrl Pts',(5.13493232,3.138525418,5.118102194));
#102111=CARTESIAN_POINT('Ctrl Pts',(5.1377195071807,3.13917254249504,5.11530584155758));
#102112=CARTESIAN_POINT('Ctrl Pts',(5.14050669436141,3.13981966699007,5.11250948911516));
#102113=CARTESIAN_POINT('',(5.13550330134345,3.13852541850725,5.4659496718453));
#102114=CARTESIAN_POINT('',(5.13521780570783,3.13852541943004,5.29202593910573));
#102115=CARTESIAN_POINT('',(4.70675971130458,3.04797057329693,5.83921339746965));
#102116=CARTESIAN_POINT('Origin',(-0.105401058942916,2.94648212894648,-0.156673128795994));
#102117=CARTESIAN_POINT('Ctrl Pts',(4.54977235062775,3.00855922349068,5.6446498313131));
#102118=CARTESIAN_POINT('Ctrl Pts',(4.57586740607629,3.01545478669787,5.67705501364761));
#102119=CARTESIAN_POINT('Ctrl Pts',(4.60201254479472,3.02218156072021,5.70948819475089));
#102120=CARTESIAN_POINT('Ctrl Pts',(4.65433402260645,3.03530792012531,5.774331305732));
#102121=CARTESIAN_POINT('Ctrl Pts',(4.68054019026196,3.0417149817775,5.80677819834263));
#102122=CARTESIAN_POINT('Ctrl Pts',(4.70675970388043,3.04797057335741,5.83921339628418));
#102123=CARTESIAN_POINT('Ctrl Pts',(4.24776584072616,3.13983235804358,6.18114485999083));
#102124=CARTESIAN_POINT('Ctrl Pts',(4.25112167836308,3.13917888802179,6.17883331049541));
#102125=CARTESIAN_POINT('Ctrl Pts',(4.254477516,3.138525418,6.176521761));
#102126=CARTESIAN_POINT('Ctrl Pts',(4.590434767,3.073105688,5.945109548));
#102127=CARTESIAN_POINT('Ctrl Pts',(4.899310006,3.007781414,5.678623201));
#102128=CARTESIAN_POINT('Ctrl Pts',(3.90800874862701,3.13983235804358,6.10655628662292));
#102129=CARTESIAN_POINT('Ctrl Pts',(3.9113242613135,3.13917888802179,6.10442937831146));
#102130=CARTESIAN_POINT('Ctrl Pts',(3.914639774,3.138525418,6.10230247));
#102131=CARTESIAN_POINT('Ctrl Pts',(4.246560042,3.073105688,5.889374925));
#102132=CARTESIAN_POINT('Ctrl Pts',(4.55342704399999,3.007781414,5.641702062));
#102133=CARTESIAN_POINT('',(4.25447749288633,3.13852541980575,6.17652173767152));
#102134=CARTESIAN_POINT('Origin',(-0.115923519980704,3.08928602198266,-0.154374961645372));
#102135=CARTESIAN_POINT('',(4.08455865372042,3.13852541968788,6.13941210969829));
#102136=CARTESIAN_POINT('Origin',(-8.94683632735038E-13,3.22948687200078,
-9.59302082215174E-13));
#102137=CARTESIAN_POINT('',(4.71200736843668,3.22840427022025,5.8349795680853));
#102138=CARTESIAN_POINT('Origin',(-0.136683026005425,3.08929956840681,-0.133922036616551));
#102139=CARTESIAN_POINT('Ctrl Pts',(4.25447750895388,3.13852541968788,6.17652175150207));
#102140=CARTESIAN_POINT('Ctrl Pts',(4.45259801400849,3.176642188,6.04005349700157));
#102141=CARTESIAN_POINT('Ctrl Pts',(4.64156542100854,3.214285714,5.8911688520013));
#102142=CARTESIAN_POINT('Ctrl Pts',(4.6769551631131,3.2213355789938,5.86328579409405));
#102143=CARTESIAN_POINT('Ctrl Pts',(4.7120073614679,3.22840426981363,5.83497957368301));
#102144=CARTESIAN_POINT('Ctrl Pts',(3.11488531,3.007773793,6.82257206));
#102145=CARTESIAN_POINT('Ctrl Pts',(3.488057068,3.07352872,6.652198303));
#102146=CARTESIAN_POINT('Ctrl Pts',(3.840420483,3.138525418,6.442140212));
#102147=CARTESIAN_POINT('Ctrl Pts',(3.84392870732549,3.13917254249503,6.44004881750999));
#102148=CARTESIAN_POINT('Ctrl Pts',(3.84743693165098,3.13981966699007,6.43795742301998));
#102149=CARTESIAN_POINT('Ctrl Pts',(3.225726914,3.007773793,6.492856527));
#102150=CARTESIAN_POINT('Ctrl Pts',(3.580864341,3.07352872,6.316420107));
#102151=CARTESIAN_POINT('Ctrl Pts',(3.914639774,3.138525418,6.10230247));
#102152=CARTESIAN_POINT('Ctrl Pts',(3.91796293140924,3.13917254249503,6.10017065758514));
#102153=CARTESIAN_POINT('Ctrl Pts',(3.92128608881848,3.13981966699007,6.09803884517028));
#102154=CARTESIAN_POINT('',(3.84042048042683,3.13852541850725,6.44214021129259));
#102155=CARTESIAN_POINT('',(3.87753012104247,3.13852541943002,6.2722213456103));
#102156=CARTESIAN_POINT('',(3.34146001010757,3.04797057324922,6.7145100401353));
#102157=CARTESIAN_POINT('Origin',(-0.0692568059026771,2.94648211319721,
-0.175668415170304));
#102158=CARTESIAN_POINT('Ctrl Pts',(3.22996834292612,3.00855922362653,6.49074762063523));
#102159=CARTESIAN_POINT('Ctrl Pts',(3.24848715409963,3.01545478681904,6.52800485343035));
#102160=CARTESIAN_POINT('Ctrl Pts',(3.26704885853801,3.02218156076036,6.56530019640403));
#102161=CARTESIAN_POINT('Ctrl Pts',(3.30420773701181,3.03530792012851,6.63987488250295));
#102162=CARTESIAN_POINT('Ctrl Pts',(3.3228260961376,3.04171498175259,6.677196736047));
#102163=CARTESIAN_POINT('Ctrl Pts',(3.34146000322131,3.04797057330893,6.71451003732055));
#102164=CARTESIAN_POINT('Ctrl Pts',(2.81969200434841,3.13983235804358,6.94977722071898));
#102165=CARTESIAN_POINT('Ctrl Pts',(2.82346629917421,3.13917888802179,6.94824111985949));
#102166=CARTESIAN_POINT('Ctrl Pts',(2.827240594,3.138525418,6.946705019));
#102167=CARTESIAN_POINT('Ctrl Pts',(3.205090136,3.073105688,6.79292397300001));
#102168=CARTESIAN_POINT('Ctrl Pts',(3.564030731,3.007781414,6.599066975));
#102169=CARTESIAN_POINT('Ctrl Pts',(2.50391258247664,3.13983235804358,6.80389475530675));
#102170=CARTESIAN_POINT('Ctrl Pts',(2.50760780273832,3.13917888802179,6.80253031015338));
#102171=CARTESIAN_POINT('Ctrl Pts',(2.511303023,3.138525418,6.801165865));
#102172=CARTESIAN_POINT('Ctrl Pts',(2.881236308,3.073105688,6.664569494));
#102173=CARTESIAN_POINT('Ctrl Pts',(3.234171275,3.007781414,6.48865441900001));
#102174=CARTESIAN_POINT('',(2.82724057644168,3.13852541980569,6.94670499124702));
#102175=CARTESIAN_POINT('Origin',(-0.0800272701647023,3.08928603326539,
-0.17568595985035));
#102176=CARTESIAN_POINT('',(2.66927181826374,3.13852541968788,6.87393543820857));
#102177=CARTESIAN_POINT('Origin',(-3.16587034365767E-14,3.22948687199933,
1.64798730217797E-13));
#102178=CARTESIAN_POINT('',(3.34749512821828,3.22840427023067,6.71150328635333));
#102179=CARTESIAN_POINT('Origin',(-0.104698240449298,3.0892995303119,-0.16017393657233));
#102180=CARTESIAN_POINT('Ctrl Pts',(2.82724058916065,3.13852541968788,6.94670500820955));
#102181=CARTESIAN_POINT('Ctrl Pts',(3.05006578700813,3.176642188,6.85601735800344));
#102182=CARTESIAN_POINT('Ctrl Pts',(3.26662104000823,3.214285714,6.75123596000317));
#102183=CARTESIAN_POINT('Ctrl Pts',(3.30717742265074,3.221335578992,6.73161254089966));
#102184=CARTESIAN_POINT('Ctrl Pts',(3.34749512040879,3.2284042698127,6.71150329039929));
#102185=CARTESIAN_POINT('Ctrl Pts',(1.575409703,3.007773793,7.332672382));
#102186=CARTESIAN_POINT('Ctrl Pts',(1.976482234,3.07352872,7.246502767));
#102187=CARTESIAN_POINT('Ctrl Pts',(2.365763869,3.138525418,7.117103436));
#102188=CARTESIAN_POINT('Ctrl Pts',(2.36963966098986,3.13917254249503,7.11581510167983));
#102189=CARTESIAN_POINT('Ctrl Pts',(2.37351545297971,3.13981966699007,7.11452676735966));
#102190=CARTESIAN_POINT('Ctrl Pts',(1.754538986,3.007773793,7.034493084));
#102191=CARTESIAN_POINT('Ctrl Pts',(2.139302112,3.07352872,6.938525699));
#102192=CARTESIAN_POINT('Ctrl Pts',(2.511303023,3.138525418,6.801165865));
#102193=CARTESIAN_POINT('Ctrl Pts',(2.5150067634836,3.13917254249503,6.7997982737846));
#102194=CARTESIAN_POINT('Ctrl Pts',(2.5187105039672,3.13981966699007,6.79843068256919));
#102195=CARTESIAN_POINT('',(2.36576386665506,3.13852541850724,7.11710343474332));
#102196=CARTESIAN_POINT('',(2.43853343772574,3.13852541943002,6.95913465339936));
#102197=CARTESIAN_POINT('',(1.81991735276004,3.04797057334258,7.27584365642433));
#102198=CARTESIAN_POINT('Origin',(-0.0298740646503137,2.94648209465332,
-0.186449427984996));
#102199=CARTESIAN_POINT('Ctrl Pts',(1.75913460499466,3.00855922359267,7.03334526460901));
#102200=CARTESIAN_POINT('Ctrl Pts',(1.76921125282428,3.01545478682352,7.07371244114721));
#102201=CARTESIAN_POINT('Ctrl Pts',(1.77932159850542,3.02218156078112,7.11412605755525));
#102202=CARTESIAN_POINT('Ctrl Pts',(1.79958036974931,3.03530792019689,7.19494528964447));
#102203=CARTESIAN_POINT('Ctrl Pts',(1.80974034659752,3.04171498183564,7.23539697594034));
#102204=CARTESIAN_POINT('Ctrl Pts',(1.81991734640429,3.04797057340381,7.27584365226265));
#102205=CARTESIAN_POINT('Ctrl Pts',(1.25977250362045,3.13983235804358,7.39344572270518));
#102206=CARTESIAN_POINT('Ctrl Pts',(1.26378877381022,3.13917888802179,7.39275689685259));
#102207=CARTESIAN_POINT('Ctrl Pts',(1.267805044,3.138525418,7.392068071));
#102208=CARTESIAN_POINT('Ctrl Pts',(1.669879053,3.073105688,7.323108823));
#102209=CARTESIAN_POINT('Ctrl Pts',(2.062101341,3.007781414,7.210945712));
#102210=CARTESIAN_POINT('Ctrl Pts',(0.982736247106169,3.13983235804358,
7.18309066712261));
#102211=CARTESIAN_POINT('Ctrl Pts',(0.986638390553085,3.13917888802179,
7.18255248506131));
#102212=CARTESIAN_POINT('Ctrl Pts',(0.990540534,3.138525418,7.182014303));
#102213=CARTESIAN_POINT('Ctrl Pts',(1.381189167,3.073105688,7.1281362));
#102214=CARTESIAN_POINT('Ctrl Pts',(1.763689251,3.007781414,7.032204507));
#102215=CARTESIAN_POINT('',(1.26780503335226,3.13852541976232,7.39206804027773));
#102216=CARTESIAN_POINT('Origin',(-0.0403889916659433,3.08928603899375,
-0.188782065731093));
#102217=CARTESIAN_POINT('',(1.12917279935051,3.13852541968788,7.28704118539612));
#102218=CARTESIAN_POINT('Origin',(-9.63855731339613E-14,3.229486871999,
-4.21537804662364E-13));
#102219=CARTESIAN_POINT('',(1.82645773643408,3.22840427022337,7.27420457056872));
#102220=CARTESIAN_POINT('Origin',(-0.067817762799324,3.08929952515512,-0.178936091177111));
#102221=CARTESIAN_POINT('Ctrl Pts',(1.26780504159327,3.13852541968788,7.39206805942139));
#102222=CARTESIAN_POINT('Ctrl Pts',(1.50491587500718,3.176642188,7.35140146700508));
#102223=CARTESIAN_POINT('Ctrl Pts',(1.73893308900733,3.214285714,7.29562277800485));
#102224=CARTESIAN_POINT('Ctrl Pts',(1.78275974095652,3.2213355789919,7.28517656685318));
#102225=CARTESIAN_POINT('Ctrl Pts',(1.8264577278493,3.22840426981285,7.27420457278075));
#102226=CARTESIAN_POINT('Ctrl Pts',(-0.03773031,3.007773793,7.499905094));
#102227=CARTESIAN_POINT('Ctrl Pts',(0.372489288,3.07352872,7.501968815));
#102228=CARTESIAN_POINT('Ctrl Pts',(0.780486765999999,3.138525418,7.459278813));
#102229=CARTESIAN_POINT('Ctrl Pts',(0.784548897924391,3.13917254249503,
7.4588537799316));
#102230=CARTESIAN_POINT('Ctrl Pts',(0.788611029848782,3.13981966699007,
7.45842874686319));
#102231=CARTESIAN_POINT('Ctrl Pts',(0.201310764,3.007773793,7.247204563));
#102232=CARTESIAN_POINT('Ctrl Pts',(0.597708493,3.07352872,7.236193541));
#102233=CARTESIAN_POINT('Ctrl Pts',(0.990540534000001,3.138525418,7.182014303));
#102234=CARTESIAN_POINT('Ctrl Pts',(0.994451674780801,3.13917254249503,
7.18147488002758));
#102235=CARTESIAN_POINT('Ctrl Pts',(0.998362815561602,3.13981966699007,
7.18093545705518));
#102236=CARTESIAN_POINT('',(0.78048676397796,3.13852541850725,7.45927881126957));
#102237=CARTESIAN_POINT('',(0.885513641295908,3.13852541943002,7.32064655905286));
#102238=CARTESIAN_POINT('',(0.213277382521218,3.04797057327008,7.49696690910154));
#102239=CARTESIAN_POINT('Origin',(0.0109054915341743,2.94648208325206,-0.188512453073895));
#102240=CARTESIAN_POINT('Ctrl Pts',(0.206045687659719,3.00855922379005,
7.24707150198745));
#102241=CARTESIAN_POINT('Ctrl Pts',(0.207208999418826,3.0154547870171,7.28866109792215));
#102242=CARTESIAN_POINT('Ctrl Pts',(0.208395237953114,3.02218156082844,
7.33030329111373));
#102243=CARTESIAN_POINT('Ctrl Pts',(0.210806624555049,3.03530792020359,
7.41358805137751));
#102244=CARTESIAN_POINT('Ctrl Pts',(0.212033149998714,3.04171498179988,
7.45527809421898));
#102245=CARTESIAN_POINT('Ctrl Pts',(0.213277377398708,3.04797057333011,
7.49696690365892));
#102246=CARTESIAN_POINT('Ctrl Pts',(-0.359052559442651,3.13983235804358,
7.49140492024465));
#102247=CARTESIAN_POINT('Ctrl Pts',(-0.354982110221325,3.13917888802179,
7.49159557812232));
#102248=CARTESIAN_POINT('Ctrl Pts',(-0.350911661,3.138525418,7.491786236));
#102249=CARTESIAN_POINT('Ctrl Pts',(0.056586281,3.073105688,7.510873243));
#102250=CARTESIAN_POINT('Ctrl Pts',(0.463750383,3.007781414,7.485648641));
#102251=CARTESIAN_POINT('Ctrl Pts',(-0.584391742461101,3.13983235804358,
7.22641324335268));
#102252=CARTESIAN_POINT('Ctrl Pts',(-0.58046513573055,3.13917888802179,
7.22672648917634));
#102253=CARTESIAN_POINT('Ctrl Pts',(-0.576538529,3.138525418,7.227039735));
#102254=CARTESIAN_POINT('Ctrl Pts',(-0.183440845,3.073105688,7.25839918));
#102255=CARTESIAN_POINT('Ctrl Pts',(0.210739078,3.007781414,7.246936528));
#102256=CARTESIAN_POINT('',(-0.350911665282579,3.13852541980569,7.49178620343906));
#102257=CARTESIAN_POINT('Origin',(0.00113783564030897,3.08928603443716,
-0.193050966742221));
#102258=CARTESIAN_POINT('',(-0.46372508454669,3.13852541968788,7.35941298615868));
#102259=CARTESIAN_POINT('Origin',(-2.81079413216867E-14,3.22948687199989,
-7.26415455565288E-13));
#102260=CARTESIAN_POINT('',(0.220017210746863,3.22840427020573,7.49677213367687));
#102261=CARTESIAN_POINT('Origin',(-0.0277662652739613,3.08929952349658,
-0.189331667288006));
#102262=CARTESIAN_POINT('Ctrl Pts',(-0.350911660861536,3.13852541968788,
7.49178622417456));
#102263=CARTESIAN_POINT('Ctrl Pts',(-0.110602231994232,3.176642188,7.50304221400634));
#102264=CARTESIAN_POINT('Ctrl Pts',(0.129934559005965,3.214285714,7.49887438300615));
#102265=CARTESIAN_POINT('Ctrl Pts',(0.17498219508154,3.22133557898442,7.4980938331641));
#102266=CARTESIAN_POINT('Ctrl Pts',(0.220017201815362,3.22840426981251,
7.49677213391338));
#102267=CARTESIAN_POINT('Ctrl Pts',(0.467202875,2.75,7.485433954));
#102268=CARTESIAN_POINT('Ctrl Pts',(0.872823804,2.68564607,7.46011715000001));
#102269=CARTESIAN_POINT('Ctrl Pts',(1.27333392,2.620518779,7.391117691));
#102270=CARTESIAN_POINT('Ctrl Pts',(0.214081497,2.75,7.24683856));
#102271=CARTESIAN_POINT('Ctrl Pts',(0.606773411,2.68564607,7.235237905));
#102272=CARTESIAN_POINT('Ctrl Pts',(0.995912368,2.620518779,7.181271375));
#102273=CARTESIAN_POINT('',(0.991263371367775,2.62129679675086,7.18191455012789));
#102274=CARTESIAN_POINT('Origin',(-0.0379383924044535,2.55361184896654,
-0.192401840764767));
#102275=CARTESIAN_POINT('Ctrl Pts',(1.02739270989941,2.66036061572379,7.42929769313666));
#102276=CARTESIAN_POINT('Ctrl Pts',(1.02133053819476,2.65417293169584,7.38803131424235));
#102277=CARTESIAN_POINT('Ctrl Pts',(1.01528456429805,2.64782918802562,7.34676106946382));
#102278=CARTESIAN_POINT('Ctrl Pts',(1.00324257965832,2.63481932854071,7.2643143704311));
#102279=CARTESIAN_POINT('Ctrl Pts',(0.997239354252857,2.62814542762809,
7.22308853316094));
#102280=CARTESIAN_POINT('Ctrl Pts',(0.991263375807131,2.62129679727074,
7.18191457244044));
#102281=CARTESIAN_POINT('Ctrl Pts',(0.77634725,2.620519775,7.459710782));
#102282=CARTESIAN_POINT('Ctrl Pts',(0.959930074,2.64969025,7.440604944));
#102283=CARTESIAN_POINT('Ctrl Pts',(1.142350843,2.678571429,7.412491791));
#102284=CARTESIAN_POINT('Ctrl Pts',(1.366589369,2.714073269,7.377934037));
#102285=CARTESIAN_POINT('Ctrl Pts',(1.588328914,2.75,7.329884805));
#102286=CARTESIAN_POINT('Ctrl Pts',(1.59236135128825,2.75065334439885,7.32901100725324));
#102287=CARTESIAN_POINT('Ctrl Pts',(1.5963937885765,2.7513066887977,7.32813720950648));
#102288=CARTESIAN_POINT('Ctrl Pts',(0.986554849,2.620519775,7.18256288));
#102289=CARTESIAN_POINT('Ctrl Pts',(1.163317088,2.64969025,7.158283853));
#102290=CARTESIAN_POINT('Ctrl Pts',(1.338671059,2.678571429,7.125339276));
#102291=CARTESIAN_POINT('Ctrl Pts',(1.554222808,2.714073269,7.08484255300001));
#102292=CARTESIAN_POINT('Ctrl Pts',(1.766932466,2.75,7.031390308));
#102293=CARTESIAN_POINT('Ctrl Pts',(1.77080069057172,2.75065334439885,7.03041825393595));
#102294=CARTESIAN_POINT('Ctrl Pts',(1.77466891514343,2.7513066887977,7.02944619987189));
#102295=CARTESIAN_POINT('Ctrl Pts',(1.76693247047358,2.75000000176745,7.03139031538271));
#102296=CARTESIAN_POINT('Ctrl Pts',(1.62477277725516,2.72598918233424,7.06711390973909));
#102297=CARTESIAN_POINT('Ctrl Pts',(1.48188408168206,2.70215892406901,7.09843317048902));
#102298=CARTESIAN_POINT('Ctrl Pts',(1.33867105724405,2.67857142871079,7.1253392763299));
#102299=CARTESIAN_POINT('Ctrl Pts',(1.22364114774488,2.65962575335661,7.1469504875505));
#102300=CARTESIAN_POINT('Ctrl Pts',(1.10777325899891,2.6405235296523,7.16583362630432));
#102301=CARTESIAN_POINT('Ctrl Pts',(0.991263374345238,2.62129679692748,
7.18191457191139));
#102302=CARTESIAN_POINT('Ctrl Pts',(2.065426964,2.75,7.20999386));
#102303=CARTESIAN_POINT('Ctrl Pts',(2.456122336,2.68564607,7.098072439));
#102304=CARTESIAN_POINT('Ctrl Pts',(2.832435904,2.620518779,6.944588314));
#102305=CARTESIAN_POINT('Ctrl Pts',(1.766932466,2.75,7.031390308));
#102306=CARTESIAN_POINT('Ctrl Pts',(2.147949663,2.68564607,6.935643716));
#102307=CARTESIAN_POINT('Ctrl Pts',(2.516389559,2.620518779,6.79928552));
#102308=CARTESIAN_POINT('',(2.51198751719057,2.62129679673515,6.80091305603547));
#102309=CARTESIAN_POINT('Origin',(-0.078412607116547,2.55361160406602,-0.179749174256227));
#102310=CARTESIAN_POINT('Ctrl Pts',(2.60045223490387,2.66036061567143,7.03474577850128));
#102311=CARTESIAN_POINT('Ctrl Pts',(2.58566074166918,2.65417293165183,6.99574737228981));
#102312=CARTESIAN_POINT('Ctrl Pts',(2.57088423644442,2.64782918797765,6.95674170839051));
#102313=CARTESIAN_POINT('Ctrl Pts',(2.54140015100389,2.63481931413965,6.87881115181285));
#102314=CARTESIAN_POINT('Ctrl Pts',(2.52667495880192,2.62814542051295,6.83983971336488));
#102315=CARTESIAN_POINT('Ctrl Pts',(2.51198752653413,2.62129679718683,6.80091307555531));
#102316=CARTESIAN_POINT('Ctrl Pts',(2.361813993,2.620519775,7.118415179));
#102317=CARTESIAN_POINT('Ctrl Pts',(2.536997563,2.64969025,7.060291145));
#102318=CARTESIAN_POINT('Ctrl Pts',(2.709109939,2.678571429,6.993620188));
#102319=CARTESIAN_POINT('Ctrl Pts',(2.920676996,2.714073269,6.911665721));
#102320=CARTESIAN_POINT('Ctrl Pts',(3.12690323,2.75,6.817072406));
#102321=CARTESIAN_POINT('Ctrl Pts',(3.1306535504753,2.75065334439885,6.8153521823447));
#102322=CARTESIAN_POINT('Ctrl Pts',(3.13440387095059,2.7513066887977,6.8136319586894));
#102323=CARTESIAN_POINT('Ctrl Pts',(2.507528449,2.620519775,6.802558422));
#102324=CARTESIAN_POINT('Ctrl Pts',(2.674938811,2.64969025,6.740848368));
#102325=CARTESIAN_POINT('Ctrl Pts',(2.839110994,2.678571429,6.670978097));
#102326=CARTESIAN_POINT('Ctrl Pts',(3.040917665,2.714073269,6.58509091));
#102327=CARTESIAN_POINT('Ctrl Pts',(3.237163637,2.75,6.48716206));
#102328=CARTESIAN_POINT('Ctrl Pts',(3.24073246174509,2.75065334439885,6.48538117808137));
#102329=CARTESIAN_POINT('Ctrl Pts',(3.24430128649018,2.7513066887977,6.48360029616274));
#102330=CARTESIAN_POINT('Ctrl Pts',(3.23716364320858,2.75000000185344,6.48716206666387));
#102331=CARTESIAN_POINT('Ctrl Pts',(3.10600708091653,2.72598918232688,6.55261059477203));
#102332=CARTESIAN_POINT('Ctrl Pts',(2.97319175854747,2.70215892403026,6.61391447450941));
#102333=CARTESIAN_POINT('Ctrl Pts',(2.83911099237912,2.67857142871485,6.67097809768983));
#102334=CARTESIAN_POINT('Ctrl Pts',(2.73141618969899,2.65962575340867,6.71681208068242));
#102335=CARTESIAN_POINT('Ctrl Pts',(2.62231654513112,2.64052352980419,6.76016191311457));
#102336=CARTESIAN_POINT('Ctrl Pts',(2.51198752491407,2.62129679699288,6.80091307706755));
#102337=CARTESIAN_POINT('Ctrl Pts',(3.567073983,2.75,6.597422466));
#102338=CARTESIAN_POINT('Ctrl Pts',(3.924575317,2.68564607,6.40412975));
#102339=CARTESIAN_POINT('Ctrl Pts',(4.259096333,2.620518779,6.17333770500001));
#102340=CARTESIAN_POINT('Ctrl Pts',(3.237163637,2.75,6.48716206));
#102341=CARTESIAN_POINT('Ctrl Pts',(3.588690177,2.68564607,6.311746536));
#102342=CARTESIAN_POINT('Ctrl Pts',(3.919203171,2.620518779,6.099372632));
#102343=CARTESIAN_POINT('',(3.91525391814552,2.62129679671748,6.10190842548336));
#102344=CARTESIAN_POINT('Origin',(-0.115220002471641,2.55361156385018,-0.158690101272749));
#102345=CARTESIAN_POINT('Ctrl Pts',(4.05191750338997,2.6603606157075,6.31125696986323));
#102346=CARTESIAN_POINT('Ctrl Pts',(4.02908832265019,2.6541729316882,6.27635005861745));
#102347=CARTESIAN_POINT('Ctrl Pts',(4.0062722191201,2.64782918796055,6.24143283708704));
#102348=CARTESIAN_POINT('Ctrl Pts',(3.96072473936658,2.63481932842818,6.17166253728937));
#102349=CARTESIAN_POINT('Ctrl Pts',(3.93796607992139,2.62814542752971,6.13676766959823));
#102350=CARTESIAN_POINT('Ctrl Pts',(3.9152539318273,2.62129679721806,6.10190844318046));
#102351=CARTESIAN_POINT('Ctrl Pts',(3.836844939,2.620519775,6.444270394));
#102352=CARTESIAN_POINT('Ctrl Pts',(3.995437865,2.64969025,6.349845979));
#102353=CARTESIAN_POINT('Ctrl Pts',(4.149194064,2.678571429,6.247734679));
#102354=CARTESIAN_POINT('Ctrl Pts',(4.338197014,2.714073269,6.122215598));
#102355=CARTESIAN_POINT('Ctrl Pts',(4.519267026,2.75,5.98550127800001));
#102356=CARTESIAN_POINT('Ctrl Pts',(4.52255986881779,2.75065334439885,5.98301506417736));
#102357=CARTESIAN_POINT('Ctrl Pts',(4.52585271163557,2.7513066887977,5.98052885035472));
#102358=CARTESIAN_POINT('Ctrl Pts',(3.911252806,2.620519775,6.104473891));
#102359=CARTESIAN_POINT('Ctrl Pts',(4.06148337,2.64969025,6.008218305));
#102360=CARTESIAN_POINT('Ctrl Pts',(4.206797255,2.678571429,5.904689396));
#102361=CARTESIAN_POINT('Ctrl Pts',(4.385422592,2.714073269,5.777427735));
#102362=CARTESIAN_POINT('Ctrl Pts',(4.556028634,2.75,5.63960132400001));
#102363=CARTESIAN_POINT('Ctrl Pts',(4.55913118463147,2.75065334439885,5.63709488628262));
#102364=CARTESIAN_POINT('Ctrl Pts',(4.56223373526293,2.7513066887977,5.63458844856525));
#102365=CARTESIAN_POINT('Ctrl Pts',(4.55602864119576,2.75000000176928,5.63960132856059));
#102366=CARTESIAN_POINT('Ctrl Pts',(4.44200794567386,2.72598918228978,5.73171449093605));
#102367=CARTESIAN_POINT('Ctrl Pts',(4.32547629386789,2.70215892402793,5.82013648845238));
#102368=CARTESIAN_POINT('Ctrl Pts',(4.20679725367195,2.67857142873605,5.90468939694617));
#102369=CARTESIAN_POINT('Ctrl Pts',(4.11147324763285,2.65962575344072,5.97260300576642));
#102370=CARTESIAN_POINT('Ctrl Pts',(4.01424322389773,2.64052352968139,6.03839254209647));
#102371=CARTESIAN_POINT('Ctrl Pts',(3.91525393011497,2.62129679688094,6.10190844418719));
#102372=CARTESIAN_POINT('Ctrl Pts',(4.901928588,2.75,5.676362931));
#102373=CARTESIAN_POINT('Ctrl Pts',(5.209519519,2.68564607,5.41073707200001));
#102374=CARTESIAN_POINT('Ctrl Pts',(5.486606152,2.620518779,5.113428687));
#102375=CARTESIAN_POINT('Ctrl Pts',(4.556028634,2.75,5.63960132400001));
#102376=CARTESIAN_POINT('Ctrl Pts',(4.861627526,2.68564607,5.392719102));
#102377=CARTESIAN_POINT('Ctrl Pts',(5.138759199,2.620518779,5.114259858));
#102378=CARTESIAN_POINT('',(5.13544739786056,2.62129679675748,5.11758533942526));
#102379=CARTESIAN_POINT('Origin',(-0.146640035537037,2.55361159747453,-0.130211287635851));
#102380=CARTESIAN_POINT('Ctrl Pts',(5.31391961274854,2.66036061567578,5.29266079998403));
#102381=CARTESIAN_POINT('Ctrl Pts',(5.28412021133306,2.65417293165882,5.26347759186377));
#102382=CARTESIAN_POINT('Ctrl Pts',(5.25433136546702,2.64782918802237,5.23428150368819));
#102383=CARTESIAN_POINT('Ctrl Pts',(5.19485020828765,2.63481932849264,5.17593375624));
#102384=CARTESIAN_POINT('Ctrl Pts',(5.16512226866306,2.62814542762031,5.14674715016722));
#102385=CARTESIAN_POINT('Ctrl Pts',(5.13544741478222,2.62129679733524,5.11758535350893));
#102386=CARTESIAN_POINT('Ctrl Pts',(5.13246928,2.620519775,5.468798688));
#102387=CARTESIAN_POINT('Ctrl Pts',(5.267055933,2.64969025,5.342489072));
#102388=CARTESIAN_POINT('Ctrl Pts',(5.395266487,2.678571429,5.209712039));
#102389=CARTESIAN_POINT('Ctrl Pts',(5.552867761,2.714073269,5.046497477));
#102390=CARTESIAN_POINT('Ctrl Pts',(5.700314919,2.75,4.874054762));
#102391=CARTESIAN_POINT('Ctrl Pts',(5.70299631449924,2.75065334439885,4.87091881061139));
#102392=CARTESIAN_POINT('Ctrl Pts',(5.70567770999848,2.7513066887977,4.86778285922278));
#102393=CARTESIAN_POINT('Ctrl Pts',(5.132091328,2.620519775,5.120950947));
#102394=CARTESIAN_POINT('Ctrl Pts',(5.258117479,2.64969025,4.994650632));
#102395=CARTESIAN_POINT('Ctrl Pts',(5.377778351,2.678571429,4.862303981));
#102396=CARTESIAN_POINT('Ctrl Pts',(5.524870032,2.714073269,4.69961846));
#102397=CARTESIAN_POINT('Ctrl Pts',(5.661858795,2.75,4.528339098));
#102398=CARTESIAN_POINT('Ctrl Pts',(5.6643499996969,2.75065334439885,4.52522430272956));
#102399=CARTESIAN_POINT('Ctrl Pts',(5.6668412043938,2.7513066887977,4.52210950745911));
#102400=CARTESIAN_POINT('Ctrl Pts',(5.66185880358697,2.75000000189433,4.52833910123001));
#102401=CARTESIAN_POINT('Ctrl Pts',(5.57030545547846,2.72598918234126,4.64280978801909));
#102402=CARTESIAN_POINT('Ctrl Pts',(5.47550636442511,2.70215892403391,4.75421538847654));
#102403=CARTESIAN_POINT('Ctrl Pts',(5.37777835008841,2.67857142877804,4.86230398217638));
#102404=CARTESIAN_POINT('Ctrl Pts',(5.29928238471252,2.65962575348233,4.94912165257316));
#102405=CARTESIAN_POINT('Ctrl Pts',(5.21846835055042,2.64052352972735,5.03427464719514));
#102406=CARTESIAN_POINT('Ctrl Pts',(5.13544741336457,2.62129679700693,5.11758535493291));
#102407=CARTESIAN_POINT('Ctrl Pts',(6.007574459,2.75,4.489882974));
#102408=CARTESIAN_POINT('Ctrl Pts',(6.250872378,2.68564607,4.164344342));
#102409=CARTESIAN_POINT('Ctrl Pts',(6.457568365,2.620518779,3.814421426));
#102410=CARTESIAN_POINT('Ctrl Pts',(5.661858795,2.75,4.528339098));
#102411=CARTESIAN_POINT('Ctrl Pts',(5.907240575,2.68564607,4.221534117));
#102412=CARTESIAN_POINT('Ctrl Pts',(6.118032557,2.620518779,3.890009978));
#102413=CARTESIAN_POINT('',(6.11551306419439,2.62129679673686,3.89396965038792));
#102414=CARTESIAN_POINT('Origin',(-0.171203284020705,2.55361160305888,-0.0956437659882275));
#102415=CARTESIAN_POINT('Ctrl Pts',(6.32744874717913,2.66036061564244,4.02658569320165));
#102416=CARTESIAN_POINT('Ctrl Pts',(6.29207251207898,2.65417293160338,4.00449076262624));
#102417=CARTESIAN_POINT('Ctrl Pts',(6.25670381706409,2.64782918797476,3.98238098412373));
#102418=CARTESIAN_POINT('Ctrl Pts',(6.18607025531124,2.63481932843167,3.93818406519795));
#102419=CARTESIAN_POINT('Ctrl Pts',(6.15076308075667,2.62814542754816,3.91607045407821));
#102420=CARTESIAN_POINT('Ctrl Pts',(6.11551308399253,2.6212967972428,3.89396966050844));
#102421=CARTESIAN_POINT('Ctrl Pts',(6.188105062,2.620519775,4.237612033));
#102422=CARTESIAN_POINT('Ctrl Pts',(6.29239232,2.64969025,4.085323313));
#102423=CARTESIAN_POINT('Ctrl Pts',(6.389062245,2.678571429,3.928089055));
#102424=CARTESIAN_POINT('Ctrl Pts',(6.50789258200001,2.714073269,3.734810744));
#102425=CARTESIAN_POINT('Ctrl Pts',(6.614822422,2.75,3.534702862));
#102426=CARTESIAN_POINT('Ctrl Pts',(6.61676699112971,2.75065334439885,3.53106380661613));
#102427=CARTESIAN_POINT('Ctrl Pts',(6.61871156025942,2.7513066887977,3.52742475123226));
#102428=CARTESIAN_POINT('Ctrl Pts',(6.112958964,2.620519775,3.897978027));
#102429=CARTESIAN_POINT('Ctrl Pts',(6.20888786,2.64969025,3.747538647));
#102430=CARTESIAN_POINT('Ctrl Pts',(6.297300509,2.678571429,3.592562637));
#102431=CARTESIAN_POINT('Ctrl Pts',(6.40598069,2.714073269,3.402060249));
#102432=CARTESIAN_POINT('Ctrl Pts',(6.502946732,2.75,3.205336768));
#102433=CARTESIAN_POINT('Ctrl Pts',(6.50471010480504,2.75065334439885,3.20175925953051));
#102434=CARTESIAN_POINT('Ctrl Pts',(6.50647347761008,2.7513066887977,3.19818175106102));
#102435=CARTESIAN_POINT('Ctrl Pts',(6.50294674220238,2.75000000214517,3.20533676924456));
#102436=CARTESIAN_POINT('Ctrl Pts',(6.43814167428525,2.72598918262104,3.33681245823215));
#102437=CARTESIAN_POINT('Ctrl Pts',(6.3695078439607,2.70215892421632,3.46599246044649));
#102438=CARTESIAN_POINT('Ctrl Pts',(6.29730050853279,2.67857142883765,3.59256263798011));
#102439=CARTESIAN_POINT('Ctrl Pts',(6.23930296822854,2.65962575352119,3.69422487150057));
#102440=CARTESIAN_POINT('Ctrl Pts',(6.17868369763219,2.64052352964207,3.7947596654705));
#102441=CARTESIAN_POINT('Ctrl Pts',(6.11551308270665,2.62129679686781,3.89396966220073));
#102442=CARTESIAN_POINT('Ctrl Pts',(6.832312826,2.75,3.093461079));
#102443=CARTESIAN_POINT('Ctrl Pts',(6.99994139199999,2.68564607,2.723231498));
#102444=CARTESIAN_POINT('Ctrl Pts',(7.126581858,2.620518779,2.337056058));
#102445=CARTESIAN_POINT('Ctrl Pts',(6.502946732,2.75,3.205336768));
#102446=CARTESIAN_POINT('Ctrl Pts',(6.676637621,2.68564607,2.852954888));
#102447=CARTESIAN_POINT('Ctrl Pts',(6.811233513,2.620518779,2.483867554));
#102448=CARTESIAN_POINT('',(6.80962413708076,2.62129679675697,2.48827626789476));
#102449=CARTESIAN_POINT('Origin',(-0.187761390900419,2.55361154127052,-0.0566040674048424));
#102450=CARTESIAN_POINT('Ctrl Pts',(7.04511341129868,2.66036061574169,2.57223191432732));
#102451=CARTESIAN_POINT('Ctrl Pts',(7.00581449606116,2.65417293172453,2.55825839585287));
#102452=CARTESIAN_POINT('Ctrl Pts',(6.96651975202736,2.64782918800484,2.54426875547398));
#102453=CARTESIAN_POINT('Ctrl Pts',(6.88803653220672,2.63481932842121,2.51628926384458));
#102454=CARTESIAN_POINT('Ctrl Pts',(6.84880104706384,2.62814542754618,2.50228265560733));
#102455=CARTESIAN_POINT('Ctrl Pts',(6.80962415850665,2.62129679727301,2.48827627372423));
#102456=CARTESIAN_POINT('Ctrl Pts',(6.954391929,2.620519775,2.808279349));
#102457=CARTESIAN_POINT('Ctrl Pts',(7.023503436,2.64969025,2.637132378));
#102458=CARTESIAN_POINT('Ctrl Pts',(7.084112554,2.678571429,2.462792993));
#102459=CARTESIAN_POINT('Ctrl Pts',(7.15861558,2.714073269,2.248488411));
#102460=CARTESIAN_POINT('Ctrl Pts',(7.22002818,2.75,2.030072186));
#102461=CARTESIAN_POINT('Ctrl Pts',(7.22114499684117,2.75065334439885,2.02610018483959));
#102462=CARTESIAN_POINT('Ctrl Pts',(7.22226181368234,2.7513066887977,2.02212818367917));
#102463=CARTESIAN_POINT('Ctrl Pts',(6.80799143300001,2.620519775,2.492739988));
#102464=CARTESIAN_POINT('Ctrl Pts',(6.86933754400001,2.64969025,2.325195919));
#102465=CARTESIAN_POINT('Ctrl Pts',(6.922367894,2.678571429,2.154837056));
#102466=CARTESIAN_POINT('Ctrl Pts',(6.987554811,2.714073269,1.945425482));
#102467=CARTESIAN_POINT('Ctrl Pts',(7.039964107,2.75,1.732456454));
#102468=CARTESIAN_POINT('Ctrl Pts',(7.04091719454892,2.75065334439885,1.72858351266357));
#102469=CARTESIAN_POINT('Ctrl Pts',(7.04187028209783,2.7513066887977,1.72471057132715));
#102470=CARTESIAN_POINT('Ctrl Pts',(7.03996411719344,2.75000000212625,1.73245645311726));
#102471=CARTESIAN_POINT('Ctrl Pts',(7.00493754211565,2.72598918242031,1.87478948781914));
#102472=CARTESIAN_POINT('Ctrl Pts',(6.96567821485752,2.702158924025,2.01570357841255));
#102473=CARTESIAN_POINT('Ctrl Pts',(6.92236789383464,2.67857142882524,2.154837057327));
#102474=CARTESIAN_POINT('Ctrl Pts',(6.88758067885014,2.65962575364295,2.26659024058532));
#102475=CARTESIAN_POINT('Ctrl Pts',(6.84999066209724,2.64052352987875,2.37780593736967));
#102476=CARTESIAN_POINT('Ctrl Pts',(6.80962415816835,2.62129679701491,2.48827627564519));
#102477=CARTESIAN_POINT('Ctrl Pts',(7.337579839,2.75,1.552392382));
#102478=CARTESIAN_POINT('Ctrl Pts',(7.421700926,2.68564607,1.154783377));
#102479=CARTESIAN_POINT('Ctrl Pts',(7.462364304,2.620518779,0.750412547000001));
#102480=CARTESIAN_POINT('Ctrl Pts',(7.039964107,2.75,1.732456454));
#102481=CARTESIAN_POINT('Ctrl Pts',(7.133842512,2.68564607,1.35097466));
#102482=CARTESIAN_POINT('Ctrl Pts',(7.18594876,2.620518779,0.961582243999999));
#102483=CARTESIAN_POINT('',(7.1853247538099,2.62129679675021,0.966233853240022));
#102484=CARTESIAN_POINT('Origin',(-0.195539767315837,2.5536115669031,-0.0149175448622552));
#102485=CARTESIAN_POINT('Ctrl Pts',(7.43335640141215,2.66036061571562,0.997603430550806));
#102486=CARTESIAN_POINT('Ctrl Pts',(7.39197237950679,2.65417293169836,0.992404710278094));
#102487=CARTESIAN_POINT('Ctrl Pts',(7.35058896583797,2.64782918801841,0.987189348332478));
#102488=CARTESIAN_POINT('Ctrl Pts',(7.26792587647577,2.63481932843988,0.976735573831541));
#102489=CARTESIAN_POINT('Ctrl Pts',(7.22659668848171,2.62814542757044,0.971490901712906));
#102490=CARTESIAN_POINT('Ctrl Pts',(7.18532477572538,2.62129679729411,0.966233854084293));
#102491=CARTESIAN_POINT('Ctrl Pts',(7.395499158,2.620519775,1.247634645));
#102492=CARTESIAN_POINT('Ctrl Pts',(7.426203336,2.64969025,1.065632063));
#102493=CARTESIAN_POINT('Ctrl Pts',(7.447917633,2.678571429,0.882339467));
#102494=CARTESIAN_POINT('Ctrl Pts',(7.474609669,2.714073269,0.657029259));
#102495=CARTESIAN_POINT('Ctrl Pts',(7.487633445,2.75,0.43051759));
#102496=CARTESIAN_POINT('Ctrl Pts',(7.48787028845513,2.75065334439885,0.426398369405856));
#102497=CARTESIAN_POINT('Ctrl Pts',(7.48810713191026,2.7513066887977,0.422279148811712));
#102498=CARTESIAN_POINT('Ctrl Pts',(7.184689789,2.620519775,0.970944197));
#102499=CARTESIAN_POINT('Ctrl Pts',(7.20858464,2.64969025,0.794129615));
#102500=CARTESIAN_POINT('Ctrl Pts',(7.22375305,2.678571429,0.616353689));
#102501=CARTESIAN_POINT('Ctrl Pts',(7.24239863499999,2.714073269,0.397824782));
#102502=CARTESIAN_POINT('Ctrl Pts',(7.247800585,2.75,0.178568402));
#102503=CARTESIAN_POINT('Ctrl Pts',(7.24789882198614,2.75065334439885,0.174581122228142));
#102504=CARTESIAN_POINT('Ctrl Pts',(7.24799705897229,2.7513066887977,0.170593842456285));
#102505=CARTESIAN_POINT('Ctrl Pts',(7.24780059470928,2.75000000206258,0.178568399286295));
#102506=CARTESIAN_POINT('Ctrl Pts',(7.24419031691365,2.72598918247015,0.325103444596959));
#102507=CARTESIAN_POINT('Ctrl Pts',(7.2361412148389,2.70215892409394,0.471162636311407));
#102508=CARTESIAN_POINT('Ctrl Pts',(7.22375304994782,2.67857142872828,0.616353690779953));
#102509=CARTESIAN_POINT('Ctrl Pts',(7.2138027715959,2.65962575337623,0.732972371121796));
#102510=CARTESIAN_POINT('Ctrl Pts',(7.20099967605123,2.64052352972992,0.84966864890671));
#102511=CARTESIAN_POINT('Ctrl Pts',(7.18532477574293,2.62129679699644,0.966233856230039));
#102512=CARTESIAN_POINT('Ctrl Pts',(7.499749774,2.75,-0.061264458));
#102513=CARTESIAN_POINT('Ctrl Pts',(7.496429973,2.68564607,-0.467661132));
#102514=CARTESIAN_POINT('Ctrl Pts',(7.449214889,2.620518779,-0.871319421));
#102515=CARTESIAN_POINT('Ctrl Pts',(7.247800585,2.75,0.178568402));
#102516=CARTESIAN_POINT('Ctrl Pts',(7.257476856,2.68564607,-0.214175642));
#102517=CARTESIAN_POINT('Ctrl Pts',(7.22465703000001,2.620518779,-0.605665582));
#102518=CARTESIAN_POINT('',(7.22504757083151,2.62129679672876,-0.600988582846018));
#102519=CARTESIAN_POINT('Origin',(-0.194175117513026,2.55361157223225,0.0274664925956096));
#102520=CARTESIAN_POINT('Ctrl Pts',(7.47402390811217,2.66036061571516,-0.623671881598151));
#102521=CARTESIAN_POINT('Ctrl Pts',(7.43248985057937,2.65417293169921,-0.619852717176769));
#102522=CARTESIAN_POINT('Ctrl Pts',(7.39095280939218,2.64782918798386,-0.616049936099405));
#102523=CARTESIAN_POINT('Ctrl Pts',(7.30797508488674,2.63481932839231,-0.608489186264437));
#102524=CARTESIAN_POINT('Ctrl Pts',(7.26648470091488,2.62814542749891,-0.604726687016057));
#102525=CARTESIAN_POINT('Ctrl Pts',(7.2250475927466,2.62129679719525,-0.600988586403805));
#102526=CARTESIAN_POINT('Ctrl Pts',(7.490801066,2.620519775,-0.37134807));
#102527=CARTESIAN_POINT('Ctrl Pts',(7.481662223,2.64969025,-0.555696023));
#102528=CARTESIAN_POINT('Ctrl Pts',(7.463466361,2.678571429,-0.739371272));
#102529=CARTESIAN_POINT('Ctrl Pts',(7.441099318,2.714073269,-0.965151851));
#102530=CARTESIAN_POINT('Ctrl Pts',(7.405125292,2.75,-1.18916753));
#102531=CARTESIAN_POINT('Ctrl Pts',(7.40447108751947,2.75065334439885,-1.19324135984913));
#102532=CARTESIAN_POINT('Ctrl Pts',(7.40381688303893,2.7513066887977,-1.19731518969825));
#102533=CARTESIAN_POINT('Ctrl Pts',(7.225440036,2.620519775,-0.596251866));
#102534=CARTESIAN_POINT('Ctrl Pts',(7.21076633,2.64969025,-0.774069308000001));
#102535=CARTESIAN_POINT('Ctrl Pts',(7.187363542,2.678571429,-0.95094969));
#102536=CARTESIAN_POINT('Ctrl Pts',(7.158595948,2.714073269,-1.168377763));
#102537=CARTESIAN_POINT('Ctrl Pts',(7.11673796300001,2.75,-1.383669311));
#102538=CARTESIAN_POINT('Ctrl Pts',(7.11597675597432,2.75065334439885,-1.38758448844839));
#102539=CARTESIAN_POINT('Ctrl Pts',(7.11521554894864,2.7513066887977,-1.39149966589679));
#102540=CARTESIAN_POINT('Ctrl Pts',(7.11673797190381,2.75000000204555,-1.38366931564545));
#102541=CARTESIAN_POINT('Ctrl Pts',(7.14471280393736,2.72598918246571,-1.23978407453484));
#102542=CARTESIAN_POINT('Ctrl Pts',(7.16825029390894,2.70215892410217,-1.09540934625179));
#102543=CARTESIAN_POINT('Ctrl Pts',(7.18736354224324,2.67857142879351,-0.95094968867717));
#102544=CARTESIAN_POINT('Ctrl Pts',(7.20271546464417,2.65962575353111,-0.83491847416344));
#102545=CARTESIAN_POINT('Ctrl Pts',(7.21529794894784,2.6405235296564,-0.718198202331916));
#102546=CARTESIAN_POINT('Ctrl Pts',(7.22504759310139,2.62129679694117,-0.600988584663608));
#102547=CARTESIAN_POINT('Ctrl Pts',(7.311239744,2.75,-1.672056639));
#102548=CARTESIAN_POINT('Ctrl Pts',(7.220634287,2.68564607,-2.068238326));
#102549=CARTESIAN_POINT('Ctrl Pts',(7.087748465,2.620518779,-2.452309461));
#102550=CARTESIAN_POINT('Ctrl Pts',(7.11673796300001,2.75,-1.383669311));
#102551=CARTESIAN_POINT('Ctrl Pts',(7.04175964800001,2.68564607,-1.769311329));
#102552=CARTESIAN_POINT('Ctrl Pts',(6.925548367,2.620518779,-2.14459316));
#102553=CARTESIAN_POINT('',(6.92693519374711,2.62129679672952,-2.14010946067906));
#102554=CARTESIAN_POINT('Origin',(-0.183731048098391,2.55361156244326,0.0685662800179587));
#102555=CARTESIAN_POINT('Ctrl Pts',(7.16521436356792,2.66036061573476,-2.21578498882252));
#102556=CARTESIAN_POINT('Ctrl Pts',(7.12547235665399,2.65417293170283,-2.20312651987865));
#102557=CARTESIAN_POINT('Ctrl Pts',(7.08572391417432,2.64782918801842,-2.19048340989173));
#102558=CARTESIAN_POINT('Ctrl Pts',(7.0063114127143,2.63481931404231,-2.16526164050143));
#102559=CARTESIAN_POINT('Ctrl Pts',(6.96659992419542,2.62814542052546,-2.15266791534343));
#102560=CARTESIAN_POINT('Ctrl Pts',(6.92693521452292,2.62129679727275,-2.14010946891741));
#102561=CARTESIAN_POINT('Ctrl Pts',(7.235841442,2.620519775,-1.972966961));
#102562=CARTESIAN_POINT('Ctrl Pts',(7.18728689900001,2.64969025,-2.15104038));
#102563=CARTESIAN_POINT('Ctrl Pts',(7.130031697,2.678571429,-2.326509831));
#102564=CARTESIAN_POINT('Ctrl Pts',(7.059651433,2.714073269,-2.542203533));
#102565=CARTESIAN_POINT('Ctrl Pts',(6.97636171000001,2.75,-2.753248498));
#102566=CARTESIAN_POINT('Ctrl Pts',(6.9748470474496,2.75065334439885,-2.75708644935128));
#102567=CARTESIAN_POINT('Ctrl Pts',(6.97333238489921,2.7513066887977,-2.76092440070255));
#102568=CARTESIAN_POINT('Ctrl Pts',(6.928336737,2.620519775,-2.135567854));
#102569=CARTESIAN_POINT('Ctrl Pts',(6.875780601,2.64969025,-2.30607361));
#102570=CARTESIAN_POINT('Ctrl Pts',(6.814900903,2.678571429,-2.47378772));
#102571=CARTESIAN_POINT('Ctrl Pts',(6.740065271,2.714073269,-2.679948262));
#102572=CARTESIAN_POINT('Ctrl Pts',(6.652904584,2.75,-2.881208184));
#102573=CARTESIAN_POINT('Ctrl Pts',(6.6513195261596,2.75065334439885,-2.88486818976985));
#102574=CARTESIAN_POINT('Ctrl Pts',(6.6497344683192,2.7513066887977,-2.8885281955397));
#102575=CARTESIAN_POINT('Ctrl Pts',(6.65290459080522,2.75000000185146,-2.88120818990272));
#102576=CARTESIAN_POINT('Ctrl Pts',(6.71115646016654,2.72598918232521,-2.74670066785988));
#102577=CARTESIAN_POINT('Ctrl Pts',(6.76517995624436,2.70215892402454,-2.6107612053006));
#102578=CARTESIAN_POINT('Ctrl Pts',(6.81490090360504,2.67857142871297,-2.47378771833322));
#102579=CARTESIAN_POINT('Ctrl Pts',(6.85483718843397,2.65962575339801,-2.36376945786321));
#102580=CARTESIAN_POINT('Ctrl Pts',(6.89221690912954,2.64052352967758,-2.25248290397871));
#102581=CARTESIAN_POINT('Ctrl Pts',(6.92693521473911,2.6212967969307,-2.14010946713021));
#102582=CARTESIAN_POINT('Ctrl Pts',(6.78086427000001,2.75,-3.20466531));
#102583=CARTESIAN_POINT('Ctrl Pts',(6.607209766,2.68564607,-3.572106995));
#102584=CARTESIAN_POINT('Ctrl Pts',(6.394866801,2.620518779,-3.918632236));
#102585=CARTESIAN_POINT('Ctrl Pts',(6.652904584,2.75,-2.881208184));
#102586=CARTESIAN_POINT('Ctrl Pts',(6.49677758500001,2.68564607,-3.241715985));
#102587=CARTESIAN_POINT('Ctrl Pts',(6.302608759,2.620518779,-3.583241945));
#102588=CARTESIAN_POINT('',(6.30492702512,2.62129679675646,-3.57916119849814));
#102589=CARTESIAN_POINT('Origin',(-0.164695427352005,2.5536115784274,0.106459792061169));
#102590=CARTESIAN_POINT('Ctrl Pts',(6.52136735922966,2.66036061573153,-3.70429045328558));
#102591=CARTESIAN_POINT('Ctrl Pts',(6.48527569502537,2.65417293170606,-3.68338457550447));
#102592=CARTESIAN_POINT('Ctrl Pts',(6.44917444389617,2.6478291880154,-3.6624923141011));
#102593=CARTESIAN_POINT('Ctrl Pts',(6.37704057755396,2.6348193285101,-3.6207889214374));
#102594=CARTESIAN_POINT('Ctrl Pts',(6.3409647573002,2.62814542763408,-3.59995280950605));
#102595=CARTESIAN_POINT('Ctrl Pts',(6.30492704406959,2.6212967973458,-3.57916121100208));
#102596=CARTESIAN_POINT('Ctrl Pts',(6.64254191400001,2.620519775,-3.48233211));
#102597=CARTESIAN_POINT('Ctrl Pts',(6.556842028,2.64969025,-3.64580448));
#102598=CARTESIAN_POINT('Ctrl Pts',(6.463204676,2.678571429,-3.804863377));
#102599=CARTESIAN_POINT('Ctrl Pts',(6.348102093,2.714073269,-4.000384604));
#102600=CARTESIAN_POINT('Ctrl Pts',(6.221391209,2.75,-4.188590626));
#102601=CARTESIAN_POINT('Ctrl Pts',(6.21908691233759,2.75065334439885,-4.19201324049569));
#102602=CARTESIAN_POINT('Ctrl Pts',(6.21678261567518,2.7513066887977,-4.19543585499139));
#102603=CARTESIAN_POINT('Ctrl Pts',(6.307272113,2.620519775,-3.575027062));
#102604=CARTESIAN_POINT('Ctrl Pts',(6.219291012,2.64969025,-3.730248473));
#102605=CARTESIAN_POINT('Ctrl Pts',(6.123781072,2.678571429,-3.880954185));
#102606=CARTESIAN_POINT('Ctrl Pts',(6.006376632,2.714073269,-4.06620736));
#102607=CARTESIAN_POINT('Ctrl Pts',(5.87798878,2.75,-4.244024965));
#102608=CARTESIAN_POINT('Ctrl Pts',(5.87565398689053,2.75065334439885,-4.247258661276));
#102609=CARTESIAN_POINT('Ctrl Pts',(5.87331919378106,2.7513066887977,-4.25049235755201));
#102610=CARTESIAN_POINT('Ctrl Pts',(5.87798878589075,2.75000000214011,-4.24402497340688));
#102611=CARTESIAN_POINT('Ctrl Pts',(5.96379390012507,2.72598918248584,-4.12518459223727));
#102612=CARTESIAN_POINT('Ctrl Pts',(6.04577732236949,2.70215892409288,-4.00403677323589));
#102613=CARTESIAN_POINT('Ctrl Pts',(6.12378107301353,2.6785714287419,-3.88095418361733));
#102614=CARTESIAN_POINT('Ctrl Pts',(6.18643434290713,2.65962575347408,-3.78209320983747));
#102615=CARTESIAN_POINT('Ctrl Pts',(6.2468634659768,2.64052352978639,-3.68144400870869));
#102616=CARTESIAN_POINT('Ctrl Pts',(6.304927044608,2.62129679704562,-3.57916120950667));
#102617=CARTESIAN_POINT('Ctrl Pts',(5.933423119,2.75,-4.587427393));
#102618=CARTESIAN_POINT('Ctrl Pts',(5.684839461,2.68564607,-4.90894791));
#102619=CARTESIAN_POINT('Ctrl Pts',(5.402968272,2.620518779,-5.201724123));
#102620=CARTESIAN_POINT('Ctrl Pts',(5.87798878,2.75,-4.244024965));
#102621=CARTESIAN_POINT('Ctrl Pts',(5.648013423,2.68564607,-4.562541604));
#102622=CARTESIAN_POINT('Ctrl Pts',(5.38496617,2.620518779,-4.854342319));
#102623=CARTESIAN_POINT('',(5.38810747655047,2.62129679676453,-4.85085533687023));
#102624=CARTESIAN_POINT('Origin',(-0.137959584860747,2.55361155743023,0.139375774651469));
#102625=CARTESIAN_POINT('Ctrl Pts',(5.57258846503529,2.66036061568084,-5.0195874129108));
#102626=CARTESIAN_POINT('Ctrl Pts',(5.54183474961983,2.65417293167813,-4.99141166200556));
#102627=CARTESIAN_POINT('Ctrl Pts',(5.51106874422187,2.64782918799662,-4.96324714814558));
#102628=CARTESIAN_POINT('Ctrl Pts',(5.44958625629412,2.63481931415693,-4.90701204664053));
#102629=CARTESIAN_POINT('Ctrl Pts',(5.41883305299396,2.62814542059962,-4.87890786977764));
#102630=CARTESIAN_POINT('Ctrl Pts',(5.38810749187737,2.62129679730596,-4.85085535319451));
#102631=CARTESIAN_POINT('Ctrl Pts',(5.73864450900001,2.620519775,-4.828867279));
#102632=CARTESIAN_POINT('Ctrl Pts',(5.619806511,2.64969025,-4.970094815));
#102633=CARTESIAN_POINT('Ctrl Pts',(5.494165387,2.678571429,-5.10530574));
#102634=CARTESIAN_POINT('Ctrl Pts',(5.33972255400001,2.714073269,-5.271512136));
#102635=CARTESIAN_POINT('Ctrl Pts',(5.175515369,2.75,-5.428078911));
#102636=CARTESIAN_POINT('Ctrl Pts',(5.17252918457452,2.75065334439885,-5.43092615099776));
#102637=CARTESIAN_POINT('Ctrl Pts',(5.16954300014905,2.7513066887977,-5.43377339099553));
#102638=CARTESIAN_POINT('Ctrl Pts',(5.391286454,2.620519775,-4.84732197900001));
#102639=CARTESIAN_POINT('Ctrl Pts',(5.271994288,2.64969025,-4.980001063));
#102640=CARTESIAN_POINT('Ctrl Pts',(5.146320044,2.678571429,-5.106651545));
#102641=CARTESIAN_POINT('Ctrl Pts',(4.991836498,2.714073269,-5.26233512));
#102642=CARTESIAN_POINT('Ctrl Pts',(4.828224754,2.75,-5.408395855));
#102643=CARTESIAN_POINT('Ctrl Pts',(4.82524939794747,2.75065334439885,-5.41105203774884));
#102644=CARTESIAN_POINT('Ctrl Pts',(4.82227404189494,2.7513066887977,-5.41370822049767));
#102645=CARTESIAN_POINT('Ctrl Pts',(4.82822475771829,2.75000000220518,-5.40839586474511));
#102646=CARTESIAN_POINT('Ctrl Pts',(4.9375709645692,2.72598918255007,-5.3107794688955));
#102647=CARTESIAN_POINT('Ctrl Pts',(5.04368086000124,2.70215892412742,-5.21008803075968));
#102648=CARTESIAN_POINT('Ctrl Pts',(5.14632004501918,2.67857142879894,-5.10665154411776));
#102649=CARTESIAN_POINT('Ctrl Pts',(5.22876070350902,2.65962575356672,-5.0235704863683));
#102650=CARTESIAN_POINT('Ctrl Pts',(5.30941363040642,2.64052352974731,-4.93826488256848));
#102651=CARTESIAN_POINT('Ctrl Pts',(5.38810749292814,2.62129679694484,-4.85085535157521));
#102652=CARTESIAN_POINT('Ctrl Pts',(4.808541698,2.75,-5.75568647));
#102653=CARTESIAN_POINT('Ctrl Pts',(4.49665238,2.68564607,-6.016251877));
#102654=CARTESIAN_POINT('Ctrl Pts',(4.158432951,2.620518779,-6.241589172));
#102655=CARTESIAN_POINT('Ctrl Pts',(4.828224754,2.75,-5.408395855));
#102656=CARTESIAN_POINT('Ctrl Pts',(4.535154431,2.68564607,-5.670027848));
#102657=CARTESIAN_POINT('Ctrl Pts',(4.215528549,2.620518779,-5.898459041));
#102658=CARTESIAN_POINT('',(4.21934601090526,2.62129679674693,-5.89572887059208));
#102659=CARTESIAN_POINT('Origin',(-0.104772268716402,2.55361159886235,0.165774192984351));
#102660=CARTESIAN_POINT('Ctrl Pts',(4.36324152744183,2.66036061573346,-6.10017404411017));
#102661=CARTESIAN_POINT('Ctrl Pts',(4.33926377051569,2.65417293173651,-6.06604588682158));
#102662=CARTESIAN_POINT('Ctrl Pts',(4.31527159526947,2.64782918804367,-6.0319260618976));
#102663=CARTESIAN_POINT('Ctrl Pts',(4.26731541777163,2.63481931396713,-5.96378878721195));
#102664=CARTESIAN_POINT('Ctrl Pts',(4.24332277513809,2.62814542050229,-5.92973064133862));
#102665=CARTESIAN_POINT('Ctrl Pts',(4.21934602294037,2.62129679727644,-5.89572888996312));
#102666=CARTESIAN_POINT('Ctrl Pts',(4.566414464,2.620519775,-5.949609982));
#102667=CARTESIAN_POINT('Ctrl Pts',(4.419995088,2.64969025,-6.061989039));
#102668=CARTESIAN_POINT('Ctrl Pts',(4.268225031,2.678571429,-6.167029681));
#102669=CARTESIAN_POINT('Ctrl Pts',(4.081663524,2.714073269,-6.29614962));
#102670=CARTESIAN_POINT('Ctrl Pts',(3.887638183,2.75,-6.41375626));
#102671=CARTESIAN_POINT('Ctrl Pts',(3.88410974146778,2.75065334439885,-6.41589499172907));
#102672=CARTESIAN_POINT('Ctrl Pts',(3.88058129993557,2.7513066887977,-6.41803372345814));
#102673=CARTESIAN_POINT('Ctrl Pts',(4.223210233,2.620519775,-5.892961507));
#102674=CARTESIAN_POINT('Ctrl Pts',(4.07818497,2.64969025,-5.996894338));
#102675=CARTESIAN_POINT('Ctrl Pts',(3.928222811,2.678571429,-6.093567555));
#102676=CARTESIAN_POINT('Ctrl Pts',(3.743883638,2.714073269,-6.212401939));
#102677=CARTESIAN_POINT('Ctrl Pts',(3.552698305,2.75,-6.319876166));
#102678=CARTESIAN_POINT('Ctrl Pts',(3.54922151034096,2.75065334439885,-6.3218306350618));
#102679=CARTESIAN_POINT('Ctrl Pts',(3.54574471568191,2.7513066887977,-6.3237851041236));
#102680=CARTESIAN_POINT('Ctrl Pts',(3.55269830635737,2.75000000180332,-6.31987617446485));
#102681=CARTESIAN_POINT('Ctrl Pts',(3.68047269970421,2.7259891823433,-6.24804819932019));
#102682=CARTESIAN_POINT('Ctrl Pts',(3.80574748764423,2.70215892406801,-6.17252136266766));
#102683=CARTESIAN_POINT('Ctrl Pts',(3.92822281185286,2.67857142883575,-6.0935675544502));
#102684=CARTESIAN_POINT('Ctrl Pts',(4.02659602465126,2.65962575356054,-6.03015118985405));
#102685=CARTESIAN_POINT('Ctrl Pts',(4.12370151429173,2.6405235297314,-5.96417797883247));
#102686=CARTESIAN_POINT('Ctrl Pts',(4.21934602375908,2.62129679691319,-5.89572888850613));
#102687=CARTESIAN_POINT('Ctrl Pts',(3.458818211,2.75,-6.654816044));
#102688=CARTESIAN_POINT('Ctrl Pts',(3.098206832,2.68564607,-6.84224259300001));
#102689=CARTESIAN_POINT('Ctrl Pts',(2.719453928,2.620518779,-6.989604448));
#102690=CARTESIAN_POINT('Ctrl Pts',(3.552698305,2.75,-6.319876166));
#102691=CARTESIAN_POINT('Ctrl Pts',(3.210236658,2.68564607,-6.512389893));
#102692=CARTESIAN_POINT('Ctrl Pts',(2.848977497,2.620518779,-6.666770374));
#102693=CARTESIAN_POINT('',(2.85329261535825,2.6212967967578,-6.66492467544232));
#102694=CARTESIAN_POINT('Origin',(-0.066686121994719,2.55361157478581,0.184421228183209));
#102695=CARTESIAN_POINT('Ctrl Pts',(2.94987426576481,2.66036061570823,-6.89552331690139));
#102696=CARTESIAN_POINT('Ctrl Pts',(2.93379364027752,2.65417293168017,-6.85703854795253));
#102697=CARTESIAN_POINT('Ctrl Pts',(2.91769714239881,2.64782918797754,-6.81855881708673));
#102698=CARTESIAN_POINT('Ctrl Pts',(2.88550968917187,2.63481932838112,-6.74170547885327));
#102699=CARTESIAN_POINT('Ctrl Pts',(2.86939945647989,2.6281454275173,-6.70328583852385));
#102700=CARTESIAN_POINT('Ctrl Pts',(2.85329262215917,2.62129679725448,-6.6649246965331));
#102701=CARTESIAN_POINT('Ctrl Pts',(3.180663955,2.620519775,-6.792155535));
#102702=CARTESIAN_POINT('Ctrl Pts',(3.013509606,2.64969025,-6.870431394));
#102703=CARTESIAN_POINT('Ctrl Pts',(2.842707217,2.678571429,-6.940390168));
#102704=CARTESIAN_POINT('Ctrl Pts',(2.632750443,2.714073269,-7.026386145));
#102705=CARTESIAN_POINT('Ctrl Pts',(2.417979356,2.75,-7.099533494));
#102706=CARTESIAN_POINT('Ctrl Pts',(2.41407364337821,2.75065334439885,-7.10086371273768));
#102707=CARTESIAN_POINT('Ctrl Pts',(2.41016793075642,2.7513066887977,-7.10219393147536));
#102708=CARTESIAN_POINT('Ctrl Pts',(2.857661396,2.620519775,-6.66305270500001));
#102709=CARTESIAN_POINT('Ctrl Pts',(2.693684256,2.64969025,-6.7333795));
#102710=CARTESIAN_POINT('Ctrl Pts',(2.526446244,2.678571429,-6.795555119));
#102711=CARTESIAN_POINT('Ctrl Pts',(2.320870939,2.714073269,-6.871983747));
#102712=CARTESIAN_POINT('Ctrl Pts',(2.111051631,2.75,-6.935846092));
#102713=CARTESIAN_POINT('Ctrl Pts',(2.10723596879426,2.75065334439885,-6.93700745859924));
#102714=CARTESIAN_POINT('Ctrl Pts',(2.10342030658853,2.7513066887977,-6.93816882519847));
#102715=CARTESIAN_POINT('Ctrl Pts',(2.11105163072352,2.75000000211533,-6.93584610220118));
#102716=CARTESIAN_POINT('Ctrl Pts',(2.25127962127389,2.72598918249932,-6.89316514142643));
#102717=CARTESIAN_POINT('Ctrl Pts',(2.38986159126746,2.70215892411409,-6.84633445600132));
#102718=CARTESIAN_POINT('Ctrl Pts',(2.52644624583777,2.6785714287138,-6.79555511846654));
#102719=CARTESIAN_POINT('Ctrl Pts',(2.63615219227389,2.65962575336085,-6.75476872620667));
#102720=CARTESIAN_POINT('Ctrl Pts',(2.74516969954801,2.64052352965217,-6.71121274234204));
#102721=CARTESIAN_POINT('Ctrl Pts',(2.85329262422745,2.62129679697703,-6.66492469606858));
#102722=CARTESIAN_POINT('Ctrl Pts',(1.947364229,2.75,-7.242773817));
#102723=CARTESIAN_POINT('Ctrl Pts',(1.554892575,2.68564607,-7.34829765));
#102724=CARTESIAN_POINT('Ctrl Pts',(1.153316261,2.620518779,-7.410793588));
#102725=CARTESIAN_POINT('Ctrl Pts',(2.111051631,2.75,-6.93584609200001));
#102726=CARTESIAN_POINT('Ctrl Pts',(1.735211787,2.68564607,-7.050239824));
#102727=CARTESIAN_POINT('Ctrl Pts',(1.349211424,2.620518779,-7.12335093400001));
#102728=CARTESIAN_POINT('',(1.35382242820159,2.62129679672353,-7.12247600992274));
#102729=CARTESIAN_POINT('Origin',(-0.0254819632860184,2.55361154608468,
0.194445344653661));
#102730=CARTESIAN_POINT('Ctrl Pts',(1.39857416152078,2.66036061573687,-7.36844558304455));
#102731=CARTESIAN_POINT('Ctrl Pts',(1.39114257989476,2.65417293171228,-7.32740370749941));
#102732=CARTESIAN_POINT('Ctrl Pts',(1.38369441393053,2.64782918799579,-7.28636334001544));
#102733=CARTESIAN_POINT('Ctrl Pts',(1.36878066512432,2.6348193141661,-7.20438734954117));
#102734=CARTESIAN_POINT('Ctrl Pts',(1.36130617631967,2.62814542053127,-7.16340276316861));
#102735=CARTESIAN_POINT('Ctrl Pts',(1.35382242975113,2.62129679720304,-7.1224760318306));
#102736=CARTESIAN_POINT('Ctrl Pts',(1.646189134,2.620519775,-7.317107443));
#102737=CARTESIAN_POINT('Ctrl Pts',(1.466115765,2.64969025,-7.35762001300001));
#102738=CARTESIAN_POINT('Ctrl Pts',(1.284267572,2.678571429,-7.389225724));
#102739=CARTESIAN_POINT('Ctrl Pts',(1.060732878,2.714073269,-7.428076663));
#102740=CARTESIAN_POINT('Ctrl Pts',(0.835258502,2.75,-7.453344433));
#102741=CARTESIAN_POINT('Ctrl Pts',(0.831158145063998,2.75065334439885,
-7.45380393921004));
#102742=CARTESIAN_POINT('Ctrl Pts',(0.827057788127997,2.7513066887977,-7.45426344542008));
#102743=CARTESIAN_POINT('Ctrl Pts',(1.358491487,2.620519775,-7.121586964));
#102744=CARTESIAN_POINT('Ctrl Pts',(1.18322986,2.64969025,-7.155019319));
#102745=CARTESIAN_POINT('Ctrl Pts',(1.00653586,2.678571429,-7.179790078));
#102746=CARTESIAN_POINT('Ctrl Pts',(0.789336895,2.714073269,-7.210239234));
#102747=CARTESIAN_POINT('Ctrl Pts',(0.570694529000001,2.75,-7.227503563));
#102748=CARTESIAN_POINT('Ctrl Pts',(0.566718415359787,2.75065334439885,
-7.22781752289387));
#102749=CARTESIAN_POINT('Ctrl Pts',(0.562742301719575,2.7513066887977,-7.22813148278776));
#102750=CARTESIAN_POINT('Ctrl Pts',(0.57069452699854,2.75000000202792,-7.22750357280113));
#102751=CARTESIAN_POINT('Ctrl Pts',(0.716819209619973,2.72598918245556,
-7.21596534231266));
#102752=CARTESIAN_POINT('Ctrl Pts',(0.862228423498231,2.7021589240943,-7.2000205595361));
#102753=CARTESIAN_POINT('Ctrl Pts',(1.00653586114367,2.67857142881306,-7.17979007783967));
#102754=CARTESIAN_POINT('Ctrl Pts',(1.12244481134483,2.65962575358551,-7.16354078428866));
#102755=CARTESIAN_POINT('Ctrl Pts',(1.23827679923776,2.64052352976744,-7.14443865663331));
#102756=CARTESIAN_POINT('Ctrl Pts',(1.35382243243794,2.62129679689708,-7.12247603205826));
#102757=CARTESIAN_POINT('Ctrl Pts',(0.344853659,2.75,-7.492067535));
#102758=CARTESIAN_POINT('Ctrl Pts',(-0.06112673,2.68564607,-7.510754476));
#102759=CARTESIAN_POINT('Ctrl Pts',(-0.466749192,2.620518779,-7.485462256));
#102760=CARTESIAN_POINT('Ctrl Pts',(0.570694529,2.75,-7.227503563));
#102761=CARTESIAN_POINT('Ctrl Pts',(0.179050341,2.68564607,-7.258428376));
#102762=CARTESIAN_POINT('Ctrl Pts',(-0.213642275,2.620518779,-7.246851522));
#102763=CARTESIAN_POINT('',(-0.208950991335437,2.62129679670998,-7.24698828190642));
#102764=CARTESIAN_POINT('Origin',(0.0169137971775209,2.55361155556727,0.195377074967155));
#102765=CARTESIAN_POINT('Ctrl Pts',(-0.218121715942913,2.66036061575241,
-7.49682752321785));
#102766=CARTESIAN_POINT('Ctrl Pts',(-0.216556761285011,2.65417293173166,
-7.45514761364917));
#102767=CARTESIAN_POINT('Ctrl Pts',(-0.215008327401407,2.64782918799023,
-7.41346561156725));
#102768=CARTESIAN_POINT('Ctrl Pts',(-0.211950989513393,2.6348193284523,
-7.33020025072329));
#102769=CARTESIAN_POINT('Ctrl Pts',(-0.21044025237885,2.62814542754474,
-7.28856701830798));
#102770=CARTESIAN_POINT('Ctrl Pts',(-0.208950993846219,2.6212967972171,
-7.24698830450965));
#102771=CARTESIAN_POINT('Ctrl Pts',(0.034740338,2.620519775,-7.49991954));
#102772=CARTESIAN_POINT('Ctrl Pts',(-0.14983202,2.64969025,-7.500774497));
#102773=CARTESIAN_POINT('Ctrl Pts',(-0.334222997,2.678571429,-7.492549298));
#102774=CARTESIAN_POINT('Ctrl Pts',(-0.560883377,2.714073269,-7.482438573));
#102775=CARTESIAN_POINT('Ctrl Pts',(-0.786518112,2.75,-7.45864527));
#102776=CARTESIAN_POINT('Ctrl Pts',(-0.790621385139384,2.75065334439885,
-7.45821257766166));
#102777=CARTESIAN_POINT('Ctrl Pts',(-0.794724658278768,2.7513066887977,
-7.45777988532332));
#102778=CARTESIAN_POINT('Ctrl Pts',(-0.204199974,2.620519775,-7.247123731));
#102779=CARTESIAN_POINT('Ctrl Pts',(-0.382551049,2.64969025,-7.242098388));
#102780=CARTESIAN_POINT('Ctrl Pts',(-0.560439023,2.678571429,-7.228306033));
#102781=CARTESIAN_POINT('Ctrl Pts',(-0.779105665,2.714073269,-7.211351947));
#102782=CARTESIAN_POINT('Ctrl Pts',(-0.996347613999999,2.75,-7.181211));
#102783=CARTESIAN_POINT('Ctrl Pts',(-1.00029826040238,2.75065334439885,
-7.18066287278802));
#102784=CARTESIAN_POINT('Ctrl Pts',(-1.00424890680475,2.7513066887977,-7.18011474557605));
#102785=CARTESIAN_POINT('Ctrl Pts',(-0.996347618322142,2.7500000020761,
-7.18121100914202));
#102786=CARTESIAN_POINT('Ctrl Pts',(-0.851158871176989,2.72598918253573,
-7.20135502381853));
#102787=CARTESIAN_POINT('Ctrl Pts',(-0.705721587186126,2.70215892416151,
-7.21704170399089));
#102788=CARTESIAN_POINT('Ctrl Pts',(-0.560439021319831,2.67857142875185,
-7.22830603329573));
#102789=CARTESIAN_POINT('Ctrl Pts',(-0.443746839286387,2.65962575341567,
-7.23735363741317));
#102790=CARTESIAN_POINT('Ctrl Pts',(-0.32651654668961,2.6405235296885,-7.24359856009063));
#102791=CARTESIAN_POINT('Ctrl Pts',(-0.208950991956025,2.62129679689047,
-7.24698830445382));
#102792=CARTESIAN_POINT('Ctrl Pts',(-1.273781884,2.75,-7.391040503));
#102793=CARTESIAN_POINT('Ctrl Pts',(-1.674287817,2.68564607,-7.32201677));
#102794=CARTESIAN_POINT('Ctrl Pts',(-2.064989971,2.620518779,-7.210119029));
#102795=CARTESIAN_POINT('Ctrl Pts',(-0.996347614,2.75,-7.181211));
#102796=CARTESIAN_POINT('Ctrl Pts',(-1.3854833,2.68564607,-7.127220885));
#102797=CARTESIAN_POINT('Ctrl Pts',(-1.766506299,2.620518779,-7.031497386));
#102798=CARTESIAN_POINT('',(-1.76195409432501,2.62129679672433,-7.03263943647596));
#102799=CARTESIAN_POINT('Origin',(0.0585186503573701,2.55361154586131,0.187173271427979));
#102800=CARTESIAN_POINT('Ctrl Pts',(-1.82461846412332,2.66036061571567,
-7.27466614044675));
#102801=CARTESIAN_POINT('Ctrl Pts',(-1.8141301486489,2.65417293170062,-7.2342971029069));
#102802=CARTESIAN_POINT('Ctrl Pts',(-1.80365751794335,2.64782918797959,
-7.19392247040153));
#102803=CARTESIAN_POINT('Ctrl Pts',(-1.78277206752517,2.63481932841364,
-7.11326104422478));
#102804=CARTESIAN_POINT('Ctrl Pts',(-1.77234673630568,2.62814542753473,
-7.07292593747618));
#102805=CARTESIAN_POINT('Ctrl Pts',(-1.76195410139986,2.62129679725034,
-7.03263945744462));
#102806=CARTESIAN_POINT('Ctrl Pts',(-1.578332876,2.620519775,-7.332043735));
#102807=CARTESIAN_POINT('Ctrl Pts',(-1.758773826,2.64969025,-7.29320110200001));
#102808=CARTESIAN_POINT('Ctrl Pts',(-1.93708567,2.678571429,-7.245529595));
#102809=CARTESIAN_POINT('Ctrl Pts',(-2.156273349,2.714073269,-7.18692997));
#102810=CARTESIAN_POINT('Ctrl Pts',(-2.371518013,2.75,-7.115188143));
#102811=CARTESIAN_POINT('Ctrl Pts',(-2.37543233784093,2.75065334439885,
-7.11388348433696));
#102812=CARTESIAN_POINT('Ctrl Pts',(-2.37934666268186,2.7513066887977,-7.11257882567393));
#102813=CARTESIAN_POINT('Ctrl Pts',(-1.75734327,2.620519775,-7.033793047));
#102814=CARTESIAN_POINT('Ctrl Pts',(-1.930444297,2.64969025,-6.990544984));
#102815=CARTESIAN_POINT('Ctrl Pts',(-2.1012084,2.678571429,-6.938834431));
#102816=CARTESIAN_POINT('Ctrl Pts',(-2.31111811,2.714073269,-6.875269858));
#102817=CARTESIAN_POINT('Ctrl Pts',(-2.516801651,2.75,-6.799132993));
#102818=CARTESIAN_POINT('Ctrl Pts',(-2.52054210234939,2.75065334439885,
-6.79774840851628));
#102819=CARTESIAN_POINT('Ctrl Pts',(-2.52428255369877,2.7513066887977,-6.79636382403254));
#102820=CARTESIAN_POINT('Ctrl Pts',(-2.5168016566078,2.75000000185138,-6.7991329999353));
#102821=CARTESIAN_POINT('Ctrl Pts',(-2.37933770907025,2.72598918241709,
-6.85001734795752));
#102822=CARTESIAN_POINT('Ctrl Pts',(-2.24067284049077,2.70215892412675,
-6.89660199923303));
#102823=CARTESIAN_POINT('Ctrl Pts',(-2.10120839845448,2.67857142876085,
-6.93883443167389));
#102824=CARTESIAN_POINT('Ctrl Pts',(-1.98918938248059,2.65962575341989,
-6.97275587723097));
#102825=CARTESIAN_POINT('Ctrl Pts',(-1.87604234262511,2.64052352971441,
-7.00405584468662));
#102826=CARTESIAN_POINT('Ctrl Pts',(-1.76195409969139,2.62129679698603,
-7.03263945807132));
#102827=CARTESIAN_POINT('Ctrl Pts',(-2.832856802,2.75,-6.944416631));
#102828=CARTESIAN_POINT('Ctrl Pts',(-3.209161066,2.68564607,-6.79090969800001));
#102829=CARTESIAN_POINT('Ctrl Pts',(-3.566674115,2.620518779,-6.59763865));
#102830=CARTESIAN_POINT('Ctrl Pts',(-2.516801651,2.75,-6.799132993));
#102831=CARTESIAN_POINT('Ctrl Pts',(-2.885233281,2.68564607,-6.662752466));
#102832=CARTESIAN_POINT('Ctrl Pts',(-3.236770452,2.620518779,-6.487358248));
#102833=CARTESIAN_POINT('',(-3.23257018276947,2.62129679674423,-6.48945218719692));
#102834=CARTESIAN_POINT('Origin',(0.0973871803849591,2.55361159636233,0.170217400774161));
#102835=CARTESIAN_POINT('Ctrl Pts',(-3.34579808097766,2.66036061570176,
-6.7123494544089));
#102836=CARTESIAN_POINT('Ctrl Pts',(-3.3268768267527,2.65417293169771,-6.67517890034009));
#102837=CARTESIAN_POINT('Ctrl Pts',(-3.30796968780511,2.64782918798304,
-6.63799951031197));
#102838=CARTESIAN_POINT('Ctrl Pts',(-3.27023266366539,2.63481931404014,
-6.56371357577716));
#102839=CARTESIAN_POINT('Ctrl Pts',(-3.25138023767489,2.6281454204954,-6.52656266338797));
#102840=CARTESIAN_POINT('Ctrl Pts',(-3.23257019393207,2.6212967972269,-6.48945220628804));
#102841=CARTESIAN_POINT('Ctrl Pts',(-3.117605,2.620519775,-6.82132971400001));
#102842=CARTESIAN_POINT('Ctrl Pts',(-3.285477323,2.64969025,-6.74460573));
#102843=CARTESIAN_POINT('Ctrl Pts',(-3.44937237,2.678571429,-6.65971698));
#102844=CARTESIAN_POINT('Ctrl Pts',(-3.650838376,2.714073269,-6.55536851));
#102845=CARTESIAN_POINT('Ctrl Pts',(-3.845628367,2.75,-6.439032727));
#102846=CARTESIAN_POINT('Ctrl Pts',(-3.84917071404994,2.75065334439885,
-6.4369171063996));
#102847=CARTESIAN_POINT('Ctrl Pts',(-3.85271306109988,2.7513066887977,-6.43480148579919));
#102848=CARTESIAN_POINT('Ctrl Pts',(-3.228315149,2.620519775,-6.491570018));
#102849=CARTESIAN_POINT('Ctrl Pts',(-3.388072114,2.64969025,-6.41212146700001));
#102850=CARTESIAN_POINT('Ctrl Pts',(-3.543727607,2.678571429,-6.324910643));
#102851=CARTESIAN_POINT('Ctrl Pts',(-3.735065241,2.714073269,-6.217707792));
#102852=CARTESIAN_POINT('Ctrl Pts',(-3.919572839,2.75,-6.099135083));
#102853=CARTESIAN_POINT('Ctrl Pts',(-3.92292819592626,2.75065334439885,
-6.09697878285453));
#102854=CARTESIAN_POINT('Ctrl Pts',(-3.92628355285251,2.7513066887977,-6.09482248270906));
#102855=CARTESIAN_POINT('Ctrl Pts',(-3.91957284540621,2.75000000173482,
-6.09913508878106));
#102856=CARTESIAN_POINT('Ctrl Pts',(-3.79626135957307,2.72598918222916,
-6.17838047388788));
#102857=CARTESIAN_POINT('Ctrl Pts',(-3.67085272169801,2.70215892397846,
-6.25368484994515));
#102858=CARTESIAN_POINT('Ctrl Pts',(-3.54372760583484,2.67857142879977,
-6.32491064390992));
#102859=CARTESIAN_POINT('Ctrl Pts',(-3.4416196408124,2.65962575360389,-6.38211980256457));
#102860=CARTESIAN_POINT('Ctrl Pts',(-3.33784648368696,2.64052352982283,
-6.43701126295269));
#102861=CARTESIAN_POINT('Ctrl Pts',(-3.23257019267236,2.62129679701602,
-6.48945220717682));
#102862=CARTESIAN_POINT('Ctrl Pts',(-4.259470484,2.75,-6.173079555));
#102863=CARTESIAN_POINT('Ctrl Pts',(-4.593977511,2.68564607,-5.942267236));
#102864=CARTESIAN_POINT('Ctrl Pts',(-4.901584541,2.620518779,-5.67666002));
#102865=CARTESIAN_POINT('Ctrl Pts',(-3.919572839,2.75,-6.099135083));
#102866=CARTESIAN_POINT('Ctrl Pts',(-4.250072961,2.68564607,-5.886741148));
#102867=CARTESIAN_POINT('Ctrl Pts',(-4.555686816,2.620518779,-5.63987744800001));
#102868=CARTESIAN_POINT('',(-4.55203488165151,2.62129679675248,-5.64282536603537));
#102869=CARTESIAN_POINT('Origin',(0.131702096318875,2.55361160479069,0.145302536969056));
#102870=CARTESIAN_POINT('Ctrl Pts',(-4.71053189794187,2.66036061569364,
-5.83617076779155));
#102871=CARTESIAN_POINT('Ctrl Pts',(-4.68406244165634,2.65417293167332,
-5.803936750918));
#102872=CARTESIAN_POINT('Ctrl Pts',(-4.65760487150524,2.64782918798595,
-5.77169107051523));
#102873=CARTESIAN_POINT('Ctrl Pts',(-4.60478083769685,2.63481931393408,
-5.70725424395961));
#102874=CARTESIAN_POINT('Ctrl Pts',(-4.57838282326677,2.62814542045161,
-5.67502461382145));
#102875=CARTESIAN_POINT('Ctrl Pts',(-4.55203489663523,2.62129679725494,
-5.64282538215023));
#102876=CARTESIAN_POINT('Ctrl Pts',(-4.511101379,2.620519775,-5.991657896));
#102877=CARTESIAN_POINT('Ctrl Pts',(-4.658555551,2.64969025,-5.880640089));
#102878=CARTESIAN_POINT('Ctrl Pts',(-4.800370252,2.678571429,-5.762503401));
#102879=CARTESIAN_POINT('Ctrl Pts',(-4.974694258,2.714073269,-5.617285305));
#102880=CARTESIAN_POINT('Ctrl Pts',(-5.139921412,2.75,-5.461795298));
#102881=CARTESIAN_POINT('Ctrl Pts',(-5.14292614503858,2.75065334439885,
-5.4589676395317));
#102882=CARTESIAN_POINT('Ctrl Pts',(-5.14593087807715,2.7513066887977,-5.4561399810634));
#102883=CARTESIAN_POINT('Ctrl Pts',(-4.548334599,2.620519775,-5.64580839));
#102884=CARTESIAN_POINT('Ctrl Pts',(-4.687277446,2.64969025,-5.533874277));
#102885=CARTESIAN_POINT('Ctrl Pts',(-4.82054605,2.678571429,-5.415241063));
#102886=CARTESIAN_POINT('Ctrl Pts',(-4.984364872,2.714073269,-5.26941262000001));
#102887=CARTESIAN_POINT('Ctrl Pts',(-5.139069158,2.75,-5.113948395));
#102888=CARTESIAN_POINT('Ctrl Pts',(-5.14188252776459,2.75065334439885,
-5.11112120538942));
#102889=CARTESIAN_POINT('Ctrl Pts',(-5.14469589752919,2.7513066887977,-5.10829401577884));
#102890=CARTESIAN_POINT('Ctrl Pts',(-5.13906916729271,2.75000000215022,
-5.11394839941884));
#102891=CARTESIAN_POINT('Ctrl Pts',(-5.03567604992564,2.72598918253933,
-5.21784939570737));
#102892=CARTESIAN_POINT('Ctrl Pts',(-4.92938761055078,2.70215892413535,
-5.31835234710694));
#102893=CARTESIAN_POINT('Ctrl Pts',(-4.82054604927562,2.67857142885136,
-5.41524106427285));
#102894=CARTESIAN_POINT('Ctrl Pts',(-4.73312359013776,2.65962575362265,
-5.49306289968832));
#102895=CARTESIAN_POINT('Ctrl Pts',(-4.64357663284416,2.64052352977815,
-5.56897918933333));
#102896=CARTESIAN_POINT('Ctrl Pts',(-4.5520348957225,2.62129679707988,-5.64282538356341));
#102897=CARTESIAN_POINT('Ctrl Pts',(-5.48691606000001,2.75,-5.113096141));
#102898=CARTESIAN_POINT('Ctrl Pts',(-5.763984674,2.68564607,-4.815770962));
#102899=CARTESIAN_POINT('Ctrl Pts',(-6.007302322,2.620518779,-4.490247077));
#102900=CARTESIAN_POINT('Ctrl Pts',(-5.13906915800001,2.75,-5.113948395));
#102901=CARTESIAN_POINT('Ctrl Pts',(-5.416183953,2.68564607,-4.835472356));
#102902=CARTESIAN_POINT('Ctrl Pts',(-5.661584328,2.620518779,-4.528682248));
#102903=CARTESIAN_POINT('',(-5.65865148836948,2.62129679673279,-4.53234630297675));
#102904=CARTESIAN_POINT('Origin',(0.159858817764672,2.55361156890335,0.113593444025223));
#102905=CARTESIAN_POINT('Ctrl Pts',(-5.85500647919589,2.66036061571563,
-4.68709922284819));
#102906=CARTESIAN_POINT('Ctrl Pts',(-5.82222650337217,2.65417293170312,
-4.66130897015096));
#102907=CARTESIAN_POINT('Ctrl Pts',(-5.7894556283497,2.64782918801518,-4.63550477145482));
#102908=CARTESIAN_POINT('Ctrl Pts',(-5.72401457821685,2.63481931397628,
-4.58393004824197));
#102909=CARTESIAN_POINT('Ctrl Pts',(-5.69130531690168,2.62814542047764,
-4.55812872183861));
#102910=CARTESIAN_POINT('Ctrl Pts',(-5.6586515072447,2.62129679723727,-4.53234631570846));
#102911=CARTESIAN_POINT('Ctrl Pts',(-5.693663671,2.620519775,-4.881822815));
#102912=CARTESIAN_POINT('Ctrl Pts',(-5.8138049,2.64969025,-4.741702254));
#102913=CARTESIAN_POINT('Ctrl Pts',(-5.926908156,2.678571429,-4.595841568));
#102914=CARTESIAN_POINT('Ctrl Pts',(-6.06593896600001,2.714073269,-4.416544081));
#102915=CARTESIAN_POINT('Ctrl Pts',(-6.193877446,2.75,-4.22917039));
#102916=CARTESIAN_POINT('Ctrl Pts',(-6.19620406706957,2.75065334439885,
-4.22576291183265));
#102917=CARTESIAN_POINT('Ctrl Pts',(-6.19853068813914,2.7513066887977,-4.22235543366531));
#102918=CARTESIAN_POINT('Ctrl Pts',(-5.655678979,2.620519775,-4.536055036));
#102919=CARTESIAN_POINT('Ctrl Pts',(-5.767310893,2.64969025,-4.396869275));
#102920=CARTESIAN_POINT('Ctrl Pts',(-5.871961118,2.678571429,-4.25236083));
#102921=CARTESIAN_POINT('Ctrl Pts',(-6.000601142,2.714073269,-4.074725571));
#102922=CARTESIAN_POINT('Ctrl Pts',(-6.118268315,2.75,-3.889639164));
#102923=CARTESIAN_POINT('Ctrl Pts',(-6.12040814754998,2.75065334439885,
-3.88627328116149));
#102924=CARTESIAN_POINT('Ctrl Pts',(-6.12254798009995,2.7513066887977,-3.88290739832298));
#102925=CARTESIAN_POINT('Ctrl Pts',(-6.11826832433658,2.75000000195366,
-3.88963916712843));
#102926=CARTESIAN_POINT('Ctrl Pts',(-6.03962812370742,2.72598918244455,
-4.01333747952319));
#102927=CARTESIAN_POINT('Ctrl Pts',(-5.95742981306564,2.7021589241026,-4.13433960064318));
#102928=CARTESIAN_POINT('Ctrl Pts',(-5.87196111701464,2.67857142872806,
-4.25236083136066));
#102929=CARTESIAN_POINT('Ctrl Pts',(-5.80331193947458,2.65962575341578,
-4.34715647935858));
#102930=CARTESIAN_POINT('Ctrl Pts',(-5.73217829903779,2.64052352969838,
-4.44054783755659));
#102931=CARTESIAN_POINT('Ctrl Pts',(-5.65865150590329,2.62129679689485,
-4.53234631705455));
#102932=CARTESIAN_POINT('Ctrl Pts',(-6.45779954,2.75,-3.814030034));
#102933=CARTESIAN_POINT('Ctrl Pts',(-6.664474319,2.68564607,-3.464094591));
#102934=CARTESIAN_POINT('Ctrl Pts',(-6.832125323,2.620518779,-3.093875171));
#102935=CARTESIAN_POINT('Ctrl Pts',(-6.118268315,2.75,-3.889639164));
#102936=CARTESIAN_POINT('Ctrl Pts',(-6.32904020300001,2.68564607,-3.55810225));
#102937=CARTESIAN_POINT('Ctrl Pts',(-6.502752449,2.620518779,-3.205730898));
#102938=CARTESIAN_POINT('',(-6.50067584106015,2.62129679674404,-3.20993976355605));
#102939=CARTESIAN_POINT('Origin',(0.180540677085579,2.55361154875563,0.0765727896387824));
#102940=CARTESIAN_POINT('Ctrl Pts',(-6.72570746453641,2.66036061567559,
-3.3188641275846));
#102941=CARTESIAN_POINT('Ctrl Pts',(-6.68814972429273,2.65417293167416,
-3.30072356240331));
#102942=CARTESIAN_POINT('Ctrl Pts',(-6.65059787432564,2.64782918802872,
-3.28256742095169));
#102943=CARTESIAN_POINT('Ctrl Pts',(-6.57559984230319,2.63481932852972,
-3.24626641781343));
#102944=CARTESIAN_POINT('Ctrl Pts',(-6.53810873796849,2.6281454276242,-3.22809981464685));
#102945=CARTESIAN_POINT('Ctrl Pts',(-6.50067586214077,2.62129679727841,
-3.20993977181534));
#102946=CARTESIAN_POINT('Ctrl Pts',(-6.609996578,2.620519775,-3.543719125));
#102947=CARTESIAN_POINT('Ctrl Pts',(-6.69720719300001,2.64969025,-3.381047692));
#102948=CARTESIAN_POINT('Ctrl Pts',(-6.776310422,2.678571429,-3.21428329));
#102949=CARTESIAN_POINT('Ctrl Pts',(-6.87354710900001,2.714073269,-3.009290165));
#102950=CARTESIAN_POINT('Ctrl Pts',(-6.958214653,2.75,-2.798794176));
#102951=CARTESIAN_POINT('Ctrl Pts',(-6.9597543718694,2.75065334439885,-2.79496620803394));
#102952=CARTESIAN_POINT('Ctrl Pts',(-6.96129409073881,2.7513066887977,-2.79113824006787));
#102953=CARTESIAN_POINT('Ctrl Pts',(-6.498570095,2.620519775,-3.21420079));
#102954=CARTESIAN_POINT('Ctrl Pts',(-6.577671293,2.64969025,-3.054271554));
#102955=CARTESIAN_POINT('Ctrl Pts',(-6.64880981,2.678571429,-2.890644931));
#102956=CARTESIAN_POINT('Ctrl Pts',(-6.736255972,2.714073269,-2.689508882));
#102957=CARTESIAN_POINT('Ctrl Pts',(-6.811384045,2.75,-2.483454729));
#102958=CARTESIAN_POINT('Ctrl Pts',(-6.81275028412961,2.75065334439885,
-2.47970753789814));
#102959=CARTESIAN_POINT('Ctrl Pts',(-6.81411652325921,2.7513066887977,-2.47596034679627));
#102960=CARTESIAN_POINT('Ctrl Pts',(-6.81138405521894,2.75000000212232,
-2.48345472924284));
#102961=CARTESIAN_POINT('Ctrl Pts',(-6.76117389920765,2.725989182386,-2.62116636306209));
#102962=CARTESIAN_POINT('Ctrl Pts',(-6.70690921864762,2.70215892399437,
-2.75700972931182));
#102963=CARTESIAN_POINT('Ctrl Pts',(-6.64880980919581,2.67857142867351,
-2.89064493284972));
#102964=CARTESIAN_POINT('Ctrl Pts',(-6.60214387345002,2.65962575339749,
-2.99798185511659));
#102965=CARTESIAN_POINT('Ctrl Pts',(-6.55274967912501,2.64052352965437,
-3.10448140515898));
#102966=CARTESIAN_POINT('Ctrl Pts',(-6.50067586096218,2.62129679690187,
-3.20993977341216));
#102967=CARTESIAN_POINT('Ctrl Pts',(-7.12672349100001,2.75,-2.336624121));
#102968=CARTESIAN_POINT('Ctrl Pts',(-7.253340552,2.68564607,-1.950441006));
#102969=CARTESIAN_POINT('Ctrl Pts',(-7.33748573700001,2.620518779,-1.5528371));
#102970=CARTESIAN_POINT('Ctrl Pts',(-6.811384045,2.75,-2.483454729));
#102971=CARTESIAN_POINT('Ctrl Pts',(-6.945957567,2.68564607,-2.114359238));
#102972=CARTESIAN_POINT('Ctrl Pts',(-7.039859092,2.620518779,-1.732883135));
#102973=CARTESIAN_POINT('',(-7.03873581629141,2.62129679674192,-1.73744000847421));
#102974=CARTESIAN_POINT('Origin',(0.192780490359736,2.55361158252651,0.0359716161125356));
#102975=CARTESIAN_POINT('Ctrl Pts',(-7.28192184408587,2.66036061572226,
-1.79544263397009));
#102976=CARTESIAN_POINT('Ctrl Pts',(-7.24134249763625,2.65417293168304,
-1.78579998894316));
#102977=CARTESIAN_POINT('Ctrl Pts',(-7.20076555515356,2.64782918799088,
-1.77614086563833));
#102978=CARTESIAN_POINT('Ctrl Pts',(-7.11971729231985,2.63481932841169,
-1.75681091979893));
#102979=CARTESIAN_POINT('Ctrl Pts',(-7.07919742648692,2.62814542752202,
-1.74712852112551));
#102980=CARTESIAN_POINT('Ctrl Pts',(-7.03873583813208,2.62129679722243,
-1.73744001214078));
#102981=CARTESIAN_POINT('Ctrl Pts',(-7.217253392,2.620519775,-2.039915067));
#102982=CARTESIAN_POINT('Ctrl Pts',(-7.26745552200001,2.64969025,-1.862299097));
#102983=CARTESIAN_POINT('Ctrl Pts',(-7.308859943,2.678571429,-1.682428699));
#102984=CARTESIAN_POINT('Ctrl Pts',(-7.359755829,2.714073269,-1.461325186));
#102985=CARTESIAN_POINT('Ctrl Pts',(-7.39719347800001,2.75,-1.237549456));
#102986=CARTESIAN_POINT('Ctrl Pts',(-7.39787429914903,2.75065334439885,
-1.23347998973562));
#102987=CARTESIAN_POINT('Ctrl Pts',(-7.39855512029806,2.7513066887977,-1.22941052347124));
#102988=CARTESIAN_POINT('Ctrl Pts',(-7.037595296,2.620519775,-1.742054088));
#102989=CARTESIAN_POINT('Ctrl Pts',(-7.080467094,2.64969025,-1.568859488));
#102990=CARTESIAN_POINT('Ctrl Pts',(-7.114767544,2.678571429,-1.393765687));
#102991=CARTESIAN_POINT('Ctrl Pts',(-7.156930959,2.714073269,-1.178533747));
#102992=CARTESIAN_POINT('Ctrl Pts',(-7.186007028,2.75,-0.961146711));
#102993=CARTESIAN_POINT('Ctrl Pts',(-7.18653578990772,2.75065334439885,
-0.9571934261227));
#102994=CARTESIAN_POINT('Ctrl Pts',(-7.18706455181544,2.7513066887977,-0.953240141245399));
#102995=CARTESIAN_POINT('Ctrl Pts',(-7.18600703699163,2.75000000185139,
-0.961146709604796));
#102996=CARTESIAN_POINT('Ctrl Pts',(-7.16657469761462,2.7259891822928,-1.10643242097761));
#102997=CARTESIAN_POINT('Ctrl Pts',(-7.14278100306208,2.70215892400084,
-1.25076514649307));
#102998=CARTESIAN_POINT('Ctrl Pts',(-7.11476754411235,2.67857142885841,
-1.39376568827563));
#102999=CARTESIAN_POINT('Ctrl Pts',(-7.09226689836446,2.65962575370281,
-1.50862492879154));
#103000=CARTESIAN_POINT('Ctrl Pts',(-7.06692176743887,2.64052352974924,
-1.62325287091066));
#103001=CARTESIAN_POINT('Ctrl Pts',(-7.03873583780033,2.62129679695612,
-1.73744001381952));
#103002=CARTESIAN_POINT('Ctrl Pts',(-7.462409772,2.75,-0.749960261));
#103003=CARTESIAN_POINT('Ctrl Pts',(-7.503048642,2.68564607,-0.345586968));
#103004=CARTESIAN_POINT('Ctrl Pts',(-7.499753473,2.620518779,0.060809907));
#103005=CARTESIAN_POINT('Ctrl Pts',(-7.186007028,2.75,-0.961146711));
#103006=CARTESIAN_POINT('Ctrl Pts',(-7.238089675,2.68564607,-0.571751139));
#103007=CARTESIAN_POINT('Ctrl Pts',(-7.247789749,2.620518779,-0.179007682));
#103008=CARTESIAN_POINT('',(-7.24767232795708,2.62129679675596,-0.183699489826389));
#103009=CARTESIAN_POINT('Origin',(0.196006361824517,2.55361159069313,-0.00631146489151906));
#103010=CARTESIAN_POINT('Ctrl Pts',(-7.49764165155661,2.66036061571001,
-0.188068238498516));
#103011=CARTESIAN_POINT('Ctrl Pts',(-7.45593814404777,2.65417293169288,
-0.18737439329813));
#103012=CARTESIAN_POINT('Ctrl Pts',(-7.41423344183167,2.64782918798851,
-0.186663938151601));
#103013=CARTESIAN_POINT('Ctrl Pts',(-7.33092467541011,2.63481932842647,
-0.185208896412547));
#103014=CARTESIAN_POINT('Ctrl Pts',(-7.28927071209075,2.62814542755626,
-0.184463440166955));
#103015=CARTESIAN_POINT('Ctrl Pts',(-7.24767235005735,2.62129679727333,
-0.183699488584394));
#103016=CARTESIAN_POINT('Ctrl Pts',(-7.487039458,2.620519775,-0.440726847));
#103017=CARTESIAN_POINT('Ctrl Pts',(-7.497885707,2.64969025,-0.256471467));
#103018=CARTESIAN_POINT('Ctrl Pts',(-7.499655298,2.678571429,-0.071905611));
#103019=CARTESIAN_POINT('Ctrl Pts',(-7.501830546,2.714073269,0.154969736));
#103020=CARTESIAN_POINT('Ctrl Pts',(-7.490287756,2.75,0.381561701));
#103021=CARTESIAN_POINT('Ctrl Pts',(-7.49007784496764,2.75065334439885,
0.385682381814436));
#103022=CARTESIAN_POINT('Ctrl Pts',(-7.48986793393528,2.7513066887977,0.389803062628871));
#103023=CARTESIAN_POINT('Ctrl Pts',(-7.247550363,2.620519775,-0.188450873));
#103024=CARTESIAN_POINT('Ctrl Pts',(-7.252188123,2.64969025,-0.010089297));
#103025=CARTESIAN_POINT('Ctrl Pts',(-7.248046656,2.678571429,0.168284491));
#103026=CARTESIAN_POINT('Ctrl Pts',(-7.242955809,2.714073269,0.387548315));
#103027=CARTESIAN_POINT('Ctrl Pts',(-7.224620308,2.75,0.606103459));
#103028=CARTESIAN_POINT('Ctrl Pts',(-7.22428686834254,2.75065334439885,
0.610077986467366));
#103029=CARTESIAN_POINT('Ctrl Pts',(-7.22395342868507,2.7513066887977,0.614052513934733));
#103030=CARTESIAN_POINT('Ctrl Pts',(-7.22462031736331,2.75000000207842,
0.606103462833411));
#103031=CARTESIAN_POINT('Ctrl Pts',(-7.23687442859809,2.72598918256373,
0.460037072307496));
#103032=CARTESIAN_POINT('Ctrl Pts',(-7.24466428685568,2.70215892418055,
0.313963824585473));
#103033=CARTESIAN_POINT('Ctrl Pts',(-7.24804665632304,2.67857142884258,
0.168284489740948));
#103034=CARTESIAN_POINT('Ctrl Pts',(-7.25076340467764,2.65962575351862,
0.0512736197741986));
#103035=CARTESIAN_POINT('Ctrl Pts',(-7.25065244802159,2.64052352961112,
-0.0661228385726127));
#103036=CARTESIAN_POINT('Ctrl Pts',(-7.24767235001763,2.62129679697412,
-0.183699490421209));
#103037=CARTESIAN_POINT('Ctrl Pts',(-7.44916206600001,2.75,0.871770907));
#103038=CARTESIAN_POINT('Ctrl Pts',(-7.401922517,2.68564607,1.275426333));
#103039=CARTESIAN_POINT('Ctrl Pts',(-7.311341072,2.620518779,1.671613511));
#103040=CARTESIAN_POINT('Ctrl Pts',(-7.224620308,2.75,0.606103459));
#103041=CARTESIAN_POINT('Ctrl Pts',(-7.19177675500001,2.68564607,0.997591409));
#103042=CARTESIAN_POINT('Ctrl Pts',(-7.116821813,2.620518779,1.383237971));
#103043=CARTESIAN_POINT('',(-7.11771573692104,2.62129679676499,1.37863061339408));
#103044=CARTESIAN_POINT('Origin',(0.190067036668271,2.55361154355146,-0.0482994856586152));
#103045=CARTESIAN_POINT('Ctrl Pts',(-7.36278006810718,2.66036061569806,
1.42810001883199));
#103046=CARTESIAN_POINT('Ctrl Pts',(-7.32190240929651,2.65417293168015,
1.41981262099689));
#103047=CARTESIAN_POINT('Ctrl Pts',(-7.28102001316054,2.64782918800092,
1.41154118785102));
#103048=CARTESIAN_POINT('Ctrl Pts',(-7.19934616913844,2.6348193285361,1.39505328929647));
#103049=CARTESIAN_POINT('Ctrl Pts',(-7.15850580107923,2.6281454276242,1.38682694622748));
#103050=CARTESIAN_POINT('Ctrl Pts',(-7.11771575851542,2.62129679728327,
1.37863061888986));
#103051=CARTESIAN_POINT('Ctrl Pts',(-7.40673988,2.620519775,1.17906927));
#103052=CARTESIAN_POINT('Ctrl Pts',(-7.37772309,2.64969025,1.361348485));
#103053=CARTESIAN_POINT('Ctrl Pts',(-7.339775105,2.678571429,1.541979703));
#103054=CARTESIAN_POINT('Ctrl Pts',(-7.293128004,2.714073269,1.764018444));
#103055=CARTESIAN_POINT('Ctrl Pts',(-7.233144504,2.75,1.982831457));
#103056=CARTESIAN_POINT('Ctrl Pts',(-7.23205367601043,2.75065334439885,
1.98681067393568));
#103057=CARTESIAN_POINT('Ctrl Pts',(-7.23096284802087,2.7513066887977,1.99078989087137));
#103058=CARTESIAN_POINT('Ctrl Pts',(-7.11861803000001,2.620519775,1.373964096));
#103059=CARTESIAN_POINT('Ctrl Pts',(-7.084804895,2.64969025,1.549152658));
#103060=CARTESIAN_POINT('Ctrl Pts',(-7.042415162,2.678571429,1.722465874));
#103061=CARTESIAN_POINT('Ctrl Pts',(-6.990308095,2.714073269,1.93550905));
#103062=CARTESIAN_POINT('Ctrl Pts',(-6.925418373,2.75,2.145012905));
#103063=CARTESIAN_POINT('Ctrl Pts',(-6.92423832306972,2.75065334439885,
2.14882283054546));
#103064=CARTESIAN_POINT('Ctrl Pts',(-6.92305827313945,2.7513066887977,2.15263275609092));
#103065=CARTESIAN_POINT('Ctrl Pts',(-6.92541838129421,2.75000000210847,
2.145012910917));
#103066=CARTESIAN_POINT('Ctrl Pts',(-6.96878595413734,2.72598918243438,
2.0049957425919));
#103067=CARTESIAN_POINT('Ctrl Pts',(-7.00779512022632,2.70215892404854,
1.86401219552958));
#103068=CARTESIAN_POINT('Ctrl Pts',(-7.04241516236796,2.6785714287493,1.72246587249559));
#103069=CARTESIAN_POINT('Ctrl Pts',(-7.07022227218096,2.65962575346698,
1.60877467199151));
#103070=CARTESIAN_POINT('Ctrl Pts',(-7.09535067827354,2.6405235297452,1.49409902583102));
#103071=CARTESIAN_POINT('Ctrl Pts',(-7.11771575821681,2.62129679697527,
1.37863061748385));
#103072=CARTESIAN_POINT('Ctrl Pts',(-7.087599821,2.75,2.452739036));
#103073=CARTESIAN_POINT('Ctrl Pts',(-6.954690722,2.68564607,2.836802116));
#103074=CARTESIAN_POINT('Ctrl Pts',(-6.781058488,2.620518779,3.204254325));
#103075=CARTESIAN_POINT('Ctrl Pts',(-6.925418373,2.75,2.145012905));
#103076=CARTESIAN_POINT('Ctrl Pts',(-6.809184347,2.68564607,2.520287691));
#103077=CARTESIAN_POINT('Ctrl Pts',(-6.653079198,2.620518779,2.880804954));
#103078=CARTESIAN_POINT('',(-6.654942668555,2.621296796722,2.87649748087442));
#103079=CARTESIAN_POINT('Origin',(0.17524062960169,2.55361151296453,-0.0880291569088504));
#103080=CARTESIAN_POINT('Ctrl Pts',(-6.8836430721632,2.66036061573128,2.9774919065786));
#103081=CARTESIAN_POINT('Ctrl Pts',(-6.84550265583457,2.65417293172294,
2.9606107751241));
#103082=CARTESIAN_POINT('Ctrl Pts',(-6.80735418082379,2.64782918801609,
2.94374421675597));
#103083=CARTESIAN_POINT('Ctrl Pts',(-6.73113415227105,2.63481931414431,
2.91008429684051));
#103084=CARTESIAN_POINT('Ctrl Pts',(-6.69301707486491,2.62814542054318,
2.89327082926511));
#103085=CARTESIAN_POINT('Ctrl Pts',(-6.65494268790158,2.62129679721243,
2.87649749143627));
#103086=CARTESIAN_POINT('Ctrl Pts',(-6.980109378,2.620519775,2.743733418));
#103087=CARTESIAN_POINT('Ctrl Pts',(-6.912586341,2.64969025,2.915513294));
#103088=CARTESIAN_POINT('Ctrl Pts',(-6.836695187,2.678571429,3.08376376));
#103089=CARTESIAN_POINT('Ctrl Pts',(-6.74340690300001,2.714073269,3.290583611));
#103090=CARTESIAN_POINT('Ctrl Pts',(-6.637787454,2.75,3.491386217));
#103091=CARTESIAN_POINT('Ctrl Pts',(-6.63586671494324,2.75065334439885,
3.49503790626459));
#103092=CARTESIAN_POINT('Ctrl Pts',(-6.63394597588646,2.7513066887977,3.49868959552918));
#103093=CARTESIAN_POINT('Ctrl Pts',(-6.65682703,2.620519775,2.872134031));
#103094=CARTESIAN_POINT('Ctrl Pts',(-6.586144065,2.64969025,3.035957957));
#103095=CARTESIAN_POINT('Ctrl Pts',(-6.507488162,2.678571429,3.196106666));
#103096=CARTESIAN_POINT('Ctrl Pts',(-6.41080134400001,2.714073269,3.392967532));
#103097=CARTESIAN_POINT('Ctrl Pts',(-6.302391571,2.75,3.583623931));
#103098=CARTESIAN_POINT('Ctrl Pts',(-6.30042008859683,2.75065334439885,
3.58709110674698));
#103099=CARTESIAN_POINT('Ctrl Pts',(-6.29844860619365,2.7513066887977,3.59055828249396));
#103100=CARTESIAN_POINT('Ctrl Pts',(-6.30239157792162,2.75000000206173,
3.58362393832676));
#103101=CARTESIAN_POINT('Ctrl Pts',(-6.37484479333945,2.72598918245582,
3.45620304037037));
#103102=CARTESIAN_POINT('Ctrl Pts',(-6.44324924246583,2.70215892407921,
3.32690142786726));
#103103=CARTESIAN_POINT('Ctrl Pts',(-6.50748816256116,2.67857142879395,
3.19610666485744));
#103104=CARTESIAN_POINT('Ctrl Pts',(-6.55908540503802,2.65962575352184,
3.09105120863447));
#103105=CARTESIAN_POINT('Ctrl Pts',(-6.6082781975179,2.64052352964498,2.9844584793457));
#103106=CARTESIAN_POINT('Ctrl Pts',(-6.654942688836,2.62129679689933,2.876497489609));
#103107=CARTESIAN_POINT('Ctrl Pts',(-6.39462928600001,2.75,3.919019814));
#103108=CARTESIAN_POINT('Ctrl Pts',(-6.182265318,2.68564607,4.265532185));
#103109=CARTESIAN_POINT('Ctrl Pts',(-5.933701147,2.620518779,4.587067767));
#103110=CARTESIAN_POINT('Ctrl Pts',(-6.302391571,2.75,3.583623931));
#103111=CARTESIAN_POINT('Ctrl Pts',(-6.108202046,2.68564607,3.925138122));
#103112=CARTESIAN_POINT('Ctrl Pts',(-5.878245994,2.620518779,4.243668699));
#103113=CARTESIAN_POINT('',(-5.88099187697605,2.62129679673668,4.23986252331473));
#103114=CARTESIAN_POINT('Origin',(0.152219762000134,2.55361156885222,-0.123642510782943));
#103115=CARTESIAN_POINT('Ctrl Pts',(-6.08263457681295,2.66036061569563,
4.38765958121683));
#103116=CARTESIAN_POINT('Ctrl Pts',(-6.04901480627198,2.6541729316607,4.36297405921584));
#103117=CARTESIAN_POINT('Ctrl Pts',(-6.01538403300628,2.64782918799544,
4.33830103740138));
#103118=CARTESIAN_POINT('Ctrl Pts',(-5.94818187354502,2.6348193140604,4.28904301441427));
#103119=CARTESIAN_POINT('Ctrl Pts',(-5.91457035089412,2.62814542052291,
4.26442859164504));
#103120=CARTESIAN_POINT('Ctrl Pts',(-5.88099189383972,2.6212967972618,4.23986253752156));
#103121=CARTESIAN_POINT('Ctrl Pts',(-6.227096719,2.620519775,4.180103641));
#103122=CARTESIAN_POINT('Ctrl Pts',(-6.124224737,2.64969025,4.333351942));
#103123=CARTESIAN_POINT('Ctrl Pts',(-6.013939,2.678571429,4.48135445));
#103124=CARTESIAN_POINT('Ctrl Pts',(-5.87837158900001,2.714073269,4.663284745));
#103125=CARTESIAN_POINT('Ctrl Pts',(-5.73205484,2.75,4.836687639));
#103126=CARTESIAN_POINT('Ctrl Pts',(-5.72939400151689,2.75065334439885,
4.83984105169261));
#103127=CARTESIAN_POINT('Ctrl Pts',(-5.72673316303378,2.7513066887977,4.84299446438521));
#103128=CARTESIAN_POINT('Ctrl Pts',(-5.88377019600001,2.620519775,4.23600617));
#103129=CARTESIAN_POINT('Ctrl Pts',(-5.779522458,2.64969025,4.380805236));
#103130=CARTESIAN_POINT('Ctrl Pts',(-5.668278248,2.678571429,4.520301063));
#103131=CARTESIAN_POINT('Ctrl Pts',(-5.531532647,2.714073269,4.69177462400001));
#103132=CARTESIAN_POINT('Ctrl Pts',(-5.384671945,2.75,4.854668686));
#103133=CARTESIAN_POINT('Ctrl Pts',(-5.38200121447729,2.75065334439885,
4.85763099066985));
#103134=CARTESIAN_POINT('Ctrl Pts',(-5.37933048395458,2.7513066887977,4.8605932953397));
#103135=CARTESIAN_POINT('Ctrl Pts',(-5.38467194950976,2.75000000185146,
4.85466869376947));
#103136=CARTESIAN_POINT('Ctrl Pts',(-5.48282297559008,2.72598918230731,
4.74580212529041));
#103137=CARTESIAN_POINT('Ctrl Pts',(-5.57742419140515,2.70215892400846,
4.63422844718347));
#103138=CARTESIAN_POINT('Ctrl Pts',(-5.66827824886269,2.67857142885437,
4.5203010622626));
#103139=CARTESIAN_POINT('Ctrl Pts',(-5.74125299381477,2.65962575370558,
4.42879362677771));
#103140=CARTESIAN_POINT('Ctrl Pts',(-5.81220997162734,2.64052352979421,
4.33526797231565));
#103141=CARTESIAN_POINT('Ctrl Pts',(-5.88099189479517,2.62129679697574,
4.23986253611313));
#103142=CARTESIAN_POINT('Ctrl Pts',(-5.40265299200001,2.75,5.202051581));
#103143=CARTESIAN_POINT('Ctrl Pts',(-5.120764059,2.68564607,5.49481071));
#103144=CARTESIAN_POINT('Ctrl Pts',(-4.808890534,2.620518779,5.75539502));
#103145=CARTESIAN_POINT('Ctrl Pts',(-5.384671945,2.75,4.854668686));
#103146=CARTESIAN_POINT('Ctrl Pts',(-5.121607007,2.68564607,5.14645345700001));
#103147=CARTESIAN_POINT('Ctrl Pts',(-4.828552541,2.620518779,5.408103212));
#103148=CARTESIAN_POINT('',(-4.83205244227338,2.62129679674723,5.40497630621078));
#103149=CARTESIAN_POINT('Origin',(0.122081501320788,2.55361158027122,-0.153474593694516));
#103150=CARTESIAN_POINT('Ctrl Pts',(-4.99720884880956,2.66036061571327,
5.59266517169272));
#103151=CARTESIAN_POINT('Ctrl Pts',(-4.96968174741625,2.65417293168221,
5.5613295265844));
#103152=CARTESIAN_POINT('Ctrl Pts',(-4.94214121319586,2.64782918798291,
5.53000372390746));
#103153=CARTESIAN_POINT('Ctrl Pts',(-4.88709922210057,2.63481931410792,
5.46745084842157));
#103154=CARTESIAN_POINT('Ctrl Pts',(-4.85956489132207,2.62814542052642,
5.43618641305384));
#103155=CARTESIAN_POINT('Ctrl Pts',(-4.83205245535895,2.62129679724376,
5.40497632383663));
#103156=CARTESIAN_POINT('Ctrl Pts',(-5.182911938,2.620519775,5.421016864));
#103157=CARTESIAN_POINT('Ctrl Pts',(-5.049501192,2.64969025,5.54856787));
#103158=CARTESIAN_POINT('Ctrl Pts',(-4.909977709,2.678571429,5.669401988));
#103159=CARTESIAN_POINT('Ctrl Pts',(-4.738470154,2.714073269,5.817935867));
#103160=CARTESIAN_POINT('Ctrl Pts',(-4.558297712,2.75,5.955830922));
#103161=CARTESIAN_POINT('Ctrl Pts',(-4.55502119191227,2.75065334439885,
5.95833860804061));
#103162=CARTESIAN_POINT('Ctrl Pts',(-4.55174467182455,2.7513066887977,5.96084629408121));
#103163=CARTESIAN_POINT('Ctrl Pts',(-4.83559480800001,2.620519775,5.401807369));
#103164=CARTESIAN_POINT('Ctrl Pts',(-4.702656805,2.64969025,5.520810931));
#103165=CARTESIAN_POINT('Ctrl Pts',(-4.564025943,2.678571429,5.633131207));
#103166=CARTESIAN_POINT('Ctrl Pts',(-4.393615631,2.714073269,5.771199548));
#103167=CARTESIAN_POINT('Ctrl Pts',(-4.215171043,2.75,5.89871452800001));
#103168=CARTESIAN_POINT('Ctrl Pts',(-4.21192594474503,2.75065334439885,
5.90103344752409));
#103169=CARTESIAN_POINT('Ctrl Pts',(-4.20868084649006,2.7513066887977,5.90335236704817));
#103170=CARTESIAN_POINT('Ctrl Pts',(-4.21517104541964,2.75000000186761,
5.89871453657559));
#103171=CARTESIAN_POINT('Ctrl Pts',(-4.33443044977284,2.72598918235011,
5.81349277726625));
#103172=CARTESIAN_POINT('Ctrl Pts',(-4.45080498379104,2.70215892405622,
5.72486409502537));
#103173=CARTESIAN_POINT('Ctrl Pts',(-4.56402594458306,2.67857142870357,
5.63313120586397));
#103174=CARTESIAN_POINT('Ctrl Pts',(-4.65496597508599,2.65962575335656,
5.55945057512922));
#103175=CARTESIAN_POINT('Ctrl Pts',(-4.74436926877494,2.64052352971437,
5.48336515216562));
#103176=CARTESIAN_POINT('Ctrl Pts',(-4.832052457168,2.62129679698418,5.4049763228133));
#103177=CARTESIAN_POINT('Ctrl Pts',(-4.158054649,2.75,6.241841198));
#103178=CARTESIAN_POINT('Ctrl Pts',(-3.819821564,2.68564607,6.467157993));
#103179=CARTESIAN_POINT('Ctrl Pts',(-3.459221545,2.620518779,6.654606397));
#103180=CARTESIAN_POINT('Ctrl Pts',(-4.215171043,2.75,5.898714528));
#103181=CARTESIAN_POINT('Ctrl Pts',(-3.895531316,2.68564607,6.127126348));
#103182=CARTESIAN_POINT('Ctrl Pts',(-3.553081338,2.620518779,6.31966083));
#103183=CARTESIAN_POINT('',(-3.55717160563945,2.62129679674548,6.31735940436044));
#103184=CARTESIAN_POINT('Origin',(0.0862346281103571,2.55361157933354,-0.176130081684605));
#103185=CARTESIAN_POINT('Ctrl Pts',(-3.67811918906671,2.66036061564738,
6.53616395320052));
#103186=CARTESIAN_POINT('Ctrl Pts',(-3.65797189341086,2.65417293161587,
6.49964340504796));
#103187=CARTESIAN_POINT('Ctrl Pts',(-3.63780936335807,2.64782918797976,
6.46312958192037));
#103188=CARTESIAN_POINT('Ctrl Pts',(-3.59750124233113,2.63481931400623,
6.39020675646657));
#103189=CARTESIAN_POINT('Ctrl Pts',(-3.5773315786538,2.628145420512,6.35375419959446));
#103190=CARTESIAN_POINT('Ctrl Pts',(-3.55717161500516,2.62129679727785,
6.31735942476804));
#103191=CARTESIAN_POINT('Ctrl Pts',(-3.896379956,2.620519775,6.408449363));
#103192=CARTESIAN_POINT('Ctrl Pts',(-3.738668582,2.64969025,6.50433893));
#103193=CARTESIAN_POINT('Ctrl Pts',(-3.576431317,2.678571429,6.592354589));
#103194=CARTESIAN_POINT('Ctrl Pts',(-3.37700312,2.714073269,6.700546775));
#103195=CARTESIAN_POINT('Ctrl Pts',(-3.17139965,2.75,6.79648617));
#103196=CARTESIAN_POINT('Ctrl Pts',(-3.16766065477918,2.75065334439885,
6.7982308727494));
#103197=CARTESIAN_POINT('Ctrl Pts',(-3.16392165955837,2.7513066887977,6.79997557549878));
#103198=CARTESIAN_POINT('Ctrl Pts',(-3.56131238,2.620519775,6.315026059));
#103199=CARTESIAN_POINT('Ctrl Pts',(-3.405900146,2.64969025,6.402669643));
#103200=CARTESIAN_POINT('Ctrl Pts',(-3.246364857,2.678571429,6.482562396));
#103201=CARTESIAN_POINT('Ctrl Pts',(-3.050258032,2.714073269,6.580769596));
#103202=CARTESIAN_POINT('Ctrl Pts',(-2.848573427,2.75,6.666943035));
#103203=CARTESIAN_POINT('Ctrl Pts',(-2.84490569817126,2.75065334439885,
6.66851013927399));
#103204=CARTESIAN_POINT('Ctrl Pts',(-2.84123796934252,2.7513066887977,6.67007724354796));
#103205=CARTESIAN_POINT('Ctrl Pts',(-2.84857342775376,2.75000000213149,
6.66694304521659));
#103206=CARTESIAN_POINT('Ctrl Pts',(-2.98336477202329,2.72598918264424,
6.6093509695434));
#103207=CARTESIAN_POINT('Ctrl Pts',(-3.11607108096161,2.70215892424239,
6.54781146106226));
#103208=CARTESIAN_POINT('Ctrl Pts',(-3.24636485877381,2.67857142870499,
6.48256239523189));
#103209=CARTESIAN_POINT('Ctrl Pts',(-3.35101792035801,2.65962575324877,
6.43015379474618));
#103210=CARTESIAN_POINT('Ctrl Pts',(-3.45468713136439,2.64052352963869,
6.37506627208961));
#103211=CARTESIAN_POINT('Ctrl Pts',(-3.5571716164275,2.62129679689988,6.31735942346803));
#103212=CARTESIAN_POINT('Ctrl Pts',(-2.719030292,2.75,6.989769257));
#103213=CARTESIAN_POINT('Ctrl Pts',(-2.340268458,2.68564607,7.137108156));
#103214=CARTESIAN_POINT('Ctrl Pts',(-1.947803201,2.620518779,7.242655776));
#103215=CARTESIAN_POINT('Ctrl Pts',(-2.848573427,2.75,6.666943035));
#103216=CARTESIAN_POINT('Ctrl Pts',(-2.48730491,2.68564607,6.82130162));
#103217=CARTESIAN_POINT('Ctrl Pts',(-2.111472,2.620518779,6.93571813100001));
#103218=CARTESIAN_POINT('',(-2.11596137812195,2.62129679672014,6.93434979846242));
#103219=CARTESIAN_POINT('Origin',(0.0463559295408789,2.55361154041299,-0.190550696625532));
#103220=CARTESIAN_POINT('Ctrl Pts',(-2.18704476419214,2.6603606156681,7.17403897349229));
#103221=CARTESIAN_POINT('Ctrl Pts',(-2.17521933937601,2.65417293164464,
7.13404118248025));
#103222=CARTESIAN_POINT('Ctrl Pts',(-2.16337759060393,2.64782918798867,
7.09404668415066));
#103223=CARTESIAN_POINT('Ctrl Pts',(-2.13968810290276,2.63481931408485,
7.01416369986587));
#103224=CARTESIAN_POINT('Ctrl Pts',(-2.12782621669689,2.62814542050594,
6.97422750164678));
#103225=CARTESIAN_POINT('Ctrl Pts',(-2.11596138231027,2.62129679721111,
6.93434982010131));
#103226=CARTESIAN_POINT('Ctrl Pts',(-2.427657577,2.620519775,7.096229893));
#103227=CARTESIAN_POINT('Ctrl Pts',(-2.253019985,2.64969025,7.155974331));
#103228=CARTESIAN_POINT('Ctrl Pts',(-2.075654973,2.678571429,7.207056017));
#103229=CARTESIAN_POINT('Ctrl Pts',(-1.857631174,2.714073269,7.269847562));
#103230=CARTESIAN_POINT('Ctrl Pts',(-1.636210464,2.75,7.319345279));
#103231=CARTESIAN_POINT('Ctrl Pts',(-1.63218382487528,2.75065334439885,
7.32024541812365));
#103232=CARTESIAN_POINT('Ctrl Pts',(-1.62815718575056,2.7513066887977,7.3211455572473));
#103233=CARTESIAN_POINT('Ctrl Pts',(-2.120506944,2.620519775,6.93296115));
#103234=CARTESIAN_POINT('Ctrl Pts',(-1.949887382,2.64969025,6.98514663800001));
#103235=CARTESIAN_POINT('Ctrl Pts',(-1.776907359,2.678571429,7.028876172));
#103236=CARTESIAN_POINT('Ctrl Pts',(-1.564273757,2.714073269,7.082630172));
#103237=CARTESIAN_POINT('Ctrl Pts',(-1.348779684,2.75,7.123432695));
#103238=CARTESIAN_POINT('Ctrl Pts',(-1.34486082353981,2.75065334439885,
7.12417470795578));
#103239=CARTESIAN_POINT('Ctrl Pts',(-1.34094196307961,2.7513066887977,7.12491672091157));
#103240=CARTESIAN_POINT('Ctrl Pts',(-1.34877968337738,2.750000001968,7.12343270485655));
#103241=CARTESIAN_POINT('Ctrl Pts',(-1.49280027486478,2.7259891824288,7.09616325474652));
#103242=CARTESIAN_POINT('Ctrl Pts',(-1.63563315914257,2.7021589240906,7.06459043961242));
#103243=CARTESIAN_POINT('Ctrl Pts',(-1.77690736049493,2.67857142875836,
7.02887617166257));
#103244=CARTESIAN_POINT('Ctrl Pts',(-1.89037999086808,2.65962575344708,
7.0001901698149));
#103245=CARTESIAN_POINT('Ctrl Pts',(-2.0034676622742,2.64052352984786,6.96867637909595));
#103246=CARTESIAN_POINT('Ctrl Pts',(-2.11596138470524,2.62129679691545,
6.93434981992751));
#103247=CARTESIAN_POINT('Ctrl Pts',(-1.1528671,2.75,7.41086347500001));
#103248=CARTESIAN_POINT('Ctrl Pts',(-0.751286999,2.68564607,7.473335074));
#103249=CARTESIAN_POINT('Ctrl Pts',(-0.345307744,2.620518779,7.49204662));
#103250=CARTESIAN_POINT('Ctrl Pts',(-1.348779684,2.75,7.123432695));
#103251=CARTESIAN_POINT('Ctrl Pts',(-0.962774892000001,2.68564607,7.196520411));
#103252=CARTESIAN_POINT('Ctrl Pts',(-0.571132578,2.620518779,7.227468961));
#103253=CARTESIAN_POINT('',(-0.575811147881845,2.62129679676424,7.22709770249865));
#103254=CARTESIAN_POINT('Origin',(0.00430938273576355,2.55361156966043,
-0.196060777350408));
#103255=CARTESIAN_POINT('Ctrl Pts',(-0.593706556239983,2.66036061570601,
7.47646390483063));
#103256=CARTESIAN_POINT('Ctrl Pts',(-0.59075594627258,2.65417293169975,
7.43485912324236));
#103257=CARTESIAN_POINT('Ctrl Pts',(-0.587788686063486,2.64782918801413,
7.39325404795638));
#103258=CARTESIAN_POINT('Ctrl Pts',(-0.581825532548915,2.63481932848156,
7.31014623567884));
#103259=CARTESIAN_POINT('Ctrl Pts',(-0.578826069372865,2.62814542760037,
7.26859371970006));
#103260=CARTESIAN_POINT('Ctrl Pts',(-0.575811147992927,2.62129679730516,
7.22709772493138));
#103261=CARTESIAN_POINT('Ctrl Pts',(-0.845420628,2.620519775,7.452198599));
#103262=CARTESIAN_POINT('Ctrl Pts',(-0.662022678,2.64969025,7.473004326));
#103263=CARTESIAN_POINT('Ctrl Pts',(-0.477823308,2.678571429,7.484763516));
#103264=CARTESIAN_POINT('Ctrl Pts',(-0.251398459,2.714073269,7.499218357));
#103265=CARTESIAN_POINT('Ctrl Pts',(-0.024513896,2.75,7.499959938));
#103266=CARTESIAN_POINT('Ctrl Pts',(-0.0203878941541442,2.75065334439885,
7.49997342399717));
#103267=CARTESIAN_POINT('Ctrl Pts',(-0.0162618923082885,2.7513066887977,
7.49998690999434));
#103268=CARTESIAN_POINT('Ctrl Pts',(-0.58054896,2.620519775,7.226718682));
#103269=CARTESIAN_POINT('Ctrl Pts',(-0.40270005,2.64969025,7.24100594));
#103270=CARTESIAN_POINT('Ctrl Pts',(-0.224363648,2.678571429,7.24652751));
#103271=CARTESIAN_POINT('Ctrl Pts',(-0.00514578,2.714073269,7.253314833));
#103272=CARTESIAN_POINT('Ctrl Pts',(0.214081497,2.75,7.24683856));
#103273=CARTESIAN_POINT('Ctrl Pts',(0.218068247520193,2.75065334439885,
7.24672078594786));
#103274=CARTESIAN_POINT('Ctrl Pts',(0.222054998040385,2.7513066887977,7.24660301189572));
#103275=CARTESIAN_POINT('Ctrl Pts',(0.214081503589313,2.75000000123159,
7.2468385607603));
#103276=CARTESIAN_POINT('Ctrl Pts',(0.0675659067429764,2.72598918224881,
7.25116683047458));
#103277=CARTESIAN_POINT('Ctrl Pts',(-0.0787148477332593,2.70215892417189,
7.25103702132724));
#103278=CARTESIAN_POINT('Ctrl Pts',(-0.224363649566028,2.67857142874639,
7.24652750995151));
#103279=CARTESIAN_POINT('Ctrl Pts',(-0.341349993970045,2.6596257535192,
7.24290543231094));
#103280=CARTESIAN_POINT('Ctrl Pts',(-0.458568273036239,2.64052352972813,
7.23643892294451));
#103281=CARTESIAN_POINT('Ctrl Pts',(-0.575811149698002,2.6212967970204,
7.2270977247663));
#103282=CARTESIAN_POINT('Ctrl Pts',(-1.353502885,3.268101717,7.122536763));
#103283=CARTESIAN_POINT('Ctrl Pts',(-0.967849888,3.203647866,7.19582279300001));
#103284=CARTESIAN_POINT('Ctrl Pts',(-0.576538529,3.138525418,7.227039735));
#103285=CARTESIAN_POINT('Ctrl Pts',(-1.64106351,3.268101717,7.318258711));
#103286=CARTESIAN_POINT('Ctrl Pts',(-1.244813059,3.203647866,7.407114842));
#103287=CARTESIAN_POINT('Ctrl Pts',(-0.841285031,3.138525418,7.452666603));
#103288=CARTESIAN_POINT('',(-1.34892078812789,3.26733592570993,7.12340597604384));
#103289=CARTESIAN_POINT('Origin',(0.00747049262276644,3.08931098836207,
-0.196900007873446));
#103290=CARTESIAN_POINT('Ctrl Pts',(-1.39671106560661,3.22840426963636,
7.3687989657909));
#103291=CARTESIAN_POINT('Ctrl Pts',(-1.38863728046114,3.23458082925561,
7.32788102997847));
#103292=CARTESIAN_POINT('Ctrl Pts',(-1.38061063134402,3.24090849484843,
7.28695168322483));
#103293=CARTESIAN_POINT('Ctrl Pts',(-1.36468010339121,3.25387487492678,
7.20516874180313));
#103294=CARTESIAN_POINT('Ctrl Pts',(-1.35676670818485,3.26052132406272,
7.16426632904137));
#103295=CARTESIAN_POINT('Ctrl Pts',(-1.34892078979801,3.26733592512212,
7.12340597672159));
#103296=CARTESIAN_POINT('Ctrl Pts',(-2.116659292,3.138525418,6.93413682));
#103297=CARTESIAN_POINT('Ctrl Pts',(-1.894237241,3.176642188,7.002031601));
#103298=CARTESIAN_POINT('Ctrl Pts',(-1.667921256,3.214285714,7.055532488));
#103299=CARTESIAN_POINT('Ctrl Pts',(-1.506869744,3.241073689,7.093604914));
#103300=CARTESIAN_POINT('Ctrl Pts',(-1.344248775,3.268112745,7.124289104));
#103301=CARTESIAN_POINT('Ctrl Pts',(-1.953220126,3.138525418,7.241196803));
#103302=CARTESIAN_POINT('Ctrl Pts',(-1.720948701,3.176642188,7.30384904599999));
#103303=CARTESIAN_POINT('Ctrl Pts',(-1.485139566,3.214285714,7.351486956));
#103304=CARTESIAN_POINT('Ctrl Pts',(-1.317332516,3.241073689,7.385387158));
#103305=CARTESIAN_POINT('Ctrl Pts',(-1.148153419,3.268112745,7.411595221));
#103306=CARTESIAN_POINT('Ctrl Pts',(-2.11665928286731,3.13852541956508,
6.93413682278777));
#103307=CARTESIAN_POINT('Ctrl Pts',(-1.96799497161502,3.16400222517069,
6.97951690431297));
#103308=CARTESIAN_POINT('Ctrl Pts',(-1.81825525112624,3.18928040270946,
7.01999367228996));
#103309=CARTESIAN_POINT('Ctrl Pts',(-1.66792125646245,3.21428571392205,
7.05553248789925));
#103310=CARTESIAN_POINT('Ctrl Pts',(-1.56236435696929,3.23184317457392,
7.08048603968294));
#103311=CARTESIAN_POINT('Ctrl Pts',(-1.45597993658122,3.24953506289061,
7.10313276635206));
#103312=CARTESIAN_POINT('Ctrl Pts',(-1.34892078643843,3.26733592560455,
7.12340597794321));
#103313=CARTESIAN_POINT('Ctrl Pts',(-2.852993603,3.268101717,6.665052701));
#103314=CARTESIAN_POINT('Ctrl Pts',(-2.492111289,3.203647866,6.819529339));
#103315=CARTESIAN_POINT('Ctrl Pts',(-2.116659292,3.138525418,6.93413682));
#103316=CARTESIAN_POINT('Ctrl Pts',(-3.175905654,3.268101717,6.794381744));
#103317=CARTESIAN_POINT('Ctrl Pts',(-2.808020759,3.203647866,6.966342602));
#103318=CARTESIAN_POINT('Ctrl Pts',(-2.423719275,3.138525418,7.097575986));
#103319=CARTESIAN_POINT('',(-2.84870549026513,3.26733592567,6.66688660531189));
#103320=CARTESIAN_POINT('Origin',(0.0496234282582414,3.08931098430521,-0.190690422862081));
#103321=CARTESIAN_POINT('Ctrl Pts',(-2.94813069419871,3.22840426962259,
6.89626894829274));
#103322=CARTESIAN_POINT('Ctrl Pts',(-2.93144952302421,3.23458082924873,
6.85804327623306));
#103323=CARTESIAN_POINT('Ctrl Pts',(-2.91481193279318,3.24090849487191,
6.81979632704499));
#103324=CARTESIAN_POINT('Ctrl Pts',(-2.88167293465831,3.25387487579441,
6.74335001312293));
#103325=CARTESIAN_POINT('Ctrl Pts',(-2.86515174144485,3.26052132458631,
6.70510502432325));
#103326=CARTESIAN_POINT('Ctrl Pts',(-2.84870548936965,3.26733592513142,
6.66688660775784));
#103327=CARTESIAN_POINT('Ctrl Pts',(-3.557807419,3.138525418,6.31700137500001));
#103328=CARTESIAN_POINT('Ctrl Pts',(-3.355180843,3.176642188,6.43112298));
#103329=CARTESIAN_POINT('Ctrl Pts',(-3.145657109,3.214285714,6.532024292));
#103330=CARTESIAN_POINT('Ctrl Pts',(-2.996555338,3.241073689,6.603827921));
#103331=CARTESIAN_POINT('Ctrl Pts',(-2.84433255,3.268112745,6.668753433));
#103332=CARTESIAN_POINT('Ctrl Pts',(-3.46419819,3.138525418,6.652017055));
#103333=CARTESIAN_POINT('Ctrl Pts',(-3.250825521,3.176642188,6.763136014));
#103334=CARTESIAN_POINT('Ctrl Pts',(-3.030770215,3.214285714,6.86035217));
#103335=CARTESIAN_POINT('Ctrl Pts',(-2.874173942,3.241073689,6.929533359));
#103336=CARTESIAN_POINT('Ctrl Pts',(-2.714584117,3.268112745,6.991497198));
#103337=CARTESIAN_POINT('Ctrl Pts',(-3.55780740986131,3.13852541971911,
6.31700138014702));
#103338=CARTESIAN_POINT('Ctrl Pts',(-3.42237416380755,3.16400222531233,
6.39327893298748));
#103339=CARTESIAN_POINT('Ctrl Pts',(-3.28483658365421,3.18928040279562,
6.4649989898295));
#103340=CARTESIAN_POINT('Ctrl Pts',(-3.14565710871316,3.21428571404078,
6.53202429228031));
#103341=CARTESIAN_POINT('Ctrl Pts',(-3.04793235033307,3.23184317406293,
6.57908605590825));
#103342=CARTESIAN_POINT('Ctrl Pts',(-2.94890351649419,3.24953506217978,
6.62407281963628));
#103343=CARTESIAN_POINT('Ctrl Pts',(-2.84870549087026,3.26733592486962,
6.66688660706085));
#103344=CARTESIAN_POINT('Ctrl Pts',(-4.219081511,3.268101717,5.895918181));
#103345=CARTESIAN_POINT('Ctrl Pts',(-3.899844336,3.203647866,6.12436227200001));
#103346=CARTESIAN_POINT('Ctrl Pts',(-3.557807419,3.138525418,6.317001375));
#103347=CARTESIAN_POINT('Ctrl Pts',(-4.562245979,3.268101717,5.952807038));
#103348=CARTESIAN_POINT('Ctrl Pts',(-4.23992853,3.203647866,6.199831924));
#103349=CARTESIAN_POINT('Ctrl Pts',(-3.892823099,3.138525418,6.410610604));
#103350=CARTESIAN_POINT('',(-4.21528788507473,3.26733592572405,5.89863103008845));
#103351=CARTESIAN_POINT('Origin',(0.0894560049937093,3.08931096832741,-0.175564515937652));
#103352=CARTESIAN_POINT('Ctrl Pts',(-4.3616990090963,3.22840426965525,6.10127705919986));
#103353=CARTESIAN_POINT('Ctrl Pts',(-4.3371904445687,3.23458082933408,6.06753104051369));
#103354=CARTESIAN_POINT('Ctrl Pts',(-4.31271986853268,3.24090849489276,
6.03375487412336));
#103355=CARTESIAN_POINT('Ctrl Pts',(-4.26392214546335,3.2538748222234,5.96622001644638));
#103356=CARTESIAN_POINT('Ctrl Pts',(-4.23956555893764,3.26052129816919,
5.93242059420358));
#103357=CARTESIAN_POINT('Ctrl Pts',(-4.21528788745792,3.26733592508906,
5.89863103001385));
#103358=CARTESIAN_POINT('Ctrl Pts',(-4.832596425,3.138525418,5.404489966));
#103359=CARTESIAN_POINT('Ctrl Pts',(-4.659239917,3.176642188,5.559502196));
#103360=CARTESIAN_POINT('Ctrl Pts',(-4.476305531,3.214285714,5.703085901));
#103361=CARTESIAN_POINT('Ctrl Pts',(-4.346125334,3.241073689,5.805263274));
#103362=CARTESIAN_POINT('Ctrl Pts',(-4.211418497,3.268112745,5.901394263));
#103363=CARTESIAN_POINT('Ctrl Pts',(-4.813194196,3.138525418,5.751796383));
#103364=CARTESIAN_POINT('Ctrl Pts',(-4.628697353,3.176642188,5.906186259));
#103365=CARTESIAN_POINT('Ctrl Pts',(-4.434685418,3.214285714,6.048434942));
#103366=CARTESIAN_POINT('Ctrl Pts',(-4.29662219,3.241073689,6.149662283));
#103367=CARTESIAN_POINT('Ctrl Pts',(-4.15408388,3.268112745,6.244484536));
#103368=CARTESIAN_POINT('Ctrl Pts',(-4.83259641748162,3.13852541965311,
5.4044899727228));
#103369=CARTESIAN_POINT('Ctrl Pts',(-4.71672694397057,3.1640022253197,5.50809834390426));
#103370=CARTESIAN_POINT('Ctrl Pts',(-4.59782260794536,3.1892804028295,5.60770814008636));
#103371=CARTESIAN_POINT('Ctrl Pts',(-4.47630553135839,3.21428571392579,
5.70308590073554));
#103372=CARTESIAN_POINT('Ctrl Pts',(-4.39098240876368,3.23184317448963,
5.77005532255571));
#103373=CARTESIAN_POINT('Ctrl Pts',(-4.30393963736397,3.24953506284712,
5.83527859361555));
#103374=CARTESIAN_POINT('Ctrl Pts',(-4.21528788457339,3.26733592566267,
5.89863103222262));
#103375=CARTESIAN_POINT('Ctrl Pts',(-5.387889857,3.268101717,4.851097081));
#103376=CARTESIAN_POINT('Ctrl Pts',(-5.125224996,3.203647866,5.142826832));
#103377=CARTESIAN_POINT('Ctrl Pts',(-4.83259642500001,3.138525418,5.404489966));
#103378=CARTESIAN_POINT('Ctrl Pts',(-5.735260753,3.268101717,4.832885691));
#103379=CARTESIAN_POINT('Ctrl Pts',(-5.47358195600001,3.203647866,5.143423997));
#103380=CARTESIAN_POINT('Ctrl Pts',(-5.179902842,3.138525418,5.423892195));
#103381=CARTESIAN_POINT('',(-5.38476810601465,3.26733592571324,4.85456202254636));
#103382=CARTESIAN_POINT('Origin',(0.125105784914014,3.08931094753363,-0.152229559399517));
#103383=CARTESIAN_POINT('Ctrl Pts',(-5.57131912513468,3.22840426958941,
5.02099623658913));
#103384=CARTESIAN_POINT('Ctrl Pts',(-5.54012916105509,3.2345808292255,4.99330779814539));
#103385=CARTESIAN_POINT('Ctrl Pts',(-5.50896981606804,3.24090849483476,
4.96558175001598));
#103386=CARTESIAN_POINT('Ctrl Pts',(-5.44679470544814,3.25387487499183,
4.9101156618356));
#103387=CARTESIAN_POINT('Ctrl Pts',(-5.41574182084466,3.26052132410651,
4.88234251745498));
#103388=CARTESIAN_POINT('Ctrl Pts',(-5.38476810759784,3.26733592515923,
4.85456202178235));
#103389=CARTESIAN_POINT('Ctrl Pts',(-5.881418593,3.138525418,4.239270613));
#103390=CARTESIAN_POINT('Ctrl Pts',(-5.745438112,3.176642188,4.427925268));
#103391=CARTESIAN_POINT('Ctrl Pts',(-5.597646882,3.214285714,4.607477551));
#103392=CARTESIAN_POINT('Ctrl Pts',(-5.492475341,3.241073689,4.73525096800001));
#103393=CARTESIAN_POINT('Ctrl Pts',(-5.381583195,3.268112745,4.858092456));
#103394=CARTESIAN_POINT('Ctrl Pts',(-5.937130591,3.138525418,4.582628105));
#103395=CARTESIAN_POINT('Ctrl Pts',(-5.790136441,3.176642188,4.773069799));
#103396=CARTESIAN_POINT('Ctrl Pts',(-5.631239659,3.214285714,4.953699618));
#103397=CARTESIAN_POINT('Ctrl Pts',(-5.518165158,3.241073689,5.082239832));
#103398=CARTESIAN_POINT('Ctrl Pts',(-5.399343297,3.268112745,5.20548671700001));
#103399=CARTESIAN_POINT('Ctrl Pts',(-5.88141858688418,3.13852541971433,
4.23927062148488));
#103400=CARTESIAN_POINT('Ctrl Pts',(-5.79053081512884,3.16400222534549,
4.36536519804455));
#103401=CARTESIAN_POINT('Ctrl Pts',(-5.69581955833051,3.18928040283087,
4.48820708978384));
#103402=CARTESIAN_POINT('Ctrl Pts',(-5.59764688247275,3.21428571388678,
4.60747755075093));
#103403=CARTESIAN_POINT('Ctrl Pts',(-5.52871501357167,3.23184317443036,
4.69122321399006));
#103404=CARTESIAN_POINT('Ctrl Pts',(-5.45772832847149,3.24953506289523,
4.77363322429347));
#103405=CARTESIAN_POINT('Ctrl Pts',(-5.38476810582414,3.26733592560558,
4.85456202488883));
#103406=CARTESIAN_POINT('Ctrl Pts',(-6.304766461,3.268101717,3.579444073));
#103407=CARTESIAN_POINT('Ctrl Pts',(-6.110955831,3.203647866,3.920818525));
#103408=CARTESIAN_POINT('Ctrl Pts',(-5.881418593,3.138525418,4.239270613));
#103409=CARTESIAN_POINT('Ctrl Pts',(-6.640101108,3.268101717,3.48698398));
#103410=CARTESIAN_POINT('Ctrl Pts',(-6.45129677200001,3.203647866,3.846515279));
#103411=CARTESIAN_POINT('Ctrl Pts',(-6.224776085,3.138525418,4.183558616));
#103412=CARTESIAN_POINT('',(-6.30246255512824,3.26733592574253,3.58349909006738));
#103413=CARTESIAN_POINT('Origin',(0.154905874552772,3.08931093362247,-0.121776565780059));
#103414=CARTESIAN_POINT('Ctrl Pts',(-6.52043055152078,3.22840426961869,
3.70593920925317));
#103415=CARTESIAN_POINT('Ctrl Pts',(-6.4840175953753,3.23458082929635,3.68560303135103));
#103416=CARTESIAN_POINT('Ctrl Pts',(-6.44762645791188,3.24090849487083,
3.66522354115463));
#103417=CARTESIAN_POINT('Ctrl Pts',(-6.37498139769519,3.25387487497803,
3.62442003059789));
#103418=CARTESIAN_POINT('Ctrl Pts',(-6.3386841072753,3.2605213240895,3.60397165931456));
#103419=CARTESIAN_POINT('Ctrl Pts',(-6.30246255720574,3.26733592512396,
3.58349908911351));
#103420=CARTESIAN_POINT('Ctrl Pts',(-6.655232165,3.138525418,2.875827678));
#103421=CARTESIAN_POINT('Ctrl Pts',(-6.562986005,3.176642188,3.089303476));
#103422=CARTESIAN_POINT('Ctrl Pts',(-6.457248486,3.214285714,3.296428672));
#103423=CARTESIAN_POINT('Ctrl Pts',(-6.382003305,3.241073689,3.44382359));
#103424=CARTESIAN_POINT('Ctrl Pts',(-6.30011104500001,3.268112745,3.587631646));
#103425=CARTESIAN_POINT('Ctrl Pts',(-6.783453358,3.138525418,3.19918123));
#103426=CARTESIAN_POINT('Ctrl Pts',(-6.680835185,3.176642188,3.4167699));
#103427=CARTESIAN_POINT('Ctrl Pts',(-6.564483393,3.214285714,3.627334805));
#103428=CARTESIAN_POINT('Ctrl Pts',(-6.481684858,3.241073689,3.777177496));
#103429=CARTESIAN_POINT('Ctrl Pts',(-6.392135422,3.268112745,3.923086125));
#103430=CARTESIAN_POINT('Ctrl Pts',(-6.65523216073996,3.13852541976028,
2.87582768785858));
#103431=CARTESIAN_POINT('Ctrl Pts',(-6.59357590057777,3.16400222528848,
3.01851242710704));
#103432=CARTESIAN_POINT('Ctrl Pts',(-6.52748631577757,3.18928040276481,
3.15884246419534));
#103433=CARTESIAN_POINT('Ctrl Pts',(-6.45724848623745,3.21428571391547,
3.29642867153488));
#103434=CARTESIAN_POINT('Ctrl Pts',(-6.40793104801386,3.23184317453693,
3.39303472214997));
#103435=CARTESIAN_POINT('Ctrl Pts',(-6.35631970871314,3.24953506296906,
3.48877807130775));
#103436=CARTESIAN_POINT('Ctrl Pts',(-6.30246255541806,3.26733592572747,
3.583499092464));
#103437=CARTESIAN_POINT('Ctrl Pts',(-6.926839193,3.268101717,2.140420238));
#103438=CARTESIAN_POINT('Ctrl Pts',(-6.810945164,3.203647866,2.515477101));
#103439=CARTESIAN_POINT('Ctrl Pts',(-6.655232165,3.138525418,2.875827678));
#103440=CARTESIAN_POINT('Ctrl Pts',(-7.234457715,3.268101717,1.978034774));
#103441=CARTESIAN_POINT('Ctrl Pts',(-7.127356121,3.203647866,2.369747783));
#103442=CARTESIAN_POINT('Ctrl Pts',(-6.978585717,3.138525418,2.747606485));
#103443=CARTESIAN_POINT('',(-6.92546085991525,3.26733592573375,2.14487572253998));
#103444=CARTESIAN_POINT('Origin',(0.177462766279987,3.08931095639599,-0.0856293580043394));
#103445=CARTESIAN_POINT('Ctrl Pts',(-7.16465389175981,3.22840426965055,
2.21759658398079));
#103446=CARTESIAN_POINT('Ctrl Pts',(-7.12472057319778,3.23458082930576,
2.20556356384048));
#103447=CARTESIAN_POINT('Ctrl Pts',(-7.08479925237754,3.24090849485858,
2.19348355363704));
#103448=CARTESIAN_POINT('Ctrl Pts',(-7.0050810446984,3.25387487495275,2.16925054701254));
#103449=CARTESIAN_POINT('Ctrl Pts',(-6.96523656935363,3.26052132407379,
2.15708309174497));
#103450=CARTESIAN_POINT('Ctrl Pts',(-6.92546086156653,3.26733592512786,
2.14487572139872));
#103451=CARTESIAN_POINT('Ctrl Pts',(-7.117854477,3.138525418,1.377914237));
#103452=CARTESIAN_POINT('Ctrl Pts',(-7.073655968,3.176642188,1.606229286));
#103453=CARTESIAN_POINT('Ctrl Pts',(-7.014916327,3.214285714,1.831242452));
#103454=CARTESIAN_POINT('Ctrl Pts',(-6.973115887,3.241073689,1.991366848));
#103455=CARTESIAN_POINT('Ctrl Pts',(-6.92405270400001,3.268112745,2.149417167));
#103456=CARTESIAN_POINT('Ctrl Pts',(-7.312589385,3.138525418,1.666144196));
#103457=CARTESIAN_POINT('Ctrl Pts',(-7.2591455,3.176642188,1.900705638));
#103458=CARTESIAN_POINT('Ctrl Pts',(-7.190779179,3.214285714,2.131359848));
#103459=CARTESIAN_POINT('Ctrl Pts',(-7.142128177,3.241073689,2.295498538));
#103460=CARTESIAN_POINT('Ctrl Pts',(-7.086038399,3.268112745,2.457246386));
#103461=CARTESIAN_POINT('Ctrl Pts',(-7.11785447504281,3.13852541968788,
1.3779142471102));
#103462=CARTESIAN_POINT('Ctrl Pts',(-7.08831270552661,3.16400222537653,
1.53051737006383));
#103463=CARTESIAN_POINT('Ctrl Pts',(-7.05393506819967,3.18928040286292,
1.68177387602203));
#103464=CARTESIAN_POINT('Ctrl Pts',(-7.01491632751934,3.21428571383937,
1.83124245149837));
#103465=CARTESIAN_POINT('Ctrl Pts',(-6.98751934921584,3.23184317436136,
1.93619169720647));
#103466=CARTESIAN_POINT('Ctrl Pts',(-6.95769664389279,3.24953506294541,
2.04079153279387));
#103467=CARTESIAN_POINT('Ctrl Pts',(-6.92546086076598,3.26733592567063,
2.14487572491838));
#103468=CARTESIAN_POINT('Ctrl Pts',(-7.225020623,3.268101717,0.601312732));
#103469=CARTESIAN_POINT('Ctrl Pts',(-7.192462271,3.203647866,0.992514764));
#103470=CARTESIAN_POINT('Ctrl Pts',(-7.117854477,3.138525418,1.377914237));
#103471=CARTESIAN_POINT('Ctrl Pts',(-7.49053912000001,3.268101717,0.376594861));
#103472=CARTESIAN_POINT('Ctrl Pts',(-7.47014822,3.203647866,0.782173513));
#103473=CARTESIAN_POINT('Ctrl Pts',(-7.406084436,3.138525418,1.183179329));
#103474=CARTESIAN_POINT('',(-7.22463231197984,3.26733592574723,0.605960350813484));
#103475=CARTESIAN_POINT('Origin',(0.191721488831114,3.08931097958864,-0.0454781312283063));
#103476=CARTESIAN_POINT('Ctrl Pts',(-7.47386597901678,3.22840426959478,
0.625561607462148));
#103477=CARTESIAN_POINT('Ctrl Pts',(-7.43227953574014,3.23458082926715,
0.622394395629625));
#103478=CARTESIAN_POINT('Ctrl Pts',(-7.39069470803807,3.24090849486445,
0.619178713171061));
#103479=CARTESIAN_POINT('Ctrl Pts',(-7.30763088765172,3.25387487500532,
0.612649318894864));
#103480=CARTESIAN_POINT('Ctrl Pts',(-7.26610231080442,3.26052132413581,
0.609331716384318));
#103481=CARTESIAN_POINT('Ctrl Pts',(-7.22463231304457,3.2673359252016,0.605960349082846));
#103482=CARTESIAN_POINT('Ctrl Pts',(-7.247653825,3.138525418,-0.184428943));
#103483=CARTESIAN_POINT('Ctrl Pts',(-7.25356963899999,3.176642188,0.048049601));
#103484=CARTESIAN_POINT('Ctrl Pts',(-7.244574478,3.214285714,0.28042937));
#103485=CARTESIAN_POINT('Ctrl Pts',(-7.238173321,3.241073689,0.445796006));
#103486=CARTESIAN_POINT('Ctrl Pts',(-7.224233354,3.268112745,0.61069833));
#103487=CARTESIAN_POINT('Ctrl Pts',(-7.49979686,3.138525418,0.055200111));
#103488=CARTESIAN_POINT('Ctrl Pts',(-7.49802624,3.176642188,0.295766492));
#103489=CARTESIAN_POINT('Ctrl Pts',(-7.480842122,3.214285714,0.535724874));
#103490=CARTESIAN_POINT('Ctrl Pts',(-7.46861352000001,3.241073689,0.706484620000001));
#103491=CARTESIAN_POINT('Ctrl Pts',(-7.448606097,3.268112745,0.876508537));
#103492=CARTESIAN_POINT('Ctrl Pts',(-7.24765382527071,3.13852541974422,
-0.184428932361817));
#103493=CARTESIAN_POINT('Ctrl Pts',(-7.25160788627811,3.16400222524267,
-0.0290429788910136));
#103494=CARTESIAN_POINT('Ctrl Pts',(-7.25054965684747,3.18928040272498,
0.126067409913584));
#103495=CARTESIAN_POINT('Ctrl Pts',(-7.24457447826883,3.21428571386402,
0.28042936941594));
#103496=CARTESIAN_POINT('Ctrl Pts',(-7.24037901156516,3.23184317446808,
0.38881450124409));
#103497=CARTESIAN_POINT('Ctrl Pts',(-7.23373941729894,3.24953506294951,
0.497379850505409));
#103498=CARTESIAN_POINT('Ctrl Pts',(-7.2246323132945,3.26733592571272,0.605960352805634));
#103499=CARTESIAN_POINT('Ctrl Pts',(-7.18536811800001,3.268101717,-0.96591149));
#103500=CARTESIAN_POINT('Ctrl Pts',(-7.237667836,3.203647866,-0.57685646));
#103501=CARTESIAN_POINT('Ctrl Pts',(-7.247653825,3.138525418,-0.184428943));
#103502=CARTESIAN_POINT('Ctrl Pts',(-7.396371241,3.268101717,-1.24245421));
#103503=CARTESIAN_POINT('Ctrl Pts',(-7.46364449,3.203647866,-0.84197432));
#103504=CARTESIAN_POINT('Ctrl Pts',(-7.487282879,3.138525418,-0.436571978));
#103505=CARTESIAN_POINT('',(-7.18598798619975,3.26733592573614,-0.961289054106258));
#103506=CARTESIAN_POINT('Origin',(0.197015451307481,3.08931093639002,-0.00320043798352432));
#103507=CARTESIAN_POINT('Ctrl Pts',(-7.43360839986677,3.22840426960252,
-0.995723935096498));
#103508=CARTESIAN_POINT('Ctrl Pts',(-7.39231336740992,3.23458082928339,
-0.989877243158041));
#103509=CARTESIAN_POINT('Ctrl Pts',(-7.35100949329422,3.24090849484591,
-0.984078236009551));
#103510=CARTESIAN_POINT('Ctrl Pts',(-7.26848403180813,3.25387487499032,
-0.972598710641352));
#103511=CARTESIAN_POINT('Ctrl Pts',(-7.22721318341613,3.26052132411662,
-0.966911333061405));
#103512=CARTESIAN_POINT('Ctrl Pts',(-7.18598798673272,3.26733592517209,
-0.961289056132491));
#103513=CARTESIAN_POINT('Ctrl Pts',(-7.038560935,3.138525418,-1.73814843));
#103514=CARTESIAN_POINT('Ctrl Pts',(-7.094314455,3.176642188,-1.51237683));
#103515=CARTESIAN_POINT('Ctrl Pts',(-7.135484378,3.214285714,-1.283496277));
#103516=CARTESIAN_POINT('Ctrl Pts',(-7.164781814,3.241073689,-1.120619762));
#103517=CARTESIAN_POINT('Ctrl Pts',(-7.18661688100001,3.268112745,-0.956576082));
#103518=CARTESIAN_POINT('Ctrl Pts',(-7.33632217,3.138525418,-1.558325069));
#103519=CARTESIAN_POINT('Ctrl Pts',(-7.386307607,3.176642188,-1.323002365));
#103520=CARTESIAN_POINT('Ctrl Pts',(-7.421109203,3.214285714,-1.08496));
#103521=CARTESIAN_POINT('Ctrl Pts',(-7.445874796,3.241073689,-0.915563734));
#103522=CARTESIAN_POINT('Ctrl Pts',(-7.462885252,3.268112745,-0.745213877));
#103523=CARTESIAN_POINT('Ctrl Pts',(-7.03856093736968,3.13852541962007,
-1.73814842040409));
#103524=CARTESIAN_POINT('Ctrl Pts',(-7.07582594128906,3.16400222522755,
-1.58724530956614));
#103525=CARTESIAN_POINT('Ctrl Pts',(-7.10813660163031,3.18928040274743,
-1.43553382686493));
#103526=CARTESIAN_POINT('Ctrl Pts',(-7.13548437796271,3.21428571388022,
-1.28349627766317));
#103527=CARTESIAN_POINT('Ctrl Pts',(-7.15468659746866,3.23184317448197,
-1.17674322920128));
#103528=CARTESIAN_POINT('Ctrl Pts',(-7.17154057430262,3.24953506288593,
-1.06928876128343));
#103529=CARTESIAN_POINT('Ctrl Pts',(-7.18598798786616,3.26733592567761,
-0.961289052512922));
#103530=CARTESIAN_POINT('Ctrl Pts',(-6.80973578600001,3.268101717,-2.487970763));
#103531=CARTESIAN_POINT('Ctrl Pts',(-6.944448097,3.203647866,-2.119254517));
#103532=CARTESIAN_POINT('Ctrl Pts',(-7.038560935,3.138525418,-1.73814843));
#103533=CARTESIAN_POINT('Ctrl Pts',(-6.956357263,3.268101717,-2.803407502));
#103534=CARTESIAN_POINT('Ctrl Pts',(-7.108149039,3.203647866,-2.42675237));
#103535=CARTESIAN_POINT('Ctrl Pts',(-7.218384296,3.138525418,-2.035909664));
#103536=CARTESIAN_POINT('',(-6.81133484954207,3.26733592570866,-2.48358965115484));
#103537=CARTESIAN_POINT('Origin',(0.193097258795751,3.08931093160372,0.0392268551923727));
#103538=CARTESIAN_POINT('Ctrl Pts',(-7.04576355357133,3.22840426963018,
-2.5704505328325));
#103539=CARTESIAN_POINT('Ctrl Pts',(-7.00669084204283,3.23458082930848,
-2.55586332204927));
#103540=CARTESIAN_POINT('Ctrl Pts',(-6.96759924474046,3.24090849486114,
-2.54132078042704));
#103541=CARTESIAN_POINT('Ctrl Pts',(-6.88947094156835,3.25387487495917,
-2.51236910518395));
#103542=CARTESIAN_POINT('Ctrl Pts',(-6.85038760072907,3.26052132408289,
-2.49794268283183));
#103543=CARTESIAN_POINT('Ctrl Pts',(-6.81133484970225,3.26733592511703,
-2.48358965305668));
#103544=CARTESIAN_POINT('Ctrl Pts',(-6.50035275900001,3.138525418,-3.210594028));
#103545=CARTESIAN_POINT('Ctrl Pts',(-6.60333701300001,3.176642188,-3.002086202));
#103546=CARTESIAN_POINT('Ctrl Pts',(-6.692746959,3.214285714,-2.787407065));
#103547=CARTESIAN_POINT('Ctrl Pts',(-6.756373074,3.241073689,-2.634636595));
#103548=CARTESIAN_POINT('Ctrl Pts',(-6.812962191,3.268112745,-2.479122059));
#103549=CARTESIAN_POINT('Ctrl Pts',(-6.829809208,3.138525418,-3.098984701));
#103550=CARTESIAN_POINT('Ctrl Pts',(-6.929213439,3.176642188,-2.879909103));
#103551=CARTESIAN_POINT('Ctrl Pts',(-7.014373465,3.214285714,-2.65491335));
#103552=CARTESIAN_POINT('Ctrl Pts',(-7.074975242,3.241073689,-2.494801346));
#103553=CARTESIAN_POINT('Ctrl Pts',(-7.128208186,3.268112745,-2.332090918));
#103554=CARTESIAN_POINT('Ctrl Pts',(-6.50035276356033,3.13852541968788,
-3.2105940187669));
#103555=CARTESIAN_POINT('Ctrl Pts',(-6.56918624068039,3.16400222532293,
-3.07122981342278));
#103556=CARTESIAN_POINT('Ctrl Pts',(-6.63335497953997,3.18928040281912,
-2.93001109800961));
#103557=CARTESIAN_POINT('Ctrl Pts',(-6.69274695865615,3.21428571385523,
-2.78740706582561));
#103558=CARTESIAN_POINT('Ctrl Pts',(-6.73444899117437,3.23184317440716,
-2.68727775405561));
#103559=CARTESIAN_POINT('Ctrl Pts',(-6.77400846551075,3.24953506287852,
-2.58595861844934));
#103560=CARTESIAN_POINT('Ctrl Pts',(-6.81133485153371,3.26733592560304,
-2.48358964988351));
#103561=CARTESIAN_POINT('Ctrl Pts',(-6.115687778,3.268101717,-3.893695289));
#103562=CARTESIAN_POINT('Ctrl Pts',(-6.326513683,3.203647866,-3.562558589));
#103563=CARTESIAN_POINT('Ctrl Pts',(-6.50035275900001,3.138525418,-3.210594028));
#103564=CARTESIAN_POINT('Ctrl Pts',(-6.191071751,3.268101717,-4.233276576));
#103565=CARTESIAN_POINT('Ctrl Pts',(-6.42028444,3.203647866,-3.898058176));
#103566=CARTESIAN_POINT('Ctrl Pts',(-6.61196208500001,3.138525418,-3.540050477));
#103567=CARTESIAN_POINT('',(-6.11819126500725,3.26733592574228,-3.88976035605099));
#103568=CARTESIAN_POINT('Origin',(0.180150236425488,3.08931097286523,0.0798200253232612));
#103569=CARTESIAN_POINT('Ctrl Pts',(-6.32846663464854,3.22840426962889,
-4.02498572048465));
#103570=CARTESIAN_POINT('Ctrl Pts',(-6.29344324060942,3.23458082928833,
-4.00234007261691));
#103571=CARTESIAN_POINT('Ctrl Pts',(-6.25839179944015,3.24090849488502,
-3.97973398944361));
#103572=CARTESIAN_POINT('Ctrl Pts',(-6.18831384716743,3.25387487495712,
-3.93466391254327));
#103573=CARTESIAN_POINT('Ctrl Pts',(-6.15324550754099,3.2605213240867,-3.91217300887544));
#103574=CARTESIAN_POINT('Ctrl Pts',(-6.11819126540562,3.26733592513327,
-3.88976035782639));
#103575=CARTESIAN_POINT('Ctrl Pts',(-5.658195312,3.138525418,-4.532915818));
#103576=CARTESIAN_POINT('Ctrl Pts',(-5.803594871,3.176642188,-4.351421359));
#103577=CARTESIAN_POINT('Ctrl Pts',(-5.93706413,3.214285714,-4.160981797));
#103578=CARTESIAN_POINT('Ctrl Pts',(-6.032043837,3.241073689,-4.025460749));
#103579=CARTESIAN_POINT('Ctrl Pts',(-6.120740961,3.268112745,-3.885747044));
#103580=CARTESIAN_POINT('Ctrl Pts',(-6.003941959,3.138525418,-4.494739253));
#103581=CARTESIAN_POINT('Ctrl Pts',(-6.14811695100001,3.176642188,-4.302154492));
#103582=CARTESIAN_POINT('Ctrl Pts',(-6.279653419,3.214285714,-4.100725903));
#103583=CARTESIAN_POINT('Ctrl Pts',(-6.373257709,3.241073689,-3.957384819));
#103584=CARTESIAN_POINT('Ctrl Pts',(-6.460224029,3.268112745,-3.80992198));
#103585=CARTESIAN_POINT('Ctrl Pts',(-5.65819531856153,3.13852541972012,
-4.53291580980959));
#103586=CARTESIAN_POINT('Ctrl Pts',(-5.7553786917797,3.16400222526261,-4.41160702510859));
#103587=CARTESIAN_POINT('Ctrl Pts',(-5.84840505051902,3.18928040275261,
-4.28748430692079));
#103588=CARTESIAN_POINT('Ctrl Pts',(-5.93706412966269,3.21428571390487,
-4.16098179748129));
#103589=CARTESIAN_POINT('Ctrl Pts',(-5.99931603428507,3.23184317451593,
-4.07215815694336));
#103590=CARTESIAN_POINT('Ctrl Pts',(-6.05973124909473,3.24953506284523,
-3.98171192458526));
#103591=CARTESIAN_POINT('Ctrl Pts',(-6.11819126715086,3.26733592561034,
-3.8897603553223));
#103592=CARTESIAN_POINT('Ctrl Pts',(-5.135677006,3.268101717,-5.117354951));
#103593=CARTESIAN_POINT('Ctrl Pts',(-5.41275852000001,3.203647866,-4.83928138000001));
#103594=CARTESIAN_POINT('Ctrl Pts',(-5.658195312,3.138525418,-4.532915818));
#103595=CARTESIAN_POINT('Ctrl Pts',(-5.136298605,3.268101717,-5.465202342));
#103596=CARTESIAN_POINT('Ctrl Pts',(-5.432214475,3.203647866,-5.187095114));
#103597=CARTESIAN_POINT('Ctrl Pts',(-5.696371877,3.138525418,-4.878662465));
#103598=CARTESIAN_POINT('',(-5.13896785769969,3.26733592570463,-5.11405019018087));
#103599=CARTESIAN_POINT('Origin',(0.15877957359841,3.08931098806011,0.116680933289348));
#103600=CARTESIAN_POINT('Ctrl Pts',(-5.31525764932106,3.2284042696144,-5.29131704928888));
#103601=CARTESIAN_POINT('Ctrl Pts',(-5.28592122767291,3.23458082926818,
-5.2616718497513));
#103602=CARTESIAN_POINT('Ctrl Pts',(-5.25654890943951,3.24090849485085,
-5.23205926065519));
#103603=CARTESIAN_POINT('Ctrl Pts',(-5.19779807493308,3.25387487494942,
-5.17297820876393));
#103604=CARTESIAN_POINT('Ctrl Pts',(-5.16838449306854,3.26052132408546,
-5.14347447343562));
#103605=CARTESIAN_POINT('Ctrl Pts',(-5.13896785708805,3.26733592514502,
-5.11405019156049));
#103606=CARTESIAN_POINT('Ctrl Pts',(-4.551466941,3.138525418,-5.643283502));
#103607=CARTESIAN_POINT('Ctrl Pts',(-4.732483083,3.176642188,-5.49728889));
#103608=CARTESIAN_POINT('Ctrl Pts',(-4.903770781,3.214285714,-5.339993645));
#103609=CARTESIAN_POINT('Ctrl Pts',(-5.025662935,3.241073689,-5.228058833));
#103610=CARTESIAN_POINT('Ctrl Pts',(-5.142320686,3.268112745,-5.110678816));
#103611=CARTESIAN_POINT('Ctrl Pts',(-4.897337056,3.138525418,-5.680324793));
#103612=CARTESIAN_POINT('Ctrl Pts',(-5.079541349,3.176642188,-5.523235918));
#103613=CARTESIAN_POINT('Ctrl Pts',(-5.251303759,3.214285714,-5.35479307));
#103614=CARTESIAN_POINT('Ctrl Pts',(-5.373533729,3.241073689,-5.234925376));
#103615=CARTESIAN_POINT('Ctrl Pts',(-5.490166976,3.268112745,-5.109605325));
#103616=CARTESIAN_POINT('Ctrl Pts',(-4.55146694901572,3.13852541968788,
-5.64328349553509));
#103617=CARTESIAN_POINT('Ctrl Pts',(-4.67245603173969,3.16400222519247,
-5.54570239561382));
#103618=CARTESIAN_POINT('Ctrl Pts',(-4.78999020139523,3.18928040269112,
-5.44447951512049));
#103619=CARTESIAN_POINT('Ctrl Pts',(-4.90377078064891,3.21428571390971,
-5.33999364537984));
#103620=CARTESIAN_POINT('Ctrl Pts',(-4.98366172793508,3.23184317458137,
-5.26662897113917));
#103621=CARTESIAN_POINT('Ctrl Pts',(-5.06210773487276,3.24953506279931,
-5.19128480698234));
#103622=CARTESIAN_POINT('Ctrl Pts',(-5.13896786002726,3.26733592552427,
-5.11405018991181));
#103623=CARTESIAN_POINT('Ctrl Pts',(-3.915527685,3.268101717,-6.101732783));
#103624=CARTESIAN_POINT('Ctrl Pts',(-4.245908786,3.203647866,-5.889724753));
#103625=CARTESIAN_POINT('Ctrl Pts',(-4.551466941,3.138525418,-5.643283502));
#103626=CARTESIAN_POINT('Ctrl Pts',(-3.841357845,3.268101717,-6.44158132));
#103627=CARTESIAN_POINT('Ctrl Pts',(-4.190140199,3.203647866,-6.23358925));
#103628=CARTESIAN_POINT('Ctrl Pts',(-4.51442565,3.138525418,-5.989153617));
#103629=CARTESIAN_POINT('',(-3.91945202400498,3.26733592572801,-6.09921272121348));
#103630=CARTESIAN_POINT('Origin',(0.129984324620748,3.08931095259013,0.148085736451091));
#103631=CARTESIAN_POINT('Ctrl Pts',(-4.05351312369227,3.22840426964832,
-6.31023227389369));
#103632=CARTESIAN_POINT('Ctrl Pts',(-4.0312354129448,3.23458082931858,-6.27497369893178));
#103633=CARTESIAN_POINT('Ctrl Pts',(-4.00891563470743,3.24090849486757,
-6.23973925566169));
#103634=CARTESIAN_POINT('Ctrl Pts',(-3.96423904174856,3.25387487499089,
-6.16940979302766));
#103635=CARTESIAN_POINT('Ctrl Pts',(-3.9418555640506,3.26052132411323,-6.13427278810945));
#103636=CARTESIAN_POINT('Ctrl Pts',(-3.91945202338612,3.26733592516335,
-6.09921272249568));
#103637=CARTESIAN_POINT('Ctrl Pts',(-3.231917035,3.138525418,-6.489777522));
#103638=CARTESIAN_POINT('Ctrl Pts',(-3.440085645,3.176642188,-6.386109302));
#103639=CARTESIAN_POINT('Ctrl Pts',(-3.641182561,3.214285714,-6.269313324));
#103640=CARTESIAN_POINT('Ctrl Pts',(-3.78428762,3.241073689,-6.18619869600001));
#103641=CARTESIAN_POINT('Ctrl Pts',(-3.923451211,3.268112745,-6.096640927));
#103642=CARTESIAN_POINT('Ctrl Pts',(-3.561738116,3.138525418,-6.600304659));
#103643=CARTESIAN_POINT('Ctrl Pts',(-3.773452038,3.176642188,-6.48605697100001));
#103644=CARTESIAN_POINT('Ctrl Pts',(-3.977408972,3.214285714,-6.358476065));
#103645=CARTESIAN_POINT('Ctrl Pts',(-4.122549284,3.241073689,-6.267686641));
#103646=CARTESIAN_POINT('Ctrl Pts',(-4.263395817,3.268112745,-6.170369204));
#103647=CARTESIAN_POINT('Ctrl Pts',(-3.23191704421808,3.13852541968788,
-6.48977751740939));
#103648=CARTESIAN_POINT('Ctrl Pts',(-3.37105452078987,3.16400222522259,
-6.42048688524908));
#103649=CARTESIAN_POINT('Ctrl Pts',(-3.50760073455668,3.18928040271179,
-6.34689691151957));
#103650=CARTESIAN_POINT('Ctrl Pts',(-3.64118256069049,3.21428571388654,
-6.26931332443069));
#103651=CARTESIAN_POINT('Ctrl Pts',(-3.73497693796392,3.2318431745299,-6.2148380678272));
#103652=CARTESIAN_POINT('Ctrl Pts',(-3.8277856892367,3.24953506285817,-6.15811898082334));
#103653=CARTESIAN_POINT('Ctrl Pts',(-3.91945202642927,3.26733592557389,
-6.09921272133924));
#103654=CARTESIAN_POINT('Ctrl Pts',(-2.512292641,3.268101717,-6.80080037100001));
#103655=CARTESIAN_POINT('Ctrl Pts',(-2.880525075,3.203647866,-6.664771142));
#103656=CARTESIAN_POINT('Ctrl Pts',(-3.231917035,3.138525418,-6.489777522));
#103657=CARTESIAN_POINT('Ctrl Pts',(-2.366799461,3.268101717,-7.116759116));
#103658=CARTESIAN_POINT('Ctrl Pts',(-2.752139625,3.203647866,-6.988607681));
#103659=CARTESIAN_POINT('Ctrl Pts',(-3.121389897,3.138525418,-6.819598603));
#103660=CARTESIAN_POINT('',(-2.51666697029969,3.26733592572713,-6.79918284407265));
#103661=CARTESIAN_POINT('Origin',(0.0951113227613803,3.08931096500382,0.172566420176966));
#103662=CARTESIAN_POINT('Ctrl Pts',(-2.60223082985599,3.22840426963563,
-7.03408805099015));
#103663=CARTESIAN_POINT('Ctrl Pts',(-2.58805351091312,3.23458082930022,
-6.99486475264879));
#103664=CARTESIAN_POINT('Ctrl Pts',(-2.57382992032545,3.24090849487529,
-6.95565597828295));
#103665=CARTESIAN_POINT('Ctrl Pts',(-2.54531659672928,3.25387487496946,
-6.87736663252218));
#103666=CARTESIAN_POINT('Ctrl Pts',(-2.53100984964101,3.26052132409144,
-6.83823932508442));
#103667=CARTESIAN_POINT('Ctrl Pts',(-2.5166669689879,3.26733592513527,-6.79918284529232));
#103668=CARTESIAN_POINT('Ctrl Pts',(-1.76124628,3.138525418,-7.032816757));
#103669=CARTESIAN_POINT('Ctrl Pts',(-1.986833627,3.176642188,-6.976322341));
#103670=CARTESIAN_POINT('Ctrl Pts',(-2.208336691,3.214285714,-6.905486881));
#103671=CARTESIAN_POINT('Ctrl Pts',(-2.365963221,3.241073689,-6.855078784));
#103672=CARTESIAN_POINT('Ctrl Pts',(-2.521125518,3.268112745,-6.79753088400001));
#103673=CARTESIAN_POINT('Ctrl Pts',(-2.05959626,3.138525418,-7.211661615));
#103674=CARTESIAN_POINT('Ctrl Pts',(-2.290920304,3.176642188,-7.14559720900001));
#103675=CARTESIAN_POINT('Ctrl Pts',(-2.517534962,3.214285714,-7.064843786));
#103676=CARTESIAN_POINT('Ctrl Pts',(-2.678799016,3.241073689,-7.007377845));
#103677=CARTESIAN_POINT('Ctrl Pts',(-2.837273008,3.268112745,-6.942613476));
#103678=CARTESIAN_POINT('Ctrl Pts',(-1.76124628998941,3.13852541968788,
-7.03281675449832));
#103679=CARTESIAN_POINT('Ctrl Pts',(-1.91202624773565,3.1640022252232,-6.99505654399892));
#103680=CARTESIAN_POINT('Ctrl Pts',(-2.06119975543362,3.18928040271826,
-6.95254046279405));
#103681=CARTESIAN_POINT('Ctrl Pts',(-2.20833669058812,3.21428571391941,
-6.90548688118375));
#103682=CARTESIAN_POINT('Ctrl Pts',(-2.31164877748298,3.23184317459871,
-6.8724482441944));
#103683=CARTESIAN_POINT('Ctrl Pts',(-2.41448063853639,3.24953506284485,
-6.83700635608134));
#103684=CARTESIAN_POINT('Ctrl Pts',(-2.51666697237623,3.26733592557854,
-6.7991828447383));
#103685=CARTESIAN_POINT('Ctrl Pts',(-0.991585586000001,3.268101717,-7.181870093));
#103686=CARTESIAN_POINT('Ctrl Pts',(-1.380451213,3.203647866,-7.128180239));
#103687=CARTESIAN_POINT('Ctrl Pts',(-1.76124628,3.138525418,-7.032816757));
#103688=CARTESIAN_POINT('Ctrl Pts',(-0.781572165,3.268101717,-7.459165164));
#103689=CARTESIAN_POINT('Ctrl Pts',(-1.18545206,3.203647866,-7.416846584));
#103690=CARTESIAN_POINT('Ctrl Pts',(-1.582401422,3.138525418,-7.331166738));
#103691=CARTESIAN_POINT('',(-0.996205365808877,3.26733592575295,-7.18123073379648));
#103692=CARTESIAN_POINT('Origin',(0.0557910408913048,3.08931098047701,0.188978248038894));
#103693=CARTESIAN_POINT('Ctrl Pts',(-1.02927111432491,3.22840426962271,
-7.42903768812463));
#103694=CARTESIAN_POINT('Ctrl Pts',(-1.02385710291355,3.23458082929551,
-7.38768370417306));
#103695=CARTESIAN_POINT('Ctrl Pts',(-1.01839477946308,3.24090849484858,
-7.34633395786893));
#103696=CARTESIAN_POINT('Ctrl Pts',(-1.00737797670184,3.25387487498619,
-7.26374545175727));
#103697=CARTESIAN_POINT('Ctrl Pts',(-1.00181692801302,3.26052132410948,
-7.22245739145548));
#103698=CARTESIAN_POINT('Ctrl Pts',(-0.996205364803589,3.2673359251782,
-7.18123073508118));
#103699=CARTESIAN_POINT('Ctrl Pts',(-0.208221606,3.138525418,-7.247009298));
#103700=CARTESIAN_POINT('Ctrl Pts',(-0.440679476,3.176642188,-7.240330301));
#103701=CARTESIAN_POINT('Ctrl Pts',(-0.672231452,3.214285714,-7.218767545));
#103702=CARTESIAN_POINT('Ctrl Pts',(-0.837009012,3.241073689,-7.203423007));
#103703=CARTESIAN_POINT('Ctrl Pts',(-1.000914798,3.268112745,-7.180575852));
#103704=CARTESIAN_POINT('Ctrl Pts',(-0.461149972000001,3.138525418,-7.485809288));
#103705=CARTESIAN_POINT('Ctrl Pts',(-0.701267683,3.176642188,-7.471017264));
#103706=CARTESIAN_POINT('Ctrl Pts',(-0.939943815,3.214285714,-7.440867263));
#103707=CARTESIAN_POINT('Ctrl Pts',(-1.109791084,3.241073689,-7.419411849));
#103708=CARTESIAN_POINT('Ctrl Pts',(-1.278482467,3.268112745,-7.390228859));
#103709=CARTESIAN_POINT('Ctrl Pts',(-0.208221615909558,3.1385254196249,
-7.24700929771528));
#103710=CARTESIAN_POINT('Ctrl Pts',(-0.363593751790943,3.16400222523584,
-7.24254513361163));
#103711=CARTESIAN_POINT('Ctrl Pts',(-0.518419366784687,3.18928040275688,
-7.23309094882667));
#103712=CARTESIAN_POINT('Ctrl Pts',(-0.672231451173942,3.21428571381686,
-7.21876754535419));
#103713=CARTESIAN_POINT('Ctrl Pts',(-0.78023048864515,3.23184317437099,
-7.20871037919489));
#103714=CARTESIAN_POINT('Ctrl Pts',(-0.888277156888164,3.24953506287325,
-7.19620291266289));
#103715=CARTESIAN_POINT('Ctrl Pts',(-0.996205367738843,3.2673359256217,
-7.18123073489443));
#103716=CARTESIAN_POINT('Ctrl Pts',(0.57548691,3.268101717,-7.22712355100001));
#103717=CARTESIAN_POINT('Ctrl Pts',(0.184171013,3.203647866,-7.258283552));
#103718=CARTESIAN_POINT('Ctrl Pts',(-0.208221606,3.138525418,-7.247009298));
#103719=CARTESIAN_POINT('Ctrl Pts',(0.840200577,3.268101717,-7.45278894));
#103720=CARTESIAN_POINT('Ctrl Pts',(0.436665925,3.203647866,-7.498281983));
#103721=CARTESIAN_POINT('Ctrl Pts',(0.030578384,3.138525418,-7.49993766400001));
#103722=CARTESIAN_POINT('',(0.57083769428385,3.26733592572195,-7.22749225621831));
#103723=CARTESIAN_POINT('Origin',(0.013861946971019,3.08931094139413,0.196553253651505));
#103724=CARTESIAN_POINT('Ctrl Pts',(0.591816174293092,3.2284042696266,-7.47661377961472));
#103725=CARTESIAN_POINT('Ctrl Pts',(0.588213725055049,3.23458082929749,
-7.43506277647234));
#103726=CARTESIAN_POINT('Ctrl Pts',(0.58465936936327,3.24090849486392,-7.39350552617535));
#103727=CARTESIAN_POINT('Ctrl Pts',(0.577664518215184,3.25387487498635,
-7.31047960671268));
#103728=CARTESIAN_POINT('Ctrl Pts',(0.574219840398537,3.26052132408112,
-7.26896137744006));
#103729=CARTESIAN_POINT('Ctrl Pts',(0.5708376961645,3.26733592511452,-7.22749225731375));
#103730=CARTESIAN_POINT('Ctrl Pts',(1.354539278,3.138525418,-7.12233973800001));
#103731=CARTESIAN_POINT('Ctrl Pts',(1.126080358,3.176642188,-7.16578846299999));
#103732=CARTESIAN_POINT('Ctrl Pts',(0.895306583,3.214285714,-7.194506663));
#103733=CARTESIAN_POINT('Ctrl Pts',(0.731082809,3.241073689,-7.214943176));
#103734=CARTESIAN_POINT('Ctrl Pts',(0.566097586,3.268112745,-7.227865074));
#103735=CARTESIAN_POINT('Ctrl Pts',(1.158859176,3.138525418,-7.40992884));
#103736=CARTESIAN_POINT('Ctrl Pts',(0.921175436,3.176642188,-7.447100854));
#103737=CARTESIAN_POINT('Ctrl Pts',(0.68159806,3.214285714,-7.468964057));
#103738=CARTESIAN_POINT('Ctrl Pts',(0.511109446,3.241073689,-7.48452240000001));
#103739=CARTESIAN_POINT('Ctrl Pts',(0.340088494,3.268112745,-7.492285353));
#103740=CARTESIAN_POINT('Ctrl Pts',(1.35453926809449,3.13852541965266,-7.12233973988385));
#103741=CARTESIAN_POINT('Ctrl Pts',(1.20183998324743,3.16400222535949,-7.15138036208737));
#103742=CARTESIAN_POINT('Ctrl Pts',(1.0486017351784,3.18928040286008,-7.17543014167008));
#103743=CARTESIAN_POINT('Ctrl Pts',(0.895306583377108,3.21428571393849,
-7.19450666295307));
#103744=CARTESIAN_POINT('Ctrl Pts',(0.787670510382668,3.23184317448289,
-7.20790122789566));
#103745=CARTESIAN_POINT('Ctrl Pts',(0.679461177112904,3.24953506300473,
-7.21891301928234));
#103746=CARTESIAN_POINT('Ctrl Pts',(0.570837692521339,3.2673359256781,-7.22749225782456));
#103747=CARTESIAN_POINT('Ctrl Pts',(2.115650277,3.268101717,-6.934444744));
#103748=CARTESIAN_POINT('Ctrl Pts',(1.740181607,3.203647866,-7.04899759200001));
#103749=CARTESIAN_POINT('Ctrl Pts',(1.354539278,3.138525418,-7.122339738));
#103750=CARTESIAN_POINT('Ctrl Pts',(2.422686474,3.268101717,-7.097928589));
#103751=CARTESIAN_POINT('Ctrl Pts',(2.038365897,3.203647866,-7.229106051));
#103752=CARTESIAN_POINT('Ctrl Pts',(1.64212838,3.138525418,-7.31801984));
#103753=CARTESIAN_POINT('',(2.11118901820754,3.26733592571401,-6.93580427368901));
#103754=CARTESIAN_POINT('Origin',(-0.0287152861479012,3.08931093193192,
0.194937927107114));
#103755=CARTESIAN_POINT('Ctrl Pts',(2.18523079690076,3.22840426966378,-7.17459172099073));
#103756=CARTESIAN_POINT('Ctrl Pts',(2.17278033341084,3.2345808293003,-7.13478657745776));
#103757=CARTESIAN_POINT('Ctrl Pts',(2.16037549600587,3.24090849486495,-7.09496499386631));
#103758=CARTESIAN_POINT('Ctrl Pts',(2.13569606206944,3.25387487492689,-7.01538386064082));
#103759=CARTESIAN_POINT('Ctrl Pts',(2.12340672683014,3.26052132405336,-6.97557680812192));
#103760=CARTESIAN_POINT('Ctrl Pts',(2.11118902049569,3.26733592510254,-6.93580427394857));
#103761=CARTESIAN_POINT('Ctrl Pts',(2.853963411,3.138525418,-6.664637488));
#103762=CARTESIAN_POINT('Ctrl Pts',(2.640185925,3.176642188,-6.75618232100001));
#103763=CARTESIAN_POINT('Ctrl Pts',(2.420981077,3.214285714,-6.833838645));
#103764=CARTESIAN_POINT('Ctrl Pts',(2.264990009,3.241073689,-6.88910062));
#103765=CARTESIAN_POINT('Ctrl Pts',(2.106639876,3.268112745,-6.937187358));
#103766=CARTESIAN_POINT('Ctrl Pts',(2.724681357,3.138525418,-6.98756835400001));
#103767=CARTESIAN_POINT('Ctrl Pts',(2.500545415,3.176642188,-7.074966286));
#103768=CARTESIAN_POINT('Ctrl Pts',(2.271269168,3.214285714,-7.147820393));
#103769=CARTESIAN_POINT('Ctrl Pts',(2.108111067,3.241073689,-7.199665003));
#103770=CARTESIAN_POINT('Ctrl Pts',(1.942757295,3.268112745,-7.244010912));
#103771=CARTESIAN_POINT('Ctrl Pts',(2.85396340153355,3.13852541968788,-6.66463749205377));
#103772=CARTESIAN_POINT('Ctrl Pts',(2.71107701654535,3.16400222536125,-6.72582499334367));
#103773=CARTESIAN_POINT('Ctrl Pts',(2.56659138536508,3.18928040285373,-6.78225419606807));
#103774=CARTESIAN_POINT('Ctrl Pts',(2.42098107764421,3.21428571387529,-6.83383864491471));
#103775=CARTESIAN_POINT('Ctrl Pts',(2.31874091118993,3.23184317441783,-6.87005862604735));
#103776=CARTESIAN_POINT('Ctrl Pts',(2.21542866235714,3.24953506278157,-6.90407477618169));
#103777=CARTESIAN_POINT('Ctrl Pts',(2.11118901681379,3.26733592566732,-6.9358042756577));
#103778=CARTESIAN_POINT('Ctrl Pts',(3.556888188,3.268101717,-6.317519008));
#103779=CARTESIAN_POINT('Ctrl Pts',(3.214823244,3.203647866,-6.510108339));
#103780=CARTESIAN_POINT('Ctrl Pts',(2.853963411,3.138525418,-6.664637488));
#103781=CARTESIAN_POINT('Ctrl Pts',(3.891890244,3.268101717,-6.411176985));
#103782=CARTESIAN_POINT('Ctrl Pts',(3.544754146,3.203647866,-6.621905155));
#103783=CARTESIAN_POINT('Ctrl Pts',(3.176894277,3.138525418,-6.793919543));
#103784=CARTESIAN_POINT('',(3.55282348998685,3.26733592572958,-6.31980579081641));
#103785=CARTESIAN_POINT('Origin',(-0.0699498340693178,3.08931098608908,
0.184207423807791));
#103786=CARTESIAN_POINT('Ctrl Pts',(3.67646645566667,3.22840426962795,-6.53709372735245));
#103787=CARTESIAN_POINT('Ctrl Pts',(3.65575014810974,3.23458082925275,-6.50089568761823));
#103788=CARTESIAN_POINT('Ctrl Pts',(3.6350748655154,3.24090849486529,-6.4646717835873));
#103789=CARTESIAN_POINT('Ctrl Pts',(3.59386483163922,3.25387487496164,-6.39225656160744));
#103790=CARTESIAN_POINT('Ctrl Pts',(3.57330547452155,3.26052132407031,-6.35602201976155));
#103791=CARTESIAN_POINT('Ctrl Pts',(3.55282349185555,3.26733592510644,-6.31980579111858));
#103792=CARTESIAN_POINT('Ctrl Pts',(4.219939387,3.138525418,-5.895304196));
#103793=CARTESIAN_POINT('Ctrl Pts',(4.030839333,3.176642188,-6.030664602));
#103794=CARTESIAN_POINT('Ctrl Pts',(3.833453187,3.214285714,-6.153627927));
#103795=CARTESIAN_POINT('Ctrl Pts',(3.692988795,3.241073689,-6.241131377));
#103796=CARTESIAN_POINT('Ctrl Pts',(3.548678026,3.268112745,-6.322134471));
#103797=CARTESIAN_POINT('Ctrl Pts',(4.163100466,3.138525418,-6.238476938));
#103798=CARTESIAN_POINT('Ctrl Pts',(3.96299267,3.176642188,-6.372014157));
#103799=CARTESIAN_POINT('Ctrl Pts',(3.754738253,3.214285714,-6.492452591));
#103800=CARTESIAN_POINT('Ctrl Pts',(3.606539757,3.241073689,-6.578159272));
#103801=CARTESIAN_POINT('Ctrl Pts',(3.454584923,3.268112745,-6.657014572));
#103802=CARTESIAN_POINT('Ctrl Pts',(4.21993937862631,3.13852541968788,-5.89530420199401));
#103803=CARTESIAN_POINT('Ctrl Pts',(4.09354710207681,3.16400222536351,-5.98577752262913));
#103804=CARTESIAN_POINT('Ctrl Pts',(3.96457007535463,3.18928040285766,-6.07194758173095));
#103805=CARTESIAN_POINT('Ctrl Pts',(3.83345318714864,3.21428571397165,-6.15362792690741));
#103806=CARTESIAN_POINT('Ctrl Pts',(3.74138956432755,3.2318431745597,-6.2109797190739));
#103807=CARTESIAN_POINT('Ctrl Pts',(3.64780516492101,3.24953506295641,-6.26640966964533));
#103808=CARTESIAN_POINT('Ctrl Pts',(3.55282348911443,3.26733592560357,-6.31980579292579));
#103809=CARTESIAN_POINT('Ctrl Pts',(4.831809961,3.268101717,-5.405193105));
#103810=CARTESIAN_POINT('Ctrl Pts',(4.539143318,3.203647866,-5.666813656));
#103811=CARTESIAN_POINT('Ctrl Pts',(4.219939387,3.138525418,-5.895304196));
#103812=CARTESIAN_POINT('Ctrl Pts',(5.179113551,3.268101717,-5.424645871));
#103813=CARTESIAN_POINT('Ctrl Pts',(4.88539363,3.203647866,-5.70507133300001));
#103814=CARTESIAN_POINT('Ctrl Pts',(4.563112129,3.138525418,-5.952143118));
#103815=CARTESIAN_POINT('',(4.82833188398055,3.26733592573913,-5.40830021374329));
#103816=CARTESIAN_POINT('Origin',(-0.107913616441742,3.08931095515453,0.164863647656065));
#103817=CARTESIAN_POINT('Ctrl Pts',(4.99579462933179,3.22840426964393,-5.59392849629774));
#103818=CARTESIAN_POINT('Ctrl Pts',(4.96778114867766,3.23458082931661,-5.56303014017645));
#103819=CARTESIAN_POINT('Ctrl Pts',(4.93980217423524,3.24090849488393,-5.53209770576372));
#103820=CARTESIAN_POINT('Ctrl Pts',(4.88398847580303,3.25387487498294,-5.4702344506208));
#103821=CARTESIAN_POINT('Ctrl Pts',(4.85612042961005,3.26052132408991,-5.43926670631695));
#103822=CARTESIAN_POINT('Ctrl Pts',(4.82833188572363,3.2673359251254,-5.40830021382373));
#103823=CARTESIAN_POINT('Ctrl Pts',(5.388595688,3.138525418,-4.850313032));
#103824=CARTESIAN_POINT('Ctrl Pts',(5.233015174,3.176642188,-5.023159709));
#103825=CARTESIAN_POINT('Ctrl Pts',(5.066677286,3.214285714,-5.185680407));
#103826=CARTESIAN_POINT('Ctrl Pts',(4.948307528,3.241073689,-5.301333767));
#103827=CARTESIAN_POINT('Ctrl Pts',(4.824783936,3.268112745,-5.411465603));
#103828=CARTESIAN_POINT('Ctrl Pts',(5.406857624,3.138525418,-5.197681275));
#103829=CARTESIAN_POINT('Ctrl Pts',(5.240134792,3.176642188,-5.371113728));
#103830=CARTESIAN_POINT('Ctrl Pts',(5.062639951,3.214285714,-5.533504923));
#103831=CARTESIAN_POINT('Ctrl Pts',(4.936330656,3.241073689,-5.649066125));
#103832=CARTESIAN_POINT('Ctrl Pts',(4.804880001,3.268112745,-5.75874362900001));
#103833=CARTESIAN_POINT('Ctrl Pts',(5.38859568103647,3.13852541970604,-4.85031303973633));
#103834=CARTESIAN_POINT('Ctrl Pts',(5.28460747541426,3.16400222529863,-4.96584174750943));
#103835=CARTESIAN_POINT('Ctrl Pts',(5.17716987523629,3.18928040278646,-5.07772344700988));
#103836=CARTESIAN_POINT('Ctrl Pts',(5.06667728632456,3.21428571392649,-5.18568040670526));
#103837=CARTESIAN_POINT('Ctrl Pts',(4.98909499935702,3.23184317453923,-5.26148230335792));
#103838=CARTESIAN_POINT('Ctrl Pts',(4.90961435227911,3.24953506289354,-5.33573421173237));
#103839=CARTESIAN_POINT('Ctrl Pts',(4.82833188365589,3.2673359255739,-5.40830021600123));
#103840=CARTESIAN_POINT('Ctrl Pts',(5.88080167,3.268101717,-4.240126379));
#103841=CARTESIAN_POINT('Ctrl Pts',(5.651218096,3.203647866,-4.558545065));
#103842=CARTESIAN_POINT('Ctrl Pts',(5.38859568799999,3.138525418,-4.850313032));
#103843=CARTESIAN_POINT('Ctrl Pts',(6.224167265,3.268101717,-4.184464345));
#103844=CARTESIAN_POINT('Ctrl Pts',(5.997597537,3.203647866,-4.521474716));
#103845=CARTESIAN_POINT('Ctrl Pts',(5.73596393,3.138525418,-4.832051096));
#103846=CARTESIAN_POINT('',(5.87807284531811,3.26733592573095,-4.24390852964466));
#103847=CARTESIAN_POINT('Origin',(-0.140831311052029,3.08931092092322,0.137810866124939));
#103848=CARTESIAN_POINT('Ctrl Pts',(6.08152499813999,3.22840426963123,-4.38919738580149));
#103849=CARTESIAN_POINT('Ctrl Pts',(6.04752422391984,3.23458082931669,-4.36504348632207));
#103850=CARTESIAN_POINT('Ctrl Pts',(6.01354982343028,3.24090849488865,-4.34084888746317));
#103851=CARTESIAN_POINT('Ctrl Pts',(5.9457422472682,3.25387487500342,-4.29243025597143));
#103852=CARTESIAN_POINT('Ctrl Pts',(5.91186859103641,3.26052132410905,-4.2681773263534));
#103853=CARTESIAN_POINT('Ctrl Pts',(5.87807284750703,3.26733592513226,-4.24390852857892));
#103854=CARTESIAN_POINT('Ctrl Pts',(6.30528724300001,3.138525418,-3.578526622));
#103855=CARTESIAN_POINT('Ctrl Pts',(6.190501041,3.176642188,-3.780777451));
#103856=CARTESIAN_POINT('Ctrl Pts',(6.062989186,3.214285714,-3.975256234));
#103857=CARTESIAN_POINT('Ctrl Pts',(5.972248902,3.241073689,-4.113651681));
#103858=CARTESIAN_POINT('Ctrl Pts',(5.875288312,3.268112745,-4.247762617));
#103859=CARTESIAN_POINT('Ctrl Pts',(6.397796129,3.138525418,-3.913847811));
#103860=CARTESIAN_POINT('Ctrl Pts',(6.272254035,3.176642188,-4.119065991));
#103861=CARTESIAN_POINT('Ctrl Pts',(6.133818231,3.214285714,-4.315816714));
#103862=CARTESIAN_POINT('Ctrl Pts',(6.03530422,3.241073689,-4.455828924));
#103863=CARTESIAN_POINT('Ctrl Pts',(5.93050422900001,3.268112745,-4.59120023400001));
#103864=CARTESIAN_POINT('Ctrl Pts',(6.3052872377432,3.13852541974561,-3.57852663126237));
#103865=CARTESIAN_POINT('Ctrl Pts',(6.22856547558023,3.16400222534719,-3.71370873221474));
#103866=CARTESIAN_POINT('Ctrl Pts',(6.14769096485557,3.18928040281778,-3.84607060772969));
#103867=CARTESIAN_POINT('Ctrl Pts',(6.06298918650265,3.21428571386929,-3.97525623361275));
#103868=CARTESIAN_POINT('Ctrl Pts',(6.00351589840414,3.23184317440521,-4.06596382168667));
#103869=CARTESIAN_POINT('Ctrl Pts',(5.94185542949822,3.24953506300735,-4.15556575210618));
#103870=CARTESIAN_POINT('Ctrl Pts',(5.87807284550827,3.26733592570877,-4.24390853185449));
#103871=CARTESIAN_POINT('Ctrl Pts',(6.65481363,3.268101717,-2.876796057));
#103872=CARTESIAN_POINT('Ctrl Pts',(6.499048197,3.203647866,-3.237123972));
#103873=CARTESIAN_POINT('Ctrl Pts',(6.305287243,3.138525418,-3.578526622));
#103874=CARTESIAN_POINT('Ctrl Pts',(6.978185836,3.268101717,-2.748621917));
#103875=CARTESIAN_POINT('Ctrl Pts',(6.82936045,3.203647866,-3.126458967));
#103876=CARTESIAN_POINT('Ctrl Pts',(6.640608432,3.138525418,-3.486017736));
#103877=CARTESIAN_POINT('',(6.65296165370764,3.26733592574237,-2.88107639920788));
#103878=CARTESIAN_POINT('Origin',(-0.167164222473216,3.0893109714355,0.104314448279226));
#103879=CARTESIAN_POINT('Ctrl Pts',(6.8828900176845,3.22840426961484,-2.97923228418363));
#103880=CARTESIAN_POINT('Ctrl Pts',(6.84449178843485,3.23458082927717,-2.96295225087537));
#103881=CARTESIAN_POINT('Ctrl Pts',(6.80611056664103,3.24090849489122,-2.946626800043));
#103882=CARTESIAN_POINT('Ctrl Pts',(6.72947971953556,3.25387487496616,-2.91391679399286));
#103883=CARTESIAN_POINT('Ctrl Pts',(6.69118434737886,3.26052132410795,-2.89751271921047));
#103884=CARTESIAN_POINT('Ctrl Pts',(6.6529616554568,3.26733592515834,-2.88107639836296));
#103885=CARTESIAN_POINT('Ctrl Pts',(6.927150574,3.138525418,-2.139412284));
#103886=CARTESIAN_POINT('Ctrl Pts',(6.85852596,3.176642188,-2.361610241));
#103887=CARTESIAN_POINT('Ctrl Pts',(6.775802451,3.214285714,-2.578953498));
#103888=CARTESIAN_POINT('Ctrl Pts',(6.716934554,3.241073689,-2.733619816));
#103889=CARTESIAN_POINT('Ctrl Pts',(6.651070736,3.268112745,-2.885438973));
#103890=CARTESIAN_POINT('Ctrl Pts',(7.089580798,3.138525418,-2.447007174));
#103891=CARTESIAN_POINT('Ctrl Pts',(7.011089651,3.176642188,-2.674415306));
#103892=CARTESIAN_POINT('Ctrl Pts',(6.918185988,3.214285714,-2.896325712));
#103893=CARTESIAN_POINT('Ctrl Pts',(6.852073667,3.241073689,-3.054242115));
#103894=CARTESIAN_POINT('Ctrl Pts',(6.778824671,3.268112745,-3.208977419));
#103895=CARTESIAN_POINT('Ctrl Pts',(6.92715057096117,3.13852541968788,-2.13941229383933));
#103896=CARTESIAN_POINT('Ctrl Pts',(6.8812826770035,3.16400222537056,-2.28792682359604));
#103897=CARTESIAN_POINT('Ctrl Pts',(6.83075285815803,3.1892804028607,-2.43457978110859));
#103898=CARTESIAN_POINT('Ctrl Pts',(6.77580245144929,3.21428571385279,-2.57895349743044));
#103899=CARTESIAN_POINT('Ctrl Pts',(6.7372190656392,3.23184317436579,-2.68032539196548));
#103900=CARTESIAN_POINT('Ctrl Pts',(6.69626195096635,3.24953506283404,-2.78108765672484));
#103901=CARTESIAN_POINT('Ctrl Pts',(6.65296165431191,3.26733592567481,-2.88107640154563));
#103902=CARTESIAN_POINT('Ctrl Pts',(7.1176539,3.268101717,-1.378949948));
#103903=CARTESIAN_POINT('Ctrl Pts',(7.042990027,3.203647866,-1.764338561));
#103904=CARTESIAN_POINT('Ctrl Pts',(6.92715057400001,3.138525418,-2.139412284));
#103905=CARTESIAN_POINT('Ctrl Pts',(7.405912192,3.268101717,-1.184256983));
#103906=CARTESIAN_POINT('Ctrl Pts',(7.341790058,3.203647866,-1.585253472));
#103907=CARTESIAN_POINT('Ctrl Pts',(7.234745464,3.138525418,-1.97698206));
#103908=CARTESIAN_POINT('',(7.11676537017746,3.26733592564584,-1.38352833888187));
#103909=CARTESIAN_POINT('Origin',(-0.185680395541384,3.08931094970989,0.065940249265263));
#103910=CARTESIAN_POINT('Ctrl Pts',(7.36241874941721,3.22840426966299,-1.42996159172976));
#103911=CARTESIAN_POINT('Ctrl Pts',(7.32141852347748,3.23458082931197,-1.42231666088157));
#103912=CARTESIAN_POINT('Ctrl Pts',(7.28042514453175,3.24090849482907,-1.41462371828302));
#103913=CARTESIAN_POINT('Ctrl Pts',(7.19855419931416,3.25387487491436,-1.39915182095323));
#103914=CARTESIAN_POINT('Ctrl Pts',(7.1576277604363,3.26052132403564,-1.3913636373889));
#103915=CARTESIAN_POINT('Ctrl Pts',(7.11676537032653,3.26733592507926,-1.38352833765408));
#103916=CARTESIAN_POINT('Ctrl Pts',(7.22510804400001,3.138525418,-0.600261405));
#103917=CARTESIAN_POINT('Ctrl Pts',(7.205853827,3.176642188,-0.832016762));
#103918=CARTESIAN_POINT('Ctrl Pts',(7.171786724,3.214285714,-1.062061763));
#103919=CARTESIAN_POINT('Ctrl Pts',(7.147543812,3.241073689,-1.225766926));
#103920=CARTESIAN_POINT('Ctrl Pts',(7.115856484,3.268112745,-1.38819541));
#103921=CARTESIAN_POINT('Ctrl Pts',(7.449864548,3.138525418,-0.865747201));
#103922=CARTESIAN_POINT('Ctrl Pts',(7.422094506,3.176642188,-1.104711934));
#103923=CARTESIAN_POINT('Ctrl Pts',(7.379067058,3.214285714,-1.341405739));
#103924=CARTESIAN_POINT('Ctrl Pts',(7.348447764,3.241073689,-1.509842339));
#103925=CARTESIAN_POINT('Ctrl Pts',(7.310174806,3.268112745,-1.676706386));
#103926=CARTESIAN_POINT('Ctrl Pts',(7.22510804312559,3.13852541973103,-0.600261415524939));
#103927=CARTESIAN_POINT('Ctrl Pts',(7.21223874827869,3.16400222530692,-0.755163999666638));
#103928=CARTESIAN_POINT('Ctrl Pts',(7.19441633930332,3.18928040278829,-0.909250710107161));
#103929=CARTESIAN_POINT('Ctrl Pts',(7.17178672409929,3.21428571389028,-1.06206176232951));
#103930=CARTESIAN_POINT('Ctrl Pts',(7.1558973568498,3.2318431745165,-1.16935792614114));
#103931=CARTESIAN_POINT('Ctrl Pts',(7.1375587053205,3.24953506279988,-1.27656899333765));
#103932=CARTESIAN_POINT('Ctrl Pts',(7.11676537124032,3.26733592538515,-1.38352834137664));
#103933=CARTESIAN_POINT('Ctrl Pts',(7.247680585,3.268101717,0.183374327));
#103934=CARTESIAN_POINT('Ctrl Pts',(7.257609471,3.203647866,-0.209054639));
#103935=CARTESIAN_POINT('Ctrl Pts',(7.225108044,3.138525418,-0.600261405));
#103936=CARTESIAN_POINT('Ctrl Pts',(7.487346326,3.268101717,0.435482491));
#103937=CARTESIAN_POINT('Ctrl Pts',(7.510925723,3.203647866,0.030076714));
#103938=CARTESIAN_POINT('Ctrl Pts',(7.49059384,3.138525418,-0.375504901));
#103939=CARTESIAN_POINT('',(7.24779704613829,3.26733592573548,0.178711968919609));
#103940=CARTESIAN_POINT('Origin',(-0.195514704512931,3.08931097303294,0.0244827985403307));
#103941=CARTESIAN_POINT('Ctrl Pts',(7.49768896349623,3.22840426965684,0.18617251498347));
#103942=CARTESIAN_POINT('Ctrl Pts',(7.45600386584464,3.23458082930064,0.184824874873088));
#103943=CARTESIAN_POINT('Ctrl Pts',(7.41431513378787,3.24090849486615,0.183525596007401));
#103944=CARTESIAN_POINT('Ctrl Pts',(7.33103228512314,3.25387487500965,0.181035935899268));
#103945=CARTESIAN_POINT('Ctrl Pts',(7.28938845447293,3.2605213241582,0.179844061555137));
#103946=CARTESIAN_POINT('Ctrl Pts',(7.24779704649391,3.26733592525333,0.178711970411889));
#103947=CARTESIAN_POINT('Ctrl Pts',(7.18522749100001,3.138525418,0.96695703));
#103948=CARTESIAN_POINT('Ctrl Pts',(7.216243979,3.176642188,0.736480897));
#103949=CARTESIAN_POINT('Ctrl Pts',(7.23242622,3.214285714,0.5044908));
#103950=CARTESIAN_POINT('Ctrl Pts',(7.243941865,3.241073689,0.339401464));
#103951=CARTESIAN_POINT('Ctrl Pts',(7.247912692,3.268112745,0.173958629));
#103952=CARTESIAN_POINT('Ctrl Pts',(7.461800912,3.138525418,0.755994149));
#103953=CARTESIAN_POINT('Ctrl Pts',(7.486050472,3.176642188,0.516646541000001));
#103954=CARTESIAN_POINT('Ctrl Pts',(7.494911153,3.214285714,0.276236876));
#103955=CARTESIAN_POINT('Ctrl Pts',(7.501216611,3.241073689,0.105155986));
#103956=CARTESIAN_POINT('Ctrl Pts',(7.499709291,3.268112745,-0.066034427));
#103957=CARTESIAN_POINT('Ctrl Pts',(7.18522749238694,3.13852541970443,0.966957019694023));
#103958=CARTESIAN_POINT('Ctrl Pts',(7.20595855182675,3.16400222522679,0.812909454265956));
#103959=CARTESIAN_POINT('Ctrl Pts',(7.22167690884421,3.18928040272318,0.658593914269724));
#103960=CARTESIAN_POINT('Ctrl Pts',(7.23242622034782,3.21428571381248,0.504490800783123));
#103961=CARTESIAN_POINT('Ctrl Pts',(7.23997384168336,3.23184317440338,0.396287417808053));
#103962=CARTESIAN_POINT('Ctrl Pts',(7.24511114796464,3.2495350629339,0.287640616691123));
#103963=CARTESIAN_POINT('Ctrl Pts',(7.24779704763703,3.26733592561058,0.178711967189));
#103964=CARTESIAN_POINT('Ctrl Pts',(7.03881378,3.268101717,1.737124223));
#103965=CARTESIAN_POINT('Ctrl Pts',(7.132871163,3.203647866,1.356004445));
#103966=CARTESIAN_POINT('Ctrl Pts',(7.185227491,3.138525418,0.96695703));
#103967=CARTESIAN_POINT('Ctrl Pts',(7.218680466,3.268101717,2.034859288));
#103968=CARTESIAN_POINT('Ctrl Pts',(7.328858849,3.203647866,1.644000547));
#103969=CARTESIAN_POINT('Ctrl Pts',(7.39619037200001,3.138525418,1.24353045));
#103970=CARTESIAN_POINT('',(7.03992978765218,3.26733592573162,1.73259590431476));
#103971=CARTESIAN_POINT('Origin',(-0.19620638574868,3.0893109602979,-0.0181194053157016));
#103972=CARTESIAN_POINT('Ctrl Pts',(7.28237557417294,3.22840426964679,1.79360140244549));
#103973=CARTESIAN_POINT('Ctrl Pts',(7.24195475358925,3.23458082933613,1.78332420568998));
#103974=CARTESIAN_POINT('Ctrl Pts',(7.20151998757062,3.24090849489714,1.77309345819916));
#103975=CARTESIAN_POINT('Ctrl Pts',(7.12071944905017,3.25387487502398,1.75275865431607));
#103976=CARTESIAN_POINT('Ctrl Pts',(7.08030544586912,3.26052132414294,1.74264245270595));
#103977=CARTESIAN_POINT('Ctrl Pts',(7.03992978822808,3.2673359251799,1.73259590600152));
#103978=CARTESIAN_POINT('Ctrl Pts',(6.809373687,3.138525418,2.488961628));
#103979=CARTESIAN_POINT('Ctrl Pts',(6.889210582,3.176642188,2.270541528));
#103980=CARTESIAN_POINT('Ctrl Pts',(6.954885505,3.214285714,2.047453934));
#103981=CARTESIAN_POINT('Ctrl Pts',(7.001621248,3.241073689,1.888699818));
#103982=CARTESIAN_POINT('Ctrl Pts',(7.04106455800001,3.268112745,1.727978555));
#103983=CARTESIAN_POINT('Ctrl Pts',(7.124831758,3.138525418,2.342386053));
#103984=CARTESIAN_POINT('Ctrl Pts',(7.199967038,3.176642188,2.113847197));
#103985=CARTESIAN_POINT('Ctrl Pts',(7.260301532,3.214285714,1.880962961));
#103986=CARTESIAN_POINT('Ctrl Pts',(7.303236907,3.241073689,1.715237335));
#103987=CARTESIAN_POINT('Ctrl Pts',(7.338565706,3.268112745,1.547725229));
#103988=CARTESIAN_POINT('Ctrl Pts',(6.80937369053532,3.13852541968788,2.48896161832797));
#103989=CARTESIAN_POINT('Ctrl Pts',(6.86273574210131,3.16400222528892,2.34297216457238));
#103990=CARTESIAN_POINT('Ctrl Pts',(6.91125989225883,3.18928040278009,2.19564341859102));
#103991=CARTESIAN_POINT('Ctrl Pts',(6.95488550497705,3.21428571389738,2.04745393452308));
#103992=CARTESIAN_POINT('Ctrl Pts',(6.98551719578398,3.23184317447546,1.94340280208701));
#103993=CARTESIAN_POINT('Ctrl Pts',(7.01389024523924,3.249535062973,1.83840047195019));
#103994=CARTESIAN_POINT('Ctrl Pts',(7.03992978951053,3.26733592562892,1.73259590295414));
#103995=CARTESIAN_POINT('Ctrl Pts',(6.500819867,3.268101717,3.209648121));
#103996=CARTESIAN_POINT('Ctrl Pts',(6.67460772600001,3.203647866,2.857658268));
#103997=CARTESIAN_POINT('Ctrl Pts',(6.809373687,3.138525418,2.488961628));
#103998=CARTESIAN_POINT('Ctrl Pts',(6.612477132,3.268101717,3.539088327));
#103999=CARTESIAN_POINT('Ctrl Pts',(6.804102681,3.203647866,3.18105274));
#104000=CARTESIAN_POINT('Ctrl Pts',(6.955949263,3.138525418,2.804419699));
#104001=CARTESIAN_POINT('',(6.50288323752183,3.26733592574725,3.20546558011673));
#104002=CARTESIAN_POINT('Origin',(-0.187724223664845,3.08931099242651,-0.0598744337741502));
#104003=CARTESIAN_POINT('Ctrl Pts',(6.72654639743712,3.22840426967264,3.31716348119342));
#104004=CARTESIAN_POINT('Ctrl Pts',(6.6892798868357,3.23458082931749,3.2984372779879));
#104005=CARTESIAN_POINT('Ctrl Pts',(6.6519897713015,3.2409084948931,3.27975344013471));
#104006=CARTESIAN_POINT('Ctrl Pts',(6.57744968623373,3.25387487500758,3.24252432532321));
#104007=CARTESIAN_POINT('Ctrl Pts',(6.54015522430933,3.26052132413064,3.22395681883508));
#104008=CARTESIAN_POINT('Ctrl Pts',(6.50288323759506,3.26733592520138,3.20546558181229));
#104009=CARTESIAN_POINT('Ctrl Pts',(6.115121138,3.138525418,3.894585148));
#104010=CARTESIAN_POINT('Ctrl Pts',(6.240045355,3.176642188,3.69843416));
#104011=CARTESIAN_POINT('Ctrl Pts',(6.352142073,3.214285714,3.494680397));
#104012=CARTESIAN_POINT('Ctrl Pts',(6.431912603,3.241073689,3.349684667));
#104013=CARTESIAN_POINT('Ctrl Pts',(6.50498407100001,3.268112745,3.201200124));
#104014=CARTESIAN_POINT('Ctrl Pts',(6.45471339,3.138525418,3.819250588));
#104015=CARTESIAN_POINT('Ctrl Pts',(6.577221147,3.176642188,3.612206708));
#104016=CARTESIAN_POINT('Ctrl Pts',(6.686208281,3.214285714,3.397737309));
#104017=CARTESIAN_POINT('Ctrl Pts',(6.763765961,3.241073689,3.245116092));
#104018=CARTESIAN_POINT('Ctrl Pts',(6.834278944,3.268112745,3.089114974));
#104019=CARTESIAN_POINT('Ctrl Pts',(6.1151211433741,3.13852541963974,3.8945851395618));
#104020=CARTESIAN_POINT('Ctrl Pts',(6.1986190363352,3.16400222521114,3.76348010129596));
#104021=CARTESIAN_POINT('Ctrl Pts',(6.27768004407713,3.18928040272125,3.63002707695493));
#104022=CARTESIAN_POINT('Ctrl Pts',(6.35214207269071,3.21428571380303,3.49468039798569));
#104023=CARTESIAN_POINT('Ctrl Pts',(6.40442552953867,3.23184317433645,3.39964683133381));
#104024=CARTESIAN_POINT('Ctrl Pts',(6.45470762996514,3.24953506283669,3.30319876439432));
#104025=CARTESIAN_POINT('Ctrl Pts',(6.50288323951224,3.2673359256285,3.20546557920868));
#104026=CARTESIAN_POINT('Ctrl Pts',(5.658854841,3.268101717,4.53209244));
#104027=CARTESIAN_POINT('Ctrl Pts',(5.904247051,3.203647866,4.225691167));
#104028=CARTESIAN_POINT('Ctrl Pts',(6.11512113800001,3.138525418,3.894585148));
#104029=CARTESIAN_POINT('Ctrl Pts',(5.697081715,3.268101717,4.877833528));
#104030=CARTESIAN_POINT('Ctrl Pts',(5.961194234,3.203647866,4.569362444));
#104031=CARTESIAN_POINT('Ctrl Pts',(6.190455698,3.138525418,4.2341774));
#104032=CARTESIAN_POINT('',(5.6617690946082,3.26733592567607,4.52845124890004));
#104033=CARTESIAN_POINT('Origin',(-0.170464175807428,3.08931094541484,-0.0988298078200384));
#104034=CARTESIAN_POINT('Ctrl Pts',(5.85619138690672,3.22840426963792,4.68561868236563));
#104035=CARTESIAN_POINT('Ctrl Pts',(5.82382172680805,3.23458082926551,4.65931908942937));
#104036=CARTESIAN_POINT('Ctrl Pts',(5.79141990628079,3.2409084948322,4.63305579687645));
#104037=CARTESIAN_POINT('Ctrl Pts',(5.72662568622392,3.25387487490412,4.58067316335606));
#104038=CARTESIAN_POINT('Ctrl Pts',(5.69419461305615,3.26052132402377,4.55452254790572));
#104039=CARTESIAN_POINT('Ctrl Pts',(5.66176909404866,3.26733592507081,4.52845125034263));
#104040=CARTESIAN_POINT('Ctrl Pts',(5.13493232,3.138525418,5.118102194));
#104041=CARTESIAN_POINT('Ctrl Pts',(5.299102543,3.176642188,4.953392122));
#104042=CARTESIAN_POINT('Ctrl Pts',(5.452379538,3.214285714,4.77849949));
#104043=CARTESIAN_POINT('Ctrl Pts',(5.561454873,3.241073689,4.654041985));
#104044=CARTESIAN_POINT('Ctrl Pts',(5.664737759,3.268112745,4.524737133));
#104045=CARTESIAN_POINT('Ctrl Pts',(5.482779798,3.138525418,5.11753121));
#104046=CARTESIAN_POINT('Ctrl Pts',(5.646931706,3.176642188,4.941663448));
#104047=CARTESIAN_POINT('Ctrl Pts',(5.799475362,3.214285714,4.755637236));
#104048=CARTESIAN_POINT('Ctrl Pts',(5.908028837,3.241073689,4.623256827));
#104049=CARTESIAN_POINT('Ctrl Pts',(6.010428894,3.268112745,4.486061135));
#104050=CARTESIAN_POINT('Ctrl Pts',(5.13493232726974,3.13852541968788,5.11810218670635));
#104051=CARTESIAN_POINT('Ctrl Pts',(5.24466179475057,3.16400222542499,5.00801189012052));
#104052=CARTESIAN_POINT('Ctrl Pts',(5.35056285532906,3.18928040292007,4.89467470347088));
#104053=CARTESIAN_POINT('Ctrl Pts',(5.45237953812021,3.21428571400291,4.77849948997936));
#104054=CARTESIAN_POINT('Ctrl Pts',(5.52387004438808,3.23184317456548,4.69692715254307));
#104055=CARTESIAN_POINT('Ctrl Pts',(5.59371006074637,3.24953506288096,4.61354315344578));
#104056=CARTESIAN_POINT('Ctrl Pts',(5.6617690969508,3.26733592546731,4.5284512482931));
#104057=CARTESIAN_POINT('Ctrl Pts',(4.552288053,3.268101717,5.642621154));
#104058=CARTESIAN_POINT('Ctrl Pts',(4.857810345,3.203647866,5.396135444));
#104059=CARTESIAN_POINT('Ctrl Pts',(5.13493232,3.138525418,5.118102194));
#104060=CARTESIAN_POINT('Ctrl Pts',(4.51529709,3.268101717,5.988496655));
#104061=CARTESIAN_POINT('Ctrl Pts',(4.839546969,3.203647866,5.744013838));
#104062=CARTESIAN_POINT('Ctrl Pts',(5.135503304,3.138525418,5.465949672));
#104063=CARTESIAN_POINT('',(4.55591692092414,3.26733592572585,5.63969156909739));
#104064=CARTESIAN_POINT('Origin',(-0.145233333313992,3.08931099796829,-0.133163996178347));
#104065=CARTESIAN_POINT('Ctrl Pts',(4.71200737576507,3.22840426963644,5.83497956214701));
#104066=CARTESIAN_POINT('Ctrl Pts',(4.68604813527371,3.23458082930412,5.80233631877584));
#104067=CARTESIAN_POINT('Ctrl Pts',(4.66004968290258,3.24090849487674,5.7697216137166));
#104068=CARTESIAN_POINT('Ctrl Pts',(4.60803103346474,3.25387487499756,5.70463481473088));
#104069=CARTESIAN_POINT('Ctrl Pts',(4.58197979008192,3.26052132414438,5.67212386389294));
#104070=CARTESIAN_POINT('Ctrl Pts',(4.55591692004631,3.26733592521512,5.63969157057812));
#104071=CARTESIAN_POINT('Ctrl Pts',(3.914639774,3.138525418,6.10230247));
#104072=CARTESIAN_POINT('Ctrl Pts',(4.110379585,3.176642188,5.976734973));
#104073=CARTESIAN_POINT('Ctrl Pts',(4.297669796,3.214285714,5.838881257));
#104074=CARTESIAN_POINT('Ctrl Pts',(4.430949694,3.241073689,5.740781472));
#104075=CARTESIAN_POINT('Ctrl Pts',(4.559614604,3.268112745,5.636702463));
#104076=CARTESIAN_POINT('Ctrl Pts',(4.254477516,3.138525418,6.176521761));
#104077=CARTESIAN_POINT('Ctrl Pts',(4.452598014,3.176642188,6.040053497));
#104078=CARTESIAN_POINT('Ctrl Pts',(4.641565421,3.214285714,5.891168852));
#104079=CARTESIAN_POINT('Ctrl Pts',(4.776038851,3.241073689,5.785219212));
#104080=CARTESIAN_POINT('Ctrl Pts',(4.90553787,3.268112745,5.673244064));
#104081=CARTESIAN_POINT('Ctrl Pts',(3.91463978266771,3.13852541968788,6.10230246443964));
#104082=CARTESIAN_POINT('Ctrl Pts',(4.04546999514332,3.16400222533056,6.01837461000903));
#104083=CARTESIAN_POINT('Ctrl Pts',(4.17325929301746,3.18928040281961,5.93045278158138));
#104084=CARTESIAN_POINT('Ctrl Pts',(4.29766979596682,3.21428571398577,5.83888125705783));
#104085=CARTESIAN_POINT('Ctrl Pts',(4.38502453499581,3.23184317464813,5.77458438070685));
#104086=CARTESIAN_POINT('Ctrl Pts',(4.47115682528837,3.24953506301695,5.70816339197302));
#104087=CARTESIAN_POINT('Ctrl Pts',(4.5559169233774,3.26733592566823,5.63969156895996));
#104088=CARTESIAN_POINT('Ctrl Pts',(3.232861335,3.268101717,6.489307173));
#104089=CARTESIAN_POINT('Ctrl Pts',(3.584227827,3.203647866,6.314262424));
#104090=CARTESIAN_POINT('Ctrl Pts',(3.914639774,3.138525418,6.10230247));
#104091=CARTESIAN_POINT('Ctrl Pts',(3.122382191,3.268101717,6.819144334));
#104092=CARTESIAN_POINT('Ctrl Pts',(3.491607867,3.203647866,6.650081528));
#104093=CARTESIAN_POINT('Ctrl Pts',(3.840420483,3.138525418,6.442140212));
#104094=CARTESIAN_POINT('',(3.23703513325096,3.26733592572603,6.48722618092339));
#104095=CARTESIAN_POINT('Origin',(-0.113211494847973,3.08931099930371,-0.161271503760252));
#104096=CARTESIAN_POINT('Ctrl Pts',(3.3474951365056,3.22840426965528,6.71150328220225));
#104097=CARTESIAN_POINT('Ctrl Pts',(3.32916014099174,3.23458082935693,6.6740427501092));
#104098=CARTESIAN_POINT('Ctrl Pts',(3.31078071561423,3.24090849490936,6.63660166006154));
#104099=CARTESIAN_POINT('Ctrl Pts',(3.27396951324241,3.25387503634,6.56185315250801));
#104100=CARTESIAN_POINT('Ctrl Pts',(3.25551646985801,3.26052140343644,6.52450253885886));
#104101=CARTESIAN_POINT('Ctrl Pts',(3.23703513444458,3.26733592526798,6.48722618166755));
#104102=CARTESIAN_POINT('Ctrl Pts',(2.511303023,3.138525418,6.801165865));
#104103=CARTESIAN_POINT('Ctrl Pts',(2.729459846,3.176642188,6.720612339));
#104104=CARTESIAN_POINT('Ctrl Pts',(2.94200579,3.214285714,6.626243425));
#104105=CARTESIAN_POINT('Ctrl Pts',(3.093258233,3.241073689,6.559088397));
#104106=CARTESIAN_POINT('Ctrl Pts',(3.241288939,3.268112745,6.485101851));
#104107=CARTESIAN_POINT('Ctrl Pts',(2.827240594,3.138525418,6.946705019));
#104108=CARTESIAN_POINT('Ctrl Pts',(3.050065787,3.176642188,6.85601735800001));
#104109=CARTESIAN_POINT('Ctrl Pts',(3.26662104,3.214285714,6.75123596));
#104110=CARTESIAN_POINT('Ctrl Pts',(3.420726596,3.241073689,6.676671176));
#104111=CARTESIAN_POINT('Ctrl Pts',(3.571269346,3.268112745,6.595152406));
#104112=CARTESIAN_POINT('Ctrl Pts',(2.51130303206539,3.13852541958392,6.80116586165265));
#104113=CARTESIAN_POINT('Ctrl Pts',(2.65711651481935,3.1640022252604,6.74732482170336));
#104114=CARTESIAN_POINT('Ctrl Pts',(2.80081876440615,3.18928040278802,6.68892947800552));
#104115=CARTESIAN_POINT('Ctrl Pts',(2.94200578981347,3.21428571395176,6.62624342515397));
#104116=CARTESIAN_POINT('Ctrl Pts',(3.04114014826,3.23184317395206,6.58222846251681));
#104117=CARTESIAN_POINT('Ctrl Pts',(3.13953726152714,3.2495350620974,6.53587625704981));
#104118=CARTESIAN_POINT('Ctrl Pts',(3.2370351341919,3.26733592505327,6.48722618256294));
#104119=CARTESIAN_POINT('Ctrl Pts',(1.762269613,3.268101717,7.032560402));
#104120=CARTESIAN_POINT('Ctrl Pts',(2.1430508,3.203647866,6.937141511));
#104121=CARTESIAN_POINT('Ctrl Pts',(2.511303023,3.138525418,6.801165865));
#104122=CARTESIAN_POINT('Ctrl Pts',(1.583468171,3.268101717,7.330936403));
#104123=CARTESIAN_POINT('Ctrl Pts',(1.980405062,3.203647866,7.245198798));
#104124=CARTESIAN_POINT('Ctrl Pts',(2.365763869,3.138525418,7.117103436));
#104125=CARTESIAN_POINT('',(1.76679318523583,3.26733592572127,7.03142530529778));
#104126=CARTESIAN_POINT('Origin',(-0.075896083697797,3.08931092501544,-0.181838197832388));
#104127=CARTESIAN_POINT('Ctrl Pts',(1.82645774549794,3.22840426964308,7.27420456827652));
#104128=CARTESIAN_POINT('Ctrl Pts',(1.81660431903139,3.23458082932623,7.23367836066828));
#104129=CARTESIAN_POINT('Ctrl Pts',(1.80670332193979,3.24090849486778,7.19316158940839));
#104130=CARTESIAN_POINT('Ctrl Pts',(1.7868217117759,3.25387487498457,7.11224834650389));
#104131=CARTESIAN_POINT('Ctrl Pts',(1.77682923752812,3.26052132408962,7.07180357369656));
#104132=CARTESIAN_POINT('Ctrl Pts',(1.76679318372669,3.26733592512765,7.03142530650721));
#104133=CARTESIAN_POINT('Ctrl Pts',(0.990540534000001,3.138525418,7.182014303));
#104134=CARTESIAN_POINT('Ctrl Pts',(1.220913599,3.176642188,7.150241342));
#104135=CARTESIAN_POINT('Ctrl Pts',(1.448776863,3.214285714,7.103769816));
#104136=CARTESIAN_POINT('Ctrl Pts',(1.610929454,3.241073689,7.07069964));
#104137=CARTESIAN_POINT('Ctrl Pts',(1.771404205,3.268112745,7.03026508300001));
#104138=CARTESIAN_POINT('Ctrl Pts',(1.267805044,3.138525418,7.392068071));
#104139=CARTESIAN_POINT('Ctrl Pts',(1.504915875,3.176642188,7.351401467));
#104140=CARTESIAN_POINT('Ctrl Pts',(1.738933089,3.214285714,7.295622778));
#104141=CARTESIAN_POINT('Ctrl Pts',(1.905464967,3.241073689,7.255929416));
#104142=CARTESIAN_POINT('Ctrl Pts',(2.070012238,3.268112745,7.208678751));
#104143=CARTESIAN_POINT('Ctrl Pts',(0.990540544201338,3.13852541968788,
7.18201430159303));
#104144=CARTESIAN_POINT('Ctrl Pts',(1.14451922017561,3.16400222521989,7.16077762395493));
#104145=CARTESIAN_POINT('Ctrl Pts',(1.29741506331278,3.18928040271736,7.13463926685995));
#104146=CARTESIAN_POINT('Ctrl Pts',(1.44877686277554,3.21428571395516,7.1037698160864));
#104147=CARTESIAN_POINT('Ctrl Pts',(1.55505543508907,3.23184317462731,7.08209485501571));
#104148=CARTESIAN_POINT('Ctrl Pts',(1.66111643389606,3.24953506298842,7.057978808402));
#104149=CARTESIAN_POINT('Ctrl Pts',(1.76679318731429,3.26733592562012,7.03142530616991));
#104150=CARTESIAN_POINT('Ctrl Pts',(0.209276124,3.268101717,7.246978923));
#104151=CARTESIAN_POINT('Ctrl Pts',(0.601667098,3.203647866,7.235647572));
#104152=CARTESIAN_POINT('Ctrl Pts',(0.990540534,3.138525418,7.18201430300001));
#104153=CARTESIAN_POINT('Ctrl Pts',(-0.029487061,3.268101717,7.499942034));
#104154=CARTESIAN_POINT('Ctrl Pts',(0.376600717,3.203647866,7.501538624));
#104155=CARTESIAN_POINT('Ctrl Pts',(0.780486766,3.138525418,7.459278813));
#104156=CARTESIAN_POINT('',(0.213937949517071,3.26733592599679,7.24684279804168));
#104157=CARTESIAN_POINT('Origin',(-0.0350318247030968,3.08931099397693,
-0.193902277461947));
#104158=CARTESIAN_POINT('Ctrl Pts',(0.220017220171418,3.22840426961572,
7.49677213338353));
#104159=CARTESIAN_POINT('Ctrl Pts',(0.219106098112348,3.23458082928566,
7.45507521069873));
#104160=CARTESIAN_POINT('Ctrl Pts',(0.218146489016196,3.24090849485656,
7.41337727728728));
#104161=CARTESIAN_POINT('Ctrl Pts',(0.216123655392674,3.25387487502344,
7.33008178262261));
#104162=CARTESIAN_POINT('Ctrl Pts',(0.215059230316357,3.2605213241711,7.28843449952145));
#104163=CARTESIAN_POINT('Ctrl Pts',(0.213937947891238,3.26733592525954,
7.24684279881095));
#104164=CARTESIAN_POINT('Ctrl Pts',(-0.576538529,3.138525418,7.22703973500001));
#104165=CARTESIAN_POINT('Ctrl Pts',(-0.344721211,3.176642188,7.245533007));
#104166=CARTESIAN_POINT('Ctrl Pts',(-0.112195259,3.214285714,7.249131826));
#104167=CARTESIAN_POINT('Ctrl Pts',(0.053275404,3.241073689,7.251692825));
#104168=CARTESIAN_POINT('Ctrl Pts',(0.218690579,3.268112745,7.246700934));
#104169=CARTESIAN_POINT('Ctrl Pts',(-0.350911661,3.138525418,7.491786236));
#104170=CARTESIAN_POINT('Ctrl Pts',(-0.110602232,3.176642188,7.503042214));
#104171=CARTESIAN_POINT('Ctrl Pts',(0.129934559,3.214285714,7.498874383));
#104172=CARTESIAN_POINT('Ctrl Pts',(0.301105915,3.241073689,7.495908461));
#104173=CARTESIAN_POINT('Ctrl Pts',(0.471963657,3.268112745,7.48513529));
#104174=CARTESIAN_POINT('Ctrl Pts',(-0.576538527796137,3.13852541819795,
7.22703973509604));
#104175=CARTESIAN_POINT('Ctrl Pts',(-0.421594524022473,3.16400222467753,
7.23940042350238));
#104176=CARTESIAN_POINT('Ctrl Pts',(-0.266654323353934,3.18928040268826,
7.24674125354813));
#104177=CARTESIAN_POINT('Ctrl Pts',(-0.112195259170487,3.21428571394946,
7.24913182614134));
#104178=CARTESIAN_POINT('Ctrl Pts',(-0.00374194548841267,3.23184317462932,
7.25081036419421));
#104179=CARTESIAN_POINT('Ctrl Pts',(0.105023642990151,3.24953506292902,
7.25005811714051));
#104180=CARTESIAN_POINT('Ctrl Pts',(0.213937950775892,3.26733592562386,
7.24684279936316));
#104181=CARTESIAN_POINT('Ctrl Pts',(0.209418136,2.750764179,7.24697482));
#104182=CARTESIAN_POINT('Ctrl Pts',(0.602103436,2.686419405,7.23562726800001));
#104183=CARTESIAN_POINT('Ctrl Pts',(0.991263375,2.621296797,7.181914572));
#104184=CARTESIAN_POINT('Ctrl Pts',(-0.029340091,2.750764179,7.49994261));
#104185=CARTESIAN_POINT('Ctrl Pts',(0.377052547,2.686419405,7.501532435));
#104186=CARTESIAN_POINT('Ctrl Pts',(0.781237513,2.621296797,7.459200222));
#104187=CARTESIAN_POINT('',(0.220796265851338,2.71105259873596,7.49674922941056));
#104188=CARTESIAN_POINT('',(0.78123750409061,2.62129679635371,7.45920022219058));
#104189=CARTESIAN_POINT('Origin',(-0.0306335706061751,2.55359536576098,
-0.188118757216246));
#104190=CARTESIAN_POINT('',(0.886250432112382,2.62129679507543,7.32055739843915));
#104191=CARTESIAN_POINT('Ctrl Pts',(0.220796264044513,2.7110525987386,7.49674922945498));
#104192=CARTESIAN_POINT('Ctrl Pts',(0.21978045853249,2.71723336186804,7.45505532086205));
#104193=CARTESIAN_POINT('Ctrl Pts',(0.218715591035989,2.72356451335006,
7.41336050560342));
#104194=CARTESIAN_POINT('Ctrl Pts',(0.216481064139124,2.73653622859594,
7.3300712036522));
#104195=CARTESIAN_POINT('Ctrl Pts',(0.215310080965755,2.74318451391785,
7.28842710414731));
#104196=CARTESIAN_POINT('Ctrl Pts',(0.214081499284118,2.74999999976668,
7.24683856077415));
#104197=CARTESIAN_POINT('Ctrl Pts',(0.973607978338463,2.61844385667099,
7.1840212125146));
#104198=CARTESIAN_POINT('Ctrl Pts',(0.982251746853771,2.61987032683551,
7.18282857737324));
#104199=CARTESIAN_POINT('Ctrl Pts',(0.990895515369072,2.621296797,7.18163594223189));
#104200=CARTESIAN_POINT('Ctrl Pts',(1.16527946970092,2.65007516,7.15757509057275));
#104201=CARTESIAN_POINT('Ctrl Pts',(1.33829010954023,2.678571429,7.12507882876051));
#104202=CARTESIAN_POINT('Ctrl Pts',(1.56242740907838,2.71548867740086,7.0829795422579));
#104203=CARTESIAN_POINT('Ctrl Pts',(1.78347548629995,2.75286253809926,7.02687582964737));
#104204=CARTESIAN_POINT('Ctrl Pts',(1.25075524478722,2.61844385667099,7.3949940680899));
#104205=CARTESIAN_POINT('Ctrl Pts',(1.25965213439361,2.61987032683551,7.39346725104492));
#104206=CARTESIAN_POINT('Ctrl Pts',(1.268549024,2.621296797,7.391940434));
#104207=CARTESIAN_POINT('Ctrl Pts',(1.448039577,2.65007516,7.36113762));
#104208=CARTESIAN_POINT('Ctrl Pts',(1.625823574,2.678571429,7.321659491));
#104209=CARTESIAN_POINT('Ctrl Pts',(1.85614481325012,2.71548867740086,7.27051511554235));
#104210=CARTESIAN_POINT('Ctrl Pts',(2.08279609425964,2.75286253809926,7.20499551915523));
#104211=CARTESIAN_POINT('',(1.2685490159974,2.62129679728566,7.39194043464768));
#104212=CARTESIAN_POINT('',(1.82721365441677,2.71105259873355,7.274014727662));
#104213=CARTESIAN_POINT('Ctrl Pts',(1.26854901542751,2.62129679564634,7.3919404353506));
#104214=CARTESIAN_POINT('Ctrl Pts',(1.38846606602389,2.64052352569893,7.3713611762831));
#104215=CARTESIAN_POINT('Ctrl Pts',(1.50762429264484,2.65962575012036,7.34790643424406));
#104216=CARTESIAN_POINT('Ctrl Pts',(1.62582357463579,2.67857142910191,7.32165949085882));
#104217=CARTESIAN_POINT('Ctrl Pts',(1.69306819243097,2.68934979355907,7.30672737260246));
#104218=CARTESIAN_POINT('Ctrl Pts',(1.76021149589615,2.700178795349,7.29084549616751));
#104219=CARTESIAN_POINT('Ctrl Pts',(1.8272136579073,2.71105259956491,7.27401472665962));
#104220=CARTESIAN_POINT('Ctrl Pts',(1.76693247010815,2.74999999878156,7.03139031416154));
#104221=CARTESIAN_POINT('Ctrl Pts',(1.77707263608141,2.74318451273276,7.0717424329524));
#104222=CARTESIAN_POINT('Ctrl Pts',(1.78716849160209,2.7365362282126,7.11216118490206));
#104223=CARTESIAN_POINT('Ctrl Pts',(1.80725542865157,2.72356456848111,7.19302252591549));
#104224=CARTESIAN_POINT('Ctrl Pts',(1.81725845691741,2.7172334745408,7.23351322974473));
#104225=CARTESIAN_POINT('Ctrl Pts',(1.82721365293153,2.71105259873601,7.27401472802745));
#104226=CARTESIAN_POINT('',(1.12851976597305,2.62129679787127,7.28587737450813));
#104227=CARTESIAN_POINT('Origin',(-6.51605505663788E-14,2.71213386199978,
-4.91794105439425E-13));
#104228=CARTESIAN_POINT('',(1.82013710546422,2.53084202099703,7.27578867997899));
#104229=CARTESIAN_POINT('Origin',(-0.043300880352663,2.55357150927427,-0.188109139924416));
#104230=CARTESIAN_POINT('',(2.36648016134961,2.62129679635371,7.11686529608004));
#104231=CARTESIAN_POINT('Origin',(-0.0266746806644327,2.41079133695599,
-0.185773302817498));
#104232=CARTESIAN_POINT('Origin',(-0.0703573078924483,2.55359539449515,
-0.177135215677642));
#104233=CARTESIAN_POINT('Ctrl Pts',(1.762407424,2.750764179,7.032525867));
#104234=CARTESIAN_POINT('Ctrl Pts',(2.143472571,2.686419405,6.937027883));
#104235=CARTESIAN_POINT('Ctrl Pts',(2.511987525,2.621296797,6.800913077));
#104236=CARTESIAN_POINT('Ctrl Pts',(1.583611829,2.750764179,7.330905372));
#104237=CARTESIAN_POINT('Ctrl Pts',(1.980844998,2.686419405,7.245095624));
#104238=CARTESIAN_POINT('Ctrl Pts',(2.36648017,2.621296797,7.11686529400001));
#104239=CARTESIAN_POINT('',(2.43923383619956,2.62129679507541,6.95888918946105));
#104240=CARTESIAN_POINT('Ctrl Pts',(2.4951977760081,2.61844385818249,6.80676585075237));
#104241=CARTESIAN_POINT('Ctrl Pts',(2.50338307239038,2.61987032759123,6.80374294562012));
#104242=CARTESIAN_POINT('Ctrl Pts',(2.51156836877267,2.621296797,6.80072004048786));
#104243=CARTESIAN_POINT('Ctrl Pts',(2.67670295147414,2.65007516,6.73973432240921));
#104244=CARTESIAN_POINT('Ctrl Pts',(2.83868296268772,2.678571429,6.67080563183334));
#104245=CARTESIAN_POINT('Ctrl Pts',(3.04852995024692,2.71548867657569,6.58150771068758));
#104246=CARTESIAN_POINT('Ctrl Pts',(3.25234940257738,2.75286253643016,6.47919687125863));
#104247=CARTESIAN_POINT('Ctrl Pts',(2.81121842139337,2.61844385818249,6.95322780681343));
#104248=CARTESIAN_POINT('Ctrl Pts',(2.81957908169667,2.61987032759123,6.9498241194067));
#104249=CARTESIAN_POINT('Ctrl Pts',(2.827939742,2.621296797,6.94642043200001));
#104250=CARTESIAN_POINT('Ctrl Pts',(2.996612211,2.65007516,6.877752607));
#104251=CARTESIAN_POINT('Ctrl Pts',(3.161753086,2.678571429,6.800979152));
#104252=CARTESIAN_POINT('Ctrl Pts',(3.37569500904041,2.71548867657569,6.70151824740522));
#104253=CARTESIAN_POINT('Ctrl Pts',(3.58296252864191,2.75286253643016,6.5888071390405));
#104254=CARTESIAN_POINT('',(2.82793973434138,2.62129679728565,6.94642043436071));
#104255=CARTESIAN_POINT('',(3.34819256234123,2.71105259871154,6.71115538203994));
#104256=CARTESIAN_POINT('Ctrl Pts',(2.82793973391823,2.62129679564642,6.94642043516145));
#104257=CARTESIAN_POINT('Ctrl Pts',(2.94062925804215,2.64052352569915,6.90054368625749));
#104258=CARTESIAN_POINT('Ctrl Pts',(3.051959555225,2.65962575012078,6.85202180692739));
#104259=CARTESIAN_POINT('Ctrl Pts',(3.16175308677398,2.67857142917795,6.80097915141693));
#104260=CARTESIAN_POINT('Ctrl Pts',(3.22421559883867,2.6893497936752,6.77194053245832));
#104261=CARTESIAN_POINT('Ctrl Pts',(3.2863749950427,2.70017879535709,6.74199614030809));
#104262=CARTESIAN_POINT('Ctrl Pts',(3.34819256604841,2.71105259960124,6.71115538033925));
#104263=CARTESIAN_POINT('Ctrl Pts',(3.23716364257135,2.74999999863177,6.4871620652196));
#104264=CARTESIAN_POINT('Ctrl Pts',(3.25574124978409,2.74318451259148,6.52439093806489));
#104265=CARTESIAN_POINT('Ctrl Pts',(3.2742899063226,2.73653622817571,6.56169441112101));
#104266=CARTESIAN_POINT('Ctrl Pts',(3.31129000836468,2.72356457243949,6.6363471384988));
#104267=CARTESIAN_POINT('Ctrl Pts',(3.32976346291393,2.71723348259965,6.67374081089451));
#104268=CARTESIAN_POINT('Ctrl Pts',(3.34819256082344,2.7110525987141,6.71115538278798));
#104269=CARTESIAN_POINT('',(2.66838386743254,2.62129679787125,6.87293921965941));
#104270=CARTESIAN_POINT('Origin',(-2.45897052719712E-13,2.71213386199967,
-5.34294830600857E-13));
#104271=CARTESIAN_POINT('',(3.34166280795518,2.53084202104404,6.71440910846402));
#104272=CARTESIAN_POINT('Origin',(-0.0827265554844064,2.55357150385517,
-0.174403115639424));
#104273=CARTESIAN_POINT('',(3.84106883469457,2.6212967963465,6.44175365808321));
#104274=CARTESIAN_POINT('Origin',(-0.0659866317829577,2.41079129086726,
-0.17569542402967));
#104275=CARTESIAN_POINT('Origin',(-0.106791213493976,2.55359538133709,-0.157869104366971));
#104276=CARTESIAN_POINT('Ctrl Pts',(3.232988499,2.750764179,6.489243821));
#104277=CARTESIAN_POINT('Ctrl Pts',(3.584615312,2.686419405,6.314060784));
#104278=CARTESIAN_POINT('Ctrl Pts',(3.91525393,2.621296797,6.101908444));
#104279=CARTESIAN_POINT('Ctrl Pts',(3.122515819,2.750764179,6.819083146));
#104280=CARTESIAN_POINT('Ctrl Pts',(3.492015338,2.686419405,6.649886193));
#104281=CARTESIAN_POINT('Ctrl Pts',(3.841068843,2.621296797,6.44175365400001));
#104282=CARTESIAN_POINT('',(3.87816137631514,2.62129679507539,6.27183105529777));
#104283=CARTESIAN_POINT('Ctrl Pts',(3.90011488472912,2.6184438573276,6.11123368563928));
#104284=CARTESIAN_POINT('Ctrl Pts',(3.90745898043263,2.61987032716382,6.10652185619153));
#104285=CARTESIAN_POINT('Ctrl Pts',(3.91480307613613,2.621296797,6.10181002674376));
#104286=CARTESIAN_POINT('Ctrl Pts',(4.06296677837533,2.65007516,6.00675106734493));
#104287=CARTESIAN_POINT('Ctrl Pts',(4.20634215577609,2.678571429,5.90461297703037));
#104288=CARTESIAN_POINT('Ctrl Pts',(4.3920866264194,2.71548867704315,5.77229189108124));
#104289=CARTESIAN_POINT('Ctrl Pts',(4.5691470888706,2.75286253737571,5.62855786246398));
#104290=CARTESIAN_POINT('Ctrl Pts',(4.24023213436743,2.6184438573276,6.18633634586204));
#104291=CARTESIAN_POINT('Ctrl Pts',(4.24766563718371,2.61987032716382,6.18121493843102));
#104292=CARTESIAN_POINT('Ctrl Pts',(4.25509914,2.621296797,6.176093531));
#104293=CARTESIAN_POINT('Ctrl Pts',(4.405066589,2.65007516,6.072771527));
#104294=CARTESIAN_POINT('Ctrl Pts',(4.549842538,2.678571429,5.962292586));
#104295=CARTESIAN_POINT('Ctrl Pts',(4.7374014663965,2.71548867704315,5.81916583099209));
#104296=CARTESIAN_POINT('Ctrl Pts',(4.91559363147713,2.75286253737572,5.66453345430643));
#104297=CARTESIAN_POINT('',(4.25509913306813,2.62129679728565,6.17609353496064));
#104298=CARTESIAN_POINT('',(4.71261370775416,2.71105259867233,5.83448986989362));
#104299=CARTESIAN_POINT('Ctrl Pts',(4.25509913278686,2.62129679564643,6.17609353582486));
#104300=CARTESIAN_POINT('Ctrl Pts',(4.35529189432767,2.64052352569895,6.107064443424));
#104301=CARTESIAN_POINT('Ctrl Pts',(4.45358858142186,2.65962575012078,6.0357442557464));
#104302=CARTESIAN_POINT('Ctrl Pts',(4.54984253890747,2.67857142917862,5.9622925853075));
#104303=CARTESIAN_POINT('Ctrl Pts',(4.60460226774719,2.68934979366353,5.92050527950756));
#104304=CARTESIAN_POINT('Ctrl Pts',(4.65887125227467,2.70017879533289,5.8778985378832));
#104305=CARTESIAN_POINT('Ctrl Pts',(4.71261371105953,2.71105259956698,5.83448986743041));
#104306=CARTESIAN_POINT('Ctrl Pts',(4.55602864061065,2.74999999872861,5.63960132741109));
#104307=CARTESIAN_POINT('Ctrl Pts',(4.58217502072053,2.74318451267426,5.67196617370914));
#104308=CARTESIAN_POINT('Ctrl Pts',(4.60830916400747,2.73653622822078,5.70441009965228));
#104309=CARTESIAN_POINT('Ctrl Pts',(4.66049235264123,2.72356457274487,5.76936355819353));
#104310=CARTESIAN_POINT('Ctrl Pts',(4.68657244090915,2.71723348320718,5.80191173891234));
#104311=CARTESIAN_POINT('Ctrl Pts',(4.71261370641489,2.71105259867639,5.83448987095173));
#104312=CARTESIAN_POINT('',(4.08347730449991,2.62129679787124,6.13863006502524));
#104313=CARTESIAN_POINT('Origin',(-5.5120838449163E-13,2.71213386200022,
-7.7715611723761E-13));
#104314=CARTESIAN_POINT('',(4.706936069564,2.53084202106156,5.8390712305403));
#104315=CARTESIAN_POINT('Origin',(-0.118283871844512,2.55357148116036,-0.152541779600568));
#104316=CARTESIAN_POINT('',(5.1360534000227,2.62129679635372,5.46543277858561));
#104317=CARTESIAN_POINT('Origin',(-0.102213261879857,2.41079127246662,-0.157402635827827));
#104318=CARTESIAN_POINT('Origin',(-0.138231744102897,2.55359539255566,-0.131221323923163));
#104319=CARTESIAN_POINT('Ctrl Pts',(4.552398626,2.750764179,5.642531945));
#104320=CARTESIAN_POINT('Ctrl Pts',(4.858145424,2.686419405,5.39585522));
#104321=CARTESIAN_POINT('Ctrl Pts',(5.135447414,2.621296797,5.117585355));
#104322=CARTESIAN_POINT('Ctrl Pts',(4.51541444,2.750764179,5.988408172));
#104323=CARTESIAN_POINT('Ctrl Pts',(4.839902922,2.686419405,5.743735475));
#104324=CARTESIAN_POINT('Ctrl Pts',(5.136053407,2.621296797,5.465432773));
#104325=CARTESIAN_POINT('',(5.13575040190729,2.62129679507543,5.29150907233978));
#104326=CARTESIAN_POINT('Ctrl Pts',(5.12266696414755,2.6184438576685,5.12994702347875));
#104327=CARTESIAN_POINT('Ctrl Pts',(5.12882645412125,2.61987032733427,5.12376659120871));
#104328=CARTESIAN_POINT('Ctrl Pts',(5.13498594409497,2.621296797,5.11758615893868));
#104329=CARTESIAN_POINT('Ctrl Pts',(5.25925079361522,2.65007516,4.99289880831642));
#104330=CARTESIAN_POINT('Ctrl Pts',(5.37731746396822,2.678571429,4.86232718154151));
#104331=CARTESIAN_POINT('Ctrl Pts',(5.53027420987107,2.71548867689151,4.69317011968511));
#104332=CARTESIAN_POINT('Ctrl Pts',(5.67229652933867,2.75286253706899,4.51473374810968));
#104333=CARTESIAN_POINT('Ctrl Pts',(5.47097731265819,2.6184438576685,5.13017866966202));
#104334=CARTESIAN_POINT('Ctrl Pts',(5.47713607232912,2.61987032733427,5.12357901533102));
#104335=CARTESIAN_POINT('Ctrl Pts',(5.483294832,2.621296797,5.11697936100001));
#104336=CARTESIAN_POINT('Ctrl Pts',(5.607544948,2.65007516,4.9838344));
#104337=CARTESIAN_POINT('Ctrl Pts',(5.72518641,2.678571429,4.844815845));
#104338=CARTESIAN_POINT('Ctrl Pts',(5.87759229249829,2.71548867689151,4.66471569004545));
#104339=CARTESIAN_POINT('Ctrl Pts',(6.01837703291872,2.75286253706899,4.47539248510704));
#104340=CARTESIAN_POINT('',(5.48329482857351,2.62129679727529,5.11697936459));
#104341=CARTESIAN_POINT('',(5.8566782740463,2.71105259871343,4.68501009565352));
#104342=CARTESIAN_POINT('Ctrl Pts',(5.48329482599272,2.62129679564642,5.11697936726269));
#104343=CARTESIAN_POINT('Ctrl Pts',(5.56630592160011,2.64052352569898,5.02802565495659));
#104344=CARTESIAN_POINT('Ctrl Pts',(5.64697275466975,2.65962575012044,4.93724201144345));
#104345=CARTESIAN_POINT('Ctrl Pts',(5.72518641047971,2.6785714291162,4.84481584443312));
#104346=CARTESIAN_POINT('Ctrl Pts',(5.76968285161177,2.68934979357867,4.79223377992844));
#104347=CARTESIAN_POINT('Ctrl Pts',(5.8135238678287,2.70017879536078,4.73895693236883));
#104348=CARTESIAN_POINT('Ctrl Pts',(5.85667827678894,2.71105259961095,4.68501009253177));
#104349=CARTESIAN_POINT('Ctrl Pts',(5.66185880256267,2.74999999874769,4.52833910004848));
#104350=CARTESIAN_POINT('Ctrl Pts',(5.69435138006959,2.74318451271068,4.55432657530881));
#104351=CARTESIAN_POINT('Ctrl Pts',(5.72684900677654,2.73653622824737,4.58039391203204));
#104352=CARTESIAN_POINT('Ctrl Pts',(5.79177555439265,2.72356451299752,4.63261119234889));
#104353=CARTESIAN_POINT('Ctrl Pts',(5.82424314025865,2.71723336167496,4.6587922416216));
#104354=CARTESIAN_POINT('Ctrl Pts',(5.85667827296397,2.711052598716,4.68501009699311));
#104355=CARTESIAN_POINT('',(5.30763188220032,2.62129679787124,5.11728539181767));
#104356=CARTESIAN_POINT('Origin',(1.64928834478495E-12,2.71213386199944,
1.26157764790413E-12));
#104357=CARTESIAN_POINT('',(5.85211823264317,2.53084202101063,4.69070487109297));
#104358=CARTESIAN_POINT('Origin',(-0.148310339986101,2.5535715273533,-0.123547826992701));
#104359=CARTESIAN_POINT('',(6.19088181638272,2.62129679635371,4.23355433693757));
#104360=CARTESIAN_POINT('Origin',(-0.133660426319354,2.4107913065854,-0.131749774071899));
#104361=CARTESIAN_POINT('Origin',(-0.163208568664093,2.55359543573746,-0.0984376405150228));
#104362=CARTESIAN_POINT('Ctrl Pts',(5.658943652,2.750764179,4.531981548));
#104363=CARTESIAN_POINT('Ctrl Pts',(5.90451405500001,2.686419405,4.225345463));
#104364=CARTESIAN_POINT('Ctrl Pts',(6.115513083,2.621296797,3.893969662));
#104365=CARTESIAN_POINT('Ctrl Pts',(5.69717730100001,2.750764179,4.877721886));
#104366=CARTESIAN_POINT('Ctrl Pts',(5.961482025,2.686419405,4.56901407));
#104367=CARTESIAN_POINT('Ctrl Pts',(6.190881822,2.621296797,4.23355433));
#104368=CARTESIAN_POINT('',(6.15319744590099,2.62129679507543,4.06376200599198));
#104369=CARTESIAN_POINT('Ctrl Pts',(6.10568883044446,2.61844385890977,3.908789733995));
#104370=CARTESIAN_POINT('Ctrl Pts',(6.11037570273752,2.61987032795487,3.90142969174084));
#104371=CARTESIAN_POINT('Ctrl Pts',(6.11506257503053,2.621296797,3.89406964948668));
#104372=CARTESIAN_POINT('Ctrl Pts',(6.20961808792042,2.65007516,3.74558415068812));
#104373=CARTESIAN_POINT('Ctrl Pts',(6.29685538488361,2.678571429,3.5926843721594));
#104374=CARTESIAN_POINT('Ctrl Pts',(6.40987231768519,2.71548867633322,3.39460093130149));
#104375=CARTESIAN_POINT('Ctrl Pts',(6.51021568666705,2.75286253593971,3.18980570664055));
#104376=CARTESIAN_POINT('Ctrl Pts',(6.44590567465352,2.61844385890977,3.83413953496176));
#104377=CARTESIAN_POINT('Ctrl Pts',(6.45050171332678,2.61987032795487,3.82637022898089));
#104378=CARTESIAN_POINT('Ctrl Pts',(6.455097752,2.621296797,3.818600923));
#104379=CARTESIAN_POINT('Ctrl Pts',(6.54782073800001,2.65007516,3.661858715));
#104380=CARTESIAN_POINT('Ctrl Pts',(6.632826928,2.678571429,3.5008009));
#104381=CARTESIAN_POINT('Ctrl Pts',(6.74295343410217,2.71548867633322,3.29214863009078));
#104382=CARTESIAN_POINT('Ctrl Pts',(6.83974781229092,2.75286253593971,3.07698714219965));
#104383=CARTESIAN_POINT('',(6.45509774941754,2.62129679727529,3.81860092724444));
#104384=CARTESIAN_POINT('',(6.72689107318539,2.71105259873439,3.31646445626091));
#104385=CARTESIAN_POINT('Ctrl Pts',(6.45509774747939,2.62129679564641,3.81860093040773));
#104386=CARTESIAN_POINT('Ctrl Pts',(6.51704567080351,2.6405235256991,3.71388197465405));
#104387=CARTESIAN_POINT('Ctrl Pts',(6.57631075817407,2.65962575012053,3.60787981774369));
#104388=CARTESIAN_POINT('Ctrl Pts',(6.63282692833652,2.67857142913362,3.50080089926179));
#104389=CARTESIAN_POINT('Ctrl Pts',(6.66497947777494,2.68934979361287,3.43988275458253));
#104390=CARTESIAN_POINT('Ctrl Pts',(6.69634256801951,2.7001787953686,3.37842696767933));
#104391=CARTESIAN_POINT('Ctrl Pts',(6.72689107500102,2.71105259961325,3.31646445271963));
#104392=CARTESIAN_POINT('Ctrl Pts',(6.50294674033191,2.74999999863963,3.20533676975677));
#104393=CARTESIAN_POINT('Ctrl Pts',(6.54026619870976,2.74318451256571,3.22373172851576));
#104394=CARTESIAN_POINT('Ctrl Pts',(6.57760775536954,2.73653622819314,3.24220359592826));
#104395=CARTESIAN_POINT('Ctrl Pts',(6.65224119207437,2.7235645713651,3.27924260980075));
#104396=CARTESIAN_POINT('Ctrl Pts',(6.68957747437631,2.71723348043905,3.29783179808093));
#104397=CARTESIAN_POINT('Ctrl Pts',(6.72689107244661,2.71105259873694,3.31646445774123));
#104398=CARTESIAN_POINT('',(6.28360749135913,2.62129679787126,3.85666214075026));
#104399=CARTESIAN_POINT('Origin',(7.74987712892639E-13,2.71213386200022,
3.90746462963776E-13));
#104400=CARTESIAN_POINT('',(6.72366185127617,2.53084202102611,3.32300636522807));
#104401=CARTESIAN_POINT('Origin',(-0.171402024182553,2.55357154600533,-0.0887769892027829));
#104402=CARTESIAN_POINT('',(6.9562314790131,2.62129679635372,2.80371959999944));
#104403=CARTESIAN_POINT('Origin',(-0.158857905554866,2.41079127488136,-0.0999365371658045));
#104404=CARTESIAN_POINT('Origin',(-0.18055420549716,2.55359536942784,-0.0610512706728089));
#104405=CARTESIAN_POINT('Ctrl Pts',(6.500882762,2.750764179,3.209520729));
#104406=CARTESIAN_POINT('Ctrl Pts',(6.674794172,2.686419405,2.857263248));
#104407=CARTESIAN_POINT('Ctrl Pts',(6.809624158,2.621296797,2.488276275));
#104408=CARTESIAN_POINT('Ctrl Pts',(6.612546483,2.750764179,3.538958747));
#104409=CARTESIAN_POINT('Ctrl Pts',(6.804308854,2.686419405,3.180650644));
#104410=CARTESIAN_POINT('Ctrl Pts',(6.956231483,2.621296797,2.803719592));
#104411=CARTESIAN_POINT('',(6.88292781620325,2.62129679507543,2.64599794467697));
#104412=CARTESIAN_POINT('Ctrl Pts',(6.80321546550788,2.61844385762072,2.50486179331884));
#104413=CARTESIAN_POINT('Ctrl Pts',(6.80621057117267,2.61987032731036,2.496666282065));
#104414=CARTESIAN_POINT('Ctrl Pts',(6.8092056768374,2.621296797,2.48847077081115));
#104415=CARTESIAN_POINT('Ctrl Pts',(6.86963054157133,2.65007516,2.3231301403394));
#104416=CARTESIAN_POINT('Ctrl Pts',(6.9219593459294,2.678571429,2.15505163367438));
#104417=CARTESIAN_POINT('Ctrl Pts',(6.98975192156349,2.71548867687936,1.93730397120084));
#104418=CARTESIAN_POINT('Ctrl Pts',(7.04372440045867,2.75286253704441,1.71572588267085));
#104419=CARTESIAN_POINT('Ctrl Pts',(7.11943064298699,2.61844385762072,2.35882031047265));
#104420=CARTESIAN_POINT('Ctrl Pts',(7.12224905899349,2.61987032731036,2.35024463023634));
#104421=CARTESIAN_POINT('Ctrl Pts',(7.125067475,2.621296797,2.34166895));
#104422=CARTESIAN_POINT('Ctrl Pts',(7.181927708,2.65007516,2.168658587));
#104423=CARTESIAN_POINT('Ctrl Pts',(7.230323831,2.678571429,1.993092396));
#104424=CARTESIAN_POINT('Ctrl Pts',(7.29302157140247,2.71548867687936,1.76564435329171));
#104425=CARTESIAN_POINT('Ctrl Pts',(7.34129959039367,2.75286253704441,1.53470528735004));
#104426=CARTESIAN_POINT('',(7.12506747340202,2.62129679727527,2.34166895469459));
#104427=CARTESIAN_POINT('',(7.28256192199589,2.71105259871254,1.79284462519801));
#104428=CARTESIAN_POINT('Ctrl Pts',(7.12506747217799,2.62129679564649,2.34166895820572));
#104429=CARTESIAN_POINT('Ctrl Pts',(7.1630556076896,2.64052352569902,2.22608130136333));
#104430=CARTESIAN_POINT('Ctrl Pts',(7.19814777998631,2.65962575012048,2.10981717414423));
#104431=CARTESIAN_POINT('Ctrl Pts',(7.23032383120981,2.67857142912354,1.99309239523888));
#104432=CARTESIAN_POINT('Ctrl Pts',(7.24862907160098,2.68934979359008,1.92668663526634));
#104433=CARTESIAN_POINT('Ctrl Pts',(7.26604773257138,2.70017879536209,1.85992551309353));
#104434=CARTESIAN_POINT('Ctrl Pts',(7.28256192321581,2.7110525996155,1.79284462117634));
#104435=CARTESIAN_POINT('Ctrl Pts',(7.03996411563262,2.74999999865509,1.73245645342098));
#104436=CARTESIAN_POINT('Ctrl Pts',(7.08036543800852,2.74318451258415,1.74239876792937));
#104437=CARTESIAN_POINT('Ctrl Pts',(7.12080487551331,2.73653622815888,1.75241144266083));
#104438=CARTESIAN_POINT('Ctrl Pts',(7.20165608093836,2.72356451293218,1.7725406130909));
#104439=CARTESIAN_POINT('Ctrl Pts',(7.2421160008973,2.71723336163673,1.78266910448064));
#104440=CARTESIAN_POINT('Ctrl Pts',(7.28256192157163,2.71105259871514,1.79284462688592));
#104441=CARTESIAN_POINT('',(6.96576859816398,2.62129679787115,2.41570565417414));
#104442=CARTESIAN_POINT('Origin',(-7.2251232774434E-13,2.71213386199956,
-9.75781955236954E-14));
#104443=CARTESIAN_POINT('',(7.28081451506275,2.53084202101684,1.79992777426825));
#104444=CARTESIAN_POINT('Origin',(-0.18647930638377,2.55357153497555,-0.0498551051272444));
#104445=CARTESIAN_POINT('',(7.39631548980067,2.62129679635372,1.24278605063635));
#104446=CARTESIAN_POINT('Origin',(-0.176627145807934,2.41079128197683,-0.0634502949292973));
#104447=CARTESIAN_POINT('Origin',(-0.189457227616135,2.55359537483203,-0.0208101339617175));
#104448=CARTESIAN_POINT('Ctrl Pts',(7.03884782,2.750764179,1.736986289));
#104449=CARTESIAN_POINT('Ctrl Pts',(7.132968332,2.686419405,1.35557858));
#104450=CARTESIAN_POINT('Ctrl Pts',(7.185324776,2.621296797,0.966233856));
#104451=CARTESIAN_POINT('Ctrl Pts',(7.21872034000001,2.750764179,2.03471783));
#104452=CARTESIAN_POINT('Ctrl Pts',(7.328973763,2.686419405,1.64356353));
#104453=CARTESIAN_POINT('Ctrl Pts',(7.396315492,2.621296797,1.242786042));
#104454=CARTESIAN_POINT('',(7.29082013220642,2.62129679507543,1.10450996083933));
#104455=CARTESIAN_POINT('Ctrl Pts',(7.18263131216403,2.61844385838297,0.983809288891911));
#104456=CARTESIAN_POINT('Ctrl Pts',(7.18379460089475,2.61987032769149,0.97516152725879));
#104457=CARTESIAN_POINT('Ctrl Pts',(7.18495788962543,2.621296797,0.96651376562567));
#104458=CARTESIAN_POINT('Ctrl Pts',(7.20842670536899,2.65007516,0.792049147333845));
#104459=CARTESIAN_POINT('Ctrl Pts',(7.22340018149012,2.678571429,0.616651075659592));
#104460=CARTESIAN_POINT('Ctrl Pts',(7.24279849383286,2.71548867651787,0.389420835413089));
#104461=CARTESIAN_POINT('Ctrl Pts',(7.24787638617303,2.75286253631321,0.161420634597048));
#104462=CARTESIAN_POINT('Ctrl Pts',(7.46005895192977,2.61844385838297,0.773205258737892));
#104463=CARTESIAN_POINT('Ctrl Pts',(7.46096795696486,2.61987032769149,0.764224199368948));
#104464=CARTESIAN_POINT('Ctrl Pts',(7.461876962,2.621296797,0.75524314));
#104465=CARTESIAN_POINT('Ctrl Pts',(7.480215721,2.65007516,0.574054393));
#104466=CARTESIAN_POINT('Ctrl Pts',(7.489738828,2.678571429,0.392189107));
#104467=CARTESIAN_POINT('Ctrl Pts',(7.50207612295756,2.71548867651787,0.15658051345081));
#104468=CARTESIAN_POINT('Ctrl Pts',(7.4995803569868,2.75286253631321,-0.0793376696427069));
#104469=CARTESIAN_POINT('Ctrl Pts',(7.24780059325685,2.7499999986265,0.178568399451582));
#104470=CARTESIAN_POINT('Ctrl Pts',(7.28939465910201,2.7431845125398,0.179593178039138));
#104471=CARTESIAN_POINT('Ctrl Pts',(7.33104107381993,2.73653622816585,0.180678478153405));
#104472=CARTESIAN_POINT('Ctrl Pts',(7.41432882964981,2.7235645705627,0.182956410170129));
#104473=CARTESIAN_POINT('Ctrl Pts',(7.45601972471698,2.71723347887198,0.184150402700255));
#104474=CARTESIAN_POINT('Ctrl Pts',(7.49770826955607,2.71105259871467,0.185393373255831));
#104475=CARTESIAN_POINT('',(7.32221810744534,2.62129679787114,0.861793456887462));
#104476=CARTESIAN_POINT('Ctrl Pts',(7.247684177,2.750764179,0.183232301));
#104477=CARTESIAN_POINT('Ctrl Pts',(7.25761282,2.686419405,-0.209491436));
#104478=CARTESIAN_POINT('Ctrl Pts',(7.22504759300001,2.621296797,-0.600988584999999));
#104479=CARTESIAN_POINT('Ctrl Pts',(7.487354858,2.750764179,0.435335768));
#104480=CARTESIAN_POINT('Ctrl Pts',(7.510944005,2.686419405,0.029625212));
#104481=CARTESIAN_POINT('Ctrl Pts',(7.490556008,2.621296797,-0.376258802));
#104482=CARTESIAN_POINT('',(7.35780180129346,2.62129679507543,-0.488623681551902));
#104483=CARTESIAN_POINT('Ctrl Pts',(7.22619529940868,2.61844385851179,-0.583245041761979));
#104484=CARTESIAN_POINT('Ctrl Pts',(7.22547237799634,2.61987032775589,-0.591940695809489));
#104485=CARTESIAN_POINT('Ctrl Pts',(7.22474945658406,2.621296797,-0.600636349857002));
#104486=CARTESIAN_POINT('Ctrl Pts',(7.21016484853215,2.65007516,-0.776067183529233));
#104487=CARTESIAN_POINT('Ctrl Pts',(7.18708285276207,2.678571429,-0.95058339985461));
#104488=CARTESIAN_POINT('Ctrl Pts',(7.15717985904099,2.71548867646293,-1.17667118689306));
#104489=CARTESIAN_POINT('Ctrl Pts',(7.11312572913838,2.75286253620207,-1.4004324670367));
#104490=CARTESIAN_POINT('Ctrl Pts',(7.45186319460198,2.61844385851179,-0.848564007989048));
#104491=CARTESIAN_POINT('Ctrl Pts',(7.45082028530099,2.61987032775589,-0.857530503994525));
#104492=CARTESIAN_POINT('Ctrl Pts',(7.44977737600001,2.621296797,-0.866497));
#104493=CARTESIAN_POINT('Ctrl Pts',(7.428737159,2.65007516,-1.047391946));
#104494=CARTESIAN_POINT('Ctrl Pts',(7.398941961,2.678571429,-1.227052509));
#104495=CARTESIAN_POINT('Ctrl Pts',(7.36034193449132,2.71548867646293,-1.45980485781117));
#104496=CARTESIAN_POINT('Ctrl Pts',(7.30718908296341,2.75286253620207,-1.6896708892753));
#104497=CARTESIAN_POINT('',(7.4497773762241,2.62129679728562,-0.866496991987696));
#104498=CARTESIAN_POINT('',(7.36227011168024,2.71105259872532,-1.43072666945356));
#104499=CARTESIAN_POINT('Ctrl Pts',(7.44977737688415,2.62129679564651,-0.866496991367734));
#104500=CARTESIAN_POINT('Ctrl Pts',(7.43572047689793,2.64052352569903,-0.987352312322432));
#104501=CARTESIAN_POINT('Ctrl Pts',(7.41875122985605,2.65962575012099,-1.10760559706222));
#104502=CARTESIAN_POINT('Ctrl Pts',(7.39894196064008,2.67857142921625,-1.22705251018873));
#104503=CARTESIAN_POINT('Ctrl Pts',(7.38767229163384,2.68934979373988,-1.29500691707787));
#104504=CARTESIAN_POINT('Ctrl Pts',(7.37544877285651,2.70017879536303,-1.36291157598306));
#104505=CARTESIAN_POINT('Ctrl Pts',(7.36227011098551,2.7110525996053,-1.43072667338086));
#104506=CARTESIAN_POINT('Ctrl Pts',(7.11673797052314,2.74999999867813,-1.38366931491681));
#104507=CARTESIAN_POINT('Ctrl Pts',(7.15757988738069,2.74318451260325,-1.39160998948805));
#104508=CARTESIAN_POINT('Ctrl Pts',(7.19848593954936,2.73653622822845,-1.39950281104339));
#104509=CARTESIAN_POINT('Ctrl Pts',(7.28031615690217,2.72356457142187,-1.41518254019115));
#104510=CARTESIAN_POINT('Ctrl Pts',(7.32128900927842,2.71723348055737,-1.4229787714934));
#104511=CARTESIAN_POINT('Ctrl Pts',(7.36227011198849,2.71105259872787,-1.43072666782516));
#104512=CARTESIAN_POINT('',(7.33628883611589,2.62129679787115,-0.732415245107293));
#104513=CARTESIAN_POINT('Origin',(3.75133951679985E-13,2.71213386199922,
-5.10659223240673E-14));
#104514=CARTESIAN_POINT('',(7.36365834535768,2.5308420210249,-1.42356445975565));
#104515=CARTESIAN_POINT('Origin',(-0.190177539396756,2.55357151332881,0.0330533513936276));
#104516=CARTESIAN_POINT('',(7.23454645265237,2.62129679635372,-1.97771019422671));
#104517=CARTESIAN_POINT('Origin',(-0.186944872904844,2.410791282204,0.0165779686647455));
#104518=CARTESIAN_POINT('Origin',(-0.180684632637054,2.55359539647965,0.0606642551306097));
#104519=CARTESIAN_POINT('Ctrl Pts',(7.117626877,2.750764179,-1.379089427));
#104520=CARTESIAN_POINT('Ctrl Pts',(7.042899399,2.686419405,-1.764765866));
#104521=CARTESIAN_POINT('Ctrl Pts',(6.926935215,2.621296797,-2.140109468));
#104522=CARTESIAN_POINT('Ctrl Pts',(7.405888984,2.750764179,-1.18440211));
#104523=CARTESIAN_POINT('Ctrl Pts',(7.341710853,2.686419405,-1.585698348));
#104524=CARTESIAN_POINT('Ctrl Pts',(7.234546451,2.621296797,-1.977710203));
#104525=CARTESIAN_POINT('',(7.0807408363434,2.62129679507543,-2.05890982400181));
#104526=CARTESIAN_POINT('Ctrl Pts',(6.9318704271471,2.61844385782496,-2.12302747772819));
#104527=CARTESIAN_POINT('Ctrl Pts',(6.92929509802686,2.61987032741248,-2.13136442748401));
#104528=CARTESIAN_POINT('Ctrl Pts',(6.92671976890657,2.621296797,-2.13970137723984));
#104529=CARTESIAN_POINT('Ctrl Pts',(6.87476369713584,2.65007516,-2.3078954757923));
#104530=CARTESIAN_POINT('Ctrl Pts',(6.81470551759715,2.678571429,-2.47336965345944));
#104531=CARTESIAN_POINT('Ctrl Pts',(6.7368994466319,2.71548867677546,-2.68774337481691));
#104532=CARTESIAN_POINT('Ctrl Pts',(6.64577321665464,2.75286253683425,-2.89680290696358));
#104533=CARTESIAN_POINT('Ctrl Pts',(7.09522659686887,2.61844385782496,-2.43065536060913));
#104534=CARTESIAN_POINT('Ctrl Pts',(7.09228053793441,2.61987032741248,-2.43918803230456));
#104535=CARTESIAN_POINT('Ctrl Pts',(7.089334479,2.621296797,-2.447720704));
#104536=CARTESIAN_POINT('Ctrl Pts',(7.029899105,2.65007516,-2.619863402));
#104537=CARTESIAN_POINT('Ctrl Pts',(6.962178791,2.678571429,-2.788918514));
#104538=CARTESIAN_POINT('Ctrl Pts',(6.87444633631865,2.71548867677546,-3.00793137901318));
#104539=CARTESIAN_POINT('Ctrl Pts',(6.77312176552132,2.75286253683425,-3.2209969797396));
#104540=CARTESIAN_POINT('',(7.08933448094888,2.62129679728562,-2.4477206962377));
#104541=CARTESIAN_POINT('',(6.88258038540553,2.71105259873557,-2.97994752197314));
#104542=CARTESIAN_POINT('Ctrl Pts',(7.08933448171907,2.62129679564653,-2.44772069575958));
#104543=CARTESIAN_POINT('Ctrl Pts',(7.04962590309123,2.64052352569907,-2.56272866850804));
#104544=CARTESIAN_POINT('Ctrl Pts',(7.00720248596634,2.65962575012069,-2.67652261175817));
#104545=CARTESIAN_POINT('Ctrl Pts',(6.9621787906131,2.67857142916281,-2.78891851496585));
#104546=CARTESIAN_POINT('Ctrl Pts',(6.93656441164756,2.68934979365771,-2.85286153970963));
#104547=CARTESIAN_POINT('Ctrl Pts',(6.910029177234,2.70017879535824,-2.91655093023377));
#104548=CARTESIAN_POINT('Ctrl Pts',(6.88258038384324,2.71105259958446,-2.97994752537253));
#104549=CARTESIAN_POINT('Ctrl Pts',(6.65290458943671,2.74999999865438,-2.88120818907132));
#104550=CARTESIAN_POINT('Ctrl Pts',(6.69108463438367,2.74318451262851,-2.89774302008144));
#104551=CARTESIAN_POINT('Ctrl Pts',(6.72933760273026,2.73653622821457,-2.91424490416687));
#104552=CARTESIAN_POINT('Ctrl Pts',(6.80588401007471,2.72356456917387,-2.94714913373006));
#104553=CARTESIAN_POINT('Ctrl Pts',(6.84422299606672,2.71723347594592,-2.96357105219085));
#104554=CARTESIAN_POINT('Ctrl Pts',(6.8825803860209,2.71105259873809,-2.97994752053274));
#104555=CARTESIAN_POINT('',(7.00732285234163,2.62129679787115,-2.29237702474075));
#104556=CARTESIAN_POINT('Origin',(5.00901403688303E-13,2.71213386200067,
-1.29453739394769E-13));
#104557=CARTESIAN_POINT('',(6.88547582676816,2.53084202099543,-2.97325118946033));
#104558=CARTESIAN_POINT('Origin',(-0.178625804802862,2.55357152389825,0.0731631300769686));
#104559=CARTESIAN_POINT('',(6.64025754551519,2.62129679635372,-3.48668606478277));
#104560=CARTESIAN_POINT('Origin',(-0.179010305405579,2.41079133936449,0.0563779573340922));
#104561=CARTESIAN_POINT('Origin',(-0.163419285777804,2.55359539665695,0.0980878048727796));
#104562=CARTESIAN_POINT('Ctrl Pts',(6.654757254,2.750764179,-2.876926465));
#104563=CARTESIAN_POINT('Ctrl Pts',(6.49886783,2.686419405,-3.237521805));
#104564=CARTESIAN_POINT('Ctrl Pts',(6.304927044,2.621296797,-3.57916121));
#104565=CARTESIAN_POINT('Ctrl Pts',(6.978131972,2.750764179,-2.748758662));
#104566=CARTESIAN_POINT('Ctrl Pts',(6.829187461,2.686419405,-3.126876416));
#104567=CARTESIAN_POINT('Ctrl Pts',(6.640257542,2.621296797,-3.486686073));
#104568=CARTESIAN_POINT('',(6.472592298737,2.62129679507543,-3.53292363098937));
#104569=CARTESIAN_POINT('Ctrl Pts',(6.31341899261438,2.61844385915646,-3.56353951913638));
#104570=CARTESIAN_POINT('Ctrl Pts',(6.30911167752144,2.61987032807824,-3.57112793249725));
#104571=CARTESIAN_POINT('Ctrl Pts',(6.3048043624285,2.621296797,-3.57871634585811));
#104572=CARTESIAN_POINT('Ctrl Pts',(6.21790623558622,2.65007516,-3.73180914091384));
#104573=CARTESIAN_POINT('Ctrl Pts',(6.12368012659908,2.678571429,-3.88050389076422));
#104574=CARTESIAN_POINT('Ctrl Pts',(6.00160910777752,2.71548867610496,-4.07313966510681));
#104575=CARTESIAN_POINT('Ctrl Pts',(5.86767174108176,2.75286253547799,-4.25772205181901));
#104576=CARTESIAN_POINT('Ctrl Pts',(6.40682508435585,2.61844385915646,-3.89909198129979));
#104577=CARTESIAN_POINT('Ctrl Pts',(6.40211363267789,2.61987032807824,-3.90679184464988));
#104578=CARTESIAN_POINT('Ctrl Pts',(6.397402181,2.621296797,-3.914491708));
#104579=CARTESIAN_POINT('Ctrl Pts',(6.302350782,2.65007516,-4.069832956));
#104580=CARTESIAN_POINT('Ctrl Pts',(6.199871879,2.678571429,-4.220377789));
#104581=CARTESIAN_POINT('Ctrl Pts',(6.06710927111963,2.71548867610496,-4.41541036735175));
#104582=CARTESIAN_POINT('Ctrl Pts',(5.92235080998031,2.75286253547799,-4.60171282101012));
#104583=CARTESIAN_POINT('',(6.39740218457622,2.62129679728566,-3.91449170085054));
#104584=CARTESIAN_POINT('',(6.08106885043357,2.71105259869766,-4.3898293404743));
#104585=CARTESIAN_POINT('Ctrl Pts',(6.39740218542778,2.62129679564633,-3.91449170053633));
#104586=CARTESIAN_POINT('Ctrl Pts',(6.33389865714133,2.64052352569892,-4.01827467958564));
#104587=CARTESIAN_POINT('Ctrl Pts',(6.26800474188442,2.65962575012044,-4.1202884031626));
#104588=CARTESIAN_POINT('Ctrl Pts',(6.1998718785814,2.6785714291164,-4.22037778961493));
#104589=CARTESIAN_POINT('Ctrl Pts',(6.16111048962537,2.68934979357377,-4.27731952756113));
#104590=CARTESIAN_POINT('Ctrl Pts',(6.12150429781491,2.70017879533987,-4.33381560487414));
#104591=CARTESIAN_POINT('Ctrl Pts',(6.08106884815002,2.7110525995626,-4.38982934357438));
#104592=CARTESIAN_POINT('Ctrl Pts',(5.87798878527351,2.7499999985941,-4.24402497176462));
#104593=CARTESIAN_POINT('Ctrl Pts',(5.91172170248899,2.7431845125011,-4.26838080871113));
#104594=CARTESIAN_POINT('Ctrl Pts',(5.94553291982931,2.73653622819684,-4.29272014485459));
#104595=CARTESIAN_POINT('Ctrl Pts',(6.0132162752591,2.72356456965486,-4.34131030473907));
#104596=CARTESIAN_POINT('Ctrl Pts',(6.04712868651706,2.71723347701746,-4.36559003416882));
#104597=CARTESIAN_POINT('Ctrl Pts',(6.08106885136474,2.71105259870017,-4.3898293391711));
#104598=CARTESIAN_POINT('',(6.35070223953008,2.62129679787127,-3.74514980190602));
#104599=CARTESIAN_POINT('Origin',(-4.18935719448399E-13,2.71213386200033,
3.29163779566599E-13));
#104600=CARTESIAN_POINT('',(6.0853361110207,2.53084202103016,-4.38391199843598));
#104601=CARTESIAN_POINT('Origin',(-0.158721868614637,2.55357153612414,0.10985197956607));
#104602=CARTESIAN_POINT('',(5.7354775761899,2.62129679635372,-4.83262836973105));
#104603=CARTESIAN_POINT('Origin',(-0.162705727064962,2.41079129892709,0.0935419213495575));
#104604=CARTESIAN_POINT('Origin',(-0.138512605094451,2.55359539186379,0.130924849469142));
#104605=CARTESIAN_POINT('Ctrl Pts',(5.880718579,2.750764179,-4.24024162));
#104606=CARTESIAN_POINT('Ctrl Pts',(5.650956424,2.686419405,-4.558894822));
#104607=CARTESIAN_POINT('Ctrl Pts',(5.388107493,2.621296797,-4.850855352));
#104608=CARTESIAN_POINT('Ctrl Pts',(6.224085265,2.750764179,-4.184586314));
#104609=CARTESIAN_POINT('Ctrl Pts',(5.997338854,2.686419405,-4.521845218));
#104610=CARTESIAN_POINT('Ctrl Pts',(5.735477571,2.621296797,-4.832628377));
#104611=CARTESIAN_POINT('',(5.56179253986235,2.62129679507543,-4.84174185546838));
#104612=CARTESIAN_POINT('Ctrl Pts',(5.39975910663828,2.61844385907082,-4.83742440510579));
#104613=CARTESIAN_POINT('Ctrl Pts',(5.39392120946597,2.61987032803543,-4.84390946034449));
#104614=CARTESIAN_POINT('Ctrl Pts',(5.38808331229366,2.621296797,-4.85039451558319));
#104615=CARTESIAN_POINT('Ctrl Pts',(5.27030639029006,2.65007516,-4.98122755742915));
#104616=CARTESIAN_POINT('Ctrl Pts',(5.14631825859592,2.678571429,-5.10619007807575));
#104617=CARTESIAN_POINT('Ctrl Pts',(4.98569019364608,2.71548867628975,-5.26808047573109));
#104618=CARTESIAN_POINT('Ctrl Pts',(4.81520445166271,2.75286253585177,-5.41955485476044));
#104619=CARTESIAN_POINT('Ctrl Pts',(5.41884755555708,2.61844385907083,-5.18521138563031));
#104620=CARTESIAN_POINT('Ctrl Pts',(5.41259101177851,2.61987032803543,-5.19171840781515));
#104621=CARTESIAN_POINT('Ctrl Pts',(5.406334468,2.621296797,-5.19822543));
#104622=CARTESIAN_POINT('Ctrl Pts',(5.280111541,2.65007516,-5.329501645));
#104623=CARTESIAN_POINT('Ctrl Pts',(5.147665849,2.678571429,-5.454496888));
#104624=CARTESIAN_POINT('Ctrl Pts',(4.97608091710626,2.71548867628975,-5.6164296779869));
#104625=CARTESIAN_POINT('Ctrl Pts',(4.79465730568439,2.75286253585177,-5.76725769523455));
#104626=CARTESIAN_POINT('',(5.40633447302854,2.62129679728566,-5.19822542376748));
#104627=CARTESIAN_POINT('',(4.99521329427887,2.71105259871137,-5.59444761728836));
#104628=CARTESIAN_POINT('Ctrl Pts',(5.40633447392874,2.62129679564632,-5.19822542366268));
#104629=CARTESIAN_POINT('Ctrl Pts',(5.32200534986941,2.64052352569893,-5.28593063299743));
#104630=CARTESIAN_POINT('Ctrl Pts',(5.23572206260184,2.65962575012048,-5.37139408829185));
#104631=CARTESIAN_POINT('Ctrl Pts',(5.14766584842139,2.67857142912449,-5.45449688854606));
#104632=CARTESIAN_POINT('Ctrl Pts',(5.09756988870475,2.68934979359114,-5.50177480760766));
#104633=CARTESIAN_POINT('Ctrl Pts',(5.04674468096891,2.70017879535905,-5.54843587768945));
#104634=CARTESIAN_POINT('Ctrl Pts',(4.99521329131249,2.71105259960729,-5.59444762016897));
#104635=CARTESIAN_POINT('Ctrl Pts',(4.82822475769958,2.7499999986702,-5.40839586282795));
#104636=CARTESIAN_POINT('Ctrl Pts',(4.85593323273153,2.74318451255374,-5.43943385389486));
#104637=CARTESIAN_POINT('Ctrl Pts',(4.88372172491011,2.73653622818544,-5.47047256236182));
#104638=CARTESIAN_POINT('Ctrl Pts',(4.9393774763658,2.72356451292338,-5.53247690297572));
#104639=CARTESIAN_POINT('Ctrl Pts',(4.96727788841002,2.71723336162852,-5.56347945870885));
#104640=CARTESIAN_POINT('Ctrl Pts',(4.99521329555192,2.71105259871396,-5.5944476161405));
#104641=CARTESIAN_POINT('',(5.39712984926632,2.62129679787127,-5.02280353669731));
#104642=CARTESIAN_POINT('Origin',(1.99493199737333E-14,2.71213386199978,
1.91253263226443E-13));
#104643=CARTESIAN_POINT('',(5.0006528418571,2.53084202098007,-5.58958595540413));
#104644=CARTESIAN_POINT('Origin',(-0.131396091024157,2.55357151509916,0.141404195937408));
#104645=CARTESIAN_POINT('',(4.56251304987736,2.62129679634652,-5.95260234279302));
#104646=CARTESIAN_POINT('Origin',(-0.138792725172361,2.4107913116991,0.126331557680013));
#104647=CARTESIAN_POINT('Origin',(-0.107129219609613,2.55359538161478,0.157639934758409));
#104648=CARTESIAN_POINT('Ctrl Pts',(4.83170403900001,2.750764179,-5.405287789));
#104649=CARTESIAN_POINT('Ctrl Pts',(4.538812577,2.686419405,-5.667098985));
#104650=CARTESIAN_POINT('Ctrl Pts',(4.219346023,2.621296797,-5.895728889));
#104651=CARTESIAN_POINT('Ctrl Pts',(5.179007248,2.750764179,-5.42474736));
#104652=CARTESIAN_POINT('Ctrl Pts',(4.88506134700001,2.686419405,-5.705377563));
#104653=CARTESIAN_POINT('Ctrl Pts',(4.562513043,2.621296797,-5.952602349));
#104654=CARTESIAN_POINT('',(4.39092954262006,2.62129679507543,-5.92416561186972));
#104655=CARTESIAN_POINT('Ctrl Pts',(4.23361250166653,2.61844385572301,-5.88511669028191));
#104656=CARTESIAN_POINT('Ctrl Pts',(4.22651698779161,2.61987032636152,-5.8901951591589));
#104657=CARTESIAN_POINT('Ctrl Pts',(4.21942147391668,2.621296797,-5.89527362803587));
#104658=CARTESIAN_POINT('Ctrl Pts',(4.0762728745308,2.65007516,-5.99772930912924));
#104659=CARTESIAN_POINT('Ctrl Pts',(3.92832026919488,2.678571429,-6.09311649260205));
#104660=CARTESIAN_POINT('Ctrl Pts',(3.73664594067155,2.71548867784011,-6.21669170275015));
#104661=CARTESIAN_POINT('Ctrl Pts',(3.53758353723714,2.75286253898775,-6.32797530411712));
#104662=CARTESIAN_POINT('Ctrl Pts',(4.17749075401,2.61844385572301,-6.22887605792468));
#104663=CARTESIAN_POINT('Ctrl Pts',(4.16998165850501,2.61987032636152,-6.23388598346234));
#104664=CARTESIAN_POINT('Ctrl Pts',(4.162472563,2.621296797,-6.238895909));
#104665=CARTESIAN_POINT('Ctrl Pts',(4.010980152,2.65007516,-6.339968761));
#104666=CARTESIAN_POINT('Ctrl Pts',(3.854760685,2.678571429,-6.433569776));
#104667=CARTESIAN_POINT('Ctrl Pts',(3.65237654195466,2.71548867784011,-6.55483098381374));
#104668=CARTESIAN_POINT('Ctrl Pts',(3.44277094001505,2.75286253898775,-6.6631320152788));
#104669=CARTESIAN_POINT('',(4.16247256710208,2.6212967972753,-6.23889590617043));
#104670=CARTESIAN_POINT('',(3.67578711654018,2.71105259872685,-6.53747574191002));
#104671=CARTESIAN_POINT('Ctrl Pts',(4.16247257015249,2.62129679564632,-6.2388959040854));
#104672=CARTESIAN_POINT('Ctrl Pts',(4.06126098658328,2.64052352569889,-6.30642234553461));
#104673=CARTESIAN_POINT('Ctrl Pts',(3.95862283821071,2.65962575012066,-6.37133935655009));
#104674=CARTESIAN_POINT('Ctrl Pts',(3.85476068413728,2.67857142915737,-6.43356977651691));
#104675=CARTESIAN_POINT('Ctrl Pts',(3.79567258495783,2.68934979364761,-6.46897321358428));
#104676=CARTESIAN_POINT('Ctrl Pts',(3.73600489189462,2.70017879536733,-6.5036174562153));
#104677=CARTESIAN_POINT('Ctrl Pts',(3.67578711304722,2.71105259961759,-6.5374757440446));
#104678=CARTESIAN_POINT('Ctrl Pts',(3.55269830572751,2.74999999880152,-6.31987617340038));
#104679=CARTESIAN_POINT('Ctrl Pts',(3.57308672129151,2.7431845127979,-6.35614501628686));
#104680=CARTESIAN_POINT('Ctrl Pts',(3.59355312983288,2.73653622825198,-6.3924317625532));
#104681=CARTESIAN_POINT('Ctrl Pts',(3.63457839142501,2.72356457278339,-6.46495048348133));
#104682=CARTESIAN_POINT('Ctrl Pts',(3.65516165798572,2.71723348319677,-6.50122560227696));
#104683=CARTESIAN_POINT('Ctrl Pts',(3.67578711801596,2.71105259872974,-6.5374757410682));
#104684=CARTESIAN_POINT('',(4.1911936646973,2.62129679787127,-6.06559656086156));
#104685=CARTESIAN_POINT('Origin',(-1.70002900645727E-13,2.71213386200011,
3.17454396103756E-13));
#104686=CARTESIAN_POINT('',(3.6821446043708,2.53084202104383,-6.53389708421412));
#104687=CARTESIAN_POINT('Origin',(-0.0979263329305657,2.55357153666071,
0.166344406806528));
#104688=CARTESIAN_POINT('',(3.17621048374422,2.62129679635372,-6.79423924757478));
#104689=CARTESIAN_POINT('Origin',(-0.108390380534508,2.41079129001318,0.153214497356897));
#104690=CARTESIAN_POINT('Origin',(-0.0707368488802823,2.55359538285412,
0.176984352893484));
#104691=CARTESIAN_POINT('Ctrl Pts',(3.556764388,2.750764179,-6.317588708));
#104692=CARTESIAN_POINT('Ctrl Pts',(3.214438897,2.686419405,-6.510315898));
#104693=CARTESIAN_POINT('Ctrl Pts',(2.853292624,2.621296797,-6.664924696));
#104694=CARTESIAN_POINT('Ctrl Pts',(3.891764609,2.750764179,-6.41125325));
#104695=CARTESIAN_POINT('Ctrl Pts',(3.544363801,2.686419405,-6.622132794));
#104696=CARTESIAN_POINT('Ctrl Pts',(3.176210476,2.621296797,-6.794239252));
#104697=CARTESIAN_POINT('',(3.01475156092796,2.62129679507543,-6.72958196910444));
#104698=CARTESIAN_POINT('Ctrl Pts',(2.86950685216909,2.61844385876436,-6.65762748361419));
#104699=CARTESIAN_POINT('Ctrl Pts',(2.86148551526963,2.6198703278822,-6.66106189130307));
#104700=CARTESIAN_POINT('Ctrl Pts',(2.85346417837015,2.621296797,-6.664496298992));
#104701=CARTESIAN_POINT('Ctrl Pts',(2.69163736967406,2.65007516,-6.73378390566189));
#104702=CARTESIAN_POINT('Ctrl Pts',(2.5266383885379,2.678571429,-6.79513555330274));
#104703=CARTESIAN_POINT('Ctrl Pts',(2.31288029197869,2.7154886763067,-6.87461732503512));
#104704=CARTESIAN_POINT('Ctrl Pts',(2.09454918097776,2.75286253588607,-6.94050664340249));
#104705=CARTESIAN_POINT('Ctrl Pts',(2.74079909590421,2.61844385876436,-6.98128543055836));
#104706=CARTESIAN_POINT('Ctrl Pts',(2.73238858195209,2.6198703278822,-6.98456398977921));
#104707=CARTESIAN_POINT('Ctrl Pts',(2.723978068,2.621296797,-6.987842549));
#104708=CARTESIAN_POINT('Ctrl Pts',(2.55429979,2.65007516,-7.053985984));
#104709=CARTESIAN_POINT('Ctrl Pts',(2.381611195,2.678571429,-7.111816091));
#104710=CARTESIAN_POINT('Ctrl Pts',(2.15789111477469,2.7154886763067,-7.18673566706576));
#104711=CARTESIAN_POINT('Ctrl Pts',(1.92990446456554,2.75286253588607,-7.24744567082467));
#104712=CARTESIAN_POINT('',(2.72397807518795,2.62129679728566,-6.98784254543705));
#104713=CARTESIAN_POINT('',(2.18448521775642,2.71105259874109,-7.17481876632998));
#104714=CARTESIAN_POINT('Ctrl Pts',(2.72397807604177,2.62129679564632,-6.98784254573787));
#104715=CARTESIAN_POINT('Ctrl Pts',(2.61061657427771,2.6405235256989,-7.03203275809993));
#104716=CARTESIAN_POINT('Ctrl Pts',(2.4964228100649,2.65962575012042,-7.07336787742856));
#104717=CARTESIAN_POINT('Ctrl Pts',(2.38161119431193,2.67857142911354,-7.11181609123042));
#104718=CARTESIAN_POINT('Ctrl Pts',(2.31629384972667,2.6893497935814,-7.13368962068548));
#104719=CARTESIAN_POINT('Ctrl Pts',(2.2505736657156,2.70017879535968,-7.15469710993931));
#104720=CARTESIAN_POINT('Ctrl Pts',(2.18448521418065,2.71105259958509,-7.17481876732073));
#104721=CARTESIAN_POINT('Ctrl Pts',(2.11105163103631,2.74999999854399,-6.93584610049946));
#104722=CARTESIAN_POINT('Ctrl Pts',(2.123166647636,2.74318451250202,-6.97564990496104));
#104723=CARTESIAN_POINT('Ctrl Pts',(2.13535398462692,2.73653622814086,-7.01548795905045));
#104724=CARTESIAN_POINT('Ctrl Pts',(2.15983072381233,2.72356456894578,-7.09513047405887));
#104725=CARTESIAN_POINT('Ctrl Pts',(2.17213469463377,2.71723347557679,-7.13498232014607));
#104726=CARTESIAN_POINT('Ctrl Pts',(2.18448521924304,2.71105259874358,-7.17481876586947));
#104727=CARTESIAN_POINT('',(2.78928192372766,2.62129679787127,-6.82476903121289));
#104728=CARTESIAN_POINT('Origin',(-4.74988971765899E-13,2.71213386200044,
1.59984872571961E-12));
#104729=CARTESIAN_POINT('',(2.19146337730603,2.53084202100558,-7.17269044818231));
#104730=CARTESIAN_POINT('Origin',(-0.0598777747865242,2.55357151181406,
0.183506744246429));
#104731=CARTESIAN_POINT('',(1.64139184552713,2.62129679635372,-7.31818507535165));
#104732=CARTESIAN_POINT('Origin',(-0.0729196359695544,2.41079129102837,
0.172932995350268));
#104733=CARTESIAN_POINT('Origin',(-0.0310366278976987,2.5535954019215,0.188052770169909));
#104734=CARTESIAN_POINT('Ctrl Pts',(2.115514388,2.750764179,-6.934486201));
#104735=CARTESIAN_POINT('Ctrl Pts',(1.739761628,2.686419405,-7.049117675));
#104736=CARTESIAN_POINT('Ctrl Pts',(1.353822432,2.621296797,-7.12247603199999));
#104737=CARTESIAN_POINT('Ctrl Pts',(2.422547381,2.750764179,-7.097976063));
#104738=CARTESIAN_POINT('Ctrl Pts',(2.037935743,2.686419405,-7.229244456));
#104739=CARTESIAN_POINT('Ctrl Pts',(1.641391837,2.621296797,-7.318185078));
#104740=CARTESIAN_POINT('',(1.49760714622486,2.62129679507543,-7.22033055256809));
#104741=CARTESIAN_POINT('Ctrl Pts',(1.37122627115081,2.61844385784376,-7.11883500295392));
#104742=CARTESIAN_POINT('Ctrl Pts',(1.36265416973951,2.61987032742189,-7.12046476629346));
#104743=CARTESIAN_POINT('Ctrl Pts',(1.35408206832823,2.621296797,-7.12209452963294));
#104744=CARTESIAN_POINT('Ctrl Pts',(1.1811438929391,2.65007516,-7.15497425010359));
#104745=CARTESIAN_POINT('Ctrl Pts',(1.00681370664644,2.678571429,-7.17942162675545));
#104746=CARTESIAN_POINT('Ctrl Pts',(0.780966920247157,2.71548867679214,
-7.21109348723412));
#104747=CARTESIAN_POINT('Ctrl Pts',(0.553576011372223,2.75286253686799,
-7.2285076148007));
#104748=CARTESIAN_POINT('Ctrl Pts',(1.1759507389645,2.61844385784376,-7.40725764432955));
#104749=CARTESIAN_POINT('Ctrl Pts',(1.16703206198225,2.61987032742189,-7.40865154116478));
#104750=CARTESIAN_POINT('Ctrl Pts',(1.158113385,2.621296797,-7.410045438));
#104751=CARTESIAN_POINT('Ctrl Pts',(0.978183208000001,2.65007516,-7.438166661));
#104752=CARTESIAN_POINT('Ctrl Pts',(0.797100213,2.678571429,-7.45752179));
#104753=CARTESIAN_POINT('Ctrl Pts',(0.562505086185012,2.71548867679214,
-7.48259658469367));
#104754=CARTESIAN_POINT('Ctrl Pts',(0.326797777798836,2.75286253686799,
-7.49287683126911));
#104755=CARTESIAN_POINT('',(1.15811338992526,2.6212967972753,-7.41004543713347));
#104756=CARTESIAN_POINT('',(0.591039218777014,2.71105259868594,-7.47667523986537));
#104757=CARTESIAN_POINT('Ctrl Pts',(1.15811339355499,2.62129679564632,-7.4100454365429));
#104758=CARTESIAN_POINT('Ctrl Pts',(1.03790263162981,2.64052352569889,-7.42883313360447));
#104759=CARTESIAN_POINT('Ctrl Pts',(0.917492825588274,2.65962575012064,
-7.44465357703255));
#104760=CARTESIAN_POINT('Ctrl Pts',(0.797100212035308,2.67857142915303,
-7.45752179009368));
#104761=CARTESIAN_POINT('Ctrl Pts',(0.728607788260009,2.68934979362689,
-7.46484263040351));
#104762=CARTESIAN_POINT('Ctrl Pts',(0.65990811678701,2.70017879532997,-7.47123107939918));
#104763=CARTESIAN_POINT('Ctrl Pts',(0.591039214965599,2.71105259954616,
-7.47667524011723));
#104764=CARTESIAN_POINT('Ctrl Pts',(0.570694527564471,2.74999999866232,
-7.22750357125241));
#104765=CARTESIAN_POINT('Ctrl Pts',(0.573969660404782,2.74318451258878,
-7.26898115529249));
#104766=CARTESIAN_POINT('Ctrl Pts',(0.577308060245781,2.73653622816014,
-7.31050773529034));
#104767=CARTESIAN_POINT('Ctrl Pts',(0.584091760165737,2.72356456942296,
-7.39355002482758));
#104768=CARTESIAN_POINT('Ctrl Pts',(0.587541101836548,2.71723347653185,
-7.43511514350048));
#104769=CARTESIAN_POINT('Ctrl Pts',(0.591039220362404,2.71105259868844,
-7.4766752397323));
#104770=CARTESIAN_POINT('',(1.25694645900164,2.62129679787127,-7.26482288705877));
#104771=CARTESIAN_POINT('Origin',(2.18398975120049E-13,2.71213386199911,
-2.48499137933678E-12));
#104772=CARTESIAN_POINT('',(0.598311757139466,2.53084202105362,-7.47609677821526));
#104773=CARTESIAN_POINT('Origin',(-0.0190293522278347,2.55357152284122,
0.192088535853675));
#104774=CARTESIAN_POINT('',(0.0298235498648649,2.62129679635372,-7.49994070321252));
#104775=CARTESIAN_POINT('Origin',(-0.0340393366185852,2.41079133825631,
0.184565482644015));
#104776=CARTESIAN_POINT('Origin',(0.0101147754415452,2.55359537888983,0.190328199564994));
#104777=CARTESIAN_POINT('Ctrl Pts',(0.575345286,2.750764179,-7.227134827));
#104778=CARTESIAN_POINT('Ctrl Pts',(0.183735038,2.686419405,-7.25831054400001));
#104779=CARTESIAN_POINT('Ctrl Pts',(-0.208950992,2.621296797,-7.246988304));
#104780=CARTESIAN_POINT('Ctrl Pts',(0.840054531,2.750764179,-7.452805404));
#104781=CARTESIAN_POINT('Ctrl Pts',(0.436216075,2.686419405,-7.498324682));
#104782=CARTESIAN_POINT('Ctrl Pts',(0.029823541,2.621296797,-7.499940704));
#104783=CARTESIAN_POINT('',(-0.089563713526468,2.62129679507543,-7.37346450414545));
#104784=CARTESIAN_POINT('Ctrl Pts',(-0.191171332133358,2.61844385795941,
-7.24717371104007));
#104785=CARTESIAN_POINT('Ctrl Pts',(-0.199893373131833,2.61987032747972,
-7.24692262307867));
#104786=CARTESIAN_POINT('Ctrl Pts',(-0.208615414130308,2.621296797,-7.24667153511732));
#104787=CARTESIAN_POINT('Ctrl Pts',(-0.384578558372457,2.65007516,-7.24160595159503));
#104788=CARTESIAN_POINT('Ctrl Pts',(-0.560088466166838,2.678571429,-7.22800592478954));
#104789=CARTESIAN_POINT('Ctrl Pts',(-0.787463593391741,2.71548867672983,
-7.2103869318697));
#104790=CARTESIAN_POINT('Ctrl Pts',(-1.01328175149655,2.75286253674194,
-7.17851160256953));
#104791=CARTESIAN_POINT('Ctrl Pts',(-0.443883772970446,2.61844385795941,
-7.48687472409367));
#104792=CARTESIAN_POINT('Ctrl Pts',(-0.452893582485223,2.61987032747972,
-7.48631878054684));
#104793=CARTESIAN_POINT('Ctrl Pts',(-0.461903392,2.621296797,-7.485762837));
#104794=CARTESIAN_POINT('Ctrl Pts',(-0.643672133,2.65007516,-7.474546933));
#104795=CARTESIAN_POINT('Ctrl Pts',(-0.824682289,2.678571429,-7.454522059));
#104796=CARTESIAN_POINT('Ctrl Pts',(-1.05918305066926,2.71548867672983,
-7.42857960078149));
#104797=CARTESIAN_POINT('Ctrl Pts',(-1.29158960267233,2.75286253674194,
-7.38794939696055));
#104798=CARTESIAN_POINT('',(-0.461903384016568,2.62129679728565,-7.48576283681868));
#104799=CARTESIAN_POINT('',(-1.03004311690273,2.71105259869645,-7.42893068869823));
#104800=CARTESIAN_POINT('Ctrl Pts',(-0.461903383331764,2.62129679564632,
-7.48576283741603));
#104801=CARTESIAN_POINT('Ctrl Pts',(-0.58334248386094,2.64052352569891,
-7.47826952876861));
#104802=CARTESIAN_POINT('Ctrl Pts',(-0.704338103259426,2.65962575012065,
-7.46783555041797));
#104803=CARTESIAN_POINT('Ctrl Pts',(-0.824682289784371,2.67857142915571,
-7.45452205871534));
#104804=CARTESIAN_POINT('Ctrl Pts',(-0.893147162736126,2.68934979363534,
-7.44694789511135));
#104805=CARTESIAN_POINT('Ctrl Pts',(-0.96161400199659,2.70017879534504,
-7.43841858722724));
#104806=CARTESIAN_POINT('Ctrl Pts',(-1.03004312088585,2.7110525995794,-7.42893068822571));
#104807=CARTESIAN_POINT('Ctrl Pts',(-0.996347617439242,2.74999999863268,
-7.18121100780128));
#104808=CARTESIAN_POINT('Ctrl Pts',(-1.00206550981139,2.74318451257133,
-7.22242292571251));
#104809=CARTESIAN_POINT('Ctrl Pts',(-1.00773214704197,2.7365362281456,-7.2636962946843));
#104810=CARTESIAN_POINT('Ctrl Pts',(-1.0189586819062,2.72356457151075,-7.34625538337394));
#104811=CARTESIAN_POINT('Ctrl Pts',(-1.02452525378015,2.71723348077225,
-7.38759022418198));
#104812=CARTESIAN_POINT('Ctrl Pts',(-1.03004311525274,2.711052598699,-7.42893068891884));
#104813=CARTESIAN_POINT('',(-0.334162424660559,2.62129679787127,-7.36518169807725));
#104814=CARTESIAN_POINT('Origin',(-1.67834496300756E-13,2.71213386199978,
-1.13537651502682E-12));
#104815=CARTESIAN_POINT('',(-1.02281625401732,2.53084202103967,-7.42992913193524));
#104816=CARTESIAN_POINT('Origin',(0.0227088632592475,2.55357152724356,0.191688081250765));
#104817=CARTESIAN_POINT('',(-1.58313926314193,2.62129679635372,-7.33100743818864));
#104818=CARTESIAN_POINT('Origin',(0.00643263499767649,2.41079132162034,
0.187568015178931));
#104819=CARTESIAN_POINT('Origin',(0.0507931682393102,2.55359540981668,0.18370366215818));
#104820=CARTESIAN_POINT('Ctrl Pts',(-0.991726322,2.750764179,-7.18185066));
#104821=CARTESIAN_POINT('Ctrl Pts',(-1.380882798,2.686419405,-7.128112879));
#104822=CARTESIAN_POINT('Ctrl Pts',(-1.7619541,2.621296797,-7.032639458));
#104823=CARTESIAN_POINT('Ctrl Pts',(-0.781718335,2.750764179,-7.45914984700001));
#104824=CARTESIAN_POINT('Ctrl Pts',(-1.185900572,2.686419405,-7.41679158));
#104825=CARTESIAN_POINT('Ctrl Pts',(-1.583139272,2.621296797,-7.33100743700001));
#104826=CARTESIAN_POINT('',(-1.67254667433767,2.62129679507543,-7.181823450216));
#104827=CARTESIAN_POINT('Ctrl Pts',(-1.74462997673912,2.61844385812637,
-7.0366426313749));
#104828=CARTESIAN_POINT('Ctrl Pts',(-1.75309412426899,2.6198703275632,-7.03452243284389));
#104829=CARTESIAN_POINT('Ctrl Pts',(-1.76155827179887,2.621296797,-7.03240223431287));
#104830=CARTESIAN_POINT('Ctrl Pts',(-1.93231854455011,2.65007516,-6.98962820678504));
#104831=CARTESIAN_POINT('Ctrl Pts',(-2.10080152458572,2.678571429,-6.93861669850337));
#104832=CARTESIAN_POINT('Ctrl Pts',(-2.31907318411729,2.71548867663121,
-6.87253069719649));
#104833=CARTESIAN_POINT('Ctrl Pts',(-2.53275958572269,2.75286253654245,
-6.79285636614659));
#104834=CARTESIAN_POINT('Ctrl Pts',(-2.042962772427,2.61844385812637,-7.21641386396929));
#104835=CARTESIAN_POINT('Ctrl Pts',(-2.0516424257135,2.6198703275632,-7.21393407548468));
#104836=CARTESIAN_POINT('Ctrl Pts',(-2.060322079,2.621296797,-7.211454287));
#104837=CARTESIAN_POINT('Ctrl Pts',(-2.235430081,2.65007516,-7.161425698));
#104838=CARTESIAN_POINT('Ctrl Pts',(-2.407903564,2.678571429,-7.102957161));
#104839=CARTESIAN_POINT('Ctrl Pts',(-2.631344966097,2.71548867663121,-7.02721049162782));
#104840=CARTESIAN_POINT('Ctrl Pts',(-2.84958368863575,2.75286253654245,
-6.93756966110655));
#104841=CARTESIAN_POINT('',(-2.06032207113013,2.62129679728566,-7.21145428851868));
#104842=CARTESIAN_POINT('',(-2.60296178177509,2.71105259870812,-7.03381759525322));
#104843=CARTESIAN_POINT('Ctrl Pts',(-2.06032207062386,2.62129679564632,
-7.21145428926972));
#104844=CARTESIAN_POINT('Ctrl Pts',(-2.17731115325981,2.64052352569889,
-7.17803035289206));
#104845=CARTESIAN_POINT('Ctrl Pts',(-2.29323496566152,2.6596257501205,-7.14182983331167));
#104846=CARTESIAN_POINT('Ctrl Pts',(-2.40790356477931,2.67857142912876,
-7.10295716073582));
#104847=CARTESIAN_POINT('Ctrl Pts',(-2.47313954588311,2.68934979359667,
-7.08084215318911));
#104848=CARTESIAN_POINT('Ctrl Pts',(-2.53817211940977,2.70017879536063,
-7.05779390899266));
#104849=CARTESIAN_POINT('Ctrl Pts',(-2.60296178584741,2.71105259961602,
-7.03381759402564));
#104850=CARTESIAN_POINT('Ctrl Pts',(-2.51680165573333,2.74999999864878,
-6.7991329985847));
#104851=CARTESIAN_POINT('Ctrl Pts',(-2.5312452108601,2.74318451262334,-6.83815222697435));
#104852=CARTESIAN_POINT('Ctrl Pts',(-2.54565191943021,2.73653622822029,
-6.87724248802998));
#104853=CARTESIAN_POINT('Ctrl Pts',(-2.57436387743132,2.72356451297556,
-6.95545837152627));
#104854=CARTESIAN_POINT('Ctrl Pts',(-2.58868622039588,2.71723336167073,
-6.99463058052567));
#104855=CARTESIAN_POINT('Ctrl Pts',(-2.60296178012173,2.71105259871072,
-7.03381759585593));
#104856=CARTESIAN_POINT('',(-1.90964624444247,2.62129679787127,-7.12115279973941));
#104857=CARTESIAN_POINT('Origin',(3.33500588256541E-13,2.71213386200044,
9.0726037793587E-13));
#104858=CARTESIAN_POINT('',(-2.59611851412711,2.53084202105566,-7.03634625720979));
#104859=CARTESIAN_POINT('Origin',(0.06338529817835,2.55357150892421,0.18232500043781));
#104860=CARTESIAN_POINT('',(-3.12207624230095,2.62129679634651,-6.81928441416267));
#104861=CARTESIAN_POINT('Origin',(0.0466038476729902,2.41079129955947,0.181800031907738));
#104862=CARTESIAN_POINT('Origin',(0.0890965167551067,2.55359536994261,0.168489747675488));
#104863=CARTESIAN_POINT('Ctrl Pts',(-2.51242591,2.750764179,-6.800751138));
#104864=CARTESIAN_POINT('Ctrl Pts',(-2.880932089,2.686419405,-6.664612578));
#104865=CARTESIAN_POINT('Ctrl Pts',(-3.232570193,2.621296797,-6.489452207));
#104866=CARTESIAN_POINT('Ctrl Pts',(-2.366938921,2.750764179,-7.116712734));
#104867=CARTESIAN_POINT('Ctrl Pts',(-2.752565827,2.686419405,-6.98845754600001));
#104868=CARTESIAN_POINT('Ctrl Pts',(-3.122076251,2.621296797,-6.819284411));
#104869=CARTESIAN_POINT('',(-3.17732321119419,2.62129679507543,-6.65436831415955));
#104870=CARTESIAN_POINT('Ctrl Pts',(-3.21651165857331,2.61844385750139,
-6.49708596452346));
#104871=CARTESIAN_POINT('Ctrl Pts',(-3.22432214072034,2.61987032725071,
-6.49319579266259));
#104872=CARTESIAN_POINT('Ctrl Pts',(-3.2321326228674,2.621296797,-6.48930562080173));
#104873=CARTESIAN_POINT('Ctrl Pts',(-3.38970546347181,2.65007516,-6.41082321484841));
#104874=CARTESIAN_POINT('Ctrl Pts',(-3.54328343796041,2.678571429,-6.32478546712723));
#104875=CARTESIAN_POINT('Ctrl Pts',(-3.74224549214338,2.71548867696324,
-6.21332256371282));
#104876=CARTESIAN_POINT('Ctrl Pts',(-3.93380839988302,2.75286253721407,
-6.08957471433534));
#104877=CARTESIAN_POINT('Ctrl Pts',(-3.54651510037374,2.61844385750139,
-6.60852151350342));
#104878=CARTESIAN_POINT('Ctrl Pts',(-3.55445874868688,2.61987032725071,
-6.60423383125171));
#104879=CARTESIAN_POINT('Ctrl Pts',(-3.562402397,2.621296797,-6.599946149));
#104880=CARTESIAN_POINT('Ctrl Pts',(-3.722661803,2.65007516,-6.513444156));
#104881=CARTESIAN_POINT('Ctrl Pts',(-3.878533944,2.678571429,-6.419265881));
#104882=CARTESIAN_POINT('Ctrl Pts',(-4.08046811734263,2.71548867696324,
-6.29725682832218));
#104883=CARTESIAN_POINT('Ctrl Pts',(-4.27433441331535,2.75286253721407,
-6.16279687550622));
#104884=CARTESIAN_POINT('',(-3.56240238961421,2.62129679728566,-6.59994615216608));
#104885=CARTESIAN_POINT('',(-4.05416884645219,2.71105259871873,-6.30981100856601));
#104886=CARTESIAN_POINT('Ctrl Pts',(-3.5624023893076,2.62129679564632,-6.59994615301723));
#104887=CARTESIAN_POINT('Ctrl Pts',(-3.6694711736048,2.6405235256989,-6.54215445488011));
#104888=CARTESIAN_POINT('Ctrl Pts',(-3.77490270970122,2.65962575012087,
-6.4818800904607));
#104889=CARTESIAN_POINT('Ctrl Pts',(-3.87853394488343,2.6785714291951,-6.41926588030341));
#104890=CARTESIAN_POINT('Ctrl Pts',(-3.93749067224208,2.68934979370444,
-6.38364410140354));
#104891=CARTESIAN_POINT('Ctrl Pts',(-3.99604812892601,2.70017879536494,
-6.34715463168932));
#104892=CARTESIAN_POINT('Ctrl Pts',(-4.05416885006854,2.71105259961824,
-6.30981100648448));
#104893=CARTESIAN_POINT('Ctrl Pts',(-3.91957284471539,2.74999999874113,
-6.09913508762071));
#104894=CARTESIAN_POINT('Ctrl Pts',(-3.94206669846907,2.74318451268703,
-6.13413713061112));
#104895=CARTESIAN_POINT('Ctrl Pts',(-3.96453983709032,2.73653622822721,
-6.16921646674623));
#104896=CARTESIAN_POINT('Ctrl Pts',(-4.0093946284799,2.72356451297479,-6.23943148399764));
#104897=CARTESIAN_POINT('Ctrl Pts',(-4.03180299005541,2.71723336166631,
-6.27460898817795));
#104898=CARTESIAN_POINT('Ctrl Pts',(-4.05416884499283,2.71105259872132,
-6.30981100949368));
#104899=CARTESIAN_POINT('',(-3.39583712923581,2.62129679787127,-6.54414671075182));
#104900=CARTESIAN_POINT('Origin',(-1.84531209757033E-13,2.71213386199944,
-1.73038666728687E-13));
#104901=CARTESIAN_POINT('',(-4.04802915911569,2.53084202100993,-6.31375165200503));
#104902=CARTESIAN_POINT('Origin',(0.101097921576143,2.55357153451447,0.164436471716356));
#104903=CARTESIAN_POINT('',(-4.51502840745966,2.62129679635372,-5.9886992297988));
#104904=CARTESIAN_POINT('Origin',(0.0845957595437319,2.41079130381635,0.167530973877907));
#104905=CARTESIAN_POINT('Origin',(0.123233812183939,2.55359542229066,0.145397460344019));
#104906=CARTESIAN_POINT('Ctrl Pts',(-3.915647254,2.750764179,-6.101656052));
#104907=CARTESIAN_POINT('Ctrl Pts',(-4.246272197,2.686419405,-5.8894824));
#104908=CARTESIAN_POINT('Ctrl Pts',(-4.552034896,2.621296797,-5.642825383));
#104909=CARTESIAN_POINT('Ctrl Pts',(-3.841484074,2.750764179,-6.44150604300001));
#104910=CARTESIAN_POINT('Ctrl Pts',(-4.190524162,2.686419405,-6.233351005));
#104911=CARTESIAN_POINT('Ctrl Pts',(-4.515028415,2.621296797,-5.988699225));
#104912=CARTESIAN_POINT('',(-4.53353164605597,2.62129679507543,-5.81576231136186));
#104913=CARTESIAN_POINT('Ctrl Pts',(-4.53799284712549,2.61844386027133,
-5.65373276708909));
#104914=CARTESIAN_POINT('Ctrl Pts',(-4.54478444599355,2.61987032863568,
-5.64825452784854));
#104915=CARTESIAN_POINT('Ctrl Pts',(-4.55157604486155,2.621296797,-5.64277628860798));
#104916=CARTESIAN_POINT('Ctrl Pts',(-4.68859352275467,2.65007516,-5.53225525539869));
#104917=CARTESIAN_POINT('Ctrl Pts',(-4.82008535682161,2.678571429,-5.41521429691583));
#104918=CARTESIAN_POINT('Ctrl Pts',(-4.99043455325611,2.71548867555358,
-5.26358637970675));
#104919=CARTESIAN_POINT('Ctrl Pts',(-5.15091669160818,2.75286253436271,
-5.10155133003253));
#104920=CARTESIAN_POINT('Ctrl Pts',(-4.88423633966056,2.61844386027133,
-5.69162202889658));
#104921=CARTESIAN_POINT('Ctrl Pts',(-4.89107253833026,2.61987032863568,
-5.68572694644828));
#104922=CARTESIAN_POINT('Ctrl Pts',(-4.897908737,2.621296797,-5.679831864));
#104923=CARTESIAN_POINT('Ctrl Pts',(-5.035825996,2.65007516,-5.560901205));
#104924=CARTESIAN_POINT('Ctrl Pts',(-5.167808388,2.678571429,-5.435416862));
#104925=CARTESIAN_POINT('Ctrl Pts',(-5.33879310681165,2.71548867555358,
-5.27285044207639));
#104926=CARTESIAN_POINT('Ctrl Pts',(-5.49922199451123,2.75286253436271,
-5.09985857233358));
#104927=CARTESIAN_POINT('',(-4.89790873051315,2.62129679728566,-5.67983186868445));
#104928=CARTESIAN_POINT('',(-5.31580748222907,2.71105259874511,-5.29076467184931));
#104929=CARTESIAN_POINT('Ctrl Pts',(-4.89790873035063,2.6212967956464,-5.67983186957653));
#104930=CARTESIAN_POINT('Ctrl Pts',(-4.99005079942674,2.64052352569892,
-5.60037468588713));
#104931=CARTESIAN_POINT('Ctrl Pts',(-5.08006019835419,2.65962575012044,
-5.51884483873591));
#104932=CARTESIAN_POINT('Ctrl Pts',(-5.16780838853741,2.67857142911603,
-5.43541686148905));
#104933=CARTESIAN_POINT('Ctrl Pts',(-5.21772911097534,2.68934979358859,
-5.38795394676343));
#104934=CARTESIAN_POINT('Ctrl Pts',(-5.26707336984754,2.70017879537978,
-5.33972945793456));
#104935=CARTESIAN_POINT('Ctrl Pts',(-5.3158074852467,2.71105259963722,-5.29076466905523));
#104936=CARTESIAN_POINT('Ctrl Pts',(-5.13906916553877,2.74999999856141,
-5.11394839909537));
#104937=CARTESIAN_POINT('Ctrl Pts',(-5.16856153009576,2.74318451249827,
-5.14329660033381));
#104938=CARTESIAN_POINT('Ctrl Pts',(-5.1980502790435,2.736536228155,-5.17272474019524));
#104939=CARTESIAN_POINT('Ctrl Pts',(-5.25695027066359,2.72356457300384,
-5.23165544222286));
#104940=CARTESIAN_POINT('Ctrl Pts',(-5.28639655221916,2.71723348380006,
-5.26119306894966));
#104941=CARTESIAN_POINT('Ctrl Pts',(-5.31580748100938,2.71105259874964,
-5.29076467304409));
#104942=CARTESIAN_POINT('',(-4.72324244319091,2.62129679787127,-5.66114359451915));
#104943=CARTESIAN_POINT('Origin',(-4.76615275024628E-13,2.71213386199922,
-4.74446870679657E-13));
#104944=CARTESIAN_POINT('',(-5.31065845856635,2.5308420210107,-5.29593303699472));
#104945=CARTESIAN_POINT('Origin',(0.134083019446607,2.55357153242441,0.138858695162986));
#104946=CARTESIAN_POINT('',(-5.6968628626643,2.62129679635371,-4.87808912527821));
#104947=CARTESIAN_POINT('Origin',(0.11863234393832,2.41079130577976,0.14542877855957));
#104948=CARTESIAN_POINT('Origin',(0.151608896027703,2.55359538524557,0.115506578058185));
#104949=CARTESIAN_POINT('Ctrl Pts',(-5.135777285,2.750764179,-5.11725431));
#104950=CARTESIAN_POINT('Ctrl Pts',(-5.413061337,2.686419405,-4.838966571));
#104951=CARTESIAN_POINT('Ctrl Pts',(-5.658651506,2.621296797,-4.532346316));
#104952=CARTESIAN_POINT('Ctrl Pts',(-5.136405701,2.750764179,-5.465101689));
#104953=CARTESIAN_POINT('Ctrl Pts',(-5.432538246,2.686419405,-5.186779898));
#104954=CARTESIAN_POINT('Ctrl Pts',(-5.696862869,2.621296797,-4.878089119));
#104955=CARTESIAN_POINT('',(-5.67775717985935,2.62129679507543,-4.70521772671993));
#104956=CARTESIAN_POINT('Ctrl Pts',(-5.64728250819685,2.6184438579262,-4.54601732828464));
#104957=CARTESIAN_POINT('Ctrl Pts',(-5.65273766822465,2.61987032746311,
-4.5392071685867));
#104958=CARTESIAN_POINT('Ctrl Pts',(-5.65819282825249,2.621296797,-4.53239700888875));
#104959=CARTESIAN_POINT('Ctrl Pts',(-5.76824815817284,2.65007516,-4.39500518746768));
#104960=CARTESIAN_POINT('Ctrl Pts',(-5.87150544120964,2.678571429,-4.25243372517932));
#104961=CARTESIAN_POINT('Ctrl Pts',(-6.0052764513976,2.71548867669054,-4.06773073697445));
#104962=CARTESIAN_POINT('Ctrl Pts',(-6.12717386396559,2.75286253666248,
-3.87498505535434));
#104963=CARTESIAN_POINT('Ctrl Pts',(-5.99357609275843,2.6184438579262,-4.50858864453285));
#104964=CARTESIAN_POINT('Ctrl Pts',(-5.99898520087922,2.61987032746311,
-4.50136179926641));
#104965=CARTESIAN_POINT('Ctrl Pts',(-6.004394309,2.621296797,-4.494134954));
#104966=CARTESIAN_POINT('Ctrl Pts',(-6.113520563,2.65007516,-4.348336694));
#104967=CARTESIAN_POINT('Ctrl Pts',(-6.215441855,2.678571429,-4.197413792));
#104968=CARTESIAN_POINT('Ctrl Pts',(-6.34748207552619,2.71548867669054,
-4.00189141849574));
#104969=CARTESIAN_POINT('Ctrl Pts',(-6.466972089439,2.75286253666248,-3.7984565275671));
#104970=CARTESIAN_POINT('',(-6.00439430365377,2.62129679728566,-4.49413495997162));
#104971=CARTESIAN_POINT('',(-6.32888486767079,2.71105259873234,-4.02432805943173));
#104972=CARTESIAN_POINT('Ctrl Pts',(-6.00439430370528,2.62129679564633,
-4.49413496087588));
#104973=CARTESIAN_POINT('Ctrl Pts',(-6.07730119665115,2.64052352569891,
-4.39672762094362));
#104974=CARTESIAN_POINT('Ctrl Pts',(-6.14767971852342,2.65962575012029,
-4.29775453615439));
#104975=CARTESIAN_POINT('Ctrl Pts',(-6.21544185532184,2.67857142908998,
-4.19741379152342));
#104976=CARTESIAN_POINT('Ctrl Pts',(-6.25399233533359,2.68934979354362,
-4.14032905383643));
#104977=CARTESIAN_POINT('Ctrl Pts',(-6.29181611341531,2.70017879537231,
-4.08262446955145));
#104978=CARTESIAN_POINT('Ctrl Pts',(-6.32888487002719,2.71105259962688,
-4.02432805604451));
#104979=CARTESIAN_POINT('Ctrl Pts',(-6.11826832263678,2.74999999864412,
-3.88963916710401));
#104980=CARTESIAN_POINT('Ctrl Pts',(-6.15338016777334,2.74318451258122,
-3.91196123685969));
#104981=CARTESIAN_POINT('Ctrl Pts',(-6.18850566656794,2.73653622817913,
-3.93436215385672));
#104982=CARTESIAN_POINT('Ctrl Pts',(-6.25869729295971,2.72356451295359,
-3.97925353934956));
#104983=CARTESIAN_POINT('Ctrl Pts',(-6.29380522164525,2.71723336165523,
-4.00177075055494));
#104984=CARTESIAN_POINT('Ctrl Pts',(-6.32888486674516,2.71105259873492,
-4.02432806087192));
#104985=CARTESIAN_POINT('',(-5.82979419021296,2.62129679787127,-4.51343169603635));
#104986=CARTESIAN_POINT('Origin',(-5.78096598369271E-13,2.71213386199944,
-3.45209971719385E-13));
#104987=CARTESIAN_POINT('',(-6.32496727096945,2.53084202101589,-4.03048247922101));
#104988=CARTESIAN_POINT('Origin',(0.160798984945445,2.55357150552199,0.106788523341716));
#104989=CARTESIAN_POINT('',(-6.61231834116049,2.62129679635372,-3.53938499548876));
#104990=CARTESIAN_POINT('Origin',(0.147121763757694,2.41079132245498,0.116526339602698));
#104991=CARTESIAN_POINT('Origin',(0.172895077899152,2.55359537142438,0.0802147940364417));
#104992=CARTESIAN_POINT('Ctrl Pts',(-6.115764078,2.750764179,-3.893575445));
#104993=CARTESIAN_POINT('Ctrl Pts',(-6.326741745,2.686419405,-3.562186043));
#104994=CARTESIAN_POINT('Ctrl Pts',(-6.500675861,2.621296797,-3.209939773));
#104995=CARTESIAN_POINT('Ctrl Pts',(-6.191154706,2.750764179,-4.233155254));
#104996=CARTESIAN_POINT('Ctrl Pts',(-6.420532878,2.686419405,-3.897680728));
#104997=CARTESIAN_POINT('Ctrl Pts',(-6.612318346,2.621296797,-3.539384988));
#104998=CARTESIAN_POINT('',(-6.55649709801999,2.62129679507543,-3.37466239114689));
#104999=CARTESIAN_POINT('Ctrl Pts',(-6.49251152790548,2.61844385805783,
-3.22573516232869));
#105000=CARTESIAN_POINT('Ctrl Pts',(-6.49637516612974,2.61987032752893,
-3.2179115226025));
#105001=CARTESIAN_POINT('Ctrl Pts',(-6.500238804354,2.621296797,-3.21008788287631));
#105002=CARTESIAN_POINT('Ctrl Pts',(-6.57818592174632,2.65007516,-3.05224956345433));
#105003=CARTESIAN_POINT('Ctrl Pts',(-6.64838045698693,2.678571429,-2.89081407897152));
#105004=CARTESIAN_POINT('Ctrl Pts',(-6.73931829222693,2.71548867670329,
-2.68167253086331));
#105005=CARTESIAN_POINT('Ctrl Pts',(-6.8169311873176,2.75286253668826,-2.46722879455499));
#105006=CARTESIAN_POINT('Ctrl Pts',(-6.82266290017222,2.61844385805783,
-3.11473865527265));
#105007=CARTESIAN_POINT('Ctrl Pts',(-6.82639198808613,2.61987032752893,
-3.10651797163632));
#105008=CARTESIAN_POINT('Ctrl Pts',(-6.830121076,2.621296797,-3.098297288));
#105009=CARTESIAN_POINT('Ctrl Pts',(-6.905353703,2.65007516,-2.932448791));
#105010=CARTESIAN_POINT('Ctrl Pts',(-6.972448169,2.678571429,-2.763144319));
#105011=CARTESIAN_POINT('Ctrl Pts',(-7.05936983164764,2.71548867670329,
-2.54380840441185));
#105012=CARTESIAN_POINT('Ctrl Pts',(-7.13233374779166,2.75286253668826,
-2.31944288760547));
#105013=CARTESIAN_POINT('',(-6.83012107208854,2.62129679728566,-3.09829729497249));
#105014=CARTESIAN_POINT('',(-7.04603063111164,2.7110525987244,-2.56971833966129));
#105015=CARTESIAN_POINT('Ctrl Pts',(-6.8301210723073,2.62129679564632,-3.09829729585335));
#105016=CARTESIAN_POINT('Ctrl Pts',(-6.8803837440735,2.64052352569889,-2.98749445823591));
#105017=CARTESIAN_POINT('Ctrl Pts',(-6.927840567671,2.65962575012087,-2.87570600767742));
#105018=CARTESIAN_POINT('Ctrl Pts',(-6.97244816946066,2.67857142919565,
-2.76314431783758));
#105019=CARTESIAN_POINT('Ctrl Pts',(-6.99782582954319,2.68934979370559,
-2.69910697527566));
#105020=CARTESIAN_POINT('Ctrl Pts',(-7.02236052837708,2.7001787953517,-2.6346204987359));
#105021=CARTESIAN_POINT('Ctrl Pts',(-7.04603063233495,2.71105259957602,
-2.56971833610226));
#105022=CARTESIAN_POINT('Ctrl Pts',(-6.81138405351766,2.74999999863303,
-2.48345472967256));
#105023=CARTESIAN_POINT('Ctrl Pts',(-6.85047358844989,2.74318451256408,
-2.49770691327413));
#105024=CARTESIAN_POINT('Ctrl Pts',(-6.8895934074537,2.73653622818423,-2.51203316538098));
#105025=CARTESIAN_POINT('Ctrl Pts',(-6.96779397439078,2.72356456920812,
-2.54078576580119));
#105026=CARTESIAN_POINT('Ctrl Pts',(-7.00692124906745,2.71723347608493,
-2.55522922667391));
#105027=CARTESIAN_POINT('Ctrl Pts',(-7.04603063056539,2.71105259872689,
-2.56971834113679));
#105028=CARTESIAN_POINT('',(-6.66375124013802,2.62129679787127,-3.1546767477559));
#105029=CARTESIAN_POINT('Origin',(-1.63324215263216E-12,2.71213386200011,
-5.73976630113826E-13));
#105030=CARTESIAN_POINT('',(-7.04352764417412,2.53084202101217,-2.57657103907726));
#105031=CARTESIAN_POINT('Origin',(0.179995935634774,2.55357153834234,0.06972483404799));
#105032=CARTESIAN_POINT('',(-7.21858916277932,2.62129679634651,-2.03518315668438));
#105033=CARTESIAN_POINT('Origin',(0.168731710674025,2.41079132945112,0.0821751309787647));
#105034=CARTESIAN_POINT('Origin',(0.18609630974445,2.55359540305191,0.0411719527489995));
#105035=CARTESIAN_POINT('Ctrl Pts',(-6.80978454,2.750764179,-2.487837318));
#105036=CARTESIAN_POINT('Ctrl Pts',(-6.944590741,2.686419405,-2.118841655));
#105037=CARTESIAN_POINT('Ctrl Pts',(-7.038735838,2.621296797,-1.737440013));
#105038=CARTESIAN_POINT('Ctrl Pts',(-6.956412198,2.750764179,-2.803271184));
#105039=CARTESIAN_POINT('Ctrl Pts',(-7.10831053000001,2.686419405,-2.42633034));
#105040=CARTESIAN_POINT('Ctrl Pts',(-7.218589166,2.621296797,-2.035183148));
#105041=CARTESIAN_POINT('',(-7.12866249893688,2.62129679507543,-1.88631159207601));
#105042=CARTESIAN_POINT('Ctrl Pts',(-7.03415792518274,2.61844385865813,
-1.7546212015925));
#105043=CARTESIAN_POINT('Ctrl Pts',(-7.03624938200634,2.61987032782908,
-1.74614990797347));
#105044=CARTESIAN_POINT('Ctrl Pts',(-7.03834083882998,2.621296797,-1.73767861435444));
#105045=CARTESIAN_POINT('Ctrl Pts',(-7.08053502353146,2.65007516,-1.56677414069536));
#105046=CARTESIAN_POINT('Ctrl Pts',(-7.11438459092148,2.678571429,-1.39402317853381));
#105047=CARTESIAN_POINT('Ctrl Pts',(-7.15823710012756,2.7154886763785,-1.17022229926958));
#105048=CARTESIAN_POINT('Ctrl Pts',(-7.18793638372117,2.7528625360313,-0.944107662566128));
#105049=CARTESIAN_POINT('Ctrl Pts',(-7.33272957398523,2.61844385865813,
-1.57524694584273));
#105050=CARTESIAN_POINT('Ctrl Pts',(-7.3346042734926,2.61987032782908,-1.56641681542136));
#105051=CARTESIAN_POINT('Ctrl Pts',(-7.336478973,2.621296797,-1.557586685));
#105052=CARTESIAN_POINT('Ctrl Pts',(-7.374300178,2.65007516,-1.379442843));
#105053=CARTESIAN_POINT('Ctrl Pts',(-7.403430556,2.678571429,-1.199673288));
#105054=CARTESIAN_POINT('Ctrl Pts',(-7.44116929989033,2.7154886763785,-0.966779739269926));
#105055=CARTESIAN_POINT('Ctrl Pts',(-7.46419540639517,2.7528625360313,-0.731974680503638));
#105056=CARTESIAN_POINT('',(-7.33647897188281,2.6212967972753,-1.55758668986226));
#105057=CARTESIAN_POINT('',(-7.43371183306277,2.71105259873374,-0.994951446310446));
#105058=CARTESIAN_POINT('Ctrl Pts',(-7.33647897108187,2.62129679564632,
-1.55758669346358));
#105059=CARTESIAN_POINT('Ctrl Pts',(-7.36174719434701,2.64052352569893,
-1.43856937610547));
#105060=CARTESIAN_POINT('Ctrl Pts',(-7.38406329122853,2.65962575012077,
-1.31919266302739));
#105061=CARTESIAN_POINT('Ctrl Pts',(-7.4034305561815,2.67857142917754,-1.19967328687996));
#105062=CARTESIAN_POINT('Ctrl Pts',(-7.4144487649051,2.6893497936799,-1.1316776551174));
#105063=CARTESIAN_POINT('Ctrl Pts',(-7.42454716987242,2.70017879535656,
-1.06342460138614));
#105064=CARTESIAN_POINT('Ctrl Pts',(-7.43371183347961,2.71105259958219,
-0.994951442592408));
#105065=CARTESIAN_POINT('Ctrl Pts',(-7.18600703533534,2.74999999872123,
-0.961146710006495));
#105066=CARTESIAN_POINT('Ctrl Pts',(-7.22724647673893,2.74318451266386,
-0.966662590906057));
#105067=CARTESIAN_POINT('Ctrl Pts',(-7.26853141705599,2.73653622824394,
-0.972244298447054));
#105068=CARTESIAN_POINT('Ctrl Pts',(-7.35108465813915,2.72356456914425,
-0.98351386869375));
#105069=CARTESIAN_POINT('Ctrl Pts',(-7.39240207692326,2.71723347589383,
-0.989208442053305));
#105070=CARTESIAN_POINT('Ctrl Pts',(-7.43371183284747,2.71105259873624,
-0.994951447861807));
#105071=CARTESIAN_POINT('',(-7.18611868862997,2.62129679787127,-1.64841262084963));
#105072=CARTESIAN_POINT('Origin',(1.28282801048485E-12,2.712133862001,2.74303149638833E-13));
#105073=CARTESIAN_POINT('',(-7.43274049270506,2.53084202102667,-1.00218200151022));
#105074=CARTESIAN_POINT('Origin',(0.190776648901901,2.55357153535686,0.0294009220419665));
#105075=CARTESIAN_POINT('',(-7.48732677872139,2.62129679634651,-0.435818415173266));
#105076=CARTESIAN_POINT('Origin',(0.182451887431564,2.41079132038099,0.0439815725696998));
#105077=CARTESIAN_POINT('Origin',(0.190596324983798,2.55359539930593,0.00020417990560892));
#105078=CARTESIAN_POINT('Ctrl Pts',(-7.185387045,2.750764179,-0.965770684));
#105079=CARTESIAN_POINT('Ctrl Pts',(-7.237718391,2.686419405,-0.576422586));
#105080=CARTESIAN_POINT('Ctrl Pts',(-7.24767235000001,2.621296797,-0.18369949));
#105081=CARTESIAN_POINT('Ctrl Pts',(-7.396395587,2.750764179,-1.242309269));
#105082=CARTESIAN_POINT('Ctrl Pts',(-7.463711481,2.686419405,-0.841527441));
#105083=CARTESIAN_POINT('Ctrl Pts',(-7.48732678,2.621296797,-0.435818406));
#105084=CARTESIAN_POINT('',(-7.36749956449699,2.62129679507543,-0.309758959963846));
#105085=CARTESIAN_POINT('Ctrl Pts',(-7.24689491401017,2.61844385892813,
-0.201463106179223));
#105086=CARTESIAN_POINT('Ctrl Pts',(-7.24711639599255,2.61987032796408,
-0.192740266134972));
#105087=CARTESIAN_POINT('Ctrl Pts',(-7.24733787797487,2.621296797,-0.184017426090723));
#105088=CARTESIAN_POINT('Ctrl Pts',(-7.25180617607661,2.65007516,-0.00803810171583814));
#105089=CARTESIAN_POINT('Ctrl Pts',(-7.24772800926328,2.678571429,0.167950695928088));
#105090=CARTESIAN_POINT('Ctrl Pts',(-7.24244469784854,2.71548867625678,
0.395946228542094));
#105091=CARTESIAN_POINT('Ctrl Pts',(-7.22284166571237,2.75286253578508,
0.623158897767339));
#105092=CARTESIAN_POINT('Ctrl Pts',(-7.49992596089625,2.61844385892813,
0.0379015589993896));
#105093=CARTESIAN_POINT('Ctrl Pts',(-7.49985861394813,2.61987032796408,
0.0469282499996948));
#105094=CARTESIAN_POINT('Ctrl Pts',(-7.499791267,2.621296797,0.055954941));
#105095=CARTESIAN_POINT('Ctrl Pts',(-7.498432573,2.65007516,0.23806432));
#105096=CARTESIAN_POINT('Ctrl Pts',(-7.488236759,2.678571429,0.419893133));
#105097=CARTESIAN_POINT('Ctrl Pts',(-7.47502796352101,2.71548867625678,
0.655454472556969));
#105098=CARTESIAN_POINT('Ctrl Pts',(-7.44703958575088,2.75286253578508,
0.889719851663243));
#105099=CARTESIAN_POINT('',(-7.49979126766924,2.6212967972884,0.0559549390073793));
#105100=CARTESIAN_POINT('',(-7.47380093222409,2.71105259872497,0.62633827058748));
#105101=CARTESIAN_POINT('Ctrl Pts',(-7.49979126689562,2.62129679671618,
0.0559549390920314));
#105102=CARTESIAN_POINT('Ctrl Pts',(-7.49888352787154,2.64052352640753,
0.177621616481776));
#105103=CARTESIAN_POINT('Ctrl Pts',(-7.49501542236969,2.65962575047207,
0.29900466727516));
#105104=CARTESIAN_POINT('Ctrl Pts',(-7.48823675894358,2.67857142915768,
0.419893134006151));
#105105=CARTESIAN_POINT('Ctrl Pts',(-7.48438031722435,2.68934979364746,
0.488667654481343));
#105106=CARTESIAN_POINT('Ctrl Pts',(-7.47957023810782,2.70017879535944,
0.557495848336267));
#105107=CARTESIAN_POINT('Ctrl Pts',(-7.47380093223093,2.71105259897497,
0.626338270548561));
#105108=CARTESIAN_POINT('Ctrl Pts',(-7.22462031598099,2.74999999861703,
0.606103461913437));
#105109=CARTESIAN_POINT('Ctrl Pts',(-7.26608135359757,2.74318451256247,
0.609581800086605));
#105110=CARTESIAN_POINT('Ctrl Pts',(-7.30760097709695,2.73653622816163,
0.613005631471987));
#105111=CARTESIAN_POINT('Ctrl Pts',(-7.39064678583536,2.72356457033612,
0.6197460432713));
#105112=CARTESIAN_POINT('Ctrl Pts',(-7.43222238227318,2.71723347837816,
0.623066628800585));
#105113=CARTESIAN_POINT('Ctrl Pts',(-7.47380093235173,2.71105259872747,
0.626338268970032));
#105114=CARTESIAN_POINT('',(-7.37247121386783,2.62129679787127,-0.065070551999726));
#105115=CARTESIAN_POINT('Origin',(9.15066633577766E-14,2.71213386199933,
1.52838625002566E-14));
#105116=CARTESIAN_POINT('',(-7.4744066564856,2.53084202101296,0.619067951245984));
#105117=CARTESIAN_POINT('Origin',(0.192636453794941,2.55357154185465,-0.0122977839903749));
#105118=CARTESIAN_POINT('',(-7.40596531666914,2.62129679635372,1.18392471111636));
#105119=CARTESIAN_POINT('Origin',(0.187641356349404,2.4107912956149,0.00373151825628901));
#105120=CARTESIAN_POINT('Origin',(0.186184210808453,2.55359535292823,-0.040773175267849));
#105121=CARTESIAN_POINT('Ctrl Pts',(-7.225008838,2.750764179,0.601454314));
#105122=CARTESIAN_POINT('Ctrl Pts',(-7.192418375,2.686419405,0.992949363));
#105123=CARTESIAN_POINT('Ctrl Pts',(-7.117715759,2.621296797,1.378630618));
#105124=CARTESIAN_POINT('Ctrl Pts',(-7.490531739,2.750764179,0.376741646));
#105125=CARTESIAN_POINT('Ctrl Pts',(-7.470117579,2.686419405,0.782624346));
#105126=CARTESIAN_POINT('Ctrl Pts',(-7.40596531600001,2.621296797,1.18392472));
#105127=CARTESIAN_POINT('',(-7.26184053958062,2.62129679507543,1.28127765720773));
#105128=CARTESIAN_POINT('Ctrl Pts',(-7.12077515222738,2.61844385828202,
1.36111517550213));
#105129=CARTESIAN_POINT('Ctrl Pts',(-7.11911630287345,2.61987032764103,
1.36968169442626));
#105130=CARTESIAN_POINT('Ctrl Pts',(-7.11745745351951,2.621296797,1.37824821335038));
#105131=CARTESIAN_POINT('Ctrl Pts',(-7.08399093103904,2.65007516,1.55107379119606));
#105132=CARTESIAN_POINT('Ctrl Pts',(-7.04217572103884,2.678571429,1.72207138310816));
#105133=CARTESIAN_POINT('Ctrl Pts',(-6.9880036296484,2.71548867665875,1.94360075211794));
#105134=CARTESIAN_POINT('Ctrl Pts',(-6.92001489751408,2.75286253659817,
2.16128724597702));
#105135=CARTESIAN_POINT('Ctrl Pts',(-7.31643414512728,2.61844385828202,
1.64927782224517));
#105136=CARTESIAN_POINT('Ctrl Pts',(-7.31442790056365,2.61987032764103,
1.6580789986226));
#105137=CARTESIAN_POINT('Ctrl Pts',(-7.312421656,2.621296797,1.666880175));
#105138=CARTESIAN_POINT('Ctrl Pts',(-7.271946595,2.65007516,1.844439859));
#105139=CARTESIAN_POINT('Ctrl Pts',(-7.222901333,2.678571429,2.019825817));
#105140=CARTESIAN_POINT('Ctrl Pts',(-7.15936262624074,2.71548867665875,
2.2470403659787));
#105141=CARTESIAN_POINT('Ctrl Pts',(-7.08166846786064,2.75286253659817,
2.46981207901721));
#105142=CARTESIAN_POINT('',(-7.31242165711993,2.62129679728566,1.66688016710317));
#105143=CARTESIAN_POINT('',(-7.16442340568091,2.71105259871166,2.21834110639597));
#105144=CARTESIAN_POINT('Ctrl Pts',(-7.31242165781292,2.62129679564631,
1.66688016651325));
#105145=CARTESIAN_POINT('Ctrl Pts',(-7.28538040220296,2.6405235256989,1.78550720985933));
#105146=CARTESIAN_POINT('Ctrl Pts',(-7.25550896261107,2.6596257501206,1.90322086635885));
#105147=CARTESIAN_POINT('Ctrl Pts',(-7.22290133274773,2.67857142914657,
2.0198258179021));
#105148=CARTESIAN_POINT('Ctrl Pts',(-7.2043505635659,2.68934979362375,2.0861634074725));
#105149=CARTESIAN_POINT('Ctrl Pts',(-7.18485691423706,2.70017879534133,
2.15234841177172));
#105150=CARTESIAN_POINT('Ctrl Pts',(-7.16442340449928,2.71105259955887,
2.21834110993971));
#105151=CARTESIAN_POINT('Ctrl Pts',(-6.9254183801212,2.74999999862198,2.14501290959327));
#105152=CARTESIAN_POINT('Ctrl Pts',(-6.96516234178542,2.74318451253604,
2.15732282371328));
#105153=CARTESIAN_POINT('Ctrl Pts',(-7.00497523682302,2.73653622813951,
2.16959209955852));
#105154=CARTESIAN_POINT('Ctrl Pts',(-7.08463049941604,2.7235645689707,2.19402732086462));
#105155=CARTESIAN_POINT('Ctrl Pts',(-7.12452026293017,2.71723347564953,
2.2062077999943));
#105156=CARTESIAN_POINT('Ctrl Pts',(-7.16442340613617,2.71105259871414,
2.21834110489999));
#105157=CARTESIAN_POINT('',(-7.21409517911789,2.62129679787127,1.52131414348509));
#105158=CARTESIAN_POINT('Origin',(2.80157841370254E-13,2.71213386200022,
-6.41847686111419E-14));
#105159=CARTESIAN_POINT('',(-7.16657787235504,2.5308420210297,2.21137097685949));
#105160=CARTESIAN_POINT('Origin',(0.185489065332484,2.55357149766622,-0.0534214076825659));
#105161=CARTESIAN_POINT('',(-6.97830914658419,2.62129679635372,2.74830883345958));
#105162=CARTESIAN_POINT('Origin',(0.184056299553969,2.41079131761793,-0.03669298340372));
#105163=CARTESIAN_POINT('Origin',(0.173066248691005,2.55359536109132,-0.0798440052102473));
#105164=CARTESIAN_POINT('Ctrl Pts',(-6.926797248,2.750764179,2.140555977));
#105165=CARTESIAN_POINT('Ctrl Pts',(-6.810808868,2.686419405,2.515892103));
#105166=CARTESIAN_POINT('Ctrl Pts',(-6.65494268900001,2.621296797,2.87649749));
#105167=CARTESIAN_POINT('Ctrl Pts',(-7.234418952,2.750764179,1.978176541));
#105168=CARTESIAN_POINT('Ctrl Pts',(-7.127229281,2.686419405,2.370181488));
#105169=CARTESIAN_POINT('Ctrl Pts',(-6.978309144,2.621296797,2.748308842));
#105170=CARTESIAN_POINT('',(-6.81662592106697,2.62129679507543,2.8124031549307));
#105171=CARTESIAN_POINT('Ctrl Pts',(-6.66169585821932,2.6184438580596,2.86004922667223));
#105172=CARTESIAN_POINT('Ctrl Pts',(-6.65823424323192,2.61987032752981,
2.86805886218263));
#105173=CARTESIAN_POINT('Ctrl Pts',(-6.65477262824444,2.621296797,2.87606849769305));
#105174=CARTESIAN_POINT('Ctrl Pts',(-6.58493614400342,2.65007516,3.03765919629072));
#105175=CARTESIAN_POINT('Ctrl Pts',(-6.50733912290844,2.678571429,3.19566992533473));
#105176=CARTESIAN_POINT('Ctrl Pts',(-6.40681127817498,2.71548867668329,
3.40037466356505));
#105177=CARTESIAN_POINT('Ctrl Pts',(-6.2936159231953,2.7528625366478,3.59835620000264));
#105178=CARTESIAN_POINT('Ctrl Pts',(-6.79083400258147,2.6184438580596,3.18353569180921));
#105179=CARTESIAN_POINT('Ctrl Pts',(-6.78698266979072,2.61987032752981,
3.19169981890462));
#105180=CARTESIAN_POINT('Ctrl Pts',(-6.783131337,2.621296797,3.199863946));
#105181=CARTESIAN_POINT('Ctrl Pts',(-6.705432476,2.65007516,3.364571441));
#105182=CARTESIAN_POINT('Ctrl Pts',(-6.619831069,2.678571429,3.525313691));
#105183=CARTESIAN_POINT('Ctrl Pts',(-6.50893345005424,2.71548867668329,
3.73355714601356));
#105184=CARTESIAN_POINT('Ctrl Pts',(-6.38516640466118,2.7528625366478,3.93441863305437));
#105185=CARTESIAN_POINT('',(-6.78313133976152,2.62129679728566,3.19986393845337));
#105186=CARTESIAN_POINT('',(-6.52004540355434,2.71105259878431,3.70661677728345));
#105187=CARTESIAN_POINT('Ctrl Pts',(-6.78313134020659,2.62129679579015,
3.19986393892462));
#105188=CARTESIAN_POINT('Ctrl Pts',(-6.73122098611652,2.64052352569892,
3.30990447608709));
#105189=CARTESIAN_POINT('Ctrl Pts',(-6.6767429675063,2.65962575012078,3.41844457593528));
#105190=CARTESIAN_POINT('Ctrl Pts',(-6.61983106845008,2.67857142917906,
3.52531369197484));
#105191=CARTESIAN_POINT('Ctrl Pts',(-6.58745338552236,2.68934979350172,
3.58611247752341));
#105192=CARTESIAN_POINT('Ctrl Pts',(-6.55418766809202,2.70017879498377,
3.64655955347962));
#105193=CARTESIAN_POINT('Ctrl Pts',(-6.52004540370745,2.71105259900381,
3.70661677733075));
#105194=CARTESIAN_POINT('Ctrl Pts',(-6.30239157675153,2.74999999863007,
3.58362393733051));
#105195=CARTESIAN_POINT('Ctrl Pts',(-6.33856007909119,2.7431845125664,3.60418982947076));
#105196=CARTESIAN_POINT('Ctrl Pts',(-6.37480463932049,2.73653622817309,
3.624730852095));
#105197=CARTESIAN_POINT('Ctrl Pts',(-6.44734506632474,2.72356451355148,
3.66571849367625));
#105198=CARTESIAN_POINT('Ctrl Pts',(-6.48368414002074,2.71723336288666,
3.68618951759012));
#105199=CARTESIAN_POINT('Ctrl Pts',(-6.5200454043226,2.71105259878665,3.70661677591662));
#105200=CARTESIAN_POINT('',(-6.71839607196138,2.62129679787127,3.03656388084945));
#105201=CARTESIAN_POINT('Ctrl Pts',(-6.304696317,2.750764179,3.579567621));
#105202=CARTESIAN_POINT('Ctrl Pts',(-6.110733509,2.686419405,3.921194524));
#105203=CARTESIAN_POINT('Ctrl Pts',(-5.880991895,2.621296797,4.239862537));
#105204=CARTESIAN_POINT('Ctrl Pts',(-6.640032775,2.750764179,3.4871141));
#105205=CARTESIAN_POINT('Ctrl Pts',(-6.451079663,2.686419405,3.846911578));
#105206=CARTESIAN_POINT('Ctrl Pts',(-6.224354992,2.621296797,4.184185097));
#105207=CARTESIAN_POINT('',(-6.22435498239899,2.62129679632898,4.18418508963427));
#105208=CARTESIAN_POINT('Origin',(0.151852228411307,2.55359611104798,-0.115179169971752));
#105209=CARTESIAN_POINT('',(-6.05267345033977,2.62129679507543,4.21202380717125));
#105210=CARTESIAN_POINT('Origin',(-7.40293243373102E-13,2.71213386200011,
4.58617518961368E-13));
#105211=CARTESIAN_POINT('',(-6.52364787172068,2.53084202044609,3.70027275230428));
#105212=CARTESIAN_POINT('Origin',(0.169668428985089,2.55357152054945,-0.0920471349585866));
#105213=CARTESIAN_POINT('Origin',(0.171861648752537,2.410790211888,-0.0753995501951926));
#105214=CARTESIAN_POINT('Ctrl Pts',(-5.89112306978218,2.61844385790313,
4.22525055585264));
#105215=CARTESIAN_POINT('Ctrl Pts',(-5.88602055030678,2.61987032745155,
4.23232878604296));
#105216=CARTESIAN_POINT('Ctrl Pts',(-5.88091803083135,2.621296797,4.23940701623327));
#105217=CARTESIAN_POINT('Ctrl Pts',(-5.77797706175249,2.65007516,4.38220703466827));
#105218=CARTESIAN_POINT('Ctrl Pts',(-5.66822657968978,2.678571429,4.51984249406189));
#105219=CARTESIAN_POINT('Ctrl Pts',(-5.52604355212437,2.71548867684756,
4.69815083468151));
#105220=CARTESIAN_POINT('Ctrl Pts',(-5.37293446337063,2.75286253698008,
4.86717001809344));
#105221=CARTESIAN_POINT('Ctrl Pts',(-5.94770200808611,2.6184438579031,4.5689349698406));
#105222=CARTESIAN_POINT('Ctrl Pts',(-5.94218567104306,2.61987032745156,
4.5760803019203));
#105223=CARTESIAN_POINT('Ctrl Pts',(-5.93666933400001,2.621296797,4.583225634));
#105224=CARTESIAN_POINT('Ctrl Pts',(-5.825379787,2.65007516,4.727379402));
#105225=CARTESIAN_POINT('Ctrl Pts',(-5.707224861,2.678571429,4.865961815));
#105226=CARTESIAN_POINT('Ctrl Pts',(-5.55415377879304,2.71548867684756,
5.04549694470018));
#105227=CARTESIAN_POINT('Ctrl Pts',(-5.39010105545041,2.75286253698008,
5.21505614693326));
#105228=CARTESIAN_POINT('',(-5.93666933833169,2.62129679728565,4.58322562730095));
#105229=CARTESIAN_POINT('',(-5.90855223050183,2.62129679787124,4.4098272657317));
#105230=CARTESIAN_POINT('',(-5.57079732493823,2.71105259873791,5.02157516776287));
#105231=CARTESIAN_POINT('Ctrl Pts',(-5.93666933920874,2.62129679564635,
4.58322562705902));
#105232=CARTESIAN_POINT('Ctrl Pts',(-5.86231715742261,2.64052352569896,
4.67953428736928));
#105233=CARTESIAN_POINT('Ctrl Pts',(-5.78577989171214,2.65962575012079,
4.77382561658219));
#105234=CARTESIAN_POINT('Ctrl Pts',(-5.70722486025002,2.67857142918088,
4.86596181587965));
#105235=CARTESIAN_POINT('Ctrl Pts',(-5.66253420708315,2.68934979368581,
4.91837891579501));
#105236=CARTESIAN_POINT('Ctrl Pts',(-5.6170518883089,2.70017879535638,4.97026162768578));
#105237=CARTESIAN_POINT('Ctrl Pts',(-5.57079732239259,2.71105259957952,
5.02157517044642));
#105238=CARTESIAN_POINT('Ctrl Pts',(-5.38467194878181,2.74999999876017,
4.85466869228265));
#105239=CARTESIAN_POINT('Ctrl Pts',(-5.4155737925532,2.74318451268803,4.88252892416039));
#105240=CARTESIAN_POINT('Ctrl Pts',(-5.4465552624774,2.73653622823916,4.91038121837523));
#105241=CARTESIAN_POINT('Ctrl Pts',(-5.50858833841322,2.72356456892389,
4.96600440205996));
#105242=CARTESIAN_POINT('Ctrl Pts',(-5.53967685772086,2.71723347543569,
4.99380838334581));
#105243=CARTESIAN_POINT('Ctrl Pts',(-5.57079732597209,2.71105259874038,
5.02157516660469));
#105244=CARTESIAN_POINT('Origin',(5.79397640976254E-13,2.71213386199956,
-3.17454396103756E-13));
#105245=CARTESIAN_POINT('',(-5.17935692493163,2.62129679635372,5.42441350133401));
#105246=CARTESIAN_POINT('Origin',(0.123545161789753,2.55359537855859,-0.145133198604221));
#105247=CARTESIAN_POINT('',(-5.57567934709768,2.53084202101785,5.01615388628296));
#105248=CARTESIAN_POINT('Origin',(0.145914194189911,2.55357152512524,-0.126368749652749));
#105249=CARTESIAN_POINT('Origin',(0.151637948404064,2.41079127387234,-0.110584830266146));
#105250=CARTESIAN_POINT('Ctrl Pts',(-5.387794793,2.750764179,4.851202662));
#105251=CARTESIAN_POINT('Ctrl Pts',(-5.124927042,2.686419405,5.143146247));
#105252=CARTESIAN_POINT('Ctrl Pts',(-4.832052457,2.621296797,5.404976323));
#105253=CARTESIAN_POINT('Ctrl Pts',(-5.73516604600001,2.750764179,4.832998079));
#105254=CARTESIAN_POINT('Ctrl Pts',(-5.47328473,2.686419405,5.143764358));
#105255=CARTESIAN_POINT('Ctrl Pts',(-5.179356919,2.621296797,5.424413508));
#105256=CARTESIAN_POINT('',(-5.00570469679279,2.62129679507542,5.41469490737137));
#105257=CARTESIAN_POINT('Ctrl Pts',(-4.84508791585569,2.61844385761768,
5.39288386372956));
#105258=CARTESIAN_POINT('Ctrl Pts',(-4.8385830795463,2.61987032730884,5.39869971856641));
#105259=CARTESIAN_POINT('Ctrl Pts',(-4.83207824323687,2.621296797,5.40451557340326));
#105260=CARTESIAN_POINT('Ctrl Pts',(-4.70084619412413,2.65007516,5.5218477415437));
#105261=CARTESIAN_POINT('Ctrl Pts',(-4.56407406143641,2.678571429,5.63267225195145));
#105262=CARTESIAN_POINT('Ctrl Pts',(-4.38688417180961,2.71548867690094,
5.7762466942276));
#105263=CARTESIAN_POINT('Ctrl Pts',(-4.20102055862152,2.75286253708806,
5.90840037550124));
#105264=CARTESIAN_POINT('Ctrl Pts',(-4.82646208002768,2.61844385761768,
5.74069592738241));
#105265=CARTESIAN_POINT('Ctrl Pts',(-4.81953867601382,2.61987032730884,
5.7464883566912));
#105266=CARTESIAN_POINT('Ctrl Pts',(-4.812615272,2.621296797,5.752280786));
#105267=CARTESIAN_POINT('Ctrl Pts',(-4.672938814,2.65007516,5.86914035499999));
#105268=CARTESIAN_POINT('Ctrl Pts',(-4.527755162,2.678571429,5.979082973));
#105269=CARTESIAN_POINT('Ctrl Pts',(-4.33966805013464,2.71548867690094,
6.12151491333678));
#105270=CARTESIAN_POINT('Ctrl Pts',(-4.1430005717275,2.75286253708806,6.25184342861707));
#105271=CARTESIAN_POINT('',(-4.81261527767175,2.62129679728565,5.75228078036772));
#105272=CARTESIAN_POINT('',(-4.36106495481695,2.71105259870975,6.10173028400751));
#105273=CARTESIAN_POINT('Ctrl Pts',(-4.81261527857913,2.62129679564633,
5.75228078034081));
#105274=CARTESIAN_POINT('Ctrl Pts',(-4.71929789451606,2.64052352569892,
5.83035427570691));
#105275=CARTESIAN_POINT('Ctrl Pts',(-4.62428017899786,2.65962575012086,
5.90598787639623));
#105276=CARTESIAN_POINT('Ctrl Pts',(-4.52775516105093,2.67857142919243,
5.97908297344371));
#105277=CARTESIAN_POINT('Ctrl Pts',(-4.47284122339138,2.68934979369743,
6.02066742111355));
#105278=CARTESIAN_POINT('Ctrl Pts',(-4.41726900647831,2.70017879535494,
6.06155979027765));
#105279=CARTESIAN_POINT('Ctrl Pts',(-4.36106495158897,2.71105259959617,
6.10173028644538));
#105280=CARTESIAN_POINT('Ctrl Pts',(-4.21517104455419,2.74999999871542,
5.89871453534225));
#105281=CARTESIAN_POINT('Ctrl Pts',(-4.23936129417448,2.74318451269066,
5.93256639331657));
#105282=CARTESIAN_POINT('Ctrl Pts',(-4.26363101473255,2.73653622824346,
5.96642761659724));
#105283=CARTESIAN_POINT('Ctrl Pts',(-4.31225643993011,2.72356457207071,
6.03408562230802));
#105284=CARTESIAN_POINT('Ctrl Pts',(-4.33664107949827,2.71723348180313,
6.06792265611851));
#105285=CARTESIAN_POINT('Ctrl Pts',(-4.36106495617808,2.71105259871231,
6.10173028302464));
#105286=CARTESIAN_POINT('',(-4.82243105446794,2.62129679787126,5.57689202868901));
#105287=CARTESIAN_POINT('Origin',(6.75457953458469E-13,2.71213386199944,
-9.74914593498966E-13));
#105288=CARTESIAN_POINT('',(-4.36699825425421,2.53084202105883,6.09748523951929));
#105289=CARTESIAN_POINT('Origin',(0.115337245586927,2.55357151413217,-0.154781541207575));
#105290=CARTESIAN_POINT('',(-3.89217788024747,2.62129679635372,6.41100236577101));
#105291=CARTESIAN_POINT('Origin',(0.124320393779957,2.41079130932435,-0.140597308762092));
#105292=CARTESIAN_POINT('Origin',(0.0894574468630682,2.55359537224088,-0.168298698688354));
#105293=CARTESIAN_POINT('Ctrl Pts',(-4.218965973,2.750764179,5.896000858));
#105294=CARTESIAN_POINT('Ctrl Pts',(-3.899484683,2.686419405,6.12461016899999));
#105295=CARTESIAN_POINT('Ctrl Pts',(-3.557171616,2.621296797,6.317359424));
#105296=CARTESIAN_POINT('Ctrl Pts',(-4.562129326,2.750764179,5.95289643900001));
#105297=CARTESIAN_POINT('Ctrl Pts',(-4.239565086,2.686419405,6.200100433));
#105298=CARTESIAN_POINT('Ctrl Pts',(-3.892177873,2.621296797,6.411002371));
#105299=CARTESIAN_POINT('',(-3.72467475483459,2.62129679507543,6.36418089145162));
#105300=CARTESIAN_POINT('Ctrl Pts',(-3.57250182821409,2.61844385875657,
6.3083519216686));
#105301=CARTESIAN_POINT('Ctrl Pts',(-3.56489883753746,2.6198703278783,6.31263345580127));
#105302=CARTESIAN_POINT('Ctrl Pts',(-3.55729584686083,2.621296797,6.31691498993395));
#105303=CARTESIAN_POINT('Ctrl Pts',(-3.40390898257575,2.65007516,6.40329298549838));
#105304=CARTESIAN_POINT('Ctrl Pts',(-3.24651051216236,2.678571429,6.48212451528638));
#105305=CARTESIAN_POINT('Ctrl Pts',(-3.04259896514593,2.71548867637279,
6.58425167726325));
#105306=CARTESIAN_POINT('Ctrl Pts',(-2.83267160933287,2.75286253601974,
6.67336049472692));
#105307=CARTESIAN_POINT('Ctrl Pts',(-3.47954214211268,2.61844385875657,
6.64402832764031));
#105308=CARTESIAN_POINT('Ctrl Pts',(-3.47153540555634,2.6198703278783,6.64819700432017));
#105309=CARTESIAN_POINT('Ctrl Pts',(-3.463528669,2.621296797,6.652365681));
#105310=CARTESIAN_POINT('Ctrl Pts',(-3.301996416,2.65007516,6.736466829));
#105311=CARTESIAN_POINT('Ctrl Pts',(-3.136572664,2.678571429,6.812628856));
#105312=CARTESIAN_POINT('Ctrl Pts',(-2.9222642706896,2.71548867637279,6.9112976463071));
#105313=CARTESIAN_POINT('Ctrl Pts',(-2.70217799339193,2.75286253601974,
6.99630145831613));
#105314=CARTESIAN_POINT('',(-3.46352867574623,2.62129679728566,6.65236567673181));
#105315=CARTESIAN_POINT('',(-2.94741403486585,2.71105259872076,6.89657527394903));
#105316=CARTESIAN_POINT('Ctrl Pts',(-3.46352867664184,2.62129679564635,
6.65236567688735));
#105317=CARTESIAN_POINT('Ctrl Pts',(-3.35560950750809,2.6405235256989,6.7085533784849));
#105318=CARTESIAN_POINT('Ctrl Pts',(-3.24655426491184,2.65962575012075,
6.76199270759947));
#105319=CARTESIAN_POINT('Ctrl Pts',(-3.13657266304808,2.67857142917358,
6.81262885629644));
#105320=CARTESIAN_POINT('Ctrl Pts',(-3.07400315580616,2.68934979367116,
6.84143620945174));
#105321=CARTESIAN_POINT('Ctrl Pts',(-3.01093953572748,2.70017879536706,
6.86942615381242));
#105322=CARTESIAN_POINT('Ctrl Pts',(-2.9474140310964,2.71105259962305,6.89657527580879));
#105323=CARTESIAN_POINT('Ctrl Pts',(-2.84857342825316,2.74999999861341,
6.66694304341797));
#105324=CARTESIAN_POINT('Ctrl Pts',(-2.86492097448018,2.7431845125352,6.70520365250962));
#105325=CARTESIAN_POINT('Ctrl Pts',(-2.88134412019263,2.73653622816043,
6.74349049123379));
#105326=CARTESIAN_POINT('Ctrl Pts',(-2.91428838878775,2.72356451291915,
6.82002006788017));
#105327=CARTESIAN_POINT('Ctrl Pts',(-2.93082913926675,2.71723336163927,
6.85830838235346));
#105328=CARTESIAN_POINT('Ctrl Pts',(-2.94741403646363,2.71105259872334,
6.89657527325697));
#105329=CARTESIAN_POINT('',(-3.51081836193504,2.62129679787127,6.48318751866981));
#105330=CARTESIAN_POINT('Origin',(-2.53052787058117E-13,2.71213386199933,
6.99093560818653E-13));
#105331=CARTESIAN_POINT('',(-2.95412117554163,2.53084202101381,6.89370496034607));
#105332=CARTESIAN_POINT('Origin',(0.079367334413924,2.55357147941704,-0.175957076628545));
#105333=CARTESIAN_POINT('',(-2.42300492349163,2.62129679634651,7.09781988531365));
#105334=CARTESIAN_POINT('Origin',(0.0911895360214926,2.41079130469772,-0.164035304077856));
#105335=CARTESIAN_POINT('Origin',(0.0511867591664122,2.55359538632789,-0.183594736051459));
#105336=CARTESIAN_POINT('Ctrl Pts',(-2.852862993,2.750764179,6.665108607));
#105337=CARTESIAN_POINT('Ctrl Pts',(-2.491706754,2.686419405,6.819694125));
#105338=CARTESIAN_POINT('Ctrl Pts',(-2.115961384,2.621296797,6.93434982));
#105339=CARTESIAN_POINT('Ctrl Pts',(-3.17577251,2.750764179,6.79444397800001));
#105340=CARTESIAN_POINT('Ctrl Pts',(-2.807608091,2.686419405,6.966526703));
#105341=CARTESIAN_POINT('Ctrl Pts',(-2.423004915,2.621296797,7.097819889));
#105342=CARTESIAN_POINT('',(-2.26948316089319,2.62129679507543,7.01608485081466));
#105343=CARTESIAN_POINT('Ctrl Pts',(-2.13286953419124,2.61844385824803,
6.92884844960035));
#105344=CARTESIAN_POINT('Ctrl Pts',(-2.12452389241223,2.61987032762403,
6.93139546602818));
#105345=CARTESIAN_POINT('Ctrl Pts',(-2.11617825063324,2.621296797,6.93394248245604));
#105346=CARTESIAN_POINT('Ctrl Pts',(-1.94780876957162,2.65007516,6.98532736639538));
#105347=CARTESIAN_POINT('Ctrl Pts',(-1.7771437402721,2.678571429,7.02847984018819));
#105348=CARTESIAN_POINT('Ctrl Pts',(-1.55604521013484,2.71548867650565,
7.08438437089874));
#105349=CARTESIAN_POINT('Ctrl Pts',(-1.33187007596143,2.75286253628849,
7.12628169757759));
#105350=CARTESIAN_POINT('Ctrl Pts',(-1.96992268858995,2.61844385824803,
7.23669334289097));
#105351=CARTESIAN_POINT('Ctrl Pts',(-1.96120700129498,2.61987032762403,
7.23904334694548));
#105352=CARTESIAN_POINT('Ctrl Pts',(-1.952491314,2.621296797,7.241393351));
#105353=CARTESIAN_POINT('Ctrl Pts',(-1.776656335,2.65007516,7.288803601));
#105354=CARTESIAN_POINT('Ctrl Pts',(-1.598727514,2.678571429,7.327623785));
#105355=CARTESIAN_POINT('Ctrl Pts',(-1.36821865771831,2.71548867650565,
7.37791578420156));
#105356=CARTESIAN_POINT('Ctrl Pts',(-1.13500456736235,2.75286253628849,
7.41362021130129));
#105357=CARTESIAN_POINT('',(-1.95249132150711,2.62129679728565,7.24139334827985));
#105358=CARTESIAN_POINT('',(-1.39594530977112,2.71105259875627,7.36894406900818));
#105359=CARTESIAN_POINT('Ctrl Pts',(-1.95249132234728,2.62129679564634,
7.24139334862629));
#105360=CARTESIAN_POINT('Ctrl Pts',(-1.83501654880178,2.64052352569891,
7.27306798144823));
#105361=CARTESIAN_POINT('Ctrl Pts',(-1.71702308126209,2.65962575012074,
7.30181427500216));
#105362=CARTESIAN_POINT('Ctrl Pts',(-1.59872751298808,2.67857142917097,
7.32762378513971));
#105363=CARTESIAN_POINT('Ctrl Pts',(-1.53142811659933,2.68934979367611,
7.34230704387087));
#105364=CARTESIAN_POINT('Ctrl Pts',(-1.46382187832016,2.70017879536824,
7.35608578463689));
#105365=CARTESIAN_POINT('Ctrl Pts',(-1.3959453061231,2.71105259959742,7.36894406960316));
#105366=CARTESIAN_POINT('Ctrl Pts',(-1.34877968348022,2.74999999856131,
7.12343270341778));
#105367=CARTESIAN_POINT('Ctrl Pts',(-1.35652013322406,2.74318451250953,
7.16431304003367));
#105368=CARTESIAN_POINT('Ctrl Pts',(-1.36432877629888,2.73653622815752,
7.20523524465526));
#105369=CARTESIAN_POINT('Ctrl Pts',(-1.38005116146527,2.7235645688885,7.2870572934719));
#105370=CARTESIAN_POINT('Ctrl Pts',(-1.3879742635373,2.71723347545156,7.32800582015948));
#105371=CARTESIAN_POINT('Ctrl Pts',(-1.39594531129452,2.71105259875875,
7.36894406871193));
#105372=CARTESIAN_POINT('',(-2.03504370448729,2.62129679787127,7.08633636636968));
#105373=CARTESIAN_POINT('Origin',(-1.04083408558608E-14,2.71213386200022,
7.84528692010511E-13));
#105374=CARTESIAN_POINT('',(-1.40311267351609,2.53084202107002,7.36758269877174));
#105375=CARTESIAN_POINT('Origin',(0.0396862191300584,2.55357152508889,-0.188904991491554));
#105376=CARTESIAN_POINT('',(-0.84053494974635,2.62129679635371,7.45275123627453));
#105377=CARTESIAN_POINT('Origin',(0.0537948407454188,2.41079129773833,-0.179803285552214));
#105378=CARTESIAN_POINT('Origin',(0.0105225792016134,2.55359538998345,-0.190305860738225));
#105379=CARTESIAN_POINT('Ctrl Pts',(-1.353363311,2.750764179,7.122563285));
#105380=CARTESIAN_POINT('Ctrl Pts',(-0.967419387,2.686419405,7.195896764));
#105381=CARTESIAN_POINT('Ctrl Pts',(-0.575811149000001,2.621296797,7.227097725));
#105382=CARTESIAN_POINT('Ctrl Pts',(-1.6409201,2.750764179,7.318290868));
#105383=CARTESIAN_POINT('Ctrl Pts',(-1.244370462,2.686419405,7.407205928));
#105384=CARTESIAN_POINT('Ctrl Pts',(-0.840534941,2.621296797,7.452751238));
#105385=CARTESIAN_POINT('',(-0.708173056919068,2.62129679507543,7.33992448035002));
#105386=CARTESIAN_POINT('Origin',(-4.32596666821716E-14,2.71213386200078,
-8.20090523268036E-13));
#105387=CARTESIAN_POINT('',(0.213503817067297,2.53084202106192,7.49696045860213));
#105388=CARTESIAN_POINT('',(-0.350157640963255,2.62129679727531,7.49182151570119));
#105389=CARTESIAN_POINT('Origin',(-0.00185061631064444,2.55357152007291,
-0.193019680036474));
#105390=CARTESIAN_POINT('Origin',(0.0138847566166005,2.41079128748424,-0.18716392002421));
#105391=CARTESIAN_POINT('Ctrl Pts',(-0.350157644662314,2.62129679564685,
7.49182151547269));
#105392=CARTESIAN_POINT('Ctrl Pts',(-0.228620255756217,2.64052352569912,
7.49750200929352));
#105393=CARTESIAN_POINT('Ctrl Pts',(-0.107205806305265,2.65962575012073,
7.500211122968));
#105394=CARTESIAN_POINT('Ctrl Pts',(0.013872358933994,2.67857142917026,
7.49998717083406));
#105395=CARTESIAN_POINT('Ctrl Pts',(0.0827547991821888,2.68934979367005,
7.49985976220329));
#105396=CARTESIAN_POINT('Ctrl Pts',(0.151742463241413,2.70017879538175,
7.49878302093725));
#105397=CARTESIAN_POINT('Ctrl Pts',(0.220796270213227,2.71105259965551,
7.49674922963173));
#105398=CARTESIAN_POINT('Ctrl Pts',(-0.593506707015565,2.61844384550212,
7.2253597183345));
#105399=CARTESIAN_POINT('Ctrl Pts',(-0.584808609650274,2.61987032125107,
7.2260531237281));
#105400=CARTESIAN_POINT('Ctrl Pts',(-0.576110512284988,2.621296797,7.22674652912171));
#105401=CARTESIAN_POINT('Ctrl Pts',(-0.400631185997974,2.65007516,7.24073560123764));
#105402=CARTESIAN_POINT('Ctrl Pts',(-0.224679703852224,2.678571429,7.24619125768236));
#105403=CARTESIAN_POINT('Ctrl Pts',(0.0032675322255622,2.71548868380392,
7.25325912441818));
#105404=CARTESIAN_POINT('Ctrl Pts',(0.231208307768356,2.75286255105096,
7.24598588434386));
#105405=CARTESIAN_POINT('Ctrl Pts',(-0.368191918198986,2.61844384550211,
7.4909786179583));
#105406=CARTESIAN_POINT('Ctrl Pts',(-0.359174777099492,2.61987032125107,
7.49140006697913));
#105407=CARTESIAN_POINT('Ctrl Pts',(-0.350157636,2.621296797,7.491821516));
#105408=CARTESIAN_POINT('Ctrl Pts',(-0.168241778,2.65007516,7.500324018));
#105409=CARTESIAN_POINT('Ctrl Pts',(0.013872358,2.678571429,7.499987171));
#105410=CARTESIAN_POINT('Ctrl Pts',(0.249803384602647,2.71548868380392,
7.49955078075478));
#105411=CARTESIAN_POINT('Ctrl Pts',(0.48524050162808,2.75286255105096,7.48428631606375));
#105412=CARTESIAN_POINT('',(-0.464112665399334,2.62129679787127,7.35813600120854));
#105413=CARTESIAN_POINT('Ctrl Pts',(-1.16100722477529,3.26861999521842,
7.40959699727959));
#105414=CARTESIAN_POINT('Ctrl Pts',(-1.15701056188764,3.26797796010921,
7.41021881713979));
#105415=CARTESIAN_POINT('Ctrl Pts',(-1.153013899,3.267335925,7.410840637));
#105416=CARTESIAN_POINT('Ctrl Pts',(-0.751738269,3.202873885,7.473273012));
#105417=CARTESIAN_POINT('Ctrl Pts',(-0.346067467,3.137747733,7.492011566));
#105418=CARTESIAN_POINT('Ctrl Pts',(-1.35660408902388,3.26861999521842,
7.12195103128405));
#105419=CARTESIAN_POINT('Ctrl Pts',(-1.35276243951194,3.26797796010921,
7.12267850364203));
#105420=CARTESIAN_POINT('Ctrl Pts',(-1.34892079,3.267335925,7.123405976));
#105421=CARTESIAN_POINT('Ctrl Pts',(-0.963208917,3.202873885,7.196446144));
#105422=CARTESIAN_POINT('Ctrl Pts',(-0.571865472,3.137747733,7.227411008));
#105423=CARTESIAN_POINT('',(-0.594693634847874,3.1776659463463,7.47638545564978));
#105424=CARTESIAN_POINT('Ctrl Pts',(-0.594693636545437,3.17766594630611,
7.47638545543473));
#105425=CARTESIAN_POINT('Ctrl Pts',(-0.591699897737181,3.17146450644349,
7.43478416571922));
#105426=CARTESIAN_POINT('Ctrl Pts',(-0.588689435224447,3.16510742592506,
7.39318254135156));
#105427=CARTESIAN_POINT('Ctrl Pts',(-0.582639747481574,3.15207191348099,
7.31008139669812));
#105428=CARTESIAN_POINT('Ctrl Pts',(-0.579596922089708,3.14538572802115,
7.2685323944097));
#105429=CARTESIAN_POINT('Ctrl Pts',(-0.576538527513735,3.13852541804481,
7.22703973443035));
#105430=CARTESIAN_POINT('',(-1.1530138984719,3.26733592582627,7.41084061853901));
#105431=CARTESIAN_POINT('Origin',(0.000867139836089673,3.08932518850483,
-0.18957817087375));
#105432=CARTESIAN_POINT('',(-1.25096733006107,3.2673359273533,7.26712330898553));
#105433=CARTESIAN_POINT('Ctrl Pts',(-2.428381113,3.13774478,7.095982326));
#105434=CARTESIAN_POINT('Ctrl Pts',(-2.198434563,3.176256335,7.174674441));
#105435=CARTESIAN_POINT('Ctrl Pts',(-1.963875725,3.214285714,7.238314178));
#105436=CARTESIAN_POINT('Ctrl Pts',(-1.80102675,3.240688665,7.282497829));
#105437=CARTESIAN_POINT('Ctrl Pts',(-1.63635545,3.267335925,7.319312867));
#105438=CARTESIAN_POINT('Ctrl Pts',(-1.63233139552941,3.26798710116569,
7.32021251203984));
#105439=CARTESIAN_POINT('Ctrl Pts',(-1.62830734105882,3.26863827733136,
7.32111215707968));
#105440=CARTESIAN_POINT('Ctrl Pts',(-2.121213834,3.13774478,6.932744901));
#105441=CARTESIAN_POINT('Ctrl Pts',(-1.896557022,3.176256335,7.001483207));
#105442=CARTESIAN_POINT('Ctrl Pts',(-1.667921256,3.214285714,7.055532488));
#105443=CARTESIAN_POINT('Ctrl Pts',(-1.509184538,3.240688665,7.093057699));
#105444=CARTESIAN_POINT('Ctrl Pts',(-1.34892079,3.267335925,7.123405976));
#105445=CARTESIAN_POINT('Ctrl Pts',(-1.34500444239351,3.26798710116569,
7.12414759351159));
#105446=CARTESIAN_POINT('Ctrl Pts',(-1.34108809478702,3.26863827733136,
7.12488921102319));
#105447=CARTESIAN_POINT('',(-1.63635545054765,3.26733592550877,7.31931286465442));
#105448=CARTESIAN_POINT('',(-1.49263812863747,3.26733592642396,7.22135941971466));
#105449=CARTESIAN_POINT('',(-2.18799190370241,3.17766594629541,7.17375016484504));
#105450=CARTESIAN_POINT('Ctrl Pts',(-1.636355450892,3.26733592483458,7.31931286668268));
#105451=CARTESIAN_POINT('Ctrl Pts',(-1.74635892260571,3.24953506265028,
7.29471974078576));
#105452=CARTESIAN_POINT('Ctrl Pts',(-1.85558425339799,3.23184317427157,
7.26769546538249));
#105453=CARTESIAN_POINT('Ctrl Pts',(-1.96387572495971,3.2142857139293,7.23831417758749));
#105454=CARTESIAN_POINT('Ctrl Pts',(-2.03878453707537,3.20214063496436,
7.21799016354287));
#105455=CARTESIAN_POINT('Ctrl Pts',(-2.1135088847609,3.18993125792355,7.19646746595664));
#105456=CARTESIAN_POINT('Ctrl Pts',(-2.18799190370039,3.1776659461067,7.17375016494029));
#105457=CARTESIAN_POINT('Ctrl Pts',(-2.11665929066702,3.1385254181032,6.93413682049357));
#105458=CARTESIAN_POINT('Ctrl Pts',(-2.12856581114192,3.1453856901219,6.97400172021665));
#105459=CARTESIAN_POINT('Ctrl Pts',(-2.14046922882565,3.15207183606137,
7.01392495842331));
#105460=CARTESIAN_POINT('Ctrl Pts',(-2.1642418900651,3.16510741554023,7.09378315124004));
#105461=CARTESIAN_POINT('Ctrl Pts',(-2.17612506755813,3.17146448527804,
7.13376491949633));
#105462=CARTESIAN_POINT('Ctrl Pts',(-2.18799190244371,3.17766594628736,
7.17375016518307));
#105463=CARTESIAN_POINT('Ctrl Pts',(-2.72670784948992,3.26861999521842,
6.98678250313633));
#105464=CARTESIAN_POINT('Ctrl Pts',(-2.72293829924496,3.26797796010921,
6.98824894956816));
#105465=CARTESIAN_POINT('Ctrl Pts',(-2.719168749,3.267335925,6.989715396));
#105466=CARTESIAN_POINT('Ctrl Pts',(-2.340695835,3.202873885,7.136950535));
#105467=CARTESIAN_POINT('Ctrl Pts',(-1.948537627,3.137747733,7.242458223));
#105468=CARTESIAN_POINT('Ctrl Pts',(-2.85589638766259,3.26861999521842,
6.6638139959214));
#105469=CARTESIAN_POINT('Ctrl Pts',(-2.85230093883129,3.26797796010921,
6.66535030146071));
#105470=CARTESIAN_POINT('Ctrl Pts',(-2.84870549,3.267335925,6.666886607));
#105471=CARTESIAN_POINT('Ctrl Pts',(-2.487712823,3.202873885,6.821135787));
#105472=CARTESIAN_POINT('Ctrl Pts',(-2.112175301,3.137747733,6.935503983));
#105473=CARTESIAN_POINT('',(-2.71916874452873,3.26733592582611,6.9897153780778));
#105474=CARTESIAN_POINT('Origin',(0.0416006174824163,3.08932515708654,-0.184959702196723));
#105475=CARTESIAN_POINT('',(-2.78393710593565,3.26733592735283,6.82830100703027));
#105476=CARTESIAN_POINT('Origin',(-5.48606299277665E-14,3.35806380000056,
2.30284541435921E-13));
#105477=CARTESIAN_POINT('',(-2.18598964806097,3.35698786818065,7.17436054673024));
#105478=CARTESIAN_POINT('Origin',(0.0119076089957454,3.08947598352193,-0.182881204940006));
#105479=CARTESIAN_POINT('Origin',(0.0351660334599163,3.48205906984505,-0.184035505550071));
#105480=CARTESIAN_POINT('Ctrl Pts',(-3.897033357,3.13774478,6.40805204500001));
#105481=CARTESIAN_POINT('Ctrl Pts',(-3.689379308,3.176256335,6.534336094));
#105482=CARTESIAN_POINT('Ctrl Pts',(-3.473984987,3.214285714,6.646911186));
#105483=CARTESIAN_POINT('Ctrl Pts',(-3.324441509,3.240688665,6.725069564));
#105484=CARTESIAN_POINT('Ctrl Pts',(-3.171534278,3.267335925,6.79642334800001));
#105485=CARTESIAN_POINT('Ctrl Pts',(-3.16779770079139,3.26798710116568,
6.7981670125821));
#105486=CARTESIAN_POINT('Ctrl Pts',(-3.16406112358279,3.26863827733137,
6.79991067716421));
#105487=CARTESIAN_POINT('Ctrl Pts',(-3.561956257,3.13774478,6.314662906));
#105488=CARTESIAN_POINT('Ctrl Pts',(-3.3573285,3.176256335,6.43008872300001));
#105489=CARTESIAN_POINT('Ctrl Pts',(-3.145657109,3.214285714,6.532024292));
#105490=CARTESIAN_POINT('Ctrl Pts',(-2.998698378,3.240688665,6.602795887));
#105491=CARTESIAN_POINT('Ctrl Pts',(-2.84870549,3.267335925,6.666886607));
#105492=CARTESIAN_POINT('Ctrl Pts',(-2.84504013027117,3.26798710116568,
6.66845278488491));
#105493=CARTESIAN_POINT('Ctrl Pts',(-2.84137477054235,3.26863827733137,
6.67001896276982));
#105494=CARTESIAN_POINT('',(-3.17153427803867,3.26733592550877,6.79642334559096));
#105495=CARTESIAN_POINT('',(-3.01011989205177,3.26733592642396,6.73165497389958));
#105496=CARTESIAN_POINT('',(-3.67898209978803,3.17766594630002,6.53567828967424));
#105497=CARTESIAN_POINT('Ctrl Pts',(-3.17153427880971,3.26733592483345,
6.79642334749546));
#105498=CARTESIAN_POINT('Ctrl Pts',(-3.27367913498392,3.24953506265028,
6.74875770096114));
#105499=CARTESIAN_POINT('Ctrl Pts',(-3.37454141781148,3.23184317427167,
6.6988850207741));
#105500=CARTESIAN_POINT('Ctrl Pts',(-3.47398498685941,3.21428571394846,
6.64691118569608));
#105501=CARTESIAN_POINT('Ctrl Pts',(-3.54277341033584,3.20214063502602,
6.61095915563011));
#105502=CARTESIAN_POINT('Ctrl Pts',(-3.6111240004649,3.18993125796488,6.57387612060236));
#105503=CARTESIAN_POINT('Ctrl Pts',(-3.6789820999354,3.17766594614085,6.53567828998717));
#105504=CARTESIAN_POINT('Ctrl Pts',(-3.55780741732562,3.13852541817353,
6.31700137554185));
#105505=CARTESIAN_POINT('Ctrl Pts',(-3.57800534213567,3.14538568922323,
6.35337470099805));
#105506=CARTESIAN_POINT('Ctrl Pts',(-3.59821277736713,3.1520718341465,6.38980566719298));
#105507=CARTESIAN_POINT('Ctrl Pts',(-3.63859680666803,3.16510741642552,
6.46268641610141));
#105508=CARTESIAN_POINT('Ctrl Pts',(-3.65879706345997,3.17146448703467,
6.49917890637104));
#105509=CARTESIAN_POINT('Ctrl Pts',(-3.67898209852761,3.17766594627311,
6.53567829018584));
#105510=CARTESIAN_POINT('Ctrl Pts',(-4.16491064522116,3.26861999521842,
6.23727382379452));
#105511=CARTESIAN_POINT('Ctrl Pts',(-4.16154446761058,3.26797796010921,
6.23951632739726));
#105512=CARTESIAN_POINT('Ctrl Pts',(-4.15817829,3.267335925,6.241758831));
#105513=CARTESIAN_POINT('Ctrl Pts',(-3.820205066,3.202873885,6.466912183));
#105514=CARTESIAN_POINT('Ctrl Pts',(-3.459896332,3.137747733,6.654255583));
#105515=CARTESIAN_POINT('Ctrl Pts',(-4.2216501449166,3.26861999521842,5.8940844244334));
#105516=CARTESIAN_POINT('Ctrl Pts',(-4.2184690159583,3.26797796010921,5.89635772721671));
#105517=CARTESIAN_POINT('Ctrl Pts',(-4.215287887,3.267335925,5.89863103000001));
#105518=CARTESIAN_POINT('Ctrl Pts',(-3.895894042,3.202873885,6.126876702));
#105519=CARTESIAN_POINT('Ctrl Pts',(-3.55372216,3.137747733,6.3193005));
#105520=CARTESIAN_POINT('',(-4.15817828176499,3.26733592582611,6.24175881447829));
#105521=CARTESIAN_POINT('Origin',(0.0803888520133322,3.08932521734779,-0.171692463230565));
#105522=CARTESIAN_POINT('',(-4.18673307644162,3.26733592735283,6.07019493881691));
#105523=CARTESIAN_POINT('Origin',(-3.03576608295941E-14,3.35806380000022,
6.24500451351651E-14));
#105524=CARTESIAN_POINT('',(-3.67715786962144,3.35698786820061,6.53670482762012));
#105525=CARTESIAN_POINT('Origin',(0.050943447341012,3.08947602065486,-0.17604612105504));
#105526=CARTESIAN_POINT('Origin',(0.0739062462862405,3.48205903813151,-0.172173467210209));
#105527=CARTESIAN_POINT('Ctrl Pts',(-5.183464652,3.13774478,5.42048837300001));
#105528=CARTESIAN_POINT('Ctrl Pts',(-5.007812776,3.176256335,5.588459453));
#105529=CARTESIAN_POINT('Ctrl Pts',(-4.821654572,3.214285714,5.744706014));
#105530=CARTESIAN_POINT('Ctrl Pts',(-4.692409079,3.240688665,5.85318452000001));
#105531=CARTESIAN_POINT('Ctrl Pts',(-4.55841568800001,3.267335925,5.955740627));
#105532=CARTESIAN_POINT('Ctrl Pts',(-4.55514130622198,3.26798710116568,
5.95824677932199));
#105533=CARTESIAN_POINT('Ctrl Pts',(-4.55186692444395,3.26863827733137,
5.96075293164398));
#105534=CARTESIAN_POINT('Ctrl Pts',(-4.836145564,3.13774478,5.401314292));
#105535=CARTESIAN_POINT('Ctrl Pts',(-4.661115028,3.176256335,5.558030436));
#105536=CARTESIAN_POINT('Ctrl Pts',(-4.476305531,3.214285714,5.703085901));
#105537=CARTESIAN_POINT('Ctrl Pts',(-4.347996415,3.240688665,5.803794678));
#105538=CARTESIAN_POINT('Ctrl Pts',(-4.215287887,3.267335925,5.89863103));
#105539=CARTESIAN_POINT('Ctrl Pts',(-4.21204490327798,3.26798710116568,
5.900948535517));
#105540=CARTESIAN_POINT('Ctrl Pts',(-4.20880191955596,3.26863827733137,
5.90326604103398));
#105541=CARTESIAN_POINT('',(-4.55841568752333,3.26733592550877,5.95574062463764));
#105542=CARTESIAN_POINT('',(-4.38685179458955,3.26733592642396,5.92718582325287));
#105543=CARTESIAN_POINT('',(-4.99794718194148,3.17766594632365,5.59200536169395));
#105544=CARTESIAN_POINT('Ctrl Pts',(-4.55841568868483,3.26733592483286,
5.9557406263308));
#105545=CARTESIAN_POINT('Ctrl Pts',(-4.64792575016103,3.24953506265028,
5.88723125139043));
#105546=CARTESIAN_POINT('Ctrl Pts',(-4.73570877677773,3.23184317427168,
5.81684215734397));
#105547=CARTESIAN_POINT('Ctrl Pts',(-4.8216545719038,3.21428571395066,5.74470601375657));
#105548=CARTESIAN_POINT('Ctrl Pts',(-4.88110613673947,3.20214063497804,
5.69480704427308));
#105549=CARTESIAN_POINT('Ctrl Pts',(-4.93988697182446,3.18993125790122,
5.64389763349253));
#105550=CARTESIAN_POINT('Ctrl Pts',(-4.99794718179529,3.17766594611035,
5.59200536158081));
#105551=CARTESIAN_POINT('Ctrl Pts',(-4.83259642346465,3.13852541816698,
5.40448996726233));
#105552=CARTESIAN_POINT('Ctrl Pts',(-4.86014133022803,3.14538569126172,
5.4356709569915));
#105553=CARTESIAN_POINT('Ctrl Pts',(-4.88770791728529,3.15207183832862,
5.46690619692211));
#105554=CARTESIAN_POINT('Ctrl Pts',(-4.94281497972511,3.16510741648527,
5.52940164199938));
#105555=CARTESIAN_POINT('Ctrl Pts',(-4.97038777257657,3.17146448713464,
5.56069850019475));
#105556=CARTESIAN_POINT('Ctrl Pts',(-4.99794718103561,3.17766594632074,
5.59200536249196));
#105557=CARTESIAN_POINT('Ctrl Pts',(-5.40836684853112,3.26861999521842,
5.19611715339498));
#105558=CARTESIAN_POINT('Ctrl Pts',(-5.40556144226556,3.26797796010921,
5.19903085719749));
#105559=CARTESIAN_POINT('Ctrl Pts',(-5.402756036,3.267335925,5.201944561));
#105560=CARTESIAN_POINT('Ctrl Pts',(-5.121085753,3.202873885,5.49448820600001));
#105561=CARTESIAN_POINT('Ctrl Pts',(-4.809474131,3.137747733,5.754907348));
#105562=CARTESIAN_POINT('Ctrl Pts',(-5.39000423404587,3.26861999521842,
4.84875401616961));
#105563=CARTESIAN_POINT('Ctrl Pts',(-5.38738617102293,3.26797796010921,
4.8516580190848));
#105564=CARTESIAN_POINT('Ctrl Pts',(-5.384768108,3.267335925,4.854562022));
#105565=CARTESIAN_POINT('Ctrl Pts',(-5.121907587,3.202873885,5.146131672));
#105566=CARTESIAN_POINT('Ctrl Pts',(-4.829100921,3.137747733,5.407613549));
#105567=CARTESIAN_POINT('',(-5.40275602441283,3.26733592582611,5.20194454661871));
#105568=CARTESIAN_POINT('Origin',(0.1154182138976,3.08932517228882,-0.150397172527648));
#105569=CARTESIAN_POINT('',(-5.39376206201143,3.26733592735283,5.02825330221466));
#105570=CARTESIAN_POINT('Origin',(3.30898503042576E-13,3.35806380000056,
-3.24826970876657E-13));
#105571=CARTESIAN_POINT('',(-4.99638627664651,3.35698786819216,5.5934000550976));
#105572=CARTESIAN_POINT('Origin',(0.0875969833521245,3.08947602033563,-0.160978744650947));
#105573=CARTESIAN_POINT('Origin',(0.109190386965071,3.48205905117618,-0.152260312179363));
#105574=CARTESIAN_POINT('Ctrl Pts',(-6.2275229,3.13774478,4.17946869));
#105575=CARTESIAN_POINT('Ctrl Pts',(-6.092086485,3.176256335,4.38127266));
#105576=CARTESIAN_POINT('Ctrl Pts',(-5.943868948,3.214285714,4.573884774));
#105577=CARTESIAN_POINT('Ctrl Pts',(-5.840964815,3.240688665,4.707611073));
#105578=CARTESIAN_POINT('Ctrl Pts',(-5.732150647,3.267335925,4.836574093));
#105579=CARTESIAN_POINT('Ctrl Pts',(-5.72949156712874,3.26798710116569,
4.83972554815443));
#105580=CARTESIAN_POINT('Ctrl Pts',(-5.72683248725748,3.26863827733136,
4.84287700330887));
#105581=CARTESIAN_POINT('Ctrl Pts',(-5.884202079,3.13774478,4.235406225));
#105582=CARTESIAN_POINT('Ctrl Pts',(-5.746952999,3.176256335,4.426084824));
#105583=CARTESIAN_POINT('Ctrl Pts',(-5.597646882,3.214285714,4.607477551));
#105584=CARTESIAN_POINT('Ctrl Pts',(-5.493986972,3.240688665,4.73341448));
#105585=CARTESIAN_POINT('Ctrl Pts',(-5.384768108,3.267335925,4.854562022));
#105586=CARTESIAN_POINT('Ctrl Pts',(-5.38209913861705,3.26798710116569,
4.857522491177));
#105587=CARTESIAN_POINT('Ctrl Pts',(-5.37943016923408,3.26863827733136,
4.860482960354));
#105588=CARTESIAN_POINT('',(-5.73215064603959,3.26733592550878,4.83657409078814));
#105589=CARTESIAN_POINT('',(-5.55845938329581,3.26733592642396,4.84556805085149));
#105590=CARTESIAN_POINT('',(-6.08321380816663,3.17766594627907,4.38685647820771));
#105591=CARTESIAN_POINT('Ctrl Pts',(-5.73215064753397,3.26733592483077,
4.83657409218913));
#105592=CARTESIAN_POINT('Ctrl Pts',(-5.80484052267461,3.24953506265028,
4.75042441136096));
#105593=CARTESIAN_POINT('Ctrl Pts',(-5.87543965620554,3.23184317427165,
4.6628102196089));
#105594=CARTESIAN_POINT('Ctrl Pts',(-5.94386894792444,3.21428571394464,
4.5738847737479));
#105595=CARTESIAN_POINT('Ctrl Pts',(-5.99120376486707,3.20214063498633,
4.51237208554023));
#105596=CARTESIAN_POINT('Ctrl Pts',(-6.03766631805085,3.18993125791425,
4.45001676666744));
#105597=CARTESIAN_POINT('Ctrl Pts',(-6.08321380823861,3.17766594609085,
4.38685647829616));
#105598=CARTESIAN_POINT('Ctrl Pts',(-5.88141859146557,3.138525418069,4.23927061465614));
#105599=CARTESIAN_POINT('Ctrl Pts',(-5.91502250643536,3.14538569154247,
4.26380127091827));
#105600=CARTESIAN_POINT('Ctrl Pts',(-5.94865925736818,3.1520718390077,4.28838024855296));
#105601=CARTESIAN_POINT('Ctrl Pts',(-6.01591261206742,3.16510741550992,
4.33756818912958));
#105602=CARTESIAN_POINT('Ctrl Pts',(-6.04956866250469,3.17146448523722,
4.36220600486341));
#105603=CARTESIAN_POINT('Ctrl Pts',(-6.08321380735238,3.17766594626958,
4.3868564792451));
#105604=CARTESIAN_POINT('Ctrl Pts',(-6.39893382949064,3.26861999521842,
3.91199581910429));
#105605=CARTESIAN_POINT('Ctrl Pts',(-6.39682037224532,3.26797796010921,
3.91544448155214));
#105606=CARTESIAN_POINT('Ctrl Pts',(-6.394706915,3.267335925,3.918893144));
#105607=CARTESIAN_POINT('Ctrl Pts',(-6.182510162,3.202873885,4.265148066));
#105608=CARTESIAN_POINT('Ctrl Pts',(-5.934166264,3.137747733,4.586466041));
#105609=CARTESIAN_POINT('Ctrl Pts',(-6.30632771577689,3.26861999521842,
3.5767012587878));
#105610=CARTESIAN_POINT('Ctrl Pts',(-6.30439513638845,3.26797796010921,
3.5801001738939));
#105611=CARTESIAN_POINT('Ctrl Pts',(-6.302462557,3.267335925,3.583499089));
#105612=CARTESIAN_POINT('Ctrl Pts',(-6.108426424,3.202873885,3.924759245));
#105613=CARTESIAN_POINT('Ctrl Pts',(-5.87867629,3.137747733,4.243072598));
#105614=CARTESIAN_POINT('',(-6.39470690059427,3.26733592582611,3.91889313243628));
#105615=CARTESIAN_POINT('Origin',(0.145050850507895,3.08932516225572,-0.122069546710017));
#105616=CARTESIAN_POINT('',(-6.34858472854829,3.26733592735283,3.7511961291114));
#105617=CARTESIAN_POINT('Origin',(6.59194920871187E-14,3.35806379999989,
-5.20417042793042E-14));
#105618=CARTESIAN_POINT('',(-6.08198921396976,3.35698786820903,4.38855411234819));
#105619=CARTESIAN_POINT('Origin',(0.120154476295529,3.08947602866354,-0.138384219053677));
#105620=CARTESIAN_POINT('Origin',(0.139369057992483,3.48205902309301,-0.12522785802636));
#105621=CARTESIAN_POINT('Ctrl Pts',(-6.9803891,3.13774478,2.743021695));
#105622=CARTESIAN_POINT('Ctrl Pts',(-6.891501001,3.176256335,2.969222426));
#105623=CARTESIAN_POINT('Ctrl Pts',(-6.788154619,3.214285714,3.189193765));
#105624=CARTESIAN_POINT('Ctrl Pts',(-6.716403528,3.240688665,3.341914965));
#105625=CARTESIAN_POINT('Ctrl Pts',(-6.63785661200001,3.267335925,3.491254731));
#105626=CARTESIAN_POINT('Ctrl Pts',(-6.63593716964131,3.26798710116568,
3.49490413045825));
#105627=CARTESIAN_POINT('Ctrl Pts',(-6.63401772728262,3.26863827733137,
3.4985535299165));
#105628=CARTESIAN_POINT('Ctrl Pts',(-6.657119845,3.13774478,2.87145527));
#105629=CARTESIAN_POINT('Ctrl Pts',(-6.564069834,3.176256335,3.087180404));
#105630=CARTESIAN_POINT('Ctrl Pts',(-6.457248486,3.214285714,3.296428672));
#105631=CARTESIAN_POINT('Ctrl Pts',(-6.383084804,3.240688665,3.441705082));
#105632=CARTESIAN_POINT('Ctrl Pts',(-6.30246255700001,3.267335925,3.583499089));
#105633=CARTESIAN_POINT('Ctrl Pts',(-6.30049240000562,3.26798710116568,
3.58696409357439));
#105634=CARTESIAN_POINT('Ctrl Pts',(-6.29852224301123,3.26863827733137,
3.59042909814879));
#105635=CARTESIAN_POINT('',(-6.63785661058304,3.26733592550878,3.4912547290495));
#105636=CARTESIAN_POINT('',(-6.47015958873108,3.26733592642396,3.53737690226101));
#105637=CARTESIAN_POINT('',(-6.88403611863456,3.17766594631347,2.97658306108282));
#105638=CARTESIAN_POINT('Ctrl Pts',(-6.63785661234512,3.26733592483146,
3.49125473009715));
#105639=CARTESIAN_POINT('Ctrl Pts',(-6.69032740376243,3.24953506265028,
3.39149300637368));
#105640=CARTESIAN_POINT('Ctrl Pts',(-6.74044150766843,3.23184317427177,
3.29075045860683));
#105641=CARTESIAN_POINT('Ctrl Pts',(-6.78815461857239,3.21428571396706,
3.18919376497703));
#105642=CARTESIAN_POINT('Ctrl Pts',(-6.82115936383275,3.20214063501202,
3.1189436228721));
#105643=CARTESIAN_POINT('Ctrl Pts',(-6.853131098539,3.18993125790658,3.0480580608225));
#105644=CARTESIAN_POINT('Ctrl Pts',(-6.88403611852835,3.17766594610698,
2.97658306107234));
#105645=CARTESIAN_POINT('Ctrl Pts',(-6.65523216405864,3.13852541811756,
2.87582767986541));
#105646=CARTESIAN_POINT('Ctrl Pts',(-6.69332378757033,3.14538568860475,
2.89256096718071));
#105647=CARTESIAN_POINT('Ctrl Pts',(-6.73145786445602,3.15207183294835,
2.90933438629054));
#105648=CARTESIAN_POINT('Ctrl Pts',(-6.80771286730689,3.16510741645553,
2.94291487484572));
#105649=CARTESIAN_POINT('Ctrl Pts',(-6.84587846600961,3.1714644871039,2.9597416187823));
#105650=CARTESIAN_POINT('Ctrl Pts',(-6.88403611813504,3.17766594631055,
2.97658306221566));
#105651=CARTESIAN_POINT('Ctrl Pts',(-7.0902937755932,3.26861999521842,2.44495390907349));
#105652=CARTESIAN_POINT('Ctrl Pts',(-7.0889710902966,3.26797796010921,2.44877627453674));
#105653=CARTESIAN_POINT('Ctrl Pts',(-7.08764840500001,3.267335925,2.45259864));
#105654=CARTESIAN_POINT('Ctrl Pts',(-6.95484726800001,3.202873885,2.836374343));
#105655=CARTESIAN_POINT('Ctrl Pts',(-6.781383379,3.137747733,3.20356668));
#105656=CARTESIAN_POINT('Ctrl Pts',(-6.92777432193795,3.26861999521842,
2.13740592539923));
#105657=CARTESIAN_POINT('Ctrl Pts',(-6.92661759146898,3.26797796010921,
2.14114082319961));
#105658=CARTESIAN_POINT('Ctrl Pts',(-6.925460861,3.267335925,2.144875721));
#105659=CARTESIAN_POINT('Ctrl Pts',(-6.809322032,3.202873885,2.519869437));
#105660=CARTESIAN_POINT('Ctrl Pts',(-6.65337129,3.137747733,2.880130289));
#105661=CARTESIAN_POINT('',(-7.08764838844522,3.26733592582611,2.45259863180721));
#105662=CARTESIAN_POINT('Origin',(0.16790095296493,3.08932520347122,-0.0880339539605168));
#105663=CARTESIAN_POINT('',(-7.0065546284336,3.26733592735283,2.29873719441841));
#105664=CARTESIAN_POINT('Origin',(-4.16333634234434E-14,3.35806379999989,
4.74880551548651E-14));
#105665=CARTESIAN_POINT('',(-6.8832050954752,3.35698786817884,2.97850425767523));
#105666=CARTESIAN_POINT('Origin',(0.147094092923507,3.08947605737589,-0.109319328977385));
#105667=CARTESIAN_POINT('Origin',(0.163031056593049,3.48205907567582,-0.0923399100765862));
#105668=CARTESIAN_POINT('Ctrl Pts',(-7.406860063,3.13774478,1.178314054));
#105669=CARTESIAN_POINT('Ctrl Pts',(-7.368676589,3.176256335,1.418334652));
#105670=CARTESIAN_POINT('Ctrl Pts',(-7.315033724,3.214285714,1.655379601));
#105671=CARTESIAN_POINT('Ctrl Pts',(-7.277790677,3.240688665,1.819954627));
#105672=CARTESIAN_POINT('Ctrl Pts',(-7.23318378,3.267335925,1.982688177));
#105673=CARTESIAN_POINT('Ctrl Pts',(-7.23209372615764,3.26798710116569,
1.98666487888668));
#105674=CARTESIAN_POINT('Ctrl Pts',(-7.23100367231527,3.26863827733136,
1.99064158077337));
#105675=CARTESIAN_POINT('Ctrl Pts',(-7.118758086,3.13774478,1.373238257));
#105676=CARTESIAN_POINT('Ctrl Pts',(-7.07425806000001,3.176256335,1.60392286));
#105677=CARTESIAN_POINT('Ctrl Pts',(-7.014916327,3.214285714,1.831242452));
#105678=CARTESIAN_POINT('Ctrl Pts',(-6.973716685,3.240688665,1.98906538));
#105679=CARTESIAN_POINT('Ctrl Pts',(-6.925460861,3.267335925,2.144875721));
#105680=CARTESIAN_POINT('Ctrl Pts',(-6.92428163872934,3.26798710116569,
2.1486832411888));
#105681=CARTESIAN_POINT('Ctrl Pts',(-6.92310241645868,3.26863827733136,
2.15249076137759));
#105682=CARTESIAN_POINT('',(-7.23318377818696,3.26733592550877,1.9826881754134));
#105683=CARTESIAN_POINT('',(-7.07932232296849,3.26733592642396,2.06378194053243));
#105684=CARTESIAN_POINT('',(-7.36296855048892,3.17766594632392,1.42712792863381));
#105685=CARTESIAN_POINT('Ctrl Pts',(-7.23318378013855,3.26733592483385,
1.98268817605887));
#105686=CARTESIAN_POINT('Ctrl Pts',(-7.2629820116059,3.24953506265028,1.87397915710101));
#105687=CARTESIAN_POINT('Ctrl Pts',(-7.29026780568012,3.23184317427141,
1.76481886353824));
#105688=CARTESIAN_POINT('Ctrl Pts',(-7.31503372343932,3.21428571389762,
1.65537960077499));
#105689=CARTESIAN_POINT('Ctrl Pts',(-7.33216513187329,3.20214063490214,
1.57967682304382));
#105690=CARTESIAN_POINT('Ctrl Pts',(-7.34815108484028,3.18993125791942,
1.50357554853497));
#105691=CARTESIAN_POINT('Ctrl Pts',(-7.36296855041346,3.1776659461216,1.42712792865164));
#105692=CARTESIAN_POINT('Ctrl Pts',(-7.11785447610388,3.13852541812603,
1.37791423853735));
#105693=CARTESIAN_POINT('Ctrl Pts',(-7.1586527173248,3.14538569137985,1.38606774128126));
#105694=CARTESIAN_POINT('Ctrl Pts',(-7.19950104905351,3.15207183861513,
1.39425131180269));
#105695=CARTESIAN_POINT('Ctrl Pts',(-7.281192024112,3.16510741562126,1.41065412762892));
#105696=CARTESIAN_POINT('Ctrl Pts',(-7.32208257888771,3.1714644853935,1.41888299491582));
#105697=CARTESIAN_POINT('Ctrl Pts',(-7.3629685502442,3.17766594632102,1.42712792984957));
#105698=CARTESIAN_POINT('Ctrl Pts',(-7.45011946511826,3.26861999521842,
0.86358867113768));
#105699=CARTESIAN_POINT('Ctrl Pts',(-7.44964939905913,3.26797796010921,
0.867606010068841));
#105700=CARTESIAN_POINT('Ctrl Pts',(-7.449179333,3.267335925,0.871623349000001));
#105701=CARTESIAN_POINT('Ctrl Pts',(-7.401983445,3.202873885,1.274974909));
#105702=CARTESIAN_POINT('Ctrl Pts',(-7.311510543,3.137747733,1.670872101));
#105703=CARTESIAN_POINT('Ctrl Pts',(-7.22528590126796,3.26861999521842,
0.598167867343195));
#105704=CARTESIAN_POINT('Ctrl Pts',(-7.22495910713398,3.26797796010921,
0.602064108171597));
#105705=CARTESIAN_POINT('Ctrl Pts',(-7.224632313,3.267335925,0.605960349000001));
#105706=CARTESIAN_POINT('Ctrl Pts',(-7.191821309,3.202873885,0.997153336));
#105707=CARTESIAN_POINT('Ctrl Pts',(-7.116962042,3.137747733,1.382516288));
#105708=CARTESIAN_POINT('',(-7.44917931507457,3.2673359258261,0.871623344572886));
#105709=CARTESIAN_POINT('Origin',(0.182900004317507,3.08932517287314,-0.0498819972482253));
#105710=CARTESIAN_POINT('',(-7.3369058215324,3.26733592735283,0.738791863574644));
#105711=CARTESIAN_POINT('Origin',(1.23468943402649E-12,3.35806380000078,
-2.36193443275967E-13));
#105712=CARTESIAN_POINT('',(-7.36256995659096,3.35698786820896,1.42918285405513));
#105713=CARTESIAN_POINT('Origin',(0.167155057817885,3.08947599877084,-0.0751425101531752));
#105714=CARTESIAN_POINT('Origin',(0.179069849303855,3.48205904621345,-0.0551341927314677));
#105715=CARTESIAN_POINT('Ctrl Pts',(-7.48699448200001,3.13774478,-0.441490242));
#105716=CARTESIAN_POINT('Ctrl Pts',(-7.50130105,3.176256335,-0.198872874));
#105717=CARTESIAN_POINT('Ctrl Pts',(-7.499869982,3.214285714,0.044161726));
#105718=CARTESIAN_POINT('Ctrl Pts',(-7.498876423,3.240688665,0.212895234));
#105719=CARTESIAN_POINT('Ctrl Pts',(-7.490295313,3.267335925,0.381413328));
#105720=CARTESIAN_POINT('Ctrl Pts',(-7.49008561735748,3.26798710116569,
0.385531386153037));
#105721=CARTESIAN_POINT('Ctrl Pts',(-7.48987592171496,3.26863827733136,
0.389649444306074));
#105722=CARTESIAN_POINT('Ctrl Pts',(-7.247531111,3.13774478,-0.189189849));
#105723=CARTESIAN_POINT('Ctrl Pts',(-7.253661841,3.176256335,0.045667665));
#105724=CARTESIAN_POINT('Ctrl Pts',(-7.244574478,3.214285714,0.28042937));
#105725=CARTESIAN_POINT('Ctrl Pts',(-7.238265325,3.240688665,0.443419191));
#105726=CARTESIAN_POINT('Ctrl Pts',(-7.224632313,3.267335925,0.605960349000001));
#105727=CARTESIAN_POINT('Ctrl Pts',(-7.22429916458321,3.26798710116569,
0.609932349424512));
#105728=CARTESIAN_POINT('Ctrl Pts',(-7.22396601616642,3.26863827733136,
0.613904349849024));
#105729=CARTESIAN_POINT('',(-7.49029531088823,3.26733592550878,0.381413326840878));
#105730=CARTESIAN_POINT('',(-7.3574638135905,3.26733592642396,0.493686829699741));
#105731=CARTESIAN_POINT('',(-7.4976167564852,3.17766594630478,-0.189058119747558));
#105732=CARTESIAN_POINT('Ctrl Pts',(-7.4902953129333,3.26733592483399,0.381413327051709));
#105733=CARTESIAN_POINT('Ctrl Pts',(-7.49602765287763,3.24953506265028,
0.268840125822009));
#105734=CARTESIAN_POINT('Ctrl Pts',(-7.49920928384314,3.23184317427167,
0.156366300058196));
#105735=CARTESIAN_POINT('Ctrl Pts',(-7.49986998160241,3.21428571394786,
0.044161726036576));
#105736=CARTESIAN_POINT('Ctrl Pts',(-7.50032700804195,3.20214063500503,
-0.0334539089873134));
#105737=CARTESIAN_POINT('Ctrl Pts',(-7.49957969348547,3.18993125793839,
-0.111212485413614));
#105738=CARTESIAN_POINT('Ctrl Pts',(-7.49761675662906,3.17766594612312,
-0.189058119722564));
#105739=CARTESIAN_POINT('Ctrl Pts',(-7.24765382489753,3.13852541804203,
-0.184428940551483));
#105740=CARTESIAN_POINT('Ctrl Pts',(-7.28925098650911,3.14538569110661,
-0.185236478160081));
#105741=CARTESIAN_POINT('Ctrl Pts',(-7.33090353108689,3.15207183813376,
-0.186025418823179));
#105742=CARTESIAN_POINT('Ctrl Pts',(-7.41421074489788,3.1651074164085,-0.1875672367013));
#105743=CARTESIAN_POINT('Ctrl Pts',(-7.45591427041447,3.17146448703968,
-0.188321016362887));
#105744=CARTESIAN_POINT('Ctrl Pts',(-7.4976167564466,3.17766594629268,-0.189058118439964));
#105745=CARTESIAN_POINT('Ctrl Pts',(-7.46158584913562,3.26861999521842,
-0.758157013164344));
#105746=CARTESIAN_POINT('Ctrl Pts',(-7.46199038206781,3.26797796010921,
-0.754132547082172));
#105747=CARTESIAN_POINT('Ctrl Pts',(-7.462394915,3.267335925,-0.750108081));
#105748=CARTESIAN_POINT('Ctrl Pts',(-7.503011102,3.202873885,-0.346040936));
#105749=CARTESIAN_POINT('Ctrl Pts',(-7.499759601,3.137747733,0.0600494));
#105750=CARTESIAN_POINT('Ctrl Pts',(-7.18495114151865,3.26861999521842,
-0.969039855917186));
#105751=CARTESIAN_POINT('Ctrl Pts',(-7.18546956425932,3.26797796010921,
-0.965164455958594));
#105752=CARTESIAN_POINT('Ctrl Pts',(-7.18598798700001,3.267335925,-0.961289056));
#105753=CARTESIAN_POINT('Ctrl Pts',(-7.238039015,3.202873885,-0.572188548));
#105754=CARTESIAN_POINT('Ctrl Pts',(-7.24777156,3.137747733,-0.179742638));
#105755=CARTESIAN_POINT('',(-7.46239489653727,3.2673359258261,-0.750108081480122));
#105756=CARTESIAN_POINT('Origin',(0.189347432826993,3.08932519891378,-0.00939766698610588));
#105757=CARTESIAN_POINT('',(-7.32419145269983,3.26733592735283,-0.855698553950613));
#105758=CARTESIAN_POINT('Origin',(-7.41160605111091E-13,3.35806379999989,
2.81350463759988E-14));
#105759=CARTESIAN_POINT('',(-7.49766922987128,3.35698786824895,-0.186965551550327));
#105760=CARTESIAN_POINT('Origin',(0.179400584072857,3.08947606338236,-0.0374523169333984));
#105761=CARTESIAN_POINT('Origin',(0.186735398645302,3.48205900677173,-0.0153504641044341));
#105762=CARTESIAN_POINT('Ctrl Pts',(-7.21704536000001,3.13774478,-2.040650945));
#105763=CARTESIAN_POINT('Ctrl Pts',(-7.283173011,3.176256335,-1.806781326));
#105764=CARTESIAN_POINT('Ctrl Pts',(-7.334020655,3.214285714,-1.569121102));
#105765=CARTESIAN_POINT('Ctrl Pts',(-7.36932304100001,3.240688665,-1.404118904));
#105766=CARTESIAN_POINT('Ctrl Pts',(-7.397168962,3.267335925,-1.237695984));
#105767=CARTESIAN_POINT('Ctrl Pts',(-7.39784942971288,3.26798710116569,
-1.23362912538387));
#105768=CARTESIAN_POINT('Ctrl Pts',(-7.39852989742575,3.26863827733136,
-1.22956226676773));
#105769=CARTESIAN_POINT('Ctrl Pts',(-7.037417636,3.13774478,-1.742771649));
#105770=CARTESIAN_POINT('Ctrl Pts',(-7.09389245600001,3.176256335,-1.514722898));
#105771=CARTESIAN_POINT('Ctrl Pts',(-7.135484378,3.214285714,-1.283496277));
#105772=CARTESIAN_POINT('Ctrl Pts',(-7.164360722,3.240688665,-1.122960787));
#105773=CARTESIAN_POINT('Ctrl Pts',(-7.185987987,3.267335925,-0.961289056000001));
#105774=CARTESIAN_POINT('Ctrl Pts',(-7.18651649009927,3.26798710116569,
-0.957338301667589));
#105775=CARTESIAN_POINT('Ctrl Pts',(-7.18704499319853,3.26863827733136,
-0.953387547335178));
#105776=CARTESIAN_POINT('',(-7.3971689596895,3.26733592550878,-1.23769598468391));
#105777=CARTESIAN_POINT('',(-7.2915784731849,3.26733592642396,-1.09949252872145));
#105778=CARTESIAN_POINT('',(-7.28168473605635,3.17766594628575,-1.79640402091834));
#105779=CARTESIAN_POINT('Ctrl Pts',(-7.3971689617301,3.26733592483313,-1.23769598491716));
#105780=CARTESIAN_POINT('Ctrl Pts',(-7.37856737175047,3.24953506265028,
-1.34886957116081));
#105781=CARTESIAN_POINT('Ctrl Pts',(-7.35749607004708,3.23184317427158,
-1.45939777806657));
#105782=CARTESIAN_POINT('Ctrl Pts',(-7.33402065462609,3.21428571393052,
-1.5691211020299));
#105783=CARTESIAN_POINT('Ctrl Pts',(-7.31778192897064,3.20214063496634,
-1.64502037415957));
#105784=CARTESIAN_POINT('Ctrl Pts',(-7.30033629090686,3.18993125792124,
-1.72080034764459));
#105785=CARTESIAN_POINT('Ctrl Pts',(-7.2816847361835,3.17766594609984,-1.79640402091955));
#105786=CARTESIAN_POINT('Ctrl Pts',(-7.03856093581467,3.13852541814607,
-1.73814842744475));
#105787=CARTESIAN_POINT('Ctrl Pts',(-7.07901199899998,3.14538569403019,
-1.74787924951643));
#105788=CARTESIAN_POINT('Ctrl Pts',(-7.11952115065935,3.15207184400054,
-1.75760381572493));
#105789=CARTESIAN_POINT('Ctrl Pts',(-7.20054920654423,3.16510741640785,
-1.77701816666527));
#105790=CARTESIAN_POINT('Ctrl Pts',(-7.24111568642906,3.17146448702765,
-1.78671934870936));
#105791=CARTESIAN_POINT('Ctrl Pts',(-7.28168473631141,3.17766594627506,
-1.79640401962634));
#105792=CARTESIAN_POINT('Ctrl Pts',(-7.12415677113848,3.26861999521842,
-2.3444521183563));
#105793=CARTESIAN_POINT('Ctrl Pts',(-7.12541698756924,3.26797796010921,
-2.34060870467815));
#105794=CARTESIAN_POINT('Ctrl Pts',(-7.126677204,3.267335925,-2.336765291));
#105795=CARTESIAN_POINT('Ctrl Pts',(-7.2532063,3.202873885,-1.950876291));
#105796=CARTESIAN_POINT('Ctrl Pts',(-7.337328235,3.137747733,-1.553581145));
#105797=CARTESIAN_POINT('Ctrl Pts',(-6.80865605252724,3.26861999521842,
-2.49093635239381));
#105798=CARTESIAN_POINT('Ctrl Pts',(-6.80999545126362,3.26797796010921,
-2.4872630026969));
#105799=CARTESIAN_POINT('Ctrl Pts',(-6.81133485,3.267335925,-2.483589653));
#105800=CARTESIAN_POINT('Ctrl Pts',(-6.945814061,3.202873885,-2.114775531));
#105801=CARTESIAN_POINT('Ctrl Pts',(-7.039683335,3.137747733,-1.733596997));
#105802=CARTESIAN_POINT('',(-7.1266771859077,3.26733592582622,-2.33676528743656));
#105803=CARTESIAN_POINT('Origin',(0.186940587355398,3.08932519213192,0.0315260866611503));
#105804=CARTESIAN_POINT('',(-6.96900603178777,3.26733592735283,-2.41017745815618));
#105805=CARTESIAN_POINT('Origin',(-1.4363510381088E-12,3.35806379999989,
-3.13984949151802E-13));
#105806=CARTESIAN_POINT('',(-7.28218582271254,3.35698786820963,-1.79437165603226));
#105807=CARTESIAN_POINT('Origin',(0.183257870511054,3.08947605308055,0.00198920916088918));
#105808=CARTESIAN_POINT('Origin',(0.18566933249872,3.48205906573847,0.0251509524794924));
#105809=CARTESIAN_POINT('Ctrl Pts',(-6.609635218,3.13774478,-3.544393078));
#105810=CARTESIAN_POINT('Ctrl Pts',(-6.724491896,3.176256335,-3.330206691));
#105811=CARTESIAN_POINT('Ctrl Pts',(-6.825240674,3.214285714,-3.109033571));
#105812=CARTESIAN_POINT('Ctrl Pts',(-6.895188305,3.240688665,-2.955478003));
#105813=CARTESIAN_POINT('Ctrl Pts',(-6.958159212,3.267335925,-2.798932008));
#105814=CARTESIAN_POINT('Ctrl Pts',(-6.95969802513763,3.26798710116569,
-2.79510651071521));
#105815=CARTESIAN_POINT('Ctrl Pts',(-6.96123683827525,3.26863827733136,
-2.79128101343042));
#105816=CARTESIAN_POINT('Ctrl Pts',(-6.498242333,3.13774478,-3.214863384));
#105817=CARTESIAN_POINT('Ctrl Pts',(-6.602420544,3.176256335,-3.004286703));
#105818=CARTESIAN_POINT('Ctrl Pts',(-6.692746959,3.214285714,-2.787407065));
#105819=CARTESIAN_POINT('Ctrl Pts',(-6.755458575,3.240688665,-2.636832366));
#105820=CARTESIAN_POINT('Ctrl Pts',(-6.81133485,3.267335925,-2.483589653));
#105821=CARTESIAN_POINT('Ctrl Pts',(-6.81270029239472,3.26798710116569,
-2.47984487765461));
#105822=CARTESIAN_POINT('Ctrl Pts',(-6.81406573478944,3.26863827733136,
-2.47610010230922));
#105823=CARTESIAN_POINT('',(-6.95815920959683,3.26733592550877,-2.79893200815632));
#105824=CARTESIAN_POINT('',(-6.88474702784079,3.26733592642396,-2.64126083873485));
#105825=CARTESIAN_POINT('',(-6.72526923023681,3.17766594630029,-3.31975206625678));
#105826=CARTESIAN_POINT('Ctrl Pts',(-6.95815921154404,3.26733592483523,
-2.79893200882494));
#105827=CARTESIAN_POINT('Ctrl Pts',(-6.91609348176499,3.24953506265028,
-2.90350762661683));
#105828=CARTESIAN_POINT('Ctrl Pts',(-6.8717545181582,3.23184317427134,-3.00692203827643));
#105829=CARTESIAN_POINT('Ctrl Pts',(-6.82524067351529,3.2142857138838,-3.10903357124645));
#105830=CARTESIAN_POINT('Ctrl Pts',(-6.7930655000057,3.20214063488939,-3.17966751488298));
#105831=CARTESIAN_POINT('Ctrl Pts',(-6.75973727706754,3.18993125792766,
-3.24992549778636));
#105832=CARTESIAN_POINT('Ctrl Pts',(-6.725269230334,3.17766594611253,-3.31975206627177));
#105833=CARTESIAN_POINT('Ctrl Pts',(-6.50035275888917,3.13852541814596,
-3.21059402588742));
#105834=CARTESIAN_POINT('Ctrl Pts',(-6.53776626148371,3.14538569432647,
-3.22879313049195));
#105835=CARTESIAN_POINT('Ctrl Pts',(-6.5752378395886,3.15207184462724,-3.24699861289385));
#105836=CARTESIAN_POINT('Ctrl Pts',(-6.65019798960515,3.16510741639772,
-3.283377702109));
#105837=CARTESIAN_POINT('Ctrl Pts',(-6.68773058054202,3.17146448703241,
-3.30157266991739));
#105838=CARTESIAN_POINT('Ctrl Pts',(-6.72526923077001,3.17766594629182,
-3.31975206507072));
#105839=CARTESIAN_POINT('Ctrl Pts',(-6.45361004080255,3.26861999521842,
-3.82112324805941));
#105840=CARTESIAN_POINT('Ctrl Pts',(-6.45566701440128,3.26797796010921,
-3.8176406005297));
#105841=CARTESIAN_POINT('Ctrl Pts',(-6.457723988,3.267335925,-3.814157953));
#105842=CARTESIAN_POINT('Ctrl Pts',(-6.664249632,3.202873885,-3.464490838));
#105843=CARTESIAN_POINT('Ctrl Pts',(-6.831811556,3.137747733,-3.094567962));
#105844=CARTESIAN_POINT('Ctrl Pts',(-6.11399577311955,3.26861999521842,
-3.89635943336084));
#105845=CARTESIAN_POINT('Ctrl Pts',(-6.11609351905978,3.26797796010921,
-3.89305989568042));
#105846=CARTESIAN_POINT('Ctrl Pts',(-6.118191265,3.267335925,-3.889760358));
#105847=CARTESIAN_POINT('Ctrl Pts',(-6.328810561,3.202873885,-3.558477961));
#105848=CARTESIAN_POINT('Ctrl Pts',(-6.50242734,3.137747733,-3.206390288));
#105849=CARTESIAN_POINT('',(-6.45772397105701,3.2673359258261,-3.81415794567119));
#105850=CARTESIAN_POINT('Origin',(0.175793103684657,3.08932515318603,0.0709758570261609));
#105851=CARTESIAN_POINT('',(-6.28795763415186,3.26733592735283,-3.85195914300908));
#105852=CARTESIAN_POINT('Origin',(-3.19189119579733E-13,3.35806379999956,
-4.5102810375397E-14));
#105853=CARTESIAN_POINT('',(-6.72619550069598,3.35698786820417,-3.31787493563951));
#105854=CARTESIAN_POINT('Origin',(0.178546055844735,3.08947598647104,0.0413378320615154));
#105855=CARTESIAN_POINT('Origin',(0.175921893134506,3.48205906426425,0.0644764226566241));
#105856=CARTESIAN_POINT('Ctrl Pts',(-5.69316587900001,3.13774478,-4.88240333000001));
#105857=CARTESIAN_POINT('Ctrl Pts',(-5.851381014,3.176256335,-4.697915292));
#105858=CARTESIAN_POINT('Ctrl Pts',(-5.997320024,3.214285714,-4.503571086));
#105859=CARTESIAN_POINT('Ctrl Pts',(-6.09864222700001,3.240688665,-4.368642235));
#105860=CARTESIAN_POINT('Ctrl Pts',(-6.19379367,3.267335925,-4.229293082));
#105861=CARTESIAN_POINT('Ctrl Pts',(-6.19611887536115,3.26798710116569,
-4.22588782205426));
#105862=CARTESIAN_POINT('Ctrl Pts',(-6.1984440807223,3.26863827733136,-4.22248256210852));
#105863=CARTESIAN_POINT('Ctrl Pts',(-5.655216442,3.13774478,-4.536631679));
#105864=CARTESIAN_POINT('Ctrl Pts',(-5.802226786,3.176256335,-4.3533734));
#105865=CARTESIAN_POINT('Ctrl Pts',(-5.93706413,3.214285714,-4.160981797));
#105866=CARTESIAN_POINT('Ctrl Pts',(-6.030678693,3.240688665,-4.027408594));
#105867=CARTESIAN_POINT('Ctrl Pts',(-6.118191265,3.267335925,-3.889760358));
#105868=CARTESIAN_POINT('Ctrl Pts',(-6.12032980010958,3.26798710116569,
-3.88639666317616));
#105869=CARTESIAN_POINT('Ctrl Pts',(-6.12246833521915,3.26863827733136,
-3.88303296835232));
#105870=CARTESIAN_POINT('',(-6.19379366761472,3.26733592550878,-4.22929308165504));
#105871=CARTESIAN_POINT('',(-6.1559924626444,3.26733592642396,-4.05952672736318));
#105872=CARTESIAN_POINT('',(-5.8543876097621,3.17766594631067,-4.68787219476722));
#105873=CARTESIAN_POINT('Ctrl Pts',(-6.19379366936754,3.26733592483246,
-4.22929308272258));
#105874=CARTESIAN_POINT('Ctrl Pts',(-6.13023074682398,3.24953506265028,
-4.32238089219935));
#105875=CARTESIAN_POINT('Ctrl Pts',(-6.06469736193084,3.23184317427164,
-4.41384596580043));
#105876=CARTESIAN_POINT('Ctrl Pts',(-5.99732002374697,3.21428571394204,
-4.50357108612209));
#105877=CARTESIAN_POINT('Ctrl Pts',(-5.9507128782345,3.20214063496735,-4.56563693622809));
#105878=CARTESIAN_POINT('Ctrl Pts',(-5.90306046074902,3.18993125790292,
-4.62708774391578));
#105879=CARTESIAN_POINT('Ctrl Pts',(-5.85438760969563,3.17766594610292,
-4.68787219467207));
#105880=CARTESIAN_POINT('Ctrl Pts',(-5.65819531310952,3.13852541812815,
-4.53291581612997));
#105881=CARTESIAN_POINT('Ctrl Pts',(-5.69082182373513,3.14538569108329,
-4.55873222060614));
#105882=CARTESIAN_POINT('Ctrl Pts',(-5.72350367863138,3.15207183800177,
-4.58456733645385));
#105883=CARTESIAN_POINT('Ctrl Pts',(-5.78889090646855,3.1651074164587,-4.63621014562947));
#105884=CARTESIAN_POINT('Ctrl Pts',(-5.82163462603071,3.17146448710556,
-4.66204812285444));
#105885=CARTESIAN_POINT('Ctrl Pts',(-5.85438761052842,3.17766594630774,
-4.68787219379599));
#105886=CARTESIAN_POINT('Ctrl Pts',(-5.48129967805377,3.26861999521842,
-5.11912290128042));
#105887=CARTESIAN_POINT('Ctrl Pts',(-5.48405722702689,3.26797796010921,
-5.11616386464021));
#105888=CARTESIAN_POINT('Ctrl Pts',(-5.48681477600001,3.267335925,-5.113204828));
#105889=CARTESIAN_POINT('Ctrl Pts',(-5.763680059,3.202873885,-4.816109645));
#105890=CARTESIAN_POINT('Ctrl Pts',(-6.006846961,3.137747733,-4.49085622));
#105891=CARTESIAN_POINT('Ctrl Pts',(-5.13345184724536,3.26861999521842,
-5.11959307791208));
#105892=CARTESIAN_POINT('Ctrl Pts',(-5.13620985212268,3.26797796010921,
-5.11682163495604));
#105893=CARTESIAN_POINT('Ctrl Pts',(-5.138967857,3.267335925,-5.114050192));
#105894=CARTESIAN_POINT('Ctrl Pts',(-5.415878914,3.202873885,-4.835789916));
#105895=CARTESIAN_POINT('Ctrl Pts',(-5.66112507100001,3.137747733,-4.529256333));
#105896=CARTESIAN_POINT('',(-5.48681476101586,3.2673359258261,-5.11320481720661));
#105897=CARTESIAN_POINT('Origin',(0.156425222198522,3.08932517488456,0.107106609688186));
#105898=CARTESIAN_POINT('',(-5.31289132665814,3.26733592735283,-5.11362749944603));
#105899=CARTESIAN_POINT('Origin',(-9.06393016197882E-14,3.35806380000078,
-5.85469173142172E-14));
#105900=CARTESIAN_POINT('',(-5.85569575173381,3.35698786820111,-4.68623807111382));
#105901=CARTESIAN_POINT('Origin',(0.165484884337215,3.08947604107569,0.0787531823238918));
#105902=CARTESIAN_POINT('Origin',(0.157948508963864,3.48205905793563,0.100787081180135));
#105903=CARTESIAN_POINT('Ctrl Pts',(-4.510490432,3.13774478,-5.992117828));
#105904=CARTESIAN_POINT('Ctrl Pts',(-4.704666059,3.176256335,-5.845954596));
#105905=CARTESIAN_POINT('Ctrl Pts',(-4.888971356,3.214285714,-5.687526623));
#105906=CARTESIAN_POINT('Ctrl Pts',(-5.016930416,3.240688665,-5.577533611));
#105907=CARTESIAN_POINT('Ctrl Pts',(-5.139813221,3.267335925,-5.461897111));
#105908=CARTESIAN_POINT('Ctrl Pts',(-5.14281609460832,3.26798710116569,
-5.45907131455102));
#105909=CARTESIAN_POINT('Ctrl Pts',(-5.14581896821665,3.26863827733136,
-5.45624551810205));
#105910=CARTESIAN_POINT('Ctrl Pts',(-4.547758915,3.13774478,-5.64627212));
#105911=CARTESIAN_POINT('Ctrl Pts',(-4.730727352,3.176256335,-5.498901196));
#105912=CARTESIAN_POINT('Ctrl Pts',(-4.903770781,3.214285714,-5.339993645));
#105913=CARTESIAN_POINT('Ctrl Pts',(-5.023910978,3.240688665,-5.229667673));
#105914=CARTESIAN_POINT('Ctrl Pts',(-5.138967857,3.267335925,-5.114050192));
#105915=CARTESIAN_POINT('Ctrl Pts',(-5.14177948931427,3.26798710116569,
-5.11122486031624));
#105916=CARTESIAN_POINT('Ctrl Pts',(-5.14459112162854,3.26863827733136,
-5.10839952863248));
#105917=CARTESIAN_POINT('',(-5.13981321874104,3.26733592550878,-5.46189711015752));
#105918=CARTESIAN_POINT('',(-5.13939053267506,3.26733592642396,-5.28797365764722));
#105919=CARTESIAN_POINT('',(-4.70976133171338,3.17766594633946,-5.83679262966929));
#105920=CARTESIAN_POINT('Ctrl Pts',(-5.13981322022166,3.2673359248313,-5.4618971115748));
#105921=CARTESIAN_POINT('Ctrl Pts',(-5.05772523537544,3.24953506265028,
-5.53914443058292));
#105922=CARTESIAN_POINT('Ctrl Pts',(-4.97406169733098,3.23184317427134,
-5.61438336149303));
#105923=CARTESIAN_POINT('Ctrl Pts',(-4.88897135546675,3.21428571388327,
-5.68752662272347));
#105924=CARTESIAN_POINT('Ctrl Pts',(-4.83011153576288,3.20214063488469,
-5.73812224877108));
#105925=CARTESIAN_POINT('Ctrl Pts',(-4.77036309859118,3.18993125793235,
-5.78789250995639));
#105926=CARTESIAN_POINT('Ctrl Pts',(-4.70976133169848,3.17766594613959,
-5.83679262960069));
#105927=CARTESIAN_POINT('Ctrl Pts',(-4.55146694246914,3.13852541813341,
-5.6432835011122));
#105928=CARTESIAN_POINT('Ctrl Pts',(-4.57778088596039,3.14538568749849,
-5.67551005078106));
#105929=CARTESIAN_POINT('Ctrl Pts',(-4.60414485520672,3.15207183068127,
-5.707766769236));
#105930=CARTESIAN_POINT('Ctrl Pts',(-4.656901714923,3.16510741563564,-5.77225855134485));
#105931=CARTESIAN_POINT('Ctrl Pts',(-4.68332549931054,3.17146448541837,
-5.80453137803275));
#105932=CARTESIAN_POINT('Ctrl Pts',(-4.70976133266641,3.17766594633659,
-5.8367926288889));
#105933=CARTESIAN_POINT('Ctrl Pts',(-4.25268983415697,3.26861999521842,
-6.17775805698345));
#105934=CARTESIAN_POINT('Ctrl Pts',(-4.25601901857848,3.26797796010921,
-6.17546099249173));
#105935=CARTESIAN_POINT('Ctrl Pts',(-4.259348203,3.267335925,-6.173163928));
#105936=CARTESIAN_POINT('Ctrl Pts',(-4.593607212,3.202873885,-5.942532517));
#105937=CARTESIAN_POINT('Ctrl Pts',(-4.901008879,3.137747733,-5.677157033));
#105938=CARTESIAN_POINT('Ctrl Pts',(-3.91287341787142,3.26861999521842,
-6.10344024028336));
#105939=CARTESIAN_POINT('Ctrl Pts',(-3.91616272043571,3.26797796010921,
-6.10132648164168));
#105940=CARTESIAN_POINT('Ctrl Pts',(-3.919452023,3.267335925,-6.09921272300001));
#105941=CARTESIAN_POINT('Ctrl Pts',(-4.249706787,3.202873885,-5.886985709));
#105942=CARTESIAN_POINT('Ctrl Pts',(-4.555114885,3.137747733,-5.640339386));
#105943=CARTESIAN_POINT('',(-4.25934819074955,3.26733592582622,-6.17316391421539));
#105944=CARTESIAN_POINT('Origin',(0.129743386737614,3.08932515652023,0.138229392214959));
#105945=CARTESIAN_POINT('',(-4.08940012518944,3.26733592735283,-6.13618831737648));
#105946=CARTESIAN_POINT('Origin',(1.05644659686988E-12,3.35806379999967,
1.36652841820073E-12));
#105947=CARTESIAN_POINT('',(-4.71139017780269,3.3569878681991,-5.83547792255985));
#105948=CARTESIAN_POINT('Origin',(0.144686138641019,3.08947604254338,0.112486115523743));
#105949=CARTESIAN_POINT('Origin',(0.132589486939138,3.48205905601155,0.132384954758726));
#105950=CARTESIAN_POINT('Ctrl Pts',(-3.116909465,3.13774478,-6.821647557));
#105951=CARTESIAN_POINT('Ctrl Pts',(-3.337966148,3.176256335,-6.72064355999999));
#105952=CARTESIAN_POINT('Ctrl Pts',(-3.55201982,3.214285714,-6.605539735));
#105953=CARTESIAN_POINT('Ctrl Pts',(-3.700632515,3.240688665,-6.525625715));
#105954=CARTESIAN_POINT('Ctrl Pts',(-3.845500817,3.267335925,-6.439108903));
#105955=CARTESIAN_POINT('Ctrl Pts',(-3.84904094778363,3.26798710116569,
-6.43699470116816));
#105956=CARTESIAN_POINT('Ctrl Pts',(-3.85258107856726,3.26863827733136,
-6.43488049933635));
#105957=CARTESIAN_POINT('Ctrl Pts',(-3.227653236,3.13774478,-6.491899151));
#105958=CARTESIAN_POINT('Ctrl Pts',(-3.438024365,3.176256335,-6.387306483));
#105959=CARTESIAN_POINT('Ctrl Pts',(-3.641182561,3.214285714,-6.269313324));
#105960=CARTESIAN_POINT('Ctrl Pts',(-3.78223077,3.240688665,-6.187393303));
#105961=CARTESIAN_POINT('Ctrl Pts',(-3.919452023,3.267335925,-6.09921272300001));
#105962=CARTESIAN_POINT('Ctrl Pts',(-3.92280528368717,3.26798710116569,
-6.09705786385231));
#105963=CARTESIAN_POINT('Ctrl Pts',(-3.92615854437433,3.26863827733136,
-6.09490300470461));
#105964=CARTESIAN_POINT('',(-3.84550081497584,3.26733592550878,-6.43910890169017));
#105965=CARTESIAN_POINT('',(-3.88247641250146,3.26733592642396,-6.26916081764383));
#105966=CARTESIAN_POINT('',(-3.34491184766582,3.17766594631022,-6.71279112817122));
#105967=CARTESIAN_POINT('Ctrl Pts',(-3.84550081611735,3.26733592483148,
-6.43910890339299));
#105968=CARTESIAN_POINT('Ctrl Pts',(-3.74872611297783,3.24953506265028,
-6.4969037326349));
#105969=CARTESIAN_POINT('Ctrl Pts',(-3.65084443590249,3.23184317427172,
-6.55239843112517));
#105970=CARTESIAN_POINT('Ctrl Pts',(-3.55201981981194,3.21428571395853,
-6.6055397349545));
#105971=CARTESIAN_POINT('Ctrl Pts',(-3.48365954638371,3.20214063501282,
-6.64229934251993));
#105972=CARTESIAN_POINT('Ctrl Pts',(-3.41460885920532,3.18993125792547,
-6.67806185439175));
#105973=CARTESIAN_POINT('Ctrl Pts',(-3.34491184770643,3.17766594611633,
-6.71279112818426));
#105974=CARTESIAN_POINT('Ctrl Pts',(-3.23191703662374,3.13852541813812,
-6.4897775205516));
#105975=CARTESIAN_POINT('Ctrl Pts',(-3.25068803514173,3.14538569335125,
-6.52690738312565));
#105976=CARTESIAN_POINT('Ctrl Pts',(-3.26950140689733,3.15207184262519,
-6.56407746803246));
#105977=CARTESIAN_POINT('Ctrl Pts',(-3.30716098130688,3.16510741642107,
-6.63840257006474));
#105978=CARTESIAN_POINT('Ctrl Pts',(-3.32602929113069,3.17146448706224,
-6.67560121406347));
#105979=CARTESIAN_POINT('Ctrl Pts',(-3.34491184880586,3.17766594630695,
-6.7127911275902));
#105980=CARTESIAN_POINT('Ctrl Pts',(-2.82522894021175,3.26861999521842,
-6.94752811231027));
#105981=CARTESIAN_POINT('Ctrl Pts',(-2.82897409110587,3.26797796010921,
-6.94600042815513));
#105982=CARTESIAN_POINT('Ctrl Pts',(-2.832719242,3.267335925,-6.944472744));
#105983=CARTESIAN_POINT('Ctrl Pts',(-3.208742396,3.202873885,-6.791089174));
#105984=CARTESIAN_POINT('Ctrl Pts',(-3.566005068,3.137747733,-6.598000292));
#105985=CARTESIAN_POINT('Ctrl Pts',(-2.5093333767475,3.26861999521842,-6.80189732065103));
#105986=CARTESIAN_POINT('Ctrl Pts',(-2.51300017287375,3.26797796010921,
-6.80054008332552));
#105987=CARTESIAN_POINT('Ctrl Pts',(-2.516666969,3.267335925,-6.799182846));
#105988=CARTESIAN_POINT('Ctrl Pts',(-2.884823095,3.202873885,-6.662912593));
#105989=CARTESIAN_POINT('Ctrl Pts',(-3.23611259,3.137747733,-6.487686437));
#105990=CARTESIAN_POINT('',(-2.83271923294473,3.2673359258261,-6.9444727279121));
#105991=CARTESIAN_POINT('Origin',(0.0969947647447311,3.08932521811194,0.162888536788507));
#105992=CARTESIAN_POINT('',(-2.67469311915078,3.26733592735283,-6.87182778968677));
#105993=CARTESIAN_POINT('Origin',(-5.73109268375838E-13,3.358063799999,
-1.16746889933239E-12));
#105994=CARTESIAN_POINT('',(-3.34678523580795,3.35698786818467,-6.71185731223826));
#105995=CARTESIAN_POINT('Origin',(0.117122493434923,3.08947601560677,0.140959894909082));
#105996=CARTESIAN_POINT('Origin',(0.101030779572149,3.48205907864295,0.15779271281936));
#105997=CARTESIAN_POINT('Ctrl Pts',(-1.577585275,3.13774478,-7.332204628));
#105998=CARTESIAN_POINT('Ctrl Pts',(-1.81518665,3.176256335,-7.2810827));
#105999=CARTESIAN_POINT('Ctrl Pts',(-2.048979786,3.214285714,-7.214685152));
#106000=CARTESIAN_POINT('Ctrl Pts',(-2.211297151,3.240688665,-7.16858681300001));
#106001=CARTESIAN_POINT('Ctrl Pts',(-2.37137707,3.267335925,-7.115235119));
#106002=CARTESIAN_POINT('Ctrl Pts',(-2.37528892539741,3.26798710116569,
-7.11393136951387));
#106003=CARTESIAN_POINT('Ctrl Pts',(-2.37920078079482,3.26863827733136,
-7.11262762002775));
#106004=CARTESIAN_POINT('Ctrl Pts',(-1.756626078,3.13774478,-7.033972194));
#106005=CARTESIAN_POINT('Ctrl Pts',(-1.984563179,3.176256335,-6.977048418));
#106006=CARTESIAN_POINT('Ctrl Pts',(-2.208336691,3.214285714,-6.905486881));
#106007=CARTESIAN_POINT('Ctrl Pts',(-2.363697654,3.240688665,-6.8558033));
#106008=CARTESIAN_POINT('Ctrl Pts',(-2.516666969,3.267335925,-6.79918284600001));
#106009=CARTESIAN_POINT('Ctrl Pts',(-2.52040506334849,3.26798710116569,
-6.7977992181848));
#106010=CARTESIAN_POINT('Ctrl Pts',(-2.52414315769698,3.26863827733136,
-6.79641559036959));
#106011=CARTESIAN_POINT('',(-2.37137706833076,3.26733592550877,-7.11523511726489));
#106012=CARTESIAN_POINT('',(-2.44402201117849,3.26733592642396,-6.9572089854233));
#106013=CARTESIAN_POINT('',(-1.82365800373359,3.17766594632019,-7.27490697422542));
#106014=CARTESIAN_POINT('Ctrl Pts',(-2.37137706908236,3.26733592483625,
-7.11523511918416));
#106015=CARTESIAN_POINT('Ctrl Pts',(-2.26444072465427,3.24953506265028,
-7.15087503666887));
#106016=CARTESIAN_POINT('Ctrl Pts',(-2.15691774689163,3.23184317427153,
-7.18403063290066));
#106017=CARTESIAN_POINT('Ctrl Pts',(-2.0489797858413,3.21428571392076,-7.21468515150108));
#106018=CARTESIAN_POINT('Ctrl Pts',(-1.97431550870438,3.20214063496236,
-7.23588990102936));
#106019=CARTESIAN_POINT('Ctrl Pts',(-1.89919130530067,3.18993125794642,
-7.25597244897035));
#106020=CARTESIAN_POINT('Ctrl Pts',(-1.8236580037907,3.17766594613755,-7.27490697433494));
#106021=CARTESIAN_POINT('Ctrl Pts',(-1.76124628115218,3.13852541813551,
-7.03281675718453));
#106022=CARTESIAN_POINT('Ctrl Pts',(-1.77159658622382,3.14538568332313,
-7.07311369491504));
#106023=CARTESIAN_POINT('Ctrl Pts',(-1.78197962487405,3.15207182215019,
-7.11345901470548));
#106024=CARTESIAN_POINT('Ctrl Pts',(-1.80278107244631,3.16510741643744,
-7.19414225903988));
#106025=CARTESIAN_POINT('Ctrl Pts',(-1.81321164292256,3.17146448706018,
-7.2345273480934));
#106026=CARTESIAN_POINT('Ctrl Pts',(-1.82365800497128,3.17766594630979,
-7.27490697385328));
#106027=CARTESIAN_POINT('Ctrl Pts',(-1.26566348041818,3.26861999521842,
-7.39243947503579));
#106028=CARTESIAN_POINT('Ctrl Pts',(-1.26964947870909,3.26797796010921,
-7.3917526040179));
#106029=CARTESIAN_POINT('Ctrl Pts',(-1.273635477,3.267335925,-7.391065733));
#106030=CARTESIAN_POINT('Ctrl Pts',(-1.673840353,3.202873885,-7.322102048));
#106031=CARTESIAN_POINT('Ctrl Pts',(-2.064258824,3.137747733,-7.210328391));
#106032=CARTESIAN_POINT('Ctrl Pts',(-0.988459695241115,3.26861999521842,
-7.18230524117258));
#106033=CARTESIAN_POINT('Ctrl Pts',(-0.992332529620557,3.26797796010921,
-7.18176798808629));
#106034=CARTESIAN_POINT('Ctrl Pts',(-0.996205364,3.267335925,-7.181230735));
#106035=CARTESIAN_POINT('Ctrl Pts',(-1.385048281,3.202873885,-7.12728909));
#106036=CARTESIAN_POINT('Ctrl Pts',(-1.765793266,3.137747733,-7.031676482));
#106037=CARTESIAN_POINT('',(-1.27363547160765,3.2673359258261,-7.39106571533973));
#106038=CARTESIAN_POINT('Origin',(0.0597108984205369,3.08932518088346,0.179931436801557));
#106039=CARTESIAN_POINT('',(-1.13492043497381,3.26733592735283,-7.28614823174549));
#106040=CARTESIAN_POINT('Origin',(1.57751416096641E-13,3.35806379999978,
5.0263612716428E-13));
#106041=CARTESIAN_POINT('',(-1.82568833597157,3.3569878682181,-7.27439771350992));
#106042=CARTESIAN_POINT('Origin',(0.0840819809147508,3.08947608719351,0.162842126678377));
#106043=CARTESIAN_POINT('Origin',(0.064747991376177,3.4820590220708,0.175822390860044));
#106044=CARTESIAN_POINT('Ctrl Pts',(0.035505048,3.13774478,-7.49991595900001));
#106045=CARTESIAN_POINT('Ctrl Pts',(-0.207531042,3.176256335,-7.501066506));
#106046=CARTESIAN_POINT('Ctrl Pts',(-0.450131734,3.214285714,-7.486479909));
#106047=CARTESIAN_POINT('Ctrl Pts',(-0.618563989,3.240688665,-7.476352759));
#106048=CARTESIAN_POINT('Ctrl Pts',(-0.786370366,3.267335925,-7.458660848));
#106049=CARTESIAN_POINT('Ctrl Pts',(-0.790471032002883,3.26798710116569,
-7.45822851271418));
#106050=CARTESIAN_POINT('Ctrl Pts',(-0.794571698005766,3.26863827733136,
-7.45779617742834));
#106051=CARTESIAN_POINT('Ctrl Pts',(-0.203461038,3.13774478,-7.24714451400001));
#106052=CARTESIAN_POINT('Ctrl Pts',(-0.438306025,3.176256335,-7.240551323));
#106053=CARTESIAN_POINT('Ctrl Pts',(-0.672231452,3.214285714,-7.218767545));
#106054=CARTESIAN_POINT('Ctrl Pts',(-0.834640663,3.240688665,-7.203643554));
#106055=CARTESIAN_POINT('Ctrl Pts',(-0.996205363999999,3.267335925,-7.181230735));
#106056=CARTESIAN_POINT('Ctrl Pts',(-1.00015350285206,3.26798710116569,
-7.18068303540392));
#106057=CARTESIAN_POINT('Ctrl Pts',(-1.00410164170411,3.26863827733136,
-7.18013533580784));
#106058=CARTESIAN_POINT('',(-0.891287856244616,3.26733592642396,-7.31994579256607));
#106059=CARTESIAN_POINT('Ctrl Pts',(-0.208221607850335,3.13852541811002,
-7.24700929788454));
#106060=CARTESIAN_POINT('Ctrl Pts',(-0.209667279556549,3.14538569103608,
-7.28858917220968));
#106061=CARTESIAN_POINT('Ctrl Pts',(-0.211134519267141,3.15207183792157,
-7.33022334130803));
#106062=CARTESIAN_POINT('Ctrl Pts',(-0.214105124329206,3.16510741640027,
-7.41349185170254));
#106063=CARTESIAN_POINT('Ctrl Pts',(-0.215610233503705,3.17146448703367,
-7.4551750242645));
#106064=CARTESIAN_POINT('Ctrl Pts',(-0.217131939498219,3.17766594626658,
-7.49685625577675));
#106065=CARTESIAN_POINT('Ctrl Pts',(0.35308299665963,3.26861999521842,-7.49168858409584));
#106066=CARTESIAN_POINT('Ctrl Pts',(0.349042531829815,3.26797796010921,
-7.49187464354792));
#106067=CARTESIAN_POINT('Ctrl Pts',(0.345002067,3.267335925,-7.49206070300001));
#106068=CARTESIAN_POINT('Ctrl Pts',(-0.060671395,3.202873885,-7.510741569));
#106069=CARTESIAN_POINT('Ctrl Pts',(-0.465990131,3.137747733,-7.485509548));
#106070=CARTESIAN_POINT('Ctrl Pts',(0.578633262375529,3.26861999521842,
-7.22687655198706));
#106071=CARTESIAN_POINT('Ctrl Pts',(0.574735479187765,3.26797796010921,
-7.22718440449353));
#106072=CARTESIAN_POINT('Ctrl Pts',(0.570837696,3.267335925,-7.227492257));
#106073=CARTESIAN_POINT('Ctrl Pts',(0.179489852,3.202873885,-7.258401471));
#106074=CARTESIAN_POINT('Ctrl Pts',(-0.212907412,3.137747733,-7.246873149));
#106075=CARTESIAN_POINT('',(0.457919866872506,3.26733592735402,-7.35977648091011));
#106076=CARTESIAN_POINT('Ctrl Pts',(1.646935195,3.13774478,-7.316939556));
#106077=CARTESIAN_POINT('Ctrl Pts',(1.409828488,3.176256335,-7.370308779));
#106078=CARTESIAN_POINT('Ctrl Pts',(1.169763977,3.214285714,-7.408215186));
#106079=CARTESIAN_POINT('Ctrl Pts',(1.003092537,3.240688665,-7.434532759));
#106080=CARTESIAN_POINT('Ctrl Pts',(0.835406142,3.267335925,-7.453327886));
#106081=CARTESIAN_POINT('Ctrl Pts',(0.831308407984072,3.26798710116569,
-7.45378718045404));
#106082=CARTESIAN_POINT('Ctrl Pts',(0.827210673968144,3.26863827733136,
-7.45424647490808));
#106083=CARTESIAN_POINT('Ctrl Pts',(1.359217614,3.13774478,-7.121448411));
#106084=CARTESIAN_POINT('Ctrl Pts',(1.128445831,3.176256335,-7.16549409600001));
#106085=CARTESIAN_POINT('Ctrl Pts',(0.895306583,3.214285714,-7.194506663));
#106086=CARTESIAN_POINT('Ctrl Pts',(0.733443198,3.240688665,-7.214649441));
#106087=CARTESIAN_POINT('Ctrl Pts',(0.570837696,3.267335925,-7.227492257));
#106088=CARTESIAN_POINT('Ctrl Pts',(0.566864123208228,3.26798710116569,
-7.22780609548393));
#106089=CARTESIAN_POINT('Ctrl Pts',(0.562890550416455,3.26863827733136,
-7.22811993396787));
#106090=CARTESIAN_POINT('',(0.835406142818811,3.26733592550878,-7.45332788373253));
#106091=CARTESIAN_POINT('',(0.703121927779861,3.26733592642396,-7.340410070659));
#106092=CARTESIAN_POINT('',(1.39954697555713,3.17766594628976,-7.3682608711216));
#106093=CARTESIAN_POINT('Ctrl Pts',(0.835406142940577,3.26733592483152,
-7.45332788577904));
#106094=CARTESIAN_POINT('Ctrl Pts',(0.94742375383149,3.24953506265028,-7.44077239346166));
#106095=CARTESIAN_POINT('Ctrl Pts',(1.05893063889937,3.23184317427131,-7.42571587126418));
#106096=CARTESIAN_POINT('Ctrl Pts',(1.16976397728219,3.21428571387816,-7.4082151854994));
#106097=CARTESIAN_POINT('Ctrl Pts',(1.24643108382801,3.20214063485909,-7.3961093787905));
#106098=CARTESIAN_POINT('Ctrl Pts',(1.32304440699507,3.18993125789757,-7.38279197147513));
#106099=CARTESIAN_POINT('Ctrl Pts',(1.39954697551669,3.17766594608606,-7.36826087108064));
#106100=CARTESIAN_POINT('Ctrl Pts',(1.3545392766959,3.13852541811858,-7.12233973838241));
#106101=CARTESIAN_POINT('Ctrl Pts',(1.36206584354755,3.14538568717469,-7.16325825206757));
#106102=CARTESIAN_POINT('Ctrl Pts',(1.36958301790223,3.1520718300302,-7.20423442404044));
#106103=CARTESIAN_POINT('Ctrl Pts',(1.38458214145238,3.16510741642671,-7.28619480500098));
#106104=CARTESIAN_POINT('Ctrl Pts',(1.39207287092915,3.17146448706813,-7.32722700216388));
#106105=CARTESIAN_POINT('Ctrl Pts',(1.39954697430732,3.17766594628681,-7.3682608713497));
#106106=CARTESIAN_POINT('Ctrl Pts',(1.95531970545204,3.26861999521842,-7.24063466103159));
#106107=CARTESIAN_POINT('Ctrl Pts',(1.95141370172602,3.26797796010921,-7.2416849510158));
#106108=CARTESIAN_POINT('Ctrl Pts',(1.947507698,3.267335925,-7.242735241));
#106109=CARTESIAN_POINT('Ctrl Pts',(1.55533449,3.202873885,-7.348187161));
#106110=CARTESIAN_POINT('Ctrl Pts',(1.154067742,3.137747733,-7.410676599));
#106111=CARTESIAN_POINT('Ctrl Pts',(2.11866997199718,3.26861999521842,-6.93352714751366));
#106112=CARTESIAN_POINT('Ctrl Pts',(2.11492949599859,3.26797796010921,-6.93466571075683));
#106113=CARTESIAN_POINT('Ctrl Pts',(2.11118902,3.267335925,-6.93580427400001));
#106114=CARTESIAN_POINT('Ctrl Pts',(1.735635238,3.202873885,-7.050119065));
#106115=CARTESIAN_POINT('Ctrl Pts',(1.349933756,3.137747733,-7.123214082));
#106116=CARTESIAN_POINT('',(1.94750769550073,3.26733592582611,-7.2427352226932));
#106117=CARTESIAN_POINT('Origin',(-0.0213591459166254,3.08932517974553,
0.188373488840997));
#106118=CARTESIAN_POINT('',(2.02934834491728,3.26733592735283,-7.08926976153127));
#106119=CARTESIAN_POINT('Origin',(-1.20996962449382E-13,3.3580638,4.05491612509579E-13));
#106120=CARTESIAN_POINT('',(1.39749046265521,3.35698786822937,-7.36865119336134));
#106121=CARTESIAN_POINT('Origin',(0.00793508467649223,3.08947604551196,
0.183096902086818));
#106122=CARTESIAN_POINT('Origin',(-0.0150621914402294,3.48205902360382,
0.186758929055496));
#106123=CARTESIAN_POINT('Ctrl Pts',(3.181356483,3.13774478,-6.791831191));
#106124=CARTESIAN_POINT('Ctrl Pts',(2.961266004,3.176256335,-6.894923605));
#106125=CARTESIAN_POINT('Ctrl Pts',(2.734962825,3.214285714,-6.983550554));
#106126=CARTESIAN_POINT('Ctrl Pts',(2.577845571,3.240688665,-7.04508227100001));
#106127=CARTESIAN_POINT('Ctrl Pts',(2.418119987,3.267335925,-7.099485596));
#106128=CARTESIAN_POINT('Ctrl Pts',(2.41421679044806,3.26798710116569,-7.10081504407736));
#106129=CARTESIAN_POINT('Ctrl Pts',(2.41031359389613,3.26863827733136,-7.10214449215472));
#106130=CARTESIAN_POINT('Ctrl Pts',(2.858340762,3.13774478,-6.662761296));
#106131=CARTESIAN_POINT('Ctrl Pts',(2.642432815,3.176256335,-6.755386329));
#106132=CARTESIAN_POINT('Ctrl Pts',(2.420981077,3.214285714,-6.833838645));
#106133=CARTESIAN_POINT('Ctrl Pts',(2.26723207,3.240688665,-6.88830634));
#106134=CARTESIAN_POINT('Ctrl Pts',(2.11118902,3.267335925,-6.935804274));
#106135=CARTESIAN_POINT('Ctrl Pts',(2.10737581312693,3.26798710116569,-6.93696497579598));
#106136=CARTESIAN_POINT('Ctrl Pts',(2.10356260625386,3.26863827733136,-6.93812567759196));
#106137=CARTESIAN_POINT('',(2.41811998730806,3.26733592550877,-7.09948559360933));
#106138=CARTESIAN_POINT('',(2.2646545118938,3.26733592642396,-7.01764493229125));
#106139=CARTESIAN_POINT('',(2.95078462776239,3.17766594632317,-6.89513379697716));
#106140=CARTESIAN_POINT('Ctrl Pts',(2.41811998786744,3.26733592483209,-7.09948559558307));
#106141=CARTESIAN_POINT('Ctrl Pts',(2.52481962986193,3.24953506265028,-7.0631431689244));
#106142=CARTESIAN_POINT('Ctrl Pts',(2.63048283882753,3.23184317427183,-7.02446797538068));
#106143=CARTESIAN_POINT('Ctrl Pts',(2.73496282496311,3.21428571397938,-6.98355055387583));
#106144=CARTESIAN_POINT('Ctrl Pts',(2.80723510623411,3.20214063505568,-6.95524661319201));
#106145=CARTESIAN_POINT('Ctrl Pts',(2.87919440373112,3.18993125793867,-6.9257709591031));
#106146=CARTESIAN_POINT('Ctrl Pts',(2.95078462775552,3.1776659461331,-6.89513379703719));
#106147=CARTESIAN_POINT('Ctrl Pts',(2.85396340915401,3.1385254181184,-6.66463748826854));
#106148=CARTESIAN_POINT('Ctrl Pts',(2.87011029021384,3.14538569143452,-6.70298138426603));
#106149=CARTESIAN_POINT('Ctrl Pts',(2.88626039462627,3.15207183875374,-6.74138361346276));
#106150=CARTESIAN_POINT('Ctrl Pts',(2.91852788258014,3.16510741556512,-6.81820338161874));
#106151=CARTESIAN_POINT('Ctrl Pts',(2.93466419007876,3.17146448533258,-6.85666597771207));
#106152=CARTESIAN_POINT('Ctrl Pts',(2.95078462657957,3.17766594631795,-6.89513379745628));
#106153=CARTESIAN_POINT('Ctrl Pts',(3.46612783746513,3.26861999521842,-6.65101670874053));
#106154=CARTESIAN_POINT('Ctrl Pts',(3.46253893523256,3.26797796010921,-6.65288211887026));
#106155=CARTESIAN_POINT('Ctrl Pts',(3.458950033,3.267335925,-6.654747529));
#106156=CARTESIAN_POINT('Ctrl Pts',(3.098614662,3.202873885,-6.842039689));
#106157=CARTESIAN_POINT('Ctrl Pts',(2.72016269,3.137747733,-6.989328647));
#106158=CARTESIAN_POINT('Ctrl Pts',(3.55964002860692,3.26861999521842,-6.31597371891253));
#106159=CARTESIAN_POINT('Ctrl Pts',(3.55623176030346,3.26797796010921,-6.31788975495627));
#106160=CARTESIAN_POINT('Ctrl Pts',(3.552823492,3.267335925,-6.319805791));
#106161=CARTESIAN_POINT('Ctrl Pts',(3.21062425,3.202873885,-6.512180928));
#106162=CARTESIAN_POINT('Ctrl Pts',(2.849653521,3.137747733,-6.666481441));
#106163=CARTESIAN_POINT('',(3.45895002662524,3.26733592582611,-6.65474751165654));
#106164=CARTESIAN_POINT('Origin',(-0.0613544418924655,3.08932515244115,
0.179377709456058));
#106165=CARTESIAN_POINT('',(3.50588674961313,3.26733592735283,-6.48727666696439));
#106166=CARTESIAN_POINT('Origin',(-1.83013326715553E-13,3.35806380000067,
3.60822483003176E-13));
#106167=CARTESIAN_POINT('',(2.94886010292606,3.35698786820659,-6.89595708331305));
#106168=CARTESIAN_POINT('Origin',(-0.0316109121111718,3.08947599794032,
0.18052218025897));
#106169=CARTESIAN_POINT('Origin',(-0.0548577581699217,3.48205904643279,
0.179154830677182));
#106170=CARTESIAN_POINT('Ctrl Pts',(4.567021077,3.13774478,-5.949144349));
#106171=CARTESIAN_POINT('Ctrl Pts',(4.374238013,3.176256335,-6.097139466));
#106172=CARTESIAN_POINT('Ctrl Pts',(4.172277851,3.214285714,-6.232342861));
#106173=CARTESIAN_POINT('Ctrl Pts',(4.032061411,3.240688665,-6.326211565));
#106174=CARTESIAN_POINT('Ctrl Pts',(3.88776523,3.267335925,-6.41367925));
#106175=CARTESIAN_POINT('Ctrl Pts',(3.88423908007441,3.26798710116569,-6.41581668821089));
#106176=CARTESIAN_POINT('Ctrl Pts',(3.88071293014881,3.26863827733136,-6.41795412642177));
#106177=CARTESIAN_POINT('Ctrl Pts',(4.223811072,3.13774478,-5.89253086800001));
#106178=CARTESIAN_POINT('Ctrl Pts',(4.032862577,3.176256335,-6.029404205));
#106179=CARTESIAN_POINT('Ctrl Pts',(3.833453187,3.214285714,-6.153627927));
#106180=CARTESIAN_POINT('Ctrl Pts',(3.69500769,3.240688665,-6.239873689));
#106181=CARTESIAN_POINT('Ctrl Pts',(3.552823492,3.267335925,-6.319805791));
#106182=CARTESIAN_POINT('Ctrl Pts',(3.549348952371,3.26798710116569,-6.32175908299683));
#106183=CARTESIAN_POINT('Ctrl Pts',(3.54587441274199,3.26863827733136,-6.32371237499365));
#106184=CARTESIAN_POINT('',(3.88776522976391,3.26733592550877,-6.41367924760373));
#106185=CARTESIAN_POINT('',(3.72029436861526,3.26733592642396,-6.36674251605016));
#106186=CARTESIAN_POINT('',(4.36404687056657,3.17766594631752,-6.09959793024141));
#106187=CARTESIAN_POINT('Ctrl Pts',(3.88776523073915,3.26733592483553,-6.41367924941769));
#106188=CARTESIAN_POINT('Ctrl Pts',(3.9841577463695,3.24953506265028,-6.35524921920966));
#106189=CARTESIAN_POINT('Ctrl Pts',(4.07903658468512,3.23184317427146,-6.29476376382527));
#106190=CARTESIAN_POINT('Ctrl Pts',(4.17227785102703,3.21428571390619,-6.23234286055702));
#106191=CARTESIAN_POINT('Ctrl Pts',(4.23677593593141,3.20214063493194,-6.18916424567221));
#106192=CARTESIAN_POINT('Ctrl Pts',(4.30071647048087,3.18993125793788,-6.14490859455356));
#106193=CARTESIAN_POINT('Ctrl Pts',(4.36404687058658,3.17766594612954,-6.09959793032027));
#106194=CARTESIAN_POINT('Ctrl Pts',(4.21993938588018,3.13852541808793,-5.89530419738614));
#106195=CARTESIAN_POINT('Ctrl Pts',(4.24395154840076,3.14538568641129,-5.92928050744133));
#106196=CARTESIAN_POINT('Ctrl Pts',(4.26797939619281,3.15207182851426,-5.9633130900975));
#106197=CARTESIAN_POINT('Ctrl Pts',(4.31600650821998,3.16510741641384,-6.03140035644281));
#106198=CARTESIAN_POINT('Ctrl Pts',(4.3400338824849,3.17146448705569,-6.06549489429013));
#106199=CARTESIAN_POINT('Ctrl Pts',(4.36404686950019,3.17766594631037,-6.09959793095783));
#106200=CARTESIAN_POINT('Ctrl Pts',(4.81486368430831,3.26861999521842,-5.75040460645348));
#106201=CARTESIAN_POINT('Ctrl Pts',(4.81175969665416,3.26797796010921,-5.75299791222674));
#106202=CARTESIAN_POINT('Ctrl Pts',(4.808655709,3.267335925,-5.755591218));
#106203=CARTESIAN_POINT('Ctrl Pts',(4.497007057,3.202873885,-6.015966045));
#106204=CARTESIAN_POINT('Ctrl Pts',(4.159065854,3.137747733,-6.241167457));
#106205=CARTESIAN_POINT('Ctrl Pts',(4.83416527354552,3.26861999521842,-5.40309237873128));
#106206=CARTESIAN_POINT('Ctrl Pts',(4.83124857977277,3.26797796010921,-5.40569629586564));
#106207=CARTESIAN_POINT('Ctrl Pts',(4.828331886,3.267335925,-5.40830021300001));
#106208=CARTESIAN_POINT('Ctrl Pts',(4.53548804,3.202873885,-5.669740449));
#106209=CARTESIAN_POINT('Ctrl Pts',(4.216126656,3.137747733,-5.898031538));
#106210=CARTESIAN_POINT('',(4.80865569902819,3.26733592582611,-5.75559120246355));
#106211=CARTESIAN_POINT('Origin',(-0.0984809776797785,3.08932516186255,
0.161994630856843));
#106212=CARTESIAN_POINT('',(4.81849378641155,3.26733592735283,-5.58194572507186));
#106213=CARTESIAN_POINT('Origin',(-1.25051878574478E-12,3.35806380000044,
1.72258041164497E-12));
#106214=CARTESIAN_POINT('',(4.36234432258694,3.35698786820303,-6.10081568391773));
#106215=CARTESIAN_POINT('Origin',(-0.0696785071250122,3.08947601273034,
0.169505791713984));
#106216=CARTESIAN_POINT('Origin',(-0.09208796268315,3.48205902148428,0.163173162085032));
#106217=CARTESIAN_POINT('Ctrl Pts',(5.739136842,3.13774478,-4.828282128));
#106218=CARTESIAN_POINT('Ctrl Pts',(5.58267551400001,3.176256335,-5.014259863));
#106219=CARTESIAN_POINT('Ctrl Pts',(5.414501802,3.214285714,-5.189717742));
#106220=CARTESIAN_POINT('Ctrl Pts',(5.29774254,3.240688665,-5.311534238));
#106221=CARTESIAN_POINT('Ctrl Pts',(5.175622891,3.267335925,-5.42797639000001));
#106222=CARTESIAN_POINT('Ctrl Pts',(5.17263866655102,3.26798710116569,-5.43082187407841));
#106223=CARTESIAN_POINT('Ctrl Pts',(5.16965444210204,3.26863827733136,-5.43366735815682));
#106224=CARTESIAN_POINT('Ctrl Pts',(5.391780671,3.13774478,-4.846772245));
#106225=CARTESIAN_POINT('Ctrl Pts',(5.234720168,3.176256335,-5.021493842));
#106226=CARTESIAN_POINT('Ctrl Pts',(5.066677286,3.214285714,-5.185680407));
#106227=CARTESIAN_POINT('Ctrl Pts',(4.950008857,3.240688665,-5.29967148));
#106228=CARTESIAN_POINT('Ctrl Pts',(4.828331886,3.267335925,-5.408300213));
#106229=CARTESIAN_POINT('Ctrl Pts',(4.82535847922468,3.26798710116569,-5.41095476141654));
#106230=CARTESIAN_POINT('Ctrl Pts',(4.82238507244937,3.26863827733136,-5.41360930983306));
#106231=CARTESIAN_POINT('',(5.17562289027218,3.26733592550877,-5.4279763877023));
#106232=CARTESIAN_POINT('',(5.00197739498063,3.26733592642396,-5.41813829551714));
#106233=CARTESIAN_POINT('',(5.57325113228991,3.17766594629067,-5.01885164342991));
#106234=CARTESIAN_POINT('Ctrl Pts',(5.17562289160948,3.26733592483259,-5.42797638925954));
#106235=CARTESIAN_POINT('Ctrl Pts',(5.25720107397617,3.24953506265028,-5.35019087963773));
#106236=CARTESIAN_POINT('Ctrl Pts',(5.33685911291995,3.23184317427168,-5.27072339506802));
#106237=CARTESIAN_POINT('Ctrl Pts',(5.41450180158225,3.21428571395063,-5.18971774176483));
#106238=CARTESIAN_POINT('Ctrl Pts',(5.46820983098211,3.20214063499304,-5.13368343749541));
#106239=CARTESIAN_POINT('Ctrl Pts',(5.52114181517994,3.1899312579122,-5.07671713370057));
#106240=CARTESIAN_POINT('Ctrl Pts',(5.57325113229803,3.17766594609559,-5.01885164347858));
#106241=CARTESIAN_POINT('Ctrl Pts',(5.38859568690581,3.13852541812473,-4.85031303370965));
#106242=CARTESIAN_POINT('Ctrl Pts',(5.41935036615269,3.14538568767711,-4.87833309643387));
#106243=CARTESIAN_POINT('Ctrl Pts',(5.45013246174096,3.15207183104302,-4.90640474502264));
#106244=CARTESIAN_POINT('Ctrl Pts',(5.5116734644145,3.16510741642622,-4.96257574886785));
#106245=CARTESIAN_POINT('Ctrl Pts',(5.54246840988429,3.17146448705763,-4.99070800020555));
#106246=CARTESIAN_POINT('Ctrl Pts',(5.57325113140873,3.17766594628625,-5.01885164437964));
#106247=CARTESIAN_POINT('Ctrl Pts',(5.93846185711766,3.26861999521842,-4.58090997634739));
#106248=CARTESIAN_POINT('Ctrl Pts',(5.93598792305883,3.26797796010921,-4.5841099176737));
#106249=CARTESIAN_POINT('Ctrl Pts',(5.933513989,3.267335925,-4.587309859));
#106250=CARTESIAN_POINT('Ctrl Pts',(5.685124401,3.202873885,-4.908592516));
#106251=CARTESIAN_POINT('Ctrl Pts',(5.403495721,3.137747733,-5.201176212));
#106252=CARTESIAN_POINT('Ctrl Pts',(5.88265032276119,3.26861999521842,-4.23756844513487));
#106253=CARTESIAN_POINT('Ctrl Pts',(5.8803615848806,3.26797796010921,-4.24073848706743));
#106254=CARTESIAN_POINT('Ctrl Pts',(5.878072847,3.267335925,-4.243908529));
#106255=CARTESIAN_POINT('Ctrl Pts',(5.64827745,3.202873885,-4.562189207));
#106256=CARTESIAN_POINT('Ctrl Pts',(5.385458394,3.137747733,-4.853796235));
#106257=CARTESIAN_POINT('',(5.93351397592557,3.2673359258261,-4.58730984595519));
#106258=CARTESIAN_POINT('Origin',(-0.13100224346366,3.08932516317078,0.137036486033113));
#106259=CARTESIAN_POINT('',(5.90579340922846,3.26733592735283,-4.41560920573176));
#106260=CARTESIAN_POINT('Origin',(5.63785129692462E-15,3.35806379999922,
1.34441069388203E-13));
#106261=CARTESIAN_POINT('',(5.57185016983664,3.35698786820608,-5.02040692449348));
#106262=CARTESIAN_POINT('Origin',(-0.104488342131043,3.08947596006111,0.150564189048316));
#106263=CARTESIAN_POINT('Origin',(-0.125012668882279,3.48205909152955,0.139562309966013));
#106264=CARTESIAN_POINT('Ctrl Pts',(6.642896946,3.13774478,-3.481654802));
#106265=CARTESIAN_POINT('Ctrl Pts',(6.530073313,3.176256335,-3.696919041));
#106266=CARTESIAN_POINT('Ctrl Pts',(6.403549666,3.214285714,-3.904427189));
#106267=CARTESIAN_POINT('Ctrl Pts',(6.315707117,3.240688665,-4.048495473));
#106268=CARTESIAN_POINT('Ctrl Pts',(6.221474178,3.267335925,-4.188467387));
#106269=CARTESIAN_POINT('Ctrl Pts',(6.21917141802021,3.26798710116569,-4.19188786528789));
#106270=CARTESIAN_POINT('Ctrl Pts',(6.21686865804042,3.26863827733136,-4.19530834357579));
#106271=CARTESIAN_POINT('Ctrl Pts',(6.307636598,3.13774478,-3.574383939));
#106272=CARTESIAN_POINT('Ctrl Pts',(6.191808061,3.176256335,-3.778784008));
#106273=CARTESIAN_POINT('Ctrl Pts',(6.062989186,3.214285714,-3.975256234));
#106274=CARTESIAN_POINT('Ctrl Pts',(5.973553112,3.240688665,-4.111662523));
#106275=CARTESIAN_POINT('Ctrl Pts',(5.878072847,3.267335925,-4.243908529));
#106276=CARTESIAN_POINT('Ctrl Pts',(5.87573960625175,3.26798710116569,-4.24714021012271));
#106277=CARTESIAN_POINT('Ctrl Pts',(5.87340636550352,3.26863827733136,-4.25037189124542));
#106278=CARTESIAN_POINT('',(6.22147417679744,3.26733592550878,-4.18846738491078));
#106279=CARTESIAN_POINT('',(6.04977351754298,3.26733592642396,-4.21618795076387));
#106280=CARTESIAN_POINT('',(6.52185636487934,3.177665946289,-3.70342943169034));
#106281=CARTESIAN_POINT('Ctrl Pts',(6.22147417843737,3.26733592483217,-4.18846738614363));
#106282=CARTESIAN_POINT('Ctrl Pts',(6.28442352312444,3.24953506265028,-4.09496356066983));
#106283=CARTESIAN_POINT('Ctrl Pts',(6.34513604112105,3.23184317427178,-4.00022985798987));
#106284=CARTESIAN_POINT('Ctrl Pts',(6.40354966577435,3.21428571396938,-3.90442718890104));
#106285=CARTESIAN_POINT('Ctrl Pts',(6.44395631252021,3.20214063502836,-3.83815729691068));
#106286=CARTESIAN_POINT('Ctrl Pts',(6.4834047045776,3.18993125791671,-3.77114402172454));
#106287=CARTESIAN_POINT('Ctrl Pts',(6.52185636493112,3.17766594609818,-3.70342943175431));
#106288=CARTESIAN_POINT('Ctrl Pts',(6.30528724149941,3.13852541814473,-3.57852662369783));
#106289=CARTESIAN_POINT('Ctrl Pts',(6.34134639814436,3.14538569135369,-3.59928025709094));
#106290=CARTESIAN_POINT('Ctrl Pts',(6.37744342249335,3.15207183854731,-3.62007837831597));
#106291=CARTESIAN_POINT('Ctrl Pts',(6.44962069464325,3.16510741639835,-3.6617066147144));
#106292=CARTESIAN_POINT('Ctrl Pts',(6.48574327389207,3.1714644870305,-3.68256114658771));
#106293=CARTESIAN_POINT('Ctrl Pts',(6.52185636420256,3.17766594628177,-3.70342943280469));
#106294=CARTESIAN_POINT('Ctrl Pts',(6.78438415313431,3.26861999521842,-3.1972170876818));
#106295=CARTESIAN_POINT('Ctrl Pts',(6.78265595106716,3.26797796010921,-3.2008740388409));
#106296=CARTESIAN_POINT('Ctrl Pts',(6.780927749,3.267335925,-3.20453099));
#106297=CARTESIAN_POINT('Ctrl Pts',(6.607411645,3.202873885,-3.571698655));
#106298=CARTESIAN_POINT('Ctrl Pts',(6.395264134,3.137747733,-3.917983749));
#106299=CARTESIAN_POINT('Ctrl Pts',(6.65606918130502,3.26861999521842,-2.87390051977844));
#106300=CARTESIAN_POINT('Ctrl Pts',(6.65451541815251,3.26797796010921,-2.87748845888922));
#106301=CARTESIAN_POINT('Ctrl Pts',(6.652961655,3.267335925,-2.881076398));
#106302=CARTESIAN_POINT('Ctrl Pts',(6.49695968400001,3.202873885,-3.241315069));
#106303=CARTESIAN_POINT('Ctrl Pts',(6.302972082,3.137747733,-3.582602815));
#106304=CARTESIAN_POINT('',(6.78092773340377,3.26733592582742,-3.20453098004515));
#106305=CARTESIAN_POINT('Origin',(-0.157398646388475,3.0893251739778,0.105671234425524));
#106306=CARTESIAN_POINT('',(6.71694469594588,3.26733592735657,-3.04280370736438));
#106307=CARTESIAN_POINT('Origin',(-2.13804668414141E-13,3.35806379999933,
1.2338220722885E-13));
#106308=CARTESIAN_POINT('',(6.52082249528588,3.35698786822526,-3.70524951664081));
#106309=CARTESIAN_POINT('Origin',(-0.134411997813779,3.08947603517803,0.124581958717571));
#106310=CARTESIAN_POINT('Origin',(-0.152091470713358,3.48205903068806,0.109425263944726));
#106311=CARTESIAN_POINT('Ctrl Pts',(7.236042573,3.13774478,-1.972229166));
#106312=CARTESIAN_POINT('Ctrl Pts',(7.172132141,3.176256335,-2.206714393));
#106313=CARTESIAN_POINT('Ctrl Pts',(7.093174665,3.214285714,-2.436569961));
#106314=CARTESIAN_POINT('Ctrl Pts',(7.038356248,3.240688665,-2.596153559));
#106315=CARTESIAN_POINT('Ctrl Pts',(6.976416247,3.267335925,-2.753110305));
#106316=CARTESIAN_POINT('Ctrl Pts',(6.97490262599906,3.26798710116569,-2.75694583976186));
#106317=CARTESIAN_POINT('Ctrl Pts',(6.97338900499812,3.26863827733136,-2.76078137452372));
#106318=CARTESIAN_POINT('Ctrl Pts',(6.92855444900001,3.13774478,-2.134861413));
#106319=CARTESIAN_POINT('Ctrl Pts',(6.859373891,3.176256335,-2.359382433));
#106320=CARTESIAN_POINT('Ctrl Pts',(6.775802451,3.214285714,-2.578953498));
#106321=CARTESIAN_POINT('Ctrl Pts',(6.717780663,3.240688665,-2.731396796));
#106322=CARTESIAN_POINT('Ctrl Pts',(6.65296165500001,3.267335925,-2.881076398));
#106323=CARTESIAN_POINT('Ctrl Pts',(6.65137768002123,3.26798710116569,-2.88473410199325));
#106324=CARTESIAN_POINT('Ctrl Pts',(6.64979370504246,3.26863827733136,-2.88839180598651));
#106325=CARTESIAN_POINT('',(6.97641624536787,3.26733592550877,-2.75311030322799));
#106326=CARTESIAN_POINT('',(6.81468895436952,3.26733592642396,-2.81709334334895));
#106327=CARTESIAN_POINT('',(7.16550684269047,3.17766594629366,-2.21483897554283));
#106328=CARTESIAN_POINT('Ctrl Pts',(6.97641624723878,3.26733592483409,-2.75311030408086));
#106329=CARTESIAN_POINT('Ctrl Pts',(7.01779331252057,3.24953506265028,-2.64826029694357));
#106330=CARTESIAN_POINT('Ctrl Pts',(7.05672145986858,3.23184317427123,-2.54269001880757));
#106331=CARTESIAN_POINT('Ctrl Pts',(7.09317466455715,3.21428571386188,-2.43656996049252));
#106332=CARTESIAN_POINT('Ctrl Pts',(7.1183905582333,3.20214063482658,-2.36316318632796));
#106333=CARTESIAN_POINT('Ctrl Pts',(7.14251079594586,3.18993125789227,-2.28923640648229));
#106334=CARTESIAN_POINT('Ctrl Pts',(7.16550684258656,3.17766594608544,-2.21483897554504));
#106335=CARTESIAN_POINT('Ctrl Pts',(6.92715057363297,3.13852541810399,-2.13941228615809));
#106336=CARTESIAN_POINT('Ctrl Pts',(6.96682809446975,3.14538568954085,-2.15192905489883));
#106337=CARTESIAN_POINT('Ctrl Pts',(7.00655215970945,3.15207183487632,-2.16448113043638));
#106338=CARTESIAN_POINT('Ctrl Pts',(7.0859908302513,3.1651074164565,-2.18962014877943));
#106339=CARTESIAN_POINT('Ctrl Pts',(7.12575199162475,3.17146448709542,-2.20222182647878));
#106340=CARTESIAN_POINT('Ctrl Pts',(7.16550684231213,3.17766594629071,-2.21483897673639));
#106341=CARTESIAN_POINT('Ctrl Pts',(7.3130761865187,3.26861999521842,-1.6640258809411));
#106342=CARTESIAN_POINT('Ctrl Pts',(7.31217452525935,3.26797796010921,-1.66796884697055));
#106343=CARTESIAN_POINT('Ctrl Pts',(7.311272864,3.267335925,-1.671911813));
#106344=CARTESIAN_POINT('Ctrl Pts',(7.220743665,3.202873885,-2.067796135));
#106345=CARTESIAN_POINT('Ctrl Pts',(7.087997104,3.137747733,-2.45159072));
#106346=CARTESIAN_POINT('Ctrl Pts',(7.11825764338814,3.26861999521842,-1.37585220051464));
#106347=CARTESIAN_POINT('Ctrl Pts',(7.11751150719407,3.26797796010921,-1.37969026875732));
#106348=CARTESIAN_POINT('Ctrl Pts',(7.116765371,3.267335925,-1.383528337));
#106349=CARTESIAN_POINT('Ctrl Pts',(7.041851304,3.202873885,-1.768880641));
#106350=CARTESIAN_POINT('Ctrl Pts',(6.925765802,3.137747733,-2.143890869));
#106351=CARTESIAN_POINT('',(7.311272846636,3.26733592582707,-1.67191180663589));
#106352=CARTESIAN_POINT('Origin',(-0.176434910672402,3.08932519130311,0.0693646279067664));
#106353=CARTESIAN_POINT('',(7.21401911446167,3.26733592735558,-1.52772008934729));
#106354=CARTESIAN_POINT('Origin',(2.17274115366095E-13,3.3580638,2.1467203015213E-14));
#106355=CARTESIAN_POINT('',(7.16488840922633,3.35698786819358,-2.2168387593173));
#106356=CARTESIAN_POINT('Origin',(-0.15805117081004,3.08947605520507,0.0927747698938322));
#106357=CARTESIAN_POINT('Origin',(-0.172058993564836,3.48205904216641,0.0741718257471044));
#106358=CARTESIAN_POINT('Ctrl Pts',(7.490838891,3.13774478,-0.370584287));
#106359=CARTESIAN_POINT('Ctrl Pts',(7.47883004200001,3.176256335,-0.613326232999999));
#106360=CARTESIAN_POINT('Ctrl Pts',(7.4511307,3.214285714,-0.854781429));
#106361=CARTESIAN_POINT('Ctrl Pts',(7.43189966400001,3.240688665,-1.022418391));
#106362=CARTESIAN_POINT('Ctrl Pts',(7.405148846,3.267335925,-1.189020844));
#106363=CARTESIAN_POINT('Ctrl Pts',(7.40449513919885,3.26798710116569,-1.19309208984433));
#106364=CARTESIAN_POINT('Ctrl Pts',(7.40384143239769,3.26863827733136,-1.19716333568867));
#106365=CARTESIAN_POINT('Ctrl Pts',(7.225500794,3.13774478,-0.595515139));
#106366=CARTESIAN_POINT('Ctrl Pts',(7.206203021,3.176256335,-0.829658758));
#106367=CARTESIAN_POINT('Ctrl Pts',(7.171786724,3.214285714,-1.062061763));
#106368=CARTESIAN_POINT('Ctrl Pts',(7.147892255,3.240688665,-1.22341399));
#106369=CARTESIAN_POINT('Ctrl Pts',(7.11676537100001,3.267335925,-1.383528337));
#106370=CARTESIAN_POINT('Ctrl Pts',(7.11600472675467,3.26798710116569,-1.38744103371067));
#106371=CARTESIAN_POINT('Ctrl Pts',(7.11524408250935,3.26863827733136,-1.39135373042133));
#106372=CARTESIAN_POINT('',(7.40514884403296,3.26733592550877,-1.18902084260647));
#106373=CARTESIAN_POINT('',(7.26095711003851,3.26733592642396,-1.28627458181517));
#106374=CARTESIAN_POINT('',(7.4741061843029,3.17766594634252,-0.62268511109573));
#106375=CARTESIAN_POINT('Ctrl Pts',(7.40514884603819,3.26733592483184,-1.18902084303671));
#106376=CARTESIAN_POINT('Ctrl Pts',(7.42301888672541,3.24953506265028,-1.07772732539843));
#106377=CARTESIAN_POINT('Ctrl Pts',(7.4383424264611,3.23184317427152,-0.966256820788148));
#106378=CARTESIAN_POINT('Ctrl Pts',(7.45113069970839,3.21428571391797,-0.854781428739896));
#106379=CARTESIAN_POINT('Ctrl Pts',(7.45997677357733,3.20214063494684,-0.777670192630329));
#106380=CARTESIAN_POINT('Ctrl Pts',(7.46764102080474,3.18993125793742,-0.700286641611116));
#106381=CARTESIAN_POINT('Ctrl Pts',(7.47410618425492,3.17766594614465,-0.622685111123001));
#106382=CARTESIAN_POINT('Ctrl Pts',(7.22510804351791,3.13852541809212,-0.600261407040693));
#106383=CARTESIAN_POINT('Ctrl Pts',(7.26654866655655,3.14538569039346,-0.603956047166329));
#106384=CARTESIAN_POINT('Ctrl Pts',(7.30804233656729,3.15207183664629,-0.607675163076698));
#106385=CARTESIAN_POINT('Ctrl Pts',(7.39102790432093,3.16510741562122,-0.615149477954107));
#106386=CARTESIAN_POINT('Ctrl Pts',(7.43256845399471,3.1714644854126,-0.618909060646346));
#106387=CARTESIAN_POINT('Ctrl Pts',(7.47410618419153,3.17766594633965,-0.622685112325538));
#106388=CARTESIAN_POINT('Ctrl Pts',(7.49981690556088,3.26861999521842,-0.0530266736009007));
#106389=CARTESIAN_POINT('Ctrl Pts',(7.49978394578045,3.26797796010921,-0.0570712858004503));
#106390=CARTESIAN_POINT('Ctrl Pts',(7.49975098600001,3.267335925,-0.061115898));
#106391=CARTESIAN_POINT('Ctrl Pts',(7.496441736,3.202873885,-0.467205767));
#106392=CARTESIAN_POINT('Ctrl Pts',(7.449303207,3.137747733,-0.870564034));
#106393=CARTESIAN_POINT('Ctrl Pts',(7.24760428844329,3.26861999521842,0.186529438107579));
#106394=CARTESIAN_POINT('Ctrl Pts',(7.24770066772165,3.26797796010921,0.182620704553789));
#106395=CARTESIAN_POINT('Ctrl Pts',(7.247797047,3.267335925,0.178711971));
#106396=CARTESIAN_POINT('Ctrl Pts',(7.257473784,3.202873885,-0.213735319));
#106397=CARTESIAN_POINT('Ctrl Pts',(7.22471841,3.137747733,-0.604932968));
#106398=CARTESIAN_POINT('',(7.49975096769167,3.26733592582611,-0.0611158955104157));
#106399=CARTESIAN_POINT('Origin',(-0.187221419669709,3.08932515470111,0.0298146441256785));
#106400=CARTESIAN_POINT('',(7.3737740166168,3.26733592735283,0.0587980218521181));
#106401=CARTESIAN_POINT('Origin',(-3.85108611666851E-13,3.35806379999967,
-2.54651985262533E-14));
#106402=CARTESIAN_POINT('',(7.4739321038036,3.35698786820595,-0.624771086166611));
#106403=CARTESIAN_POINT('Origin',(-0.174300000169229,3.08947598391187,0.0566294523323047));
#106404=CARTESIAN_POINT('Origin',(-0.183981315399253,3.48205904876804,0.0354501451864496));
#106405=CARTESIAN_POINT('Ctrl Pts',(7.39537190800001,3.13774478,1.248388701));
#106406=CARTESIAN_POINT('Ctrl Pts',(7.435826162,3.176256335,1.008740379));
#106407=CARTESIAN_POINT('Ctrl Pts',(7.460680145,3.214285714,0.766975733));
#106408=CARTESIAN_POINT('Ctrl Pts',(7.477935712,3.240688665,0.599123926));
#106409=CARTESIAN_POINT('Ctrl Pts',(7.487624915,3.267335925,0.43066591));
#106410=CARTESIAN_POINT('Ctrl Pts',(7.48786168898945,3.26798710116569,0.42654931996645));
#106411=CARTESIAN_POINT('Ctrl Pts',(7.4880984629789,3.26863827733136,0.4224327299329));
#106412=CARTESIAN_POINT('Ctrl Pts',(7.184590752,3.13774478,0.971676760000001));
#106413=CARTESIAN_POINT('Ctrl Pts',(7.21607810799999,3.176256335,0.738858839));
#106414=CARTESIAN_POINT('Ctrl Pts',(7.23242622,3.214285714,0.5044908));
#106415=CARTESIAN_POINT('Ctrl Pts',(7.243776351,3.240688665,0.341774293));
#106416=CARTESIAN_POINT('Ctrl Pts',(7.247797047,3.267335925,0.178711971));
#106417=CARTESIAN_POINT('Ctrl Pts',(7.24789530030652,3.26798710116569,0.174727234948065));
#106418=CARTESIAN_POINT('Ctrl Pts',(7.24799355361303,3.26863827733136,0.170742498896129));
#106419=CARTESIAN_POINT('',(7.48762491278461,3.26733592550878,0.430665910956628));
#106420=CARTESIAN_POINT('',(7.36771098063556,3.26733592642396,0.304688949312516));
#106421=CARTESIAN_POINT('',(7.43322462765509,3.17766594627913,0.998584817437513));
#106422=CARTESIAN_POINT('Ctrl Pts',(7.48762491482875,3.26733592482897,0.430665910966661));
#106423=CARTESIAN_POINT('Ctrl Pts',(7.48115234803168,3.24953506265028,0.543198978936239));
#106424=CARTESIAN_POINT('Ctrl Pts',(7.47215476859609,3.23184317427177,0.655357473301201));
#106425=CARTESIAN_POINT('Ctrl Pts',(7.46068014479904,3.21428571396803,0.766975732996196));
#106426=CARTESIAN_POINT('Ctrl Pts',(7.45274276608358,3.20214063500042,0.844185795256662));
#106427=CARTESIAN_POINT('Ctrl Pts',(7.443592651207,3.18993125788061,0.921407748626982));
#106428=CARTESIAN_POINT('Ctrl Pts',(7.43322462755758,3.17766594606887,0.998584817391001));
#106429=CARTESIAN_POINT('Ctrl Pts',(7.18522749154915,3.1385254181464,0.966957027476661));
#106430=CARTESIAN_POINT('Ctrl Pts',(7.22649349814379,3.14538569106813,0.972257275447814));
#106431=CARTESIAN_POINT('Ctrl Pts',(7.26781657356803,3.15207183795633,0.977545023491235));
#106432=CARTESIAN_POINT('Ctrl Pts',(7.35046873326897,3.16510741557627,0.988084897019536));
#106433=CARTESIAN_POINT('Ctrl Pts',(7.39184628693084,3.17146448532406,0.993343201591113));
#106434=CARTESIAN_POINT('Ctrl Pts',(7.43322462781404,3.17766594627615,0.998584816186248));
#106435=CARTESIAN_POINT('Ctrl Pts',(7.3358745212548,3.26861999521842,1.56045200257577));
#106436=CARTESIAN_POINT('Ctrl Pts',(7.3367118041274,3.26797796010921,1.55649486578788));
#106437=CARTESIAN_POINT('Ctrl Pts',(7.337549087,3.267335925,1.552537729));
#106438=CARTESIAN_POINT('Ctrl Pts',(7.421614524,3.202873885,1.155230625));
#106439=CARTESIAN_POINT('Ctrl Pts',(7.462288171,3.137747733,0.751169259));
#106440=CARTESIAN_POINT('Ctrl Pts',(7.03806101166501,3.26861999521842,1.74018916767838));
#106441=CARTESIAN_POINT('Ctrl Pts',(7.0389953998325,3.26797796010921,1.73639253683919));
#106442=CARTESIAN_POINT('Ctrl Pts',(7.039929788,3.267335925,1.732595906));
#106443=CARTESIAN_POINT('Ctrl Pts',(7.133744856,3.202873885,1.351404028));
#106444=CARTESIAN_POINT('Ctrl Pts',(7.185851215,3.137747733,0.962310925));
#106445=CARTESIAN_POINT('',(7.33754906858522,3.26733592582611,1.55253772749335));
#106446=CARTESIAN_POINT('Origin',(-0.189253261452819,3.08932519143167,-0.0111294346502501));
#106447=CARTESIAN_POINT('',(7.18873944076293,3.26733592735283,1.64256680321968));
#106448=CARTESIAN_POINT('Origin',(6.80878964320897E-14,3.35806379999933,
7.99057001121817E-14));
#106449=CARTESIAN_POINT('',(7.43350303965737,3.35698786821069,0.996510189375122));
#106450=CARTESIAN_POINT('Origin',(-0.18239831389786,3.08947604963738,0.0178361568675284));
#106451=CARTESIAN_POINT('Origin',(-0.187300472847888,3.48205906456362,-0.0049291658198608));
#106452=CARTESIAN_POINT('Ctrl Pts',(6.954105553,3.13774478,2.808988422));
#106453=CARTESIAN_POINT('Ctrl Pts',(7.045131315,3.176256335,2.583639413));
#106454=CARTESIAN_POINT('Ctrl Pts',(7.121376478,3.214285714,2.352869961));
#106455=CARTESIAN_POINT('Ctrl Pts',(7.174311796,3.240688665,2.192651873));
#106456=CARTESIAN_POINT('Ctrl Pts',(7.219987966,3.267335925,2.030215204));
#106457=CARTESIAN_POINT('Ctrl Pts',(7.22110414954922,3.26798710116569,2.0262457569617));
#106458=CARTESIAN_POINT('Ctrl Pts',(7.22222033309843,3.26863827733136,2.02227630992341));
#106459=CARTESIAN_POINT('Ctrl Pts',(6.807737232,3.13774478,2.493434134));
#106460=CARTESIAN_POINT('Ctrl Pts',(6.888537402,3.176256335,2.272828217));
#106461=CARTESIAN_POINT('Ctrl Pts',(6.954885505,3.214285714,2.047453934));
#106462=CARTESIAN_POINT('Ctrl Pts',(7.000949515,3.240688665,1.890981591));
#106463=CARTESIAN_POINT('Ctrl Pts',(7.039929788,3.267335925,1.732595906));
#106464=CARTESIAN_POINT('Ctrl Pts',(7.0408823446497,3.26798710116569,1.72872545241275));
#106465=CARTESIAN_POINT('Ctrl Pts',(7.04183490129941,3.26863827733136,1.7248549988255));
#106466=CARTESIAN_POINT('',(7.21998796362802,3.26733592550877,2.03021520441968));
#106467=CARTESIAN_POINT('',(7.12995887474965,3.26733592642396,1.88140556352814));
#106468=CARTESIAN_POINT('',(7.04477374845227,3.17766594629653,2.57316202957168));
#106469=CARTESIAN_POINT('Ctrl Pts',(7.2199879656346,3.26733592483455,2.03021520487331));
#106470=CARTESIAN_POINT('Ctrl Pts',(7.18947543979791,3.24953506265028,2.13872590177304));
#106471=CARTESIAN_POINT('Ctrl Pts',(7.15657745751694,3.23184317427162,2.24632797920249));
#106472=CARTESIAN_POINT('Ctrl Pts',(7.12137647774863,3.21428571393803,2.35286996114285));
#106473=CARTESIAN_POINT('Ctrl Pts',(7.09702678946891,3.20214063496177,2.42656859355009));
#106474=CARTESIAN_POINT('Ctrl Pts',(7.07149016196026,3.18993125790088,2.50001813618026));
#106475=CARTESIAN_POINT('Ctrl Pts',(7.04477374840842,3.17766594609248,2.57316202952145));
#106476=CARTESIAN_POINT('Ctrl Pts',(6.80937368739756,3.13852541803299,2.48896162643405));
#106477=CARTESIAN_POINT('Ctrl Pts',(6.84853550984038,3.14538568902674,2.50300892517016));
#106478=CARTESIAN_POINT('Ctrl Pts',(6.88775575239195,3.1520718339132,2.51705628372973));
#106479=CARTESIAN_POINT('Ctrl Pts',(6.96620981330809,3.16510741556216,2.54511752053223));
#106480=CARTESIAN_POINT('Ctrl Pts',(7.00548960277271,3.17146448533082,2.5591478397402));
#106481=CARTESIAN_POINT('Ctrl Pts',(7.04477374887695,3.17766594629358,2.57316202838253));
#106482=CARTESIAN_POINT('Ctrl Pts',(6.82891479781365,3.26861999521842,3.10096567712822));
#106483=CARTESIAN_POINT('Ctrl Pts',(6.83058317290683,3.26797796010921,3.09728104706411));
#106484=CARTESIAN_POINT('Ctrl Pts',(6.832251548,3.267335925,3.093596417));
#106485=CARTESIAN_POINT('Ctrl Pts',(6.999760864,3.202873885,2.723649716));
#106486=CARTESIAN_POINT('Ctrl Pts',(7.126344834,3.137747733,2.337778712));
#106487=CARTESIAN_POINT('Ctrl Pts',(6.49942582582478,3.26861999521842,3.21247958576346));
#106488=CARTESIAN_POINT('Ctrl Pts',(6.5011545319124,3.26797796010921,3.20897258388173));
#106489=CARTESIAN_POINT('Ctrl Pts',(6.502883238,3.267335925,3.205465582));
#106490=CARTESIAN_POINT('Ctrl Pts',(6.676449947,3.202873885,2.853353225));
#106491=CARTESIAN_POINT('Ctrl Pts',(6.810981603,3.137747733,2.48455823));
#106492=CARTESIAN_POINT('',(6.83225153036765,3.26733592582623,3.09359641153269));
#106493=CARTESIAN_POINT('Origin',(-0.182436357475877,3.08932519069727,-0.0515531776573969));
#106494=CARTESIAN_POINT('',(6.66756739925649,3.26733592735283,3.14953098625499));
#106495=CARTESIAN_POINT('Origin',(8.76035355368288E-14,3.35806379999989,
1.7130394325271E-14));
#106496=CARTESIAN_POINT('',(7.04549163559553,3.35698786820739,2.57119575562601));
#106497=CARTESIAN_POINT('Origin',(-0.181968764875183,3.08947600358288,-0.0217912721665592));
#106498=CARTESIAN_POINT('Origin',(-0.181861914083051,3.48205904784782,-0.0450780114584393));
#106499=CARTESIAN_POINT('Ctrl Pts',(6.187672952,3.13774478,4.238242965));
#106500=CARTESIAN_POINT('Ctrl Pts',(6.325013958,3.176256335,4.03773034));
#106501=CARTESIAN_POINT('Ctrl Pts',(6.449085162,3.214285714,3.828746606));
#106502=CARTESIAN_POINT('Ctrl Pts',(6.53522503500001,3.240688665,3.683653856));
#106503=CARTESIAN_POINT('Ctrl Pts',(6.614752403,3.267335925,3.534833892));
#106504=CARTESIAN_POINT('Ctrl Pts',(6.61669580455652,3.26798710116569,3.53119719488613));
#106505=CARTESIAN_POINT('Ctrl Pts',(6.61863920611304,3.26863827733136,3.52756049777226));
#106506=CARTESIAN_POINT('Ctrl Pts',(6.112561485,3.13774478,3.898601299));
#106507=CARTESIAN_POINT('Ctrl Pts',(6.238896343,3.176256335,3.700522674));
#106508=CARTESIAN_POINT('Ctrl Pts',(6.352142073,3.214285714,3.494680397));
#106509=CARTESIAN_POINT('Ctrl Pts',(6.43076606,3.240688665,3.351768692));
#106510=CARTESIAN_POINT('Ctrl Pts',(6.502883238,3.267335925,3.205465582));
#106511=CARTESIAN_POINT('Ctrl Pts',(6.50464555755743,3.26798710116569,3.20189038897088));
#106512=CARTESIAN_POINT('Ctrl Pts',(6.50640787711486,3.26863827733136,3.19831519594175));
#106513=CARTESIAN_POINT('',(6.61475240058954,3.26733592550878,3.53483389192562));
#106514=CARTESIAN_POINT('',(6.55881781646897,3.26733592642396,3.370149744845));
#106515=CARTESIAN_POINT('',(6.32691707896555,3.17766594633841,4.02742104519011));
#106516=CARTESIAN_POINT('Ctrl Pts',(6.61475240244418,3.2673359248308,3.53483389279533));
#106517=CARTESIAN_POINT('Ctrl Pts',(6.56162665075058,3.24953506265028,3.63424837905445));
#106518=CARTESIAN_POINT('Ctrl Pts',(6.50636653917648,3.23184317427181,3.73226268627465));
#106519=CARTESIAN_POINT('Ctrl Pts',(6.44908516185502,3.21428571397487,3.82874660592103));
#106520=CARTESIAN_POINT('Ctrl Pts',(6.40946172851625,3.20214063504681,3.89548774174869));
#106521=CARTESIAN_POINT('Ctrl Pts',(6.36873265250859,3.18993125794093,3.96173045481968));
#106522=CARTESIAN_POINT('Ctrl Pts',(6.32691707897758,3.17766594614415,4.02742104516149));
#106523=CARTESIAN_POINT('Ctrl Pts',(6.11512113831487,3.13852541809098,3.89458514643187));
#106524=CARTESIAN_POINT('Ctrl Pts',(6.15034763687084,3.14538569136909,3.91672266857401));
#106525=CARTESIAN_POINT('Ctrl Pts',(6.18563117853984,3.15207183861718,3.9388728088184));
#106526=CARTESIAN_POINT('Ctrl Pts',(6.25621867002753,3.16510741645027,3.98314328041782));
#106527=CARTESIAN_POINT('Ctrl Pts',(6.2915640212103,3.17146448710136,4.0052895754468));
#106528=CARTESIAN_POINT('Ctrl Pts',(6.3269170796288,3.17766594633554,4.02742104413145));
#106529=CARTESIAN_POINT('Ctrl Pts',(6.00264260807393,3.26861999521841,4.49648164327883));
#106530=CARTESIAN_POINT('Ctrl Pts',(6.00506406403696,3.26797796010921,4.49324180913942));
#106531=CARTESIAN_POINT('Ctrl Pts',(6.00748552,3.267335925,4.490001975));
#106532=CARTESIAN_POINT('Ctrl Pts',(6.250606167,3.202873885,4.164713973));
#106533=CARTESIAN_POINT('Ctrl Pts',(6.457181533,3.137747733,3.815076231));
#106534=CARTESIAN_POINT('Ctrl Pts',(5.65688471072712,3.26861999521841,4.53455802985732));
#106535=CARTESIAN_POINT('Ctrl Pts',(5.65932690236356,3.26797796010921,4.53150464042866));
#106536=CARTESIAN_POINT('Ctrl Pts',(5.66176909400001,3.267335925,4.528451251));
#106537=CARTESIAN_POINT('Ctrl Pts',(5.906971658,3.202873885,4.221882796));
#106538=CARTESIAN_POINT('Ctrl Pts',(6.117638062,3.137747733,3.890630353));
#106539=CARTESIAN_POINT('',(6.00748550389026,3.26733592582694,4.49000196590072));
#106540=CARTESIAN_POINT('Origin',(-0.167088647873811,3.08932514333194,-0.0895662798971653));
#106541=CARTESIAN_POINT('',(5.8346273159664,3.26733592735517,4.50922660139811));
#106542=CARTESIAN_POINT('Origin',(-8.46545056276682E-13,3.35806380000011,
-5.56846235788555E-13));
#106543=CARTESIAN_POINT('',(6.32804087305524,3.35698786821253,4.0256550662547));
#106544=CARTESIAN_POINT('Origin',(-0.173029777855969,3.08947603555603,-0.0603996013206703));
#106545=CARTESIAN_POINT('Origin',(-0.167919645100388,3.48205903152799,-0.0831190532386661));
#106546=CARTESIAN_POINT('Ctrl Pts',(5.131911641,3.13774478,5.469321979));
#106547=CARTESIAN_POINT('Ctrl Pts',(5.30914597800001,3.176256335,5.303021483));
#106548=CARTESIAN_POINT('Ctrl Pts',(5.475241792,3.214285714,5.125595314));
#106549=CARTESIAN_POINT('Ctrl Pts',(5.59055841400001,3.240688665,5.002412278));
#106550=CARTESIAN_POINT('Ctrl Pts',(5.70021837,3.267335925,4.874167676));
#106551=CARTESIAN_POINT('Ctrl Pts',(5.70289811829972,3.26798710116569,4.87103377674732));
#106552=CARTESIAN_POINT('Ctrl Pts',(5.70557786659942,3.26863827733136,4.86789987749465));
#106553=CARTESIAN_POINT('Ctrl Pts',(5.131569157,3.13774478,5.121474201));
#106554=CARTESIAN_POINT('Ctrl Pts',(5.297531425,3.176256335,4.95518480299999));
#106555=CARTESIAN_POINT('Ctrl Pts',(5.452379538,3.214285714,4.77849949));
#106556=CARTESIAN_POINT('Ctrl Pts',(5.559887133,3.240688665,4.655830813));
#106557=CARTESIAN_POINT('Ctrl Pts',(5.661769094,3.267335925,4.52845125000001));
#106558=CARTESIAN_POINT('Ctrl Pts',(5.66425877229023,3.26798710116569,4.52533848961035));
#106559=CARTESIAN_POINT('Ctrl Pts',(5.66674845058047,3.26863827733136,4.5222257292207));
#106560=CARTESIAN_POINT('',(5.7002183676652,3.26733592550878,4.87416767540058));
#106561=CARTESIAN_POINT('',(5.68099372637676,3.26733592642396,4.70130946979503));
#106562=CARTESIAN_POINT('',(5.31322079860285,3.17766594630138,5.2933623289354));
#106563=CARTESIAN_POINT('Ctrl Pts',(5.7002183692918,3.26733592483215,4.87416767665088));
#106564=CARTESIAN_POINT('Ctrl Pts',(5.62696349193861,3.24953506265028,4.95983744082131));
#106565=CARTESIAN_POINT('Ctrl Pts',(5.55192515245494,3.23184317427144,5.04368093738522));
#106566=CARTESIAN_POINT('Ctrl Pts',(5.47524179152958,3.21428571390225,5.12559531379616));
#106567=CARTESIAN_POINT('Ctrl Pts',(5.4221973602718,3.2021406349187,5.18225821197392));
#106568=CARTESIAN_POINT('Ctrl Pts',(5.3681802826392,3.18993125792519,5.23819666005832));
#106569=CARTESIAN_POINT('Ctrl Pts',(5.3132207986748,3.17766594611117,5.29336232896479));
#106570=CARTESIAN_POINT('Ctrl Pts',(5.13493232101444,3.13852541806714,5.11810219227241));
#106571=CARTESIAN_POINT('Ctrl Pts',(5.16457633453219,3.14538569225177,5.1472948114721));
#106572=CARTESIAN_POINT('Ctrl Pts',(5.19427334580649,3.15207184046988,5.17651201696921));
#106573=CARTESIAN_POINT('Ctrl Pts',(5.25369368567045,3.1651074155469,5.23492168157518));
#106574=CARTESIAN_POINT('Ctrl Pts',(5.28345187892572,3.17146448529656,5.26414840986732));
#106575=CARTESIAN_POINT('Ctrl Pts',(5.31322079949224,3.17766594629473,5.29336232799384));
#106576=CARTESIAN_POINT('Ctrl Pts',(4.89569352152841,3.26861999521842,5.68174712431132));
#106577=CARTESIAN_POINT('Ctrl Pts',(4.89875483376421,3.26797796010921,5.67910357715566));
#106578=CARTESIAN_POINT('Ctrl Pts',(4.901816146,3.267335925,5.67646003));
#106579=CARTESIAN_POINT('Ctrl Pts',(5.209180072,3.202873885,5.411040834));
#106580=CARTESIAN_POINT('Ctrl Pts',(5.4860876,3.137747733,5.113985026));
#106581=CARTESIAN_POINT('Ctrl Pts',(4.54983395395533,3.26861999521842,5.64460557872374));
#106582=CARTESIAN_POINT('Ctrl Pts',(4.55287543697766,3.26797796010921,5.64214857486187));
#106583=CARTESIAN_POINT('Ctrl Pts',(4.55591692,3.267335925,5.639691571));
#106584=CARTESIAN_POINT('Ctrl Pts',(4.86128994,3.202873885,5.39300182));
#106585=CARTESIAN_POINT('Ctrl Pts',(5.138240564,3.137747733,5.114780924));
#106586=CARTESIAN_POINT('',(4.90181613226231,3.26733592582611,5.67646001765269));
#106587=CARTESIAN_POINT('Origin',(-0.143928092233303,3.08932515400138,-0.123391387392208));
#106588=CARTESIAN_POINT('',(4.72886654423971,3.26733592735283,5.65807579110616));
#106589=CARTESIAN_POINT('Origin',(2.1987620058006E-13,3.35806380000022,
2.23345647532014E-13));
#106590=CARTESIAN_POINT('',(5.31469795204853,3.35698786817063,5.29187921992739));
#106591=CARTESIAN_POINT('Origin',(-0.156000037174683,3.0894760332274,-0.0961835375372055));
#106592=CARTESIAN_POINT('Origin',(-0.146125483290186,3.48205904005493,-0.117273373961345));
#106593=CARTESIAN_POINT('Ctrl Pts',(3.836187846,3.13774478,6.444661575));
#106594=CARTESIAN_POINT('Ctrl Pts',(4.045028233,3.176256335,6.320349236));
#106595=CARTESIAN_POINT('Ctrl Pts',(4.2453822,3.214285714,6.182776882));
#106596=CARTESIAN_POINT('Ctrl Pts',(4.384483496,3.240688665,6.087263462));
#106597=CARTESIAN_POINT('Ctrl Pts',(4.519148461,3.267335925,5.985590797));
#106598=CARTESIAN_POINT('Ctrl Pts',(4.52243925395809,3.26798710116569,5.98310623325313));
#106599=CARTESIAN_POINT('Ctrl Pts',(4.52573004691619,3.26863827733136,5.98062166950626));
#106600=CARTESIAN_POINT('Ctrl Pts',(3.910630358,3.13774478,6.104872661));
#106601=CARTESIAN_POINT('Ctrl Pts',(4.108459826,3.176256335,5.978147999));
#106602=CARTESIAN_POINT('Ctrl Pts',(4.297669796,3.214285714,5.838881257));
#106603=CARTESIAN_POINT('Ctrl Pts',(4.429034062,3.240688665,5.74219146));
#106604=CARTESIAN_POINT('Ctrl Pts',(4.55591692,3.267335925,5.639691571));
#106605=CARTESIAN_POINT('Ctrl Pts',(4.55901754246412,3.26798710116569,5.6371867924711));
#106606=CARTESIAN_POINT('Ctrl Pts',(4.56211816492825,3.26863827733136,5.63468201394221));
#106607=CARTESIAN_POINT('',(4.5191484588534,3.26733592550877,5.9855907959051));
#106608=CARTESIAN_POINT('',(4.5375326835475,3.26733592642396,5.81264118942734));
#106609=CARTESIAN_POINT('',(4.05108421901788,3.17766594629334,6.31179187331946));
#106610=CARTESIAN_POINT('Ctrl Pts',(4.51914846017482,3.26733592483341,5.9855907974783));
#106611=CARTESIAN_POINT('Ctrl Pts',(4.42918977470013,3.24953506265028,6.05351001663708));
#106612=CARTESIAN_POINT('Ctrl Pts',(4.33788191641198,3.23184317427191,6.11926227378783));
#106613=CARTESIAN_POINT('Ctrl Pts',(4.24538220000967,3.2142857139959,6.18277688180928));
#106614=CARTESIAN_POINT('Ctrl Pts',(4.18139707048148,3.20214063507977,6.22671204840464));
#106615=CARTESIAN_POINT('Ctrl Pts',(4.11661776882006,3.18993125792659,6.26973061157319));
#106616=CARTESIAN_POINT('Ctrl Pts',(4.05108421910799,3.17766594610806,6.31179187340583));
#106617=CARTESIAN_POINT('Ctrl Pts',(3.91463977526643,3.13852541808699,6.10230246946549));
#106618=CARTESIAN_POINT('Ctrl Pts',(3.93731515698753,3.14538568580912,6.13718513501166));
#106619=CARTESIAN_POINT('Ctrl Pts',(3.96003700862289,3.15207182728962,6.17210320009783));
#106620=CARTESIAN_POINT('Ctrl Pts',(4.00551183172567,3.16510741638777,6.24192097074481));
#106621=CARTESIAN_POINT('Ctrl Pts',(4.02829141568943,3.17146448702112,6.2768615314487));
#106622=CARTESIAN_POINT('Ctrl Pts',(4.05108422008695,3.17766594628283,6.31179187256125));
#106623=CARTESIAN_POINT('Ctrl Pts',(3.55982724710696,3.26861999521842,6.60134042570219));
#106624=CARTESIAN_POINT('Ctrl Pts',(3.56338527205348,3.26797796010921,6.5994167748511));
#106625=CARTESIAN_POINT('Ctrl Pts',(3.566943297,3.267335925,6.597493124));
#106626=CARTESIAN_POINT('Ctrl Pts',(3.924178506,3.202873885,6.40435344));
#106627=CARTESIAN_POINT('Ctrl Pts',(4.258470309,3.137747733,6.173769564));
#106628=CARTESIAN_POINT('Ctrl Pts',(3.2300380178948,3.26861999521842,6.49071764506209));
#106629=CARTESIAN_POINT('Ctrl Pts',(3.2335365759474,3.26797796010921,6.48897191353104));
#106630=CARTESIAN_POINT('Ctrl Pts',(3.237035134,3.267335925,6.487226182));
#106631=CARTESIAN_POINT('Ctrl Pts',(3.588299708,3.202873885,6.311950073));
#106632=CARTESIAN_POINT('Ctrl Pts',(3.918584648,3.137747733,6.099770025));
#106633=CARTESIAN_POINT('',(3.56694328621157,3.26733592582706,6.59749310897334));
#106634=CARTESIAN_POINT('Origin',(-0.114037627145149,3.08932521420518,-0.151446856230543));
#106635=CARTESIAN_POINT('',(3.40198922851141,3.26733592735556,6.54235964623415));
#106636=CARTESIAN_POINT('Origin',(-6.21464685268691E-13,3.35806379999967,
-9.96598636948676E-13));
#106637=CARTESIAN_POINT('',(4.05284566209122,3.35698786818625,6.31066098278468));
#106638=CARTESIAN_POINT('Origin',(-0.131676465737328,3.08947593480512,-0.127470530566424));
#106639=CARTESIAN_POINT('Origin',(-0.117498977325006,3.48205908444918,-0.145944454804838));
#106640=CARTESIAN_POINT('Ctrl Pts',(2.36108817,3.13774478,7.118655958));
#106641=CARTESIAN_POINT('Ctrl Pts',(2.591769463,3.176256335,7.042144483));
#106642=CARTESIAN_POINT('Ctrl Pts',(2.817013256,3.214285714,6.950858675));
#106643=CARTESIAN_POINT('Ctrl Pts',(2.973395002,3.240688665,6.887480972));
#106644=CARTESIAN_POINT('Ctrl Pts',(3.126768193,3.267335925,6.817134344));
#106645=CARTESIAN_POINT('Ctrl Pts',(3.13051615682195,3.26798710116569,6.81541529117844));
#106646=CARTESIAN_POINT('Ctrl Pts',(3.13426412064389,3.26863827733136,6.81369623835689));
#106647=CARTESIAN_POINT('Ctrl Pts',(2.50683483,3.13774478,6.80281406));
#106648=CARTESIAN_POINT('Ctrl Pts',(2.727281211,3.176256335,6.721579638));
#106649=CARTESIAN_POINT('Ctrl Pts',(2.94200579,3.214285714,6.626243425));
#106650=CARTESIAN_POINT('Ctrl Pts',(3.09108428,3.240688665,6.560053617));
#106651=CARTESIAN_POINT('Ctrl Pts',(3.237035134,3.267335925,6.487226182));
#106652=CARTESIAN_POINT('Ctrl Pts',(3.24060171898795,3.26798710116569,6.48544650597028));
#106653=CARTESIAN_POINT('Ctrl Pts',(3.24416830397589,3.26863827733136,6.48366682994055));
#106654=CARTESIAN_POINT('',(3.12676819112568,3.26733592550878,6.81713434248249));
#106655=CARTESIAN_POINT('',(3.18190165554333,3.26733592642396,6.65218026680587));
#106656=CARTESIAN_POINT('',(2.59952344355989,3.17766594625804,7.03508904441724));
#106657=CARTESIAN_POINT('Ctrl Pts',(3.12676819207577,3.26733592483072,6.81713434429708));
#106658=CARTESIAN_POINT('Ctrl Pts',(3.02431206592027,3.24953506265028,6.86412719177397));
#106659=CARTESIAN_POINT('Ctrl Pts',(2.92100414310148,3.23184317427142,6.90871370745156));
#106660=CARTESIAN_POINT('Ctrl Pts',(2.81701325564168,3.21428571389909,6.95085867462062));
#106661=CARTESIAN_POINT('Ctrl Pts',(2.74507930028266,3.20214063492807,6.98001174970034));
#106662=CARTESIAN_POINT('Ctrl Pts',(2.67256678374785,3.18993125793566,7.0080989278413));
#106663=CARTESIAN_POINT('Ctrl Pts',(2.59952344370808,3.17766594609591,7.03508904474461));
#106664=CARTESIAN_POINT('Ctrl Pts',(2.51130302491627,3.13852541819266,6.8011658645337));
#106665=CARTESIAN_POINT('Ctrl Pts',(2.5259495383277,3.1453856913761,6.84010756067898));
#106666=CARTESIAN_POINT('Ctrl Pts',(2.54063382725774,3.15207183853582,6.87909382298944));
#106667=CARTESIAN_POINT('Ctrl Pts',(2.57003669000114,3.16510741550788,6.95705496333845));
#106668=CARTESIAN_POINT('Ctrl Pts',(2.58477250992851,3.17146448518842,6.99607556414552));
#106669=CARTESIAN_POINT('Ctrl Pts',(2.59952344479365,3.17766594623031,7.03508904377181));
#106670=CARTESIAN_POINT('Ctrl Pts',(2.05750740624301,3.26861999521841,7.21226238556067));
#106671=CARTESIAN_POINT('Ctrl Pts',(2.06139577462151,3.26797796010921,7.21114857878034));
#106672=CARTESIAN_POINT('Ctrl Pts',(2.065284143,3.267335925,7.21003477200001));
#106673=CARTESIAN_POINT('Ctrl Pts',(2.455686715,3.202873885,7.098205596));
#106674=CARTESIAN_POINT('Ctrl Pts',(2.831731678,3.137747733,6.944875499));
#106675=CARTESIAN_POINT('Ctrl Pts',(1.7592090952449,3.26861999521841,7.03333096846917));
#106676=CARTESIAN_POINT('Ctrl Pts',(1.76300113962245,3.26797796010921,7.03237813773459));
#106677=CARTESIAN_POINT('Ctrl Pts',(1.766793184,3.267335925,7.031425307));
#106678=CARTESIAN_POINT('Ctrl Pts',(2.147524569,3.202873885,6.935758556));
#106679=CARTESIAN_POINT('Ctrl Pts',(2.51570007,3.137747733,6.799540658));
#106680=CARTESIAN_POINT('',(2.0652841356999,3.26733592582647,7.21003475501715));
#106681=CARTESIAN_POINT('Origin',(-0.0788149208579259,3.08932516908768,
-0.172420872875289));
#106682=CARTESIAN_POINT('',(1.91603867765137,3.26733592735385,7.12073003569217));
#106683=CARTESIAN_POINT('Origin',(2.68665298341908E-13,3.35806380000067,
6.44449771325384E-13));
#106684=CARTESIAN_POINT('',(2.6014868129463,3.35698786818497,7.03436325179611));
#106685=CARTESIAN_POINT('Origin',(-0.101195453104435,3.08947598274281,-0.1527966907843));
#106686=CARTESIAN_POINT('Origin',(-0.0833780850768881,3.48205905312549,
-0.167790905124618));
#106687=CARTESIAN_POINT('Ctrl Pts',(0.775586635,3.13774478,7.459789901));
#106688=CARTESIAN_POINT('Ctrl Pts',(1.017322434,3.176256335,7.43465688100001));
#106689=CARTESIAN_POINT('Ctrl Pts',(1.256923902,3.214285714,7.393926041));
#106690=CARTESIAN_POINT('Ctrl Pts',(1.423273863,3.240688665,7.365647527));
#106691=CARTESIAN_POINT('Ctrl Pts',(1.588183719,3.267335925,7.329916267));
#106692=CARTESIAN_POINT('Ctrl Pts',(1.59221360303736,3.26798710116569,7.3290431061241));
#106693=CARTESIAN_POINT('Ctrl Pts',(1.59624348707472,3.26863827733136,7.32816994524821));
#106694=CARTESIAN_POINT('Ctrl Pts',(0.985822492000001,3.13774478,7.182663435));
#106695=CARTESIAN_POINT('Ctrl Pts',(1.218577958,3.176256335,7.15071768400001));
#106696=CARTESIAN_POINT('Ctrl Pts',(1.448776863,3.214285714,7.103769816));
#106697=CARTESIAN_POINT('Ctrl Pts',(1.608598834,3.240688665,7.071174957));
#106698=CARTESIAN_POINT('Ctrl Pts',(1.766793184,3.267335925,7.031425307));
#106699=CARTESIAN_POINT('Ctrl Pts',(1.77065896195487,3.26798710116569,7.03045394916905));
#106700=CARTESIAN_POINT('Ctrl Pts',(1.77452473990974,3.26863827733136,7.02948259133811));
#106701=CARTESIAN_POINT('',(1.58818371752725,3.26733592550877,7.32991626509525));
#106702=CARTESIAN_POINT('',(1.6774884429112,3.26733592642396,7.18067078900645));
#106703=CARTESIAN_POINT('',(1.02641184128338,3.17766594629658,7.42943327122658));
#106704=CARTESIAN_POINT('Ctrl Pts',(1.58818371806689,3.26733592483612,7.32991626708421));
#106705=CARTESIAN_POINT('Ctrl Pts',(1.4780208864729,3.24953506265028,7.35378540900346));
#106706=CARTESIAN_POINT('Ctrl Pts',(1.3675434625844,3.23184317427187,7.3751213666415));
#106707=CARTESIAN_POINT('Ctrl Pts',(1.25692390201705,3.21428571398719,7.39392604086586));
#106708=CARTESIAN_POINT('Ctrl Pts',(1.18040467351101,3.20214063506812,7.40693385968585));
#106709=CARTESIAN_POINT('Ctrl Pts',(1.10354954581301,3.1899312579316,7.41877632737252));
#106710=CARTESIAN_POINT('Ctrl Pts',(1.02641184133089,3.17766594611356,7.42943327135974));
#106711=CARTESIAN_POINT('Ctrl Pts',(0.990540536095495,3.13852541801635,
7.18201430225601));
#106712=CARTESIAN_POINT('Ctrl Pts',(0.996473310127783,3.14538569321089,
7.2231941425004));
#106713=CARTESIAN_POINT('Ctrl Pts',(1.00243339650977,3.15207184247826,7.2644256295697));
#106714=CARTESIAN_POINT('Ctrl Pts',(1.01438949230819,3.16510741552789,7.34688480317291));
#106715=CARTESIAN_POINT('Ctrl Pts',(1.02039252128369,3.17146448527065,7.38816089009443));
#106716=CARTESIAN_POINT('Ctrl Pts',(1.0264118425723,3.17766594628502,7.42943327098007));
#106717=CARTESIAN_POINT('Ctrl Pts',(0.458980806959232,3.26861999521842,
7.48594697166454));
#106718=CARTESIAN_POINT('Ctrl Pts',(0.463017702979616,3.26797796010921,
7.48569508933226));
#106719=CARTESIAN_POINT('Ctrl Pts',(0.467054599,3.267335925,7.485443207));
#106720=CARTESIAN_POINT('Ctrl Pts',(0.872369743,3.202873885,7.460153548));
#106721=CARTESIAN_POINT('Ctrl Pts',(1.272584422,3.137747733,7.391246775));
#106722=CARTESIAN_POINT('Ctrl Pts',(0.206121509127987,3.26861999521842,
7.24707355226296));
#106723=CARTESIAN_POINT('Ctrl Pts',(0.210029728063993,3.26797796010921,
7.24695817563147));
#106724=CARTESIAN_POINT('Ctrl Pts',(0.213937947,3.267335925,7.246842799));
#106725=CARTESIAN_POINT('Ctrl Pts',(0.606333568,3.202873885,7.235258677));
#106726=CARTESIAN_POINT('Ctrl Pts',(0.995184151,3.137747733,7.181372327));
#106727=CARTESIAN_POINT('',(0.467054595523074,3.26733592582729,7.48544318882912));
#106728=CARTESIAN_POINT('Origin',(-0.0399068760955543,3.0893251625822,-0.185332644120294));
#106729=CARTESIAN_POINT('',(0.340496287653564,3.26733592735618,7.36614300232264));
#106730=CARTESIAN_POINT('Origin',(1.97107954957865E-13,3.35806379999933,
7.19476561661381E-13));
#106731=CARTESIAN_POINT('',(1.02848533195528,3.356987868206,7.42914651327288));
#106732=CARTESIAN_POINT('Origin',(-0.0659827140366118,3.08947603214728,
-0.170978110658462));
#106733=CARTESIAN_POINT('Origin',(-0.0453586688464361,3.48205903721848,
-0.181791902684507));
#106734=CARTESIAN_POINT('Origin',(-1.17935785378005E-13,3.35806379999978,
1.91860416443035E-12));
#106735=CARTESIAN_POINT('',(-0.0246624610395199,3.26733592550877,7.49995944882694));
#106736=CARTESIAN_POINT('Ctrl Pts',(-0.0246624565254798,3.26733592553159,
7.49995945089605));
#106737=CARTESIAN_POINT('Ctrl Pts',(-0.137380907419657,3.24953506265028,
7.49958879335285));
#106738=CARTESIAN_POINT('Ctrl Pts',(-0.249862030784193,3.23184317427147,
7.49667654792688));
#106739=CARTESIAN_POINT('Ctrl Pts',(-0.361937816335415,3.21428571390813,
7.49126164372827));
#106740=CARTESIAN_POINT('Ctrl Pts',(-0.439464363273653,3.20214063517061,
7.48751597453169));
#106741=CARTESIAN_POINT('Ctrl Pts',(-0.517068439202277,3.18993125839334,
7.48255999142523));
#106742=CARTESIAN_POINT('Ctrl Pts',(-0.594693633718237,3.17766594678636,
7.47638545586979));
#106743=CARTESIAN_POINT('',(-0.592606979416598,3.3569878682049,7.47655114140618));
#106744=CARTESIAN_POINT('Origin',(-0.027684826236559,3.08947596084301,-0.181165925910972));
#106745=CARTESIAN_POINT('Origin',(-0.00521827043682879,3.48205907355581,
-0.187292892979214));
#106746=CARTESIAN_POINT('Ctrl Pts',(-0.846180468000001,3.13774478,7.452112359));
#106747=CARTESIAN_POINT('Ctrl Pts',(-0.604693462,3.176256335,7.479532986));
#106748=CARTESIAN_POINT('Ctrl Pts',(-0.361937816,3.214285714,7.491261644));
#106749=CARTESIAN_POINT('Ctrl Pts',(-0.193397981,3.240688665,7.49940459));
#106750=CARTESIAN_POINT('Ctrl Pts',(-0.02466246,3.267335925,7.499959451));
#106751=CARTESIAN_POINT('Ctrl Pts',(-0.0205390886072463,3.26798710116569,
7.49997301007732));
#106752=CARTESIAN_POINT('Ctrl Pts',(-0.0164157172144926,3.26863827733136,
7.49998656915463));
#106753=CARTESIAN_POINT('Ctrl Pts',(-0.58128581,3.13774478,7.22665945000001));
#106754=CARTESIAN_POINT('Ctrl Pts',(-0.347104645,3.176256335,7.245496119));
#106755=CARTESIAN_POINT('Ctrl Pts',(-0.112195259,3.214285714,7.249131826));
#106756=CARTESIAN_POINT('Ctrl Pts',(0.050897094,3.240688665,7.251656016));
#106757=CARTESIAN_POINT('Ctrl Pts',(0.213937947,3.267335925,7.246842799));
#106758=CARTESIAN_POINT('Ctrl Pts',(0.21792215841634,3.26798710116569,7.24672517894485));
#106759=CARTESIAN_POINT('Ctrl Pts',(0.221906369832681,3.26863827733136,
7.24660755888971));
#106760=CARTESIAN_POINT('',(0.0946377346806782,3.26733592642396,7.3734011251132));
#106761=CARTESIAN_POINT('Ctrl Pts',(-0.037736949,2.490655005,7.49990506100001));
#106762=CARTESIAN_POINT('Ctrl Pts',(0.372864527,2.556411293,7.501971067));
#106763=CARTESIAN_POINT('Ctrl Pts',(0.781237513,2.621296797,7.459200222));
#106764=CARTESIAN_POINT('Ctrl Pts',(0.201304349,2.490655005,7.247204741));
#106765=CARTESIAN_POINT('Ctrl Pts',(0.598071101,2.556411293,7.23618382));
#106766=CARTESIAN_POINT('Ctrl Pts',(0.991263374999999,2.621296797,7.181914572));
#106767=CARTESIAN_POINT('',(0.206045683893195,2.49144077928712,7.2470715026123));
#106768=CARTESIAN_POINT('Origin',(0.0078834845902781,2.41076923579639,-0.195169088968804));
#106769=CARTESIAN_POINT('Ctrl Pts',(0.206045688489983,2.49144078088258,
7.24707150221496));
#106770=CARTESIAN_POINT('Ctrl Pts',(0.207247253803597,2.49833629958132,
7.28865974208964));
#106771=CARTESIAN_POINT('Ctrl Pts',(0.208471474059975,2.50506214895585,
7.33030086491627));
#106772=CARTESIAN_POINT('Ctrl Pts',(0.210958287707542,2.51818504852657,
7.41358339843687));
#106773=CARTESIAN_POINT('Ctrl Pts',(0.212222310116712,2.52458961896209,
7.45527257747634));
#106774=CARTESIAN_POINT('Ctrl Pts',(0.213503815207118,2.53084202106317,
7.49696045865912));
#106775=CARTESIAN_POINT('Ctrl Pts',(1.24150092168421,2.62578637474627,7.39711075669431));
#106776=CARTESIAN_POINT('Ctrl Pts',(1.25530842931597,2.62354158587314,7.39474029520798));
#106777=CARTESIAN_POINT('Ctrl Pts',(1.26911593694773,2.621296797,7.39236983372176));
#106778=CARTESIAN_POINT('Ctrl Pts',(1.67083202238252,2.555986835,7.32340354854394));
#106779=CARTESIAN_POINT('Ctrl Pts',(2.06270905602151,2.49066265,7.21131183416782));
#106780=CARTESIAN_POINT('Ctrl Pts',(0.9644345386314,2.62578637474628,7.18561754598309));
#106781=CARTESIAN_POINT('Ctrl Pts',(0.977848956815707,2.62354158587314,
7.18376605899156));
#106782=CARTESIAN_POINT('Ctrl Pts',(0.991263375,2.621296797,7.181914572));
#106783=CARTESIAN_POINT('Ctrl Pts',(1.381542903,2.555986835,7.128047348));
#106784=CARTESIAN_POINT('Ctrl Pts',(1.763686919,2.49066265,7.032205092));
#106785=CARTESIAN_POINT('Ctrl Pts',(0.961669527889655,2.62578637474628,
7.18350692905078));
#106786=CARTESIAN_POINT('Ctrl Pts',(0.97508002319983,2.62354158587314,7.18166062121545));
#106787=CARTESIAN_POINT('Ctrl Pts',(0.988490518509999,2.621296797,7.17981431338));
#106788=CARTESIAN_POINT('Ctrl Pts',(1.37865591428,2.555986835,7.12609777192));
#106789=CARTESIAN_POINT('Ctrl Pts',(1.76070279869,2.49066265,7.03041767896));
#106790=CARTESIAN_POINT('',(1.75913460167848,2.49144077991026,7.03334526603423));
#106791=CARTESIAN_POINT('Origin',(-0.038363327590185,2.5535712699457,-0.19584155044322));
#106792=CARTESIAN_POINT('Ctrl Pts',(1.82013710423508,2.53084202099787,7.2757886802893));
#106793=CARTESIAN_POINT('Ctrl Pts',(1.80992389783541,2.52458961887095,7.23535092406327));
#106794=CARTESIAN_POINT('Ctrl Pts',(1.79972748647046,2.51818504845322,7.1949081423779));
#106795=CARTESIAN_POINT('Ctrl Pts',(1.77939553036727,2.50506214886567,7.11410729951541));
#106796=CARTESIAN_POINT('Ctrl Pts',(1.76924832116017,2.49833629940387,7.07370289367457));
#106797=CARTESIAN_POINT('Ctrl Pts',(1.75913460568594,2.49144078071445,7.03334526489254));
#106798=CARTESIAN_POINT('Ctrl Pts',(1.575403212,2.490655005,7.332673777));
#106799=CARTESIAN_POINT('Ctrl Pts',(1.976849185,2.556411293,7.2464243));
#106800=CARTESIAN_POINT('Ctrl Pts',(2.36648017,2.621296797,7.11686529400001));
#106801=CARTESIAN_POINT('Ctrl Pts',(1.754532759,2.490655005,7.034494637));
#106802=CARTESIAN_POINT('Ctrl Pts',(2.139654152,2.556411293,6.93843825600001));
#106803=CARTESIAN_POINT('Ctrl Pts',(2.511987525,2.621296797,6.800913077));
#106804=CARTESIAN_POINT('Origin',(-0.0342563549590419,2.41076920033269,
-0.192300740412121));
#106805=CARTESIAN_POINT('Ctrl Pts',(2.80263547683302,2.62578637456442,6.95728441748718));
#106806=CARTESIAN_POINT('Ctrl Pts',(2.81561059294644,2.62354158578221,6.95200117027106));
#106807=CARTESIAN_POINT('Ctrl Pts',(2.82858570905987,2.621296797,6.94671792305479));
#106808=CARTESIAN_POINT('Ctrl Pts',(3.20608418331737,2.555986835,6.79300694691972));
#106809=CARTESIAN_POINT('Ctrl Pts',(3.56470294445959,2.49066265,6.59929389665742));
#106810=CARTESIAN_POINT('Ctrl Pts',(2.48658196293848,2.62578637456442,6.81029688395013));
#106811=CARTESIAN_POINT('Ctrl Pts',(2.49928474396925,2.62354158578221,6.80560498047508));
#106812=CARTESIAN_POINT('Ctrl Pts',(2.511987525,2.621296797,6.800913077));
#106813=CARTESIAN_POINT('Ctrl Pts',(2.881562673,2.555986835,6.664406676));
#106814=CARTESIAN_POINT('Ctrl Pts',(3.234169123,2.49066265,6.488655491));
#106815=CARTESIAN_POINT('Ctrl Pts',(2.48342787635703,2.62578637456442,6.80883000765624));
#106816=CARTESIAN_POINT('Ctrl Pts',(2.49612793959352,2.62354158578221,6.80414400555304));
#106817=CARTESIAN_POINT('Ctrl Pts',(2.50882800283,2.621296797,6.79945800345));
#106818=CARTESIAN_POINT('Ctrl Pts',(2.87832407923,2.555986835,6.66312329717));
#106819=CARTESIAN_POINT('Ctrl Pts',(3.23087052879,2.49066265,6.48755136434));
#106820=CARTESIAN_POINT('',(3.22996834025018,2.49144077989572,6.49074762261724));
#106821=CARTESIAN_POINT('Origin',(-0.079566625270621,2.55357127829657,-0.183016063847826));
#106822=CARTESIAN_POINT('Ctrl Pts',(3.34166280629982,2.53084202104486,6.71440910928901));
#106823=CARTESIAN_POINT('Ctrl Pts',(3.32299542484375,2.5245896082431,6.6771122392648));
#106824=CARTESIAN_POINT('Ctrl Pts',(3.30434341444964,2.51818504331344,6.63980694869523));
#106825=CARTESIAN_POINT('Ctrl Pts',(3.26711702995851,2.50506214888135,6.56526598359231));
#106826=CARTESIAN_POINT('Ctrl Pts',(3.24852130392302,2.49833629942832,6.52798756039885));
#106827=CARTESIAN_POINT('Ctrl Pts',(3.22996834425851,2.49144078075648,6.4907476204609));
#106828=CARTESIAN_POINT('Ctrl Pts',(3.114879271,2.490655005,6.822574817));
#106829=CARTESIAN_POINT('Ctrl Pts',(3.488398571,2.556411293,6.652042788));
#106830=CARTESIAN_POINT('Ctrl Pts',(3.841068843,2.621296797,6.441753654));
#106831=CARTESIAN_POINT('Ctrl Pts',(3.225721167,2.490655005,6.492859382));
#106832=CARTESIAN_POINT('Ctrl Pts',(3.581189353,2.556411293,6.31625903));
#106833=CARTESIAN_POINT('Ctrl Pts',(3.91525393,2.621296797,6.101908444));
#106834=CARTESIAN_POINT('Origin',(-0.0747944090379393,2.41076919092955,
-0.180440693997387));
#106835=CARTESIAN_POINT('Ctrl Pts',(4.23272190964437,2.62578637467355,6.19214319192852));
#106836=CARTESIAN_POINT('Ctrl Pts',(4.24425793307671,2.62354158583678,6.18419419749439));
#106837=CARTESIAN_POINT('Ctrl Pts',(4.25579395650908,2.621296797,6.17624520306028));
#106838=CARTESIAN_POINT('Ctrl Pts',(4.59142341067218,2.555986835,5.94497689134849));
#106839=CARTESIAN_POINT('Ctrl Pts',(4.9000152847214,2.49066265,5.6787003118293));
#106840=CARTESIAN_POINT('Ctrl Pts',(3.89245957637013,2.62578637467355,6.11653430794237));
#106841=CARTESIAN_POINT('Ctrl Pts',(3.9038567531851,2.62354158583678,6.10922137597126));
#106842=CARTESIAN_POINT('Ctrl Pts',(3.91525393,2.621296797,6.101908444));
#106843=CARTESIAN_POINT('Ctrl Pts',(4.246843776,2.555986835,5.889145755));
#106844=CARTESIAN_POINT('Ctrl Pts',(4.553425174,2.49066265,5.641703571));
#106845=CARTESIAN_POINT('Ctrl Pts',(3.88906389553661,2.62578637467355,6.11577976177873));
#106846=CARTESIAN_POINT('Ctrl Pts',(3.90045968671834,2.62354158583678,6.10847317745445));
#106847=CARTESIAN_POINT('Ctrl Pts',(3.9118554779,2.621296797,6.10116659312999));
#106848=CARTESIAN_POINT('Ctrl Pts',(4.24340501024,2.555986835,5.88858858277999));
#106849=CARTESIAN_POINT('Ctrl Pts',(4.5499663445,2.49066265,5.64133435845));
#106850=CARTESIAN_POINT('',(4.54977234856427,2.49144077987894,5.64464983369171));
#106851=CARTESIAN_POINT('Origin',(-0.117049403437909,2.55357126053773,-0.161632706015022));
#106852=CARTESIAN_POINT('Ctrl Pts',(4.70693606860209,2.53084202106238,5.83907123131914));
#106853=CARTESIAN_POINT('Ctrl Pts',(4.68068744031113,2.52458961891124,5.80665933175817));
#106854=CARTESIAN_POINT('Ctrl Pts',(4.65445194454156,2.51818504844758,5.77423581901437));
#106855=CARTESIAN_POINT('Ctrl Pts',(4.60207176775531,2.50506214889181,5.70944012703404));
#106856=CARTESIAN_POINT('Ctrl Pts',(4.5758970400296,2.49833629932961,5.6770307834315));
#106857=CARTESIAN_POINT('Ctrl Pts',(4.54977235220718,2.49144078070503,5.64464983057672));
#106858=CARTESIAN_POINT('Ctrl Pts',(4.508707036,2.490655005,5.99345984100001));
#106859=CARTESIAN_POINT('Ctrl Pts',(4.83683431699999,2.556411293,5.746619148));
#106860=CARTESIAN_POINT('Ctrl Pts',(5.136053407,2.621296797,5.465432773));
#106861=CARTESIAN_POINT('Ctrl Pts',(4.546078438,2.490655005,5.647625239));
#106862=CARTESIAN_POINT('Ctrl Pts',(4.85527212,2.556411293,5.398738552));
#106863=CARTESIAN_POINT('Ctrl Pts',(5.135447414,2.621296797,5.117585355));
#106864=CARTESIAN_POINT('Origin',(-0.111835230384976,2.41076916224554,-0.160143598903905));
#106865=CARTESIAN_POINT('Ctrl Pts',(5.46489097127033,2.6257863747464,5.13746423310914));
#106866=CARTESIAN_POINT('Ctrl Pts',(5.47444849018765,2.6235415858732,5.1272211775746));
#106867=CARTESIAN_POINT('Ctrl Pts',(5.48400600910498,2.621296797,5.11697812203994));
#106868=CARTESIAN_POINT('Ctrl Pts',(5.7620727817793,2.555986835,4.81896632426268));
#106869=CARTESIAN_POINT('Ctrl Pts',(6.00620835592956,2.49066265,4.49257701135858));
#106870=CARTESIAN_POINT('Ctrl Pts',(5.1163301078429,2.6257863747464,5.1367693869352));
#106871=CARTESIAN_POINT('Ctrl Pts',(5.12588876092139,2.6235415858732,5.12717737096759));
#106872=CARTESIAN_POINT('Ctrl Pts',(5.135447414,2.621296797,5.117585355));
#106873=CARTESIAN_POINT('Ctrl Pts',(5.413547184,2.555986835,4.838514924));
#106874=CARTESIAN_POINT('Ctrl Pts',(5.659768124,2.49066265,4.530951863));
#106875=CARTESIAN_POINT('Ctrl Pts',(5.11285161102587,2.6257863747464,5.13676245265066));
#106876=CARTESIAN_POINT('Ctrl Pts',(5.12241027542293,2.6235415858732,5.12717693379532));
#106877=CARTESIAN_POINT('Ctrl Pts',(5.13196893981999,2.621296797,5.11759141494));
#106878=CARTESIAN_POINT('Ctrl Pts',(5.41006903912,2.555986835,4.83871001114));
#106879=CARTESIAN_POINT('Ctrl Pts',(5.65631079023,2.49066265,4.53133482854));
#106880=CARTESIAN_POINT('',(5.65683405948763,2.49144077991402,4.53461449353211));
#106881=CARTESIAN_POINT('Origin',(-0.149059046435998,2.55357125054164,-0.13269161056075));
#106882=CARTESIAN_POINT('Ctrl Pts',(5.85211823186666,2.53084202101146,4.69070487206605));
#106883=CARTESIAN_POINT('Ctrl Pts',(5.81951568170992,2.52458961890036,4.66469342404254));
#106884=CARTESIAN_POINT('Ctrl Pts',(5.78692346058046,2.51818504847848,4.63866781124984));
#106885=CARTESIAN_POINT('Ctrl Pts',(5.72183874466787,2.5050621489152,4.5866471962267));
#106886=CARTESIAN_POINT('Ctrl Pts',(5.6893089173677,2.49833629949945,4.56062235843184));
#106887=CARTESIAN_POINT('Ctrl Pts',(5.65683406228975,2.49144078081474,4.53461448979442));
#106888=CARTESIAN_POINT('Ctrl Pts',(5.691712671,2.490655005,4.884097344));
#106889=CARTESIAN_POINT('Ctrl Pts',(5.959105067,2.556411293,4.572489983));
#106890=CARTESIAN_POINT('Ctrl Pts',(6.19088182200001,2.621296797,4.23355433));
#106891=CARTESIAN_POINT('Ctrl Pts',(5.653866134,2.490655005,4.538314416));
#106892=CARTESIAN_POINT('Ctrl Pts',(5.902327759,2.556411293,4.22877906));
#106893=CARTESIAN_POINT('Ctrl Pts',(6.115513083,2.621296797,3.893969662));
#106894=CARTESIAN_POINT('Origin',(-0.143646806777386,2.41076920669575,-0.132358290931466));
#106895=CARTESIAN_POINT('Ctrl Pts',(6.44152780532351,2.62578637474175,3.84256315617851));
#106896=CARTESIAN_POINT('Ctrl Pts',(6.44865992058243,2.62354158587088,3.83050499356447));
#106897=CARTESIAN_POINT('Ctrl Pts',(6.45579203584126,2.621296797,3.8184468309505));
#106898=CARTESIAN_POINT('Ctrl Pts',(6.66329403417114,2.555986835,3.46762624718635));
#106899=CARTESIAN_POINT('Ctrl Pts',(6.83155779937354,2.49066265,3.09638580299899));
#106900=CARTESIAN_POINT('Ctrl Pts',(6.10096672854028,2.62578637474176,3.91681483759952));
#106901=CARTESIAN_POINT('Ctrl Pts',(6.10823990577019,2.62354158587088,3.90539224979975));
#106902=CARTESIAN_POINT('Ctrl Pts',(6.115513083,2.621296797,3.893969662));
#106903=CARTESIAN_POINT('Ctrl Pts',(6.32711914299999,2.555986835,3.561640513));
#106904=CARTESIAN_POINT('Ctrl Pts',(6.501466607,2.49066265,3.208337881));
#106905=CARTESIAN_POINT('Ctrl Pts',(6.09756806636723,2.62578637474176,3.91755583942896));
#106906=CARTESIAN_POINT('Ctrl Pts',(6.1048426513386,2.62354158587088,3.90613959440948));
#106907=CARTESIAN_POINT('Ctrl Pts',(6.11211723631001,2.621296797,3.89472334939));
#106908=CARTESIAN_POINT('Ctrl Pts',(6.32376425318999,2.555986835,3.56257873745));
#106909=CARTESIAN_POINT('Ctrl Pts',(6.49817243005,2.49066265,3.20945511758));
#106910=CARTESIAN_POINT('',(6.49938849676083,2.49144077990629,3.21254561858896));
#106911=CARTESIAN_POINT('Origin',(-0.174099247004624,2.55357123366904,-0.0975462565322924));
#106912=CARTESIAN_POINT('Ctrl Pts',(6.72366185073863,2.53084202102691,3.32300636632164));
#106913=CARTESIAN_POINT('Ctrl Pts',(6.68622983778571,2.52458961891645,3.30461163604301));
#106914=CARTESIAN_POINT('Ctrl Pts',(6.6488048672343,2.51818504847267,3.28620085165096));
#106915=CARTESIAN_POINT('Ctrl Pts',(6.57405890157978,2.50506214891626,3.24938773966147));
#106916=CARTESIAN_POINT('Ctrl Pts',(6.53669503270045,2.49833629947486,3.23096429927423));
#106917=CARTESIAN_POINT('Ctrl Pts',(6.49938849887346,2.49144078080004,3.21254561397528));
#106918=CARTESIAN_POINT('Ctrl Pts',(6.608580148,2.490655005,3.546359884));
#106919=CARTESIAN_POINT('Ctrl Pts',(6.802734686,2.556411293,3.184556269));
#106920=CARTESIAN_POINT('Ctrl Pts',(6.956231483,2.621296797,2.803719592));
#106921=CARTESIAN_POINT('Ctrl Pts',(6.497285334,2.490655005,3.216797055));
#106922=CARTESIAN_POINT('Ctrl Pts',(6.673397112,2.556411293,2.861086559));
#106923=CARTESIAN_POINT('Ctrl Pts',(6.809624158,2.621296797,2.488276275));
#106924=CARTESIAN_POINT('Origin',(-0.1687414122409,2.41076915116035,-0.0983839597344316));
#106925=CARTESIAN_POINT('Ctrl Pts',(7.11696595813061,2.62578637464404,2.36798809633568));
#106926=CARTESIAN_POINT('Ctrl Pts',(7.1213391798758,2.62354158582205,2.35467865318869));
#106927=CARTESIAN_POINT('Ctrl Pts',(7.12571240162084,2.621296797,2.34136921004164));
#106928=CARTESIAN_POINT('Ctrl Pts',(7.2529470631546,2.555986835,1.95414382044684));
#106929=CARTESIAN_POINT('Ctrl Pts',(7.33747119381903,2.49066265,1.55541103631253));
#106930=CARTESIAN_POINT('Ctrl Pts',(6.80032892691287,2.62578637464404,2.51371437875452));
#106931=CARTESIAN_POINT('Ctrl Pts',(6.80497654245637,2.62354158582205,2.50099532687726));
#106932=CARTESIAN_POINT('Ctrl Pts',(6.809624158,2.621296797,2.488276275));
#106933=CARTESIAN_POINT('Ctrl Pts',(6.944842042,2.555986835,2.118227749));
#106934=CARTESIAN_POINT('Ctrl Pts',(7.039163737,2.49066265,1.735705586));
#106935=CARTESIAN_POINT('Ctrl Pts',(6.79716901706411,2.62578637464404,2.51516866827108));
#106936=CARTESIAN_POINT('Ctrl Pts',(6.80181937094693,2.62354158582205,2.50245550826054));
#106937=CARTESIAN_POINT('Ctrl Pts',(6.80646972483,2.621296797,2.48974234825));
#106938=CARTESIAN_POINT('Ctrl Pts',(6.94176727817,2.555986835,2.11986524042));
#106939=CARTESIAN_POINT('Ctrl Pts',(7.03618674890999,2.49066265,1.73750485288));
#106940=CARTESIAN_POINT('',(7.03803875113731,2.49144077992003,1.74026168046717));
#106941=CARTESIAN_POINT('Origin',(-0.190998271340511,2.55357130199046,-0.0578394435494334));
#106942=CARTESIAN_POINT('Ctrl Pts',(7.28081451460901,2.5308420210154,1.79992777604475));
#106943=CARTESIAN_POINT('Ctrl Pts',(7.24030324971045,2.52458960837035,1.79000986396438));
#106944=CARTESIAN_POINT('Ctrl Pts',(7.19979551660118,2.51818504338184,1.78007478494001));
#106945=CARTESIAN_POINT('Ctrl Pts',(7.11888337027677,2.5050621488933,1.76019052401277));
#106946=CARTESIAN_POINT('Ctrl Pts',(7.07843255283466,2.49833629947179,1.75022994088429));
#106947=CARTESIAN_POINT('Ctrl Pts',(7.03803875201506,2.49144078078745,1.74026167631028));
#106948=CARTESIAN_POINT('Ctrl Pts',(7.216437762,2.490655005,2.042798577));
#106949=CARTESIAN_POINT('Ctrl Pts',(7.328275993,2.556411293,1.647716243));
#106950=CARTESIAN_POINT('Ctrl Pts',(7.396315492,2.621296797,1.242786042));
#106951=CARTESIAN_POINT('Ctrl Pts',(7.036898692,2.490655005,1.744865839));
#106952=CARTESIAN_POINT('Ctrl Pts',(7.132425833,2.556411293,1.35961283));
#106953=CARTESIAN_POINT('Ctrl Pts',(7.185324776,2.621296797,0.966233856));
#106954=CARTESIAN_POINT('Origin',(-0.185946087418248,2.41076918789427,-0.0598094055549393));
#106955=CARTESIAN_POINT('Ctrl Pts',(7.45962269256189,2.62578637465542,0.782688546059122));
#106956=CARTESIAN_POINT('Ctrl Pts',(7.46103253396334,2.62354158582774,0.768750156846797));
#106957=CARTESIAN_POINT('Ctrl Pts',(7.46244237536476,2.621296797,0.754811767634472));
#106958=CARTESIAN_POINT('Ctrl Pts',(7.50346034873277,2.555986835,0.349287800947316));
#106959=CARTESIAN_POINT('Ctrl Pts',(7.50029259058375,2.49066265,-0.0582930225763819));
#106960=CARTESIAN_POINT('Ctrl Pts',(7.18171530263629,2.62578637465542,0.993075431001356));
#106961=CARTESIAN_POINT('Ctrl Pts',(7.18352003931813,2.62354158582774,0.979654643500677));
#106962=CARTESIAN_POINT('Ctrl Pts',(7.185324776,2.621296797,0.966233856));
#106963=CARTESIAN_POINT('Ctrl Pts',(7.237831846,2.555986835,0.575769011));
#106964=CARTESIAN_POINT('Ctrl Pts',(7.247717395,2.49066265,0.181913626));
#106965=CARTESIAN_POINT('Ctrl Pts',(7.17894189898503,2.62578637465542,0.99517500724877));
#106966=CARTESIAN_POINT('Ctrl Pts',(7.18075057656252,2.62354158582774,0.98175938520438));
#106967=CARTESIAN_POINT('Ctrl Pts',(7.18255925414001,2.621296797,0.968343763159999));
#106968=CARTESIAN_POINT('Ctrl Pts',(7.23518098069,2.555986835,0.578029202120001));
#106969=CARTESIAN_POINT('Ctrl Pts',(7.24519679643001,2.49066265,0.18431079146));
#106970=CARTESIAN_POINT('',(7.24759813578468,2.49144077987902,0.186605041169715));
#106971=CARTESIAN_POINT('Origin',(-0.198966747438476,2.55357127314528,-0.0154282146168049));
#106972=CARTESIAN_POINT('Ctrl Pts',(7.49752438372847,2.53084202102278,0.19268656358911));
#106973=CARTESIAN_POINT('Ctrl Pts',(7.4558282619199,2.52458961889093,0.191709252839032));
#106974=CARTESIAN_POINT('Ctrl Pts',(7.41413179084399,2.51818504845344,0.19071441476443));
#106975=CARTESIAN_POINT('Ctrl Pts',(7.33083676504294,2.50506214889565,0.188688755670287));
#106976=CARTESIAN_POINT('Ctrl Pts',(7.28919043403217,2.4983362994351,0.187656775431307));
#106977=CARTESIAN_POINT('Ctrl Pts',(7.24759813575377,2.49144078078428,0.186605036456807));
#106978=CARTESIAN_POINT('Ctrl Pts',(7.48686276700001,2.490655005,0.443718279));
#106979=CARTESIAN_POINT('Ctrl Pts',(7.511155258,2.556411293,0.033830836));
#106980=CARTESIAN_POINT('Ctrl Pts',(7.490556008,2.621296797,-0.376258802));
#106981=CARTESIAN_POINT('Ctrl Pts',(7.247474489,2.490655005,0.191346636));
#106982=CARTESIAN_POINT('Ctrl Pts',(7.25795025,2.556411293,-0.205434883));
#106983=CARTESIAN_POINT('Ctrl Pts',(7.22504759300001,2.621296797,-0.600988585));
#106984=CARTESIAN_POINT('Origin',(-0.194455944157425,2.41076918068398,-0.018438186900226));
#106985=CARTESIAN_POINT('Ctrl Pts',(7.45347576122951,2.62578637474903,-0.839208650378814));
#106986=CARTESIAN_POINT('Ctrl Pts',(7.45185629962364,2.62354158587455,-0.853124242334209));
#106987=CARTESIAN_POINT('Ctrl Pts',(7.45023683801784,2.621296797,-0.867039834289613));
#106988=CARTESIAN_POINT('Ctrl Pts',(7.40312016832359,2.555986835,-1.27190052837077));
#106989=CARTESIAN_POINT('Ctrl Pts',(7.31240864069535,2.49066265,-1.66927136382544));
#106990=CARTESIAN_POINT('Ctrl Pts',(7.22729265237664,2.62578637474904,-0.573998620455721));
#106991=CARTESIAN_POINT('Ctrl Pts',(7.22617012268838,2.62354158587455,-0.587493602727866));
#106992=CARTESIAN_POINT('Ctrl Pts',(7.225047593,2.621296797,-0.600988585));
#106993=CARTESIAN_POINT('Ctrl Pts',(7.192388677,2.555986835,-0.993612047));
#106994=CARTESIAN_POINT('Ctrl Pts',(7.117375842,2.49066265,-1.380384412));
#106995=CARTESIAN_POINT('Ctrl Pts',(7.22503543618639,2.62578637474904,-0.571351931335677));
#106996=CARTESIAN_POINT('Ctrl Pts',(7.22391786567831,2.62354158587455,-0.584842716092841));
#106997=CARTESIAN_POINT('Ctrl Pts',(7.22280029517,2.621296797,-0.59833350085));
#106998=CARTESIAN_POINT('Ctrl Pts',(7.19028566172001,2.555986835,-0.99083484021));
#106999=CARTESIAN_POINT('Ctrl Pts',(7.11542949334,2.49066265,-1.37750143675));
#107000=CARTESIAN_POINT('',(7.11826788656464,2.4914407799091,-1.37577704263276));
#107001=CARTESIAN_POINT('Origin',(-0.197631358335422,2.55357126158124,0.0277044275792105));
#107002=CARTESIAN_POINT('Ctrl Pts',(7.36365834559444,2.53084202102572,-1.42356445854499));
#107003=CARTESIAN_POINT('Ctrl Pts',(7.32272696298888,2.52458961890017,-1.41555548667759));
#107004=CARTESIAN_POINT('Ctrl Pts',(7.28179147137135,2.51818504846001,-1.40756355721964));
#107005=CARTESIAN_POINT('Ctrl Pts',(7.20000837997913,2.50506214889318,-1.3916358889752));
#107006=CARTESIAN_POINT('Ctrl Pts',(7.15911387198551,2.49833629947242,-1.38369101187184));
#107007=CARTESIAN_POINT('Ctrl Pts',(7.1182678855985,2.49144078080531,-1.37577704683838));
#107008=CARTESIAN_POINT('Ctrl Pts',(7.40721039,2.490655005,-1.176109793));
#107009=CARTESIAN_POINT('Ctrl Pts',(7.342821252,2.556411293,-1.581636462));
#107010=CARTESIAN_POINT('Ctrl Pts',(7.234546451,2.621296797,-1.977710203));
#107011=CARTESIAN_POINT('Ctrl Pts',(7.11916643300001,2.490655005,-1.371119723));
#107012=CARTESIAN_POINT('Ctrl Pts',(7.044100979,2.556411293,-1.76087669));
#107013=CARTESIAN_POINT('Ctrl Pts',(6.926935215,2.621296797,-2.140109468));
#107014=CARTESIAN_POINT('Origin',(-0.19387335622159,2.4107691791716,0.0237951653835827));
#107015=CARTESIAN_POINT('Ctrl Pts',(7.09881258653112,2.62578637474301,-2.42186538442023));
#107016=CARTESIAN_POINT('Ctrl Pts',(7.09423954612711,2.62354158587153,-2.4351075011484));
#107017=CARTESIAN_POINT('Ctrl Pts',(7.0896665057231,2.621296797,-2.4483496178766));
#107018=CARTESIAN_POINT('Ctrl Pts',(6.95661831629296,2.555986835,-2.83361620186909));
#107019=CARTESIAN_POINT('Ctrl Pts',(6.78260459090735,2.49066265,-3.20219643111982));
#107020=CARTESIAN_POINT('Ctrl Pts',(6.93492983067391,2.625786374743,-2.1142331352719));
#107021=CARTESIAN_POINT('Ctrl Pts',(6.93093252283703,2.62354158587153,-2.12717130163598));
#107022=CARTESIAN_POINT('Ctrl Pts',(6.926935215,2.621296797,-2.140109468));
#107023=CARTESIAN_POINT('Ctrl Pts',(6.810637408,2.555986835,-2.51653291));
#107024=CARTESIAN_POINT('Ctrl Pts',(6.654233705,2.49066265,-2.878137209));
#107025=CARTESIAN_POINT('Ctrl Pts',(6.93329434687637,2.625786374743,-2.11116308951596));
#107026=CARTESIAN_POINT('Ctrl Pts',(6.92930278461823,2.62354158587153,-2.12409822257802));
#107027=CARTESIAN_POINT('Ctrl Pts',(6.92531122236,2.621296797,-2.13703335564));
#107028=CARTESIAN_POINT('Ctrl Pts',(6.80918057742,2.555986835,-2.51336854665));
#107029=CARTESIAN_POINT('Ctrl Pts',(6.65295261534,2.49066265,-2.87490322868));
#107030=CARTESIAN_POINT('',(6.65609534290415,2.49144077992861,-2.87382932098846));
#107031=CARTESIAN_POINT('Origin',(-0.187055439915538,2.55357125199513,0.0695416967133695));
#107032=CARTESIAN_POINT('Ctrl Pts',(6.88547582727293,2.53084202099626,-2.9732511882983));
#107033=CARTESIAN_POINT('Ctrl Pts',(6.8472230899018,2.52458961887946,-2.95663042439173));
#107034=CARTESIAN_POINT('Ctrl Pts',(6.80896267611096,2.51818504847444,-2.94002542125642));
#107035=CARTESIAN_POINT('Ctrl Pts',(6.73251560584466,2.50506214892888,-2.90688918613168));
#107036=CARTESIAN_POINT('Ctrl Pts',(6.69428510228322,2.49833629948875,-2.89033894558378));
#107037=CARTESIAN_POINT('Ctrl Pts',(6.65609534087841,2.49144078083071,-2.8738293252976));
#107038=CARTESIAN_POINT('Ctrl Pts',(6.981205087,2.490655005,-2.740944277));
#107039=CARTESIAN_POINT('Ctrl Pts',(6.831145085,2.556411293,-3.123148198));
#107040=CARTESIAN_POINT('Ctrl Pts',(6.640257542,2.621296797,-3.486686073));
#107041=CARTESIAN_POINT('Ctrl Pts',(6.657974068,2.490655005,-2.869474048));
#107042=CARTESIAN_POINT('Ctrl Pts',(6.500877375,2.556411293,-3.23398186));
#107043=CARTESIAN_POINT('Ctrl Pts',(6.304927044,2.621296797,-3.57916121));
#107044=CARTESIAN_POINT('Origin',(-0.184225460090732,2.410769191445,0.0649159095010382));
#107045=CARTESIAN_POINT('Ctrl Pts',(6.41221682473796,2.62578637463497,-3.89127838495056));
#107046=CARTESIAN_POINT('Ctrl Pts',(6.40490403598196,2.62354158581749,-3.90322783954274));
#107047=CARTESIAN_POINT('Ctrl Pts',(6.39759124722611,2.621296797,-3.91517729413494));
#107048=CARTESIAN_POINT('Ctrl Pts',(6.18483272311034,2.555986835,-4.26283513136997));
#107049=CARTESIAN_POINT('Ctrl Pts',(5.93565348803106,2.49066265,-4.58539035288199));
#107050=CARTESIAN_POINT('Ctrl Pts',(6.31829739625385,2.62578637463497,-3.55560845819269));
#107051=CARTESIAN_POINT('Ctrl Pts',(6.31161222012691,2.62354158581749,-3.56738483409634));
#107052=CARTESIAN_POINT('Ctrl Pts',(6.304927044,2.621296797,-3.57916121));
#107053=CARTESIAN_POINT('Ctrl Pts',(6.110428303,2.555986835,-3.92178349));
#107054=CARTESIAN_POINT('Ctrl Pts',(5.879946996,2.49066265,-4.24131151));
#107055=CARTESIAN_POINT('Ctrl Pts',(6.31736011824208,2.62578637463497,-3.5522586077237));
#107056=CARTESIAN_POINT('Ctrl Pts',(6.31068120543602,2.62354158581749,-3.56403325637183));
#107057=CARTESIAN_POINT('Ctrl Pts',(6.30400229263001,2.621296797,-3.57580790502));
#107058=CARTESIAN_POINT('Ctrl Pts',(6.1096857769,2.555986835,-3.91837993219));
#107059=CARTESIAN_POINT('Ctrl Pts',(5.87939106768,2.49066265,-4.23787774194));
#107060=CARTESIAN_POINT('',(5.88269117803411,2.49144077925192,-4.23750453416556));
#107061=CARTESIAN_POINT('Origin',(-0.167732537891393,2.55357122438483,0.108127094189924));
#107062=CARTESIAN_POINT('Ctrl Pts',(6.08533611175123,2.53084202103098,-4.38391199742654));
#107063=CARTESIAN_POINT('Ctrl Pts',(6.05155067503814,2.52458961889364,-4.35945660995114));
#107064=CARTESIAN_POINT('Ctrl Pts',(6.01775435318723,2.51818504845103,-4.33501496450926));
#107065=CARTESIAN_POINT('Ctrl Pts',(5.95021788409655,2.50506214889897,-4.2862195759487));
#107066=CARTESIAN_POINT('Ctrl Pts',(5.91643900043463,2.49833629934497,-4.26183784232312));
#107067=CARTESIAN_POINT('Ctrl Pts',(5.8826911748804,2.49144078071014,-4.2375045381262));
#107068=CARTESIAN_POINT('Ctrl Pts',(6.228766394,2.490655005,-4.177615254));
#107069=CARTESIAN_POINT('Ctrl Pts',(6.000052166,2.556411293,-4.518624994));
#107070=CARTESIAN_POINT('Ctrl Pts',(5.735477571,2.621296797,-4.832628377));
#107071=CARTESIAN_POINT('Ctrl Pts',(5.885462235,2.490655005,-4.233654956));
#107072=CARTESIAN_POINT('Ctrl Pts',(5.653679971,2.556411293,-4.555869632));
#107073=CARTESIAN_POINT('Ctrl Pts',(5.388107493,2.621296797,-4.850855352));
#107074=CARTESIAN_POINT('Origin',(-0.165963364033447,2.41076915419993,0.103001217880749));
#107075=CARTESIAN_POINT('Ctrl Pts',(5.42579293193456,2.62578637464283,-5.17873953196371));
#107076=CARTESIAN_POINT('Ctrl Pts',(5.41608233257228,2.62354158582141,-5.18883758156318));
#107077=CARTESIAN_POINT('Ctrl Pts',(5.40637173320981,2.621296797,-5.19893563116276));
#107078=CARTESIAN_POINT('Ctrl Pts',(5.12385122646595,2.555986835,-5.49272862822822));
#107079=CARTESIAN_POINT('Ctrl Pts',(4.81115782554438,2.49066265,-5.75417651719663));
#107080=CARTESIAN_POINT('Ctrl Pts',(5.40622839938115,2.62578637464282,-4.83072748088294));
#107081=CARTESIAN_POINT('Ctrl Pts',(5.3971679461906,2.62354158582141,-4.84079141644148));
#107082=CARTESIAN_POINT('Ctrl Pts',(5.388107493,2.621296797,-4.850855352));
#107083=CARTESIAN_POINT('Ctrl Pts',(5.124502361,2.555986835,-5.143655834));
#107084=CARTESIAN_POINT('Ctrl Pts',(4.830720501,2.49066265,-5.406166798));
#107085=CARTESIAN_POINT('Ctrl Pts',(5.40603315323804,2.62578637464282,-4.82725446099159));
#107086=CARTESIAN_POINT('Ctrl Pts',(5.39697918824405,2.62354158582141,-4.83731805610587));
#107087=CARTESIAN_POINT('Ctrl Pts',(5.38792522325,2.621296797,-4.84738165122));
#107088=CARTESIAN_POINT('Ctrl Pts',(5.12450885906,2.555986835,-5.14017222832));
#107089=CARTESIAN_POINT('Ctrl Pts',(4.83091572861001,2.49066265,-5.40269380138));
#107090=CARTESIAN_POINT('',(4.83421891288047,2.49144077990264,-5.40303874585956));
#107091=CARTESIAN_POINT('Origin',(-0.140567026918504,2.55357128902595,0.141656766217955));
#107092=CARTESIAN_POINT('Ctrl Pts',(5.00065284321323,2.53084202097844,-5.58958595417019));
#107093=CARTESIAN_POINT('Ctrl Pts',(4.97291443011114,2.52458960835985,-5.55843939754943));
#107094=CARTESIAN_POINT('Ctrl Pts',(4.9451625040527,2.51818504337976,-5.52730400233));
#107095=CARTESIAN_POINT('Ctrl Pts',(4.88969458781793,2.50506214891053,-5.4651311021405));
#107096=CARTESIAN_POINT('Ctrl Pts',(4.86194678848643,2.49833629952378,-5.43405793901533));
#107097=CARTESIAN_POINT('Ctrl Pts',(4.83421890948478,2.4914407808494,-5.40303874868449));
#107098=CARTESIAN_POINT('Ctrl Pts',(5.185077507,2.490655005,-5.418945585));
#107099=CARTESIAN_POINT('Ctrl Pts',(4.888403477,2.556411293,-5.702815909));
#107100=CARTESIAN_POINT('Ctrl Pts',(4.562513043,2.621296797,-5.952602349));
#107101=CARTESIAN_POINT('Ctrl Pts',(4.837752729,2.490655005,-5.399874863));
#107102=CARTESIAN_POINT('Ctrl Pts',(4.542122774,2.556411293,-5.664730004));
#107103=CARTESIAN_POINT('Ctrl Pts',(4.219346023,2.621296797,-5.895728889));
#107104=CARTESIAN_POINT('Origin',(-0.139941037339313,2.41076919133494,0.136270381714059));
#107105=CARTESIAN_POINT('Ctrl Pts',(4.18566499123835,2.62578637470629,-6.2240485747905));
#107106=CARTESIAN_POINT('Ctrl Pts',(4.17401063797517,2.62354158585314,-6.23182304588717));
#107107=CARTESIAN_POINT('Ctrl Pts',(4.16235628471194,2.621296797,-6.23959751698383));
#107108=CARTESIAN_POINT('Ctrl Pts',(3.82328414093743,2.555986835,-6.46578823919025));
#107109=CARTESIAN_POINT('Ctrl Pts',(3.46169776941117,2.49066265,-6.65390378403682));
#107110=CARTESIAN_POINT('Ctrl Pts',(4.24137017021633,2.62578637470629,-5.87996705533536));
#107111=CARTESIAN_POINT('Ctrl Pts',(4.23035809660814,2.62354158585314,-5.88784797216773));
#107112=CARTESIAN_POINT('Ctrl Pts',(4.219346023,2.621296797,-5.895728889));
#107113=CARTESIAN_POINT('Ctrl Pts',(3.898960385,2.555986835,-6.125016547));
#107114=CARTESIAN_POINT('Ctrl Pts',(3.555614883,2.49066265,-6.31823573500001));
#107115=CARTESIAN_POINT('Ctrl Pts',(4.24192608543249,2.62578637470629,-5.87653326056434));
#107116=CARTESIAN_POINT('Ctrl Pts',(4.23092042151628,2.62354158585314,-5.88441523968222));
#107117=CARTESIAN_POINT('Ctrl Pts',(4.2199147576,2.621296797,-5.8922972188));
#107118=CARTESIAN_POINT('Ctrl Pts',(3.89971560339,2.555986835,-6.12161578297));
#107119=CARTESIAN_POINT('Ctrl Pts',(3.55655213791,2.49066265,-6.31488590327));
#107120=CARTESIAN_POINT('',(3.55970394316432,2.49144077994426,-6.31593287016467));
#107121=CARTESIAN_POINT('Origin',(-0.106828722370003,2.55357124591186,0.168562830045095));
#107122=CARTESIAN_POINT('Ctrl Pts',(3.68214460546017,2.53084202104465,-6.53389708360331));
#107123=CARTESIAN_POINT('Ctrl Pts',(3.66175032427548,2.52458961893437,-6.49751583846893));
#107124=CARTESIAN_POINT('Ctrl Pts',(3.64134039390339,2.51818504852252,-6.4611424947273));
#107125=CARTESIAN_POINT('Ctrl Pts',(3.60053460648105,2.5050621489647,-6.38849917192798));
#107126=CARTESIAN_POINT('Ctrl Pts',(3.58011534677004,2.49833629958865,-6.35218752553789));
#107127=CARTESIAN_POINT('Ctrl Pts',(3.55970393905361,2.49144078091802,-6.3159328722938));
#107128=CARTESIAN_POINT('Ctrl Pts',(3.898940158,2.490655005,-6.406892042));
#107129=CARTESIAN_POINT('Ctrl Pts',(3.548178474,2.556411293,-6.620349489));
#107130=CARTESIAN_POINT('Ctrl Pts',(3.176210476,2.621296797,-6.794239252));
#107131=CARTESIAN_POINT('Ctrl Pts',(3.563835282,2.490655005,-6.313602623));
#107132=CARTESIAN_POINT('Ctrl Pts',(3.218180965,2.556411293,-6.508713897));
#107133=CARTESIAN_POINT('Ctrl Pts',(2.853292624,2.621296797,-6.664924696));
#107134=CARTESIAN_POINT('Origin',(-0.10737519180722,2.41076923273296,0.163167647018698));
#107135=CARTESIAN_POINT('Ctrl Pts',(2.74982000782157,2.62578637464853,-6.97832802384387));
#107136=CARTESIAN_POINT('Ctrl Pts',(2.73676684554022,2.62354158582426,-6.9834153906098));
#107137=CARTESIAN_POINT('Ctrl Pts',(2.72371368325887,2.621296797,-6.98850275737571));
#107138=CARTESIAN_POINT('Ctrl Pts',(2.34394453822343,2.555986835,-7.13651477818134));
#107139=CARTESIAN_POINT('Ctrl Pts',(1.95037257434254,2.49066265,-7.24250190481632));
#107140=CARTESIAN_POINT('Ctrl Pts',(2.87819018699071,2.62578637464852,-6.65426590596132));
#107141=CARTESIAN_POINT('Ctrl Pts',(2.86574140549535,2.62354158582426,-6.65959530098065));
#107142=CARTESIAN_POINT('Ctrl Pts',(2.853292624,2.621296797,-6.664924696));
#107143=CARTESIAN_POINT('Ctrl Pts',(2.491107354,2.555986835,-6.819978295));
#107144=CARTESIAN_POINT('Ctrl Pts',(2.114252666,2.49066265,-6.934870991));
#107145=CARTESIAN_POINT('Ctrl Pts',(2.8794712695978,2.62578637464852,-6.65103189674261));
#107146=CARTESIAN_POINT('Ctrl Pts',(2.8670285195789,2.62354158582426,-6.65636370710631));
#107147=CARTESIAN_POINT('Ctrl Pts',(2.85458576956,2.621296797,-6.66169551747));
#107148=CARTESIAN_POINT('Ctrl Pts',(2.49257597954,2.555986835,-6.81681938857999));
#107149=CARTESIAN_POINT('Ctrl Pts',(2.11588812321,2.49066265,-6.93180095857));
#107150=CARTESIAN_POINT('',(2.11874117385913,2.49144077990718,-6.93350099308308));
#107151=CARTESIAN_POINT('Origin',(-0.0680950929919488,2.55357123368024,
0.187586940969906));
#107152=CARTESIAN_POINT('Ctrl Pts',(2.19146337849108,2.5308420210064,-7.17269044782304));
#107153=CARTESIAN_POINT('Ctrl Pts',(2.17936679654677,2.52458961889286,-7.13277560835312));
#107154=CARTESIAN_POINT('Ctrl Pts',(2.16725323268617,2.51818504846641,-7.09286512135973));
#107155=CARTESIAN_POINT('Ctrl Pts',(2.14301762893445,2.5050621489118,-7.01314812101274));
#107156=CARTESIAN_POINT('Ctrl Pts',(2.13088169066015,2.49833629949416,-6.97329588324911));
#107157=CARTESIAN_POINT('Ctrl Pts',(2.11874116901779,2.49144078082763,-6.93350099440057));
#107158=CARTESIAN_POINT('Ctrl Pts',(2.430492701,2.490655005,-7.095259349));
#107159=CARTESIAN_POINT('Ctrl Pts',(2.042044589,2.556411293,-7.228322886));
#107160=CARTESIAN_POINT('Ctrl Pts',(1.641391837,2.621296797,-7.318185078));
#107161=CARTESIAN_POINT('Ctrl Pts',(2.123276858,2.490655005,-6.932113342));
#107162=CARTESIAN_POINT('Ctrl Pts',(1.743760591,2.556411293,-7.048357562));
#107163=CARTESIAN_POINT('Ctrl Pts',(1.353822432,2.621296797,-7.122476032));
#107164=CARTESIAN_POINT('Origin',(-0.06978859721431,2.41076920475297,0.182435340521501));
#107165=CARTESIAN_POINT('Ctrl Pts',(1.185396495819,2.62578637457119,-7.40630861043433));
#107166=CARTESIAN_POINT('Ctrl Pts',(1.17155487598352,2.6235415857856,-7.40847099329535));
#107167=CARTESIAN_POINT('Ctrl Pts',(1.15771325614802,2.621296797,-7.41063337615642));
#107168=CARTESIAN_POINT('Ctrl Pts',(0.755004693420207,2.555986835,-7.4735458173585));
#107169=CARTESIAN_POINT('Ctrl Pts',(0.347850124077357,2.49066265,-7.49244868540235));
#107170=CARTESIAN_POINT('Ctrl Pts',(1.38042922812604,2.6257863745712,-7.1174186787875));
#107171=CARTESIAN_POINT('Ctrl Pts',(1.36712583006301,2.6235415857856,-7.11994735539381));
#107172=CARTESIAN_POINT('Ctrl Pts',(1.353822432,2.621296797,-7.12247603199999));
#107173=CARTESIAN_POINT('Ctrl Pts',(0.966772911999999,2.555986835,-7.196045436));
#107174=CARTESIAN_POINT('Ctrl Pts',(0.574030344,2.49066265,-7.227239388));
#107175=CARTESIAN_POINT('Ctrl Pts',(1.38237557612367,2.6257863745712,-7.11453567379976));
#107176=CARTESIAN_POINT('Ctrl Pts',(1.36907754929682,2.6235415857856,-7.11706800587));
#107177=CARTESIAN_POINT('Ctrl Pts',(1.35577952247,2.621296797,-7.11960033794));
#107178=CARTESIAN_POINT('Ctrl Pts',(0.968886273399999,2.555986835,-7.19327609412999));
#107179=CARTESIAN_POINT('Ctrl Pts',(0.57628753136,2.49066265,-7.22459270619));
#107180=CARTESIAN_POINT('',(0.578708421721061,2.49144077986087,-7.22686631479657));
#107181=CARTESIAN_POINT('Origin',(-0.0261773973728766,2.55357124537482,
0.197839503071522));
#107182=CARTESIAN_POINT('Ctrl Pts',(0.598311758986545,2.53084202105489,
-7.47609677807153));
#107183=CARTESIAN_POINT('Ctrl Pts',(0.595078493574171,2.52458960821832,
-7.43451464653647));
#107184=CARTESIAN_POINT('Ctrl Pts',(0.591827716122453,2.51818504328756,
-7.39293322468143));
#107185=CARTESIAN_POINT('Ctrl Pts',(0.585295528807562,2.50506214885077,
-7.30987005778724));
#107186=CARTESIAN_POINT('Ctrl Pts',(0.582010375225292,2.49833629930322,
-7.26834067461977));
#107187=CARTESIAN_POINT('Ctrl Pts',(0.578708417200044,2.49144078060891,
-7.22686631503214));
#107188=CARTESIAN_POINT('Ctrl Pts',(0.848398107,2.490655005,-7.45186021400001));
#107189=CARTESIAN_POINT('Ctrl Pts',(0.440426968,2.556411293,-7.498307938));
#107190=CARTESIAN_POINT('Ctrl Pts',(0.029823541,2.621296797,-7.499940704));
#107191=CARTESIAN_POINT('Ctrl Pts',(0.583436368,2.490655005,-7.226486145));
#107192=CARTESIAN_POINT('Ctrl Pts',(0.18780391,2.556411293,-7.258427861));
#107193=CARTESIAN_POINT('Ctrl Pts',(-0.208950992,2.621296797,-7.246988304));
#107194=CARTESIAN_POINT('Origin',(-0.0289387772614658,2.4107691699622,0.193172334428261));
#107195=CARTESIAN_POINT('Ctrl Pts',(-0.434454836636775,2.62578637474255,
-7.48797843674285));
#107196=CARTESIAN_POINT('Ctrl Pts',(-0.448437696021263,2.62354158587127,
-7.48711472518744));
#107197=CARTESIAN_POINT('Ctrl Pts',(-0.46242055540574,2.621296797,-7.486251013632));
#107198=CARTESIAN_POINT('Ctrl Pts',(-0.869238330894812,2.555986835,-7.46112216094296));
#107199=CARTESIAN_POINT('Ctrl Pts',(-1.27093741073832,2.49066265,-7.39205689301602));
#107200=CARTESIAN_POINT('Ctrl Pts',(-0.181879065534724,2.62578637474254,
-7.24776886349915));
#107201=CARTESIAN_POINT('Ctrl Pts',(-0.195415028767364,2.62354158587127,
-7.24737858374956));
#107202=CARTESIAN_POINT('Ctrl Pts',(-0.208950992,2.621296797,-7.246988304));
#107203=CARTESIAN_POINT('Ctrl Pts',(-0.602766756,2.555986835,-7.235633492));
#107204=CARTESIAN_POINT('Ctrl Pts',(-0.993032999,2.49066265,-7.181670103));
#107205=CARTESIAN_POINT('Ctrl Pts',(-0.179358461221376,2.62578637474254,
-7.24537166885228));
#107206=CARTESIAN_POINT('Ctrl Pts',(-0.192889964610694,2.62354158587127,
-7.24498611376109));
#107207=CARTESIAN_POINT('Ctrl Pts',(-0.206421468,2.621296797,-7.24460055867));
#107208=CARTESIAN_POINT('Ctrl Pts',(-0.60010747717,2.555986835,-7.23338320603999));
#107209=CARTESIAN_POINT('Ctrl Pts',(-0.990259625069999,2.49066265,-7.1795705277));
#107210=CARTESIAN_POINT('',(-0.988384093003052,2.4914407799151,-7.18231140161213));
#107211=CARTESIAN_POINT('Origin',(0.0169642529078204,2.55357128339156,0.198841623721516));
#107212=CARTESIAN_POINT('Ctrl Pts',(-1.02281625280334,2.53084202104047,
-7.42992913210504));
#107213=CARTESIAN_POINT('Ctrl Pts',(-1.0170350070352,2.52458961892557,-7.38862418208833));
#107214=CARTESIAN_POINT('Ctrl Pts',(-1.01127100116621,2.51818504848532,
-7.34731605168382));
#107215=CARTESIAN_POINT('Ctrl Pts',(-0.999794339433034,2.5050621489194,
-7.26479059594511));
#107216=CARTESIAN_POINT('Ctrl Pts',(-0.994075098219575,2.49833629950665,
-7.22352593649113));
#107217=CARTESIAN_POINT('Ctrl Pts',(-0.988384096897287,2.49144078082864,
-7.18231140092156));
#107218=CARTESIAN_POINT('Ctrl Pts',(-0.773366640000001,2.490655005,-7.46002037800001));
#107219=CARTESIAN_POINT('Ctrl Pts',(-1.181784528,2.556411293,-7.417680444));
#107220=CARTESIAN_POINT('Ctrl Pts',(-1.583139272,2.621296797,-7.331007437));
#107221=CARTESIAN_POINT('Ctrl Pts',(-0.983684957,2.490655005,-7.182956488));
#107222=CARTESIAN_POINT('Ctrl Pts',(-1.376934274,2.556411293,-7.12910214));
#107223=CARTESIAN_POINT('Ctrl Pts',(-1.7619541,2.621296797,-7.032639458));
#107224=CARTESIAN_POINT('Origin',(0.0132641981247958,2.41076921905478,0.194877278076248));
#107225=CARTESIAN_POINT('Ctrl Pts',(-2.03399154486877,2.62578637460005,
-7.21951871510429));
#107226=CARTESIAN_POINT('Ctrl Pts',(-2.04746181990288,2.62354158580003,
-7.21566929529137));
#107227=CARTESIAN_POINT('Ctrl Pts',(-2.06093209493694,2.621296797,-7.21181987547841));
#107228=CARTESIAN_POINT('Ctrl Pts',(-2.45283673674309,2.555986835,-7.09982472399587));
#107229=CARTESIAN_POINT('Ctrl Pts',(-2.83029732434835,2.49066265,-6.94602073587784));
#107230=CARTESIAN_POINT('Ctrl Pts',(-1.73568289820837,2.62578637460005,
-7.03922143219571));
#107231=CARTESIAN_POINT('Ctrl Pts',(-1.74881849910419,2.62354158580002,
-7.0359304450978));
#107232=CARTESIAN_POINT('Ctrl Pts',(-1.7619541,2.621296797,-7.032639458));
#107233=CARTESIAN_POINT('Ctrl Pts',(-2.144121721,2.555986835,-6.936891367));
#107234=CARTESIAN_POINT('Ctrl Pts',(-2.513663223,2.49066265,-6.80029390600001));
#107235=CARTESIAN_POINT('Ctrl Pts',(-1.73270589824414,2.62578637460005,
-7.03742213803926));
#107236=CARTESIAN_POINT('Ctrl Pts',(-1.7458381592271,2.62354158580002,-7.03413672387456));
#107237=CARTESIAN_POINT('Ctrl Pts',(-1.75897042021,2.621296797,-7.03085130971));
#107238=CARTESIAN_POINT('Ctrl Pts',(-2.14104086967,2.555986835,-6.93526535782));
#107239=CARTESIAN_POINT('Ctrl Pts',(-2.51050334239,2.49066265,-6.79883961102));
#107240=CARTESIAN_POINT('',(-2.50926086557921,2.49144077988688,-6.80191958859535));
#107241=CARTESIAN_POINT('Origin',(0.0593126565459542,2.55357125085242,0.190545812164162));
#107242=CARTESIAN_POINT('Ctrl Pts',(-2.59611851297963,2.53084202105645,
-7.03634625763598));
#107243=CARTESIAN_POINT('Ctrl Pts',(-2.58159308632968,2.52458961892987,
-6.99724979130256));
#107244=CARTESIAN_POINT('Ctrl Pts',(-2.56708381281763,2.51818504847661,
-6.95814651287555));
#107245=CARTESIAN_POINT('Ctrl Pts',(-2.53813493563216,2.5050621488739,-6.88001759932194));
#107246=CARTESIAN_POINT('Ctrl Pts',(-2.52367872523227,2.49833629948252,
-6.84094715263981));
#107247=CARTESIAN_POINT('Ctrl Pts',(-2.50926086955057,2.49144078078428,
-6.80191958696967));
#107248=CARTESIAN_POINT('Ctrl Pts',(-2.358969622,2.490655005,-7.11935828));
#107249=CARTESIAN_POINT('Ctrl Pts',(-2.748737092,2.556411293,-6.990210457));
#107250=CARTESIAN_POINT('Ctrl Pts',(-3.122076251,2.621296797,-6.819284411));
#107251=CARTESIAN_POINT('Ctrl Pts',(-2.504810268,2.490655005,-6.803559768));
#107252=CARTESIAN_POINT('Ctrl Pts',(-2.877288541,2.556411293,-6.666427527));
#107253=CARTESIAN_POINT('Ctrl Pts',(-3.232570193,2.621296797,-6.48945220700001));
#107254=CARTESIAN_POINT('Origin',(0.0548469433709137,2.41076919432706,0.187469768850078));
#107255=CARTESIAN_POINT('Ctrl Pts',(-3.53842107017982,2.62578637453734,
-6.61348232156691));
#107256=CARTESIAN_POINT('Ctrl Pts',(-3.55074890599494,2.62354158576867,
-6.60682718819617));
#107257=CARTESIAN_POINT('Ctrl Pts',(-3.56307674181012,2.621296797,-6.60017205482555));
#107258=CARTESIAN_POINT('Ctrl Pts',(-3.92174322298082,2.555986835,-6.40654737458525));
#107259=CARTESIAN_POINT('Ctrl Pts',(-4.25731568083912,2.49066265,-6.17519636984647));
#107260=CARTESIAN_POINT('Ctrl Pts',(-3.2083281275445,2.62578637453734,-6.50152782997209));
#107261=CARTESIAN_POINT('Ctrl Pts',(-3.22044916027223,2.62354158576867,
-6.49549001848606));
#107262=CARTESIAN_POINT('Ctrl Pts',(-3.232570193,2.621296797,-6.489452207));
#107263=CARTESIAN_POINT('Ctrl Pts',(-3.585219938,2.555986835,-6.313787911));
#107264=CARTESIAN_POINT('Ctrl Pts',(-3.916757348,2.49066265,-6.100943523));
#107265=CARTESIAN_POINT('Ctrl Pts',(-3.20503393312735,2.62578637453734,
-6.50041056930515));
#107266=CARTESIAN_POINT('Ctrl Pts',(-3.21715290204361,2.62354158576867,
-6.49437891844269));
#107267=CARTESIAN_POINT('Ctrl Pts',(-3.22927187096,2.621296797,-6.48834726758));
#107268=CARTESIAN_POINT('Ctrl Pts',(-3.58186157136,2.555986835,-6.31286220897));
#107269=CARTESIAN_POINT('Ctrl Pts',(-3.91335871321,2.49066265,-6.10020250954));
#107270=CARTESIAN_POINT('',(-3.91280738900435,2.49144077992664,-6.10347757543066));
#107271=CARTESIAN_POINT('Origin',(0.0988877438209256,2.55357123314395,0.173340571503654));
#107272=CARTESIAN_POINT('Ctrl Pts',(-4.04802915756938,2.5308420210067,-6.31375165296533));
#107273=CARTESIAN_POINT('Ctrl Pts',(-4.02543870508658,2.52458960847576,
-6.27869171914355));
#107274=CARTESIAN_POINT('Ctrl Pts',(-4.00286262173711,2.51818504343692,
-6.24362175005694));
#107275=CARTESIAN_POINT('Ctrl Pts',(-3.95779516364708,2.50506214893107,
-6.17354262673062));
#107276=CARTESIAN_POINT('Ctrl Pts',(-3.93527794006458,2.49833629948923,
-6.13849328278224));
#107277=CARTESIAN_POINT('Ctrl Pts',(-3.91280739300335,2.49144078084299,
-6.10347757268393));
#107278=CARTESIAN_POINT('Ctrl Pts',(-3.834269807,2.490655005,-6.445802902));
#107279=CARTESIAN_POINT('Ctrl Pts',(-4.187161766,2.556411293,-6.235885999));
#107280=CARTESIAN_POINT('Ctrl Pts',(-4.515028415,2.621296797,-5.98869922500001));
#107281=CARTESIAN_POINT('Ctrl Pts',(-3.908813434,2.490655005,-6.106036156));
#107282=CARTESIAN_POINT('Ctrl Pts',(-4.243103994,2.556411293,-5.892038171));
#107283=CARTESIAN_POINT('Ctrl Pts',(-4.55203489600001,2.621296797,-5.642825383));
#107284=CARTESIAN_POINT('Origin',(0.0938651415814157,2.41076919440569,0.171296399202997));
#107285=CARTESIAN_POINT('Ctrl Pts',(-4.87739795608349,2.62578637477553,
-5.69820684568798));
#107286=CARTESIAN_POINT('Ctrl Pts',(-4.88800691759883,2.62354158588777,
-5.68905718488216));
#107287=CARTESIAN_POINT('Ctrl Pts',(-4.89861587911403,2.621296797,-5.67990752407633));
#107288=CARTESIAN_POINT('Ctrl Pts',(-5.20727335563351,2.555986835,-5.41370699056624));
#107289=CARTESIAN_POINT('Ctrl Pts',(-5.48526668878452,2.49066265,-5.11562668380304));
#107290=CARTESIAN_POINT('Ctrl Pts',(-4.5309554974236,2.62578637477554,-5.65983001298165));
#107291=CARTESIAN_POINT('Ctrl Pts',(-4.54149519671181,2.62354158588777,
-5.65132769799085));
#107292=CARTESIAN_POINT('Ctrl Pts',(-4.552034896,2.621296797,-5.642825383));
#107293=CARTESIAN_POINT('Ctrl Pts',(-4.858677255,2.555986835,-5.39545875));
#107294=CARTESIAN_POINT('Ctrl Pts',(-5.136708253,2.49066265,-5.116319803));
#107295=CARTESIAN_POINT('Ctrl Pts',(-4.52749814143179,2.62578637477554,
-5.65944702767146));
#107296=CARTESIAN_POINT('Ctrl Pts',(-4.53803714951089,2.62354158588777,
-5.65095117293073));
#107297=CARTESIAN_POINT('Ctrl Pts',(-4.54857615759,2.621296797,-5.64245531819));
#107298=CARTESIAN_POINT('Ctrl Pts',(-4.85519840653001,2.555986835,-5.39527663992));
#107299=CARTESIAN_POINT('Ctrl Pts',(-5.13322978040999,2.49066265,-5.11632672005));
#107300=CARTESIAN_POINT('',(-5.13339538778399,2.49144077986205,-5.11964373418254));
#107301=CARTESIAN_POINT('Origin',(0.133838830789741,2.55357128992126,0.148029969099299));
#107302=CARTESIAN_POINT('Ctrl Pts',(-5.31065845768252,2.53084202101153,
-5.29593303788484));
#107303=CARTESIAN_POINT('Ctrl Pts',(-5.28105935724433,2.52458961887591,
-5.26654911421029));
#107304=CARTESIAN_POINT('Ctrl Pts',(-5.2514720567994,2.51818504843525,-5.23715222562454));
#107305=CARTESIAN_POINT('Ctrl Pts',(-5.19239328821142,2.50506214886337,
-5.17839966207316));
#107306=CARTESIAN_POINT('Ctrl Pts',(-5.1628679316371,2.49833629933328,-5.14901028953704));
#107307=CARTESIAN_POINT('Ctrl Pts',(-5.13339539093447,2.49144078066965,
-5.11964373083106));
#107308=CARTESIAN_POINT('Ctrl Pts',(-5.130283797,2.490655005,-5.470848943));
#107309=CARTESIAN_POINT('Ctrl Pts',(-5.429799409,2.556411293,-5.189978441));
#107310=CARTESIAN_POINT('Ctrl Pts',(-5.696862869,2.621296797,-4.878089119));
#107311=CARTESIAN_POINT('Ctrl Pts',(-5.130044829,2.490655005,-5.123001079));
#107312=CARTESIAN_POINT('Ctrl Pts',(-5.41051662,2.556411293,-4.84214366));
#107313=CARTESIAN_POINT('Ctrl Pts',(-5.658651506,2.621296797,-4.532346316));
#107314=CARTESIAN_POINT('Origin',(0.128494115922295,2.41076916488146,0.147113210000817));
#107315=CARTESIAN_POINT('Ctrl Pts',(-5.98831313732953,2.62578637459952,
-4.51648954957938));
#107316=CARTESIAN_POINT('Ctrl Pts',(-5.99670716025373,2.62354158579976,
-4.50527319005812));
#107317=CARTESIAN_POINT('Ctrl Pts',(-6.00510118317796,2.621296797,-4.49405683053693));
#107318=CARTESIAN_POINT('Ctrl Pts',(-6.2493171727924,2.555986835,-4.1677276835873));
#107319=CARTESIAN_POINT('Ctrl Pts',(-6.4567327218282,2.49066265,-3.81685598088725));
#107320=CARTESIAN_POINT('Ctrl Pts',(-5.64172042550917,2.62578637459952,
-4.55348483398021));
#107321=CARTESIAN_POINT('Ctrl Pts',(-5.65018596575455,2.62354158579976,
-4.54291557499014));
#107322=CARTESIAN_POINT('Ctrl Pts',(-5.658651506,2.621296797,-4.532346316));
#107323=CARTESIAN_POINT('Ctrl Pts',(-5.904948223,2.555986835,-4.224843934));
#107324=CARTESIAN_POINT('Ctrl Pts',(-6.116472389,2.49066265,-3.892462655));
#107325=CARTESIAN_POINT('Ctrl Pts',(-5.63826157005114,2.62578637459952,
-4.5538540319957));
#107326=CARTESIAN_POINT('Ctrl Pts',(-5.64672782401051,2.62354158579976,
-4.54329123080786));
#107327=CARTESIAN_POINT('Ctrl Pts',(-5.65519407797001,2.621296797,-4.53272842962));
#107328=CARTESIAN_POINT('Ctrl Pts',(-5.90151155978999,2.555986835,-4.22541393114));
#107329=CARTESIAN_POINT('Ctrl Pts',(-6.11307672812999,2.49066265,-3.89321717911));
#107330=CARTESIAN_POINT('',(-6.11395152353538,2.49144077987698,-3.89642104262899));
#107331=CARTESIAN_POINT('Origin',(0.162531914113915,2.55357126815225,0.115797771320377));
#107332=CARTESIAN_POINT('Ctrl Pts',(-6.3249672702921,2.53084202101672,-4.03048248028905));
#107333=CARTESIAN_POINT('Ctrl Pts',(-6.28974350540492,2.52458961887847,
-4.00814846808179));
#107334=CARTESIAN_POINT('Ctrl Pts',(-6.25452847761627,2.51818504844432,
-3.98579925744782));
#107335=CARTESIAN_POINT('Ctrl Pts',(-6.18420087352717,2.50506214887975,
-3.94112048507921));
#107336=CARTESIAN_POINT('Ctrl Pts',(-6.14904795691205,2.49833629931285,
-3.91876529849178));
#107337=CARTESIAN_POINT('Ctrl Pts',(-6.11395152592254,2.49144078066012,
-3.89642103863775));
#107338=CARTESIAN_POINT('Ctrl Pts',(-6.186411418,2.490655005,-4.240084169));
#107339=CARTESIAN_POINT('Ctrl Pts',(-6.418545666,2.556411293,-3.90139326));
#107340=CARTESIAN_POINT('Ctrl Pts',(-6.612318346,2.621296797,-3.539384988));
#107341=CARTESIAN_POINT('Ctrl Pts',(-6.111401029,2.490655005,-3.900420166));
#107342=CARTESIAN_POINT('Ctrl Pts',(-6.32493950200001,2.556411293,-3.565835892));
#107343=CARTESIAN_POINT('Ctrl Pts',(-6.500675861,2.621296797,-3.209939773));
#107344=CARTESIAN_POINT('Origin',(0.157115078729169,2.410769176666,0.116051396770692));
#107345=CARTESIAN_POINT('Ctrl Pts',(-6.81922145039121,2.62578637461624,
-3.12358622217615));
#107346=CARTESIAN_POINT('Ctrl Pts',(-6.8250080400054,2.62354158580812,-3.11082762807019));
#107347=CARTESIAN_POINT('Ctrl Pts',(-6.83079462961958,2.621296797,-3.09806903396429));
#107348=CARTESIAN_POINT('Ctrl Pts',(-6.99914986484065,2.555986835,-2.72687006272141));
#107349=CARTESIAN_POINT('Ctrl Pts',(-7.1262891087385,2.49066265,-2.3396133331402));
#107350=CARTESIAN_POINT('Ctrl Pts',(-6.48868477624709,2.62578637461624,
-3.23422376610269));
#107351=CARTESIAN_POINT('Ctrl Pts',(-6.49468031862353,2.62354158580812,
-3.22208176955133));
#107352=CARTESIAN_POINT('Ctrl Pts',(-6.500675861,2.621296797,-3.209939773));
#107353=CARTESIAN_POINT('Ctrl Pts',(-6.675110375,2.555986835,-2.856680112));
#107354=CARTESIAN_POINT('Ctrl Pts',(-6.810237074,2.49066265,-2.486598279));
#107355=CARTESIAN_POINT('Ctrl Pts',(-6.48538615356852,2.62578637461624,
-3.23532788416292));
#107356=CARTESIAN_POINT('Ctrl Pts',(-6.49138378120926,2.62354158580812,
-3.22319204100645));
#107357=CARTESIAN_POINT('Ctrl Pts',(-6.49738140885,2.621296797,-3.21105619785));
#107358=CARTESIAN_POINT('Ctrl Pts',(-6.6718765916,2.555986835,-2.85797556393));
#107359=CARTESIAN_POINT('Ctrl Pts',(-6.80708300218,2.49066265,-2.48806512947));
#107360=CARTESIAN_POINT('',(-6.80862608162008,2.4914407798974,-2.49100603347877));
#107361=CARTESIAN_POINT('Origin',(0.183624911732442,2.55357125500911,0.078150840754438));
#107362=CARTESIAN_POINT('Ctrl Pts',(-7.04352764352837,2.53084202101004,
-2.57657104078789));
#107363=CARTESIAN_POINT('Ctrl Pts',(-7.0043261726185,2.52458960840355,-2.56233122981495));
#107364=CARTESIAN_POINT('Ctrl Pts',(-6.96513006845,2.51818504338796,-2.54807473423963));
#107365=CARTESIAN_POINT('Ctrl Pts',(-6.88684209941904,2.50506214888574,
-2.51955889384003));
#107366=CARTESIAN_POINT('Ctrl Pts',(-6.8477053345953,2.4983362994034,-2.50528319728224));
#107367=CARTESIAN_POINT('Ctrl Pts',(-6.80862608309262,2.49144078072764,
-2.49100602904715));
#107368=CARTESIAN_POINT('Ctrl Pts',(-6.953269318,2.490655005,-2.811057772));
#107369=CARTESIAN_POINT('Ctrl Pts',(-7.107167862,2.556411293,-2.430383266));
#107370=CARTESIAN_POINT('Ctrl Pts',(-7.218589166,2.621296797,-2.035183148));
#107371=CARTESIAN_POINT('Ctrl Pts',(-6.806994909,2.490655005,-2.49545994));
#107372=CARTESIAN_POINT('Ctrl Pts',(-6.943615243,2.556411293,-2.122793602));
#107373=CARTESIAN_POINT('Ctrl Pts',(-7.038735838,2.621296797,-1.737440013));
#107374=CARTESIAN_POINT('Origin',(0.178389307057937,2.41076914731909,0.0795630440553063));
#107375=CARTESIAN_POINT('Ctrl Pts',(-7.33127054800828,2.6257863745359,-1.5846274748125));
#107376=CARTESIAN_POINT('Ctrl Pts',(-7.33417912971875,2.62354158576795,
-1.57092322405954));
#107377=CARTESIAN_POINT('Ctrl Pts',(-7.33708771142923,2.621296797,-1.55721897330657));
#107378=CARTESIAN_POINT('Ctrl Pts',(-7.42171008824151,2.555986835,-1.15850702824784));
#107379=CARTESIAN_POINT('Ctrl Pts',(-7.46262813804136,2.49066265,-0.752972966339287));
#107380=CARTESIAN_POINT('Ctrl Pts',(-7.03224543889095,2.6257863745359,-1.76373398808824));
#107381=CARTESIAN_POINT('Ctrl Pts',(-7.03549063844555,2.62354158576795,
-1.75058700054412));
#107382=CARTESIAN_POINT('Ctrl Pts',(-7.038735838,2.621296797,-1.737440013));
#107383=CARTESIAN_POINT('Ctrl Pts',(-7.133151786,2.555986835,-1.354941103));
#107384=CARTESIAN_POINT('Ctrl Pts',(-7.18556264200001,2.49066265,-0.964463331));
#107385=CARTESIAN_POINT('Ctrl Pts',(-7.0292612889204,2.6257863745359,-1.76552139884411));
#107386=CARTESIAN_POINT('Ctrl Pts',(-7.03250984778524,2.62354158576795,
-1.75237997256209));
#107387=CARTESIAN_POINT('Ctrl Pts',(-7.03575840664999,2.621296797,-1.73923854628));
#107388=CARTESIAN_POINT('Ctrl Pts',(-7.13027209054,2.555986835,-1.35690143583));
#107389=CARTESIAN_POINT('Ctrl Pts',(-7.18279764011001,2.49066265,-0.96657391953));
#107390=CARTESIAN_POINT('',(-7.1849368512499,2.49144077995398,-0.969114350955572));
#107391=CARTESIAN_POINT('Origin',(0.196132190812308,2.55357125277221,0.036849830138366));
#107392=CARTESIAN_POINT('Ctrl Pts',(-7.43274049243919,2.53084202102401,
-1.0021820033146));
#107393=CARTESIAN_POINT('Ctrl Pts',(-7.39139439192935,2.52458960846359,
-0.996702268783386));
#107394=CARTESIAN_POINT('Ctrl Pts',(-7.35004994567745,2.51818504345243,
-0.991205086004076));
#107395=CARTESIAN_POINT('Ctrl Pts',(-7.26746224275289,2.50506214895304,
-0.980185529411156));
#107396=CARTESIAN_POINT('Ctrl Pts',(-7.22617162141718,2.49833629958382,
-0.97465683841716));
#107397=CARTESIAN_POINT('Ctrl Pts',(-7.18493685170376,2.49144078092553,
-0.969114346370235));
#107398=CARTESIAN_POINT('Ctrl Pts',(-7.39500007200001,2.490655005,-1.250589437));
#107399=CARTESIAN_POINT('Ctrl Pts',(-7.463466788,2.556411293,-0.845731252));
#107400=CARTESIAN_POINT('Ctrl Pts',(-7.48732678,2.621296797,-0.435818406));
#107401=CARTESIAN_POINT('Ctrl Pts',(-7.184301272,2.490655005,-0.973814782));
#107402=CARTESIAN_POINT('Ctrl Pts',(-7.237615252,2.556411293,-0.580491841));
#107403=CARTESIAN_POINT('Ctrl Pts',(-7.24767235,2.621296797,-0.18369949));
#107404=CARTESIAN_POINT('Origin',(0.191322602224666,2.4107692487785,0.0393544752637704));
#107405=CARTESIAN_POINT('Ctrl Pts',(-7.50051758257422,2.62578637468215,
0.0284266915779838));
#107406=CARTESIAN_POINT('Ctrl Pts',(-7.50041215445485,2.62354158584108,
0.0424358040812995));
#107407=CARTESIAN_POINT('Ctrl Pts',(-7.50030672633549,2.621296797,0.0564449165846143));
#107408=CARTESIAN_POINT('Ctrl Pts',(-7.49723939708654,2.555986835,0.464026506667262));
#107409=CARTESIAN_POINT('Ctrl Pts',(-7.4500229692408,2.49066265,0.86887557847777));
#107410=CARTESIAN_POINT('Ctrl Pts',(-7.24698612022987,2.62578637468215,
-0.210773971470443));
#107411=CARTESIAN_POINT('Ctrl Pts',(-7.24732923511492,2.62354158584108,
-0.197236730735224));
#107412=CARTESIAN_POINT('Ctrl Pts',(-7.24767235000001,2.621296797,-0.18369949));
#107413=CARTESIAN_POINT('Ctrl Pts',(-7.257654946,2.555986835,0.210153447));
#107414=CARTESIAN_POINT('Ctrl Pts',(-7.224899287,2.49066265,0.60276885));
#107415=CARTESIAN_POINT('Ctrl Pts',(-7.24445597850344,2.62578637468215,
-0.213161097600633));
#107416=CARTESIAN_POINT('Ctrl Pts',(-7.24480356966667,2.62354158584108,
-0.199628565955319));
#107417=CARTESIAN_POINT('Ctrl Pts',(-7.24515116083001,2.621296797,-0.18609603431));
#107418=CARTESIAN_POINT('Ctrl Pts',(-7.25526398982,2.555986835,0.20761989627));
#107419=CARTESIAN_POINT('Ctrl Pts',(-7.22265264346,2.49066265,0.60011321219));
#107420=CARTESIAN_POINT('',(-7.22528795887604,2.49144077931082,0.598092041708296));
#107421=CARTESIAN_POINT('Origin',(0.199468459704493,2.55357127355161,-0.00617432263186217));
#107422=CARTESIAN_POINT('Ctrl Pts',(-7.4744066565912,2.53084202101378,0.619067950003639));
#107423=CARTESIAN_POINT('Ctrl Pts',(-7.43284929343279,2.52458961890745,
0.615531388015672));
#107424=CARTESIAN_POINT('Ctrl Pts',(-7.3912896880179,2.51818504849757,0.612012212856936));
#107425=CARTESIAN_POINT('Ctrl Pts',(-7.30826392881563,2.50506214895256,
0.605020221165677));
#107426=CARTESIAN_POINT('Ctrl Pts',(-7.26675015383567,2.49833629953379,
0.60154339156249));
#107427=CARTESIAN_POINT('Ctrl Pts',(-7.22528795819245,2.49144078086637,
0.598092046812624));
#107428=CARTESIAN_POINT('Ctrl Pts',(-7.490948841,2.490655005,0.36835507));
#107429=CARTESIAN_POINT('Ctrl Pts',(-7.470782301,2.556411293,0.778466215));
#107430=CARTESIAN_POINT('Ctrl Pts',(-7.405965316,2.621296797,1.18392472));
#107431=CARTESIAN_POINT('Ctrl Pts',(-7.225677693,2.490655005,0.593364874000001));
#107432=CARTESIAN_POINT('Ctrl Pts',(-7.19319241600001,2.556411293,0.988953072));
#107433=CARTESIAN_POINT('Ctrl Pts',(-7.117715759,2.621296797,1.378630618));
#107434=CARTESIAN_POINT('Origin',(0.19530968465359,2.41076918195982,-0.00269430202695181));
#107435=CARTESIAN_POINT('Ctrl Pts',(-7.31904875066757,2.6257863747346,1.64015165671534));
#107436=CARTESIAN_POINT('Ctrl Pts',(-7.31593424229251,2.6235415858673,1.65381058023396));
#107437=CARTESIAN_POINT('Ctrl Pts',(-7.31281973391756,2.621296797,1.66746950375251));
#107438=CARTESIAN_POINT('Ctrl Pts',(-7.2222061236215,2.555986835,2.06486267909892));
#107439=CARTESIAN_POINT('Ctrl Pts',(-7.08906300674665,2.49066265,2.45009646767005));
#107440=CARTESIAN_POINT('Ctrl Pts',(-7.12286578617508,2.6257863747346,1.35204160345207));
#107441=CARTESIAN_POINT('Ctrl Pts',(-7.1202907725876,2.6235415858673,1.36533611072604));
#107442=CARTESIAN_POINT('Ctrl Pts',(-7.117715759,2.621296797,1.378630618));
#107443=CARTESIAN_POINT('Ctrl Pts',(-7.04279822799999,2.555986835,1.765421455));
#107444=CARTESIAN_POINT('Ctrl Pts',(-6.926407672,2.49066265,2.141816229));
#107445=CARTESIAN_POINT('Ctrl Pts',(-7.12090795932432,2.6257863747346,1.34916638133631));
#107446=CARTESIAN_POINT('Ctrl Pts',(-7.11833832967726,2.6235415858673,1.36245725188317));
#107447=CARTESIAN_POINT('Ctrl Pts',(-7.11576870003,2.621296797,1.37574812243));
#107448=CARTESIAN_POINT('Ctrl Pts',(-7.04100780956999,2.555986835,1.76243315237));
#107449=CARTESIAN_POINT('Ctrl Pts',(-6.92478443737,2.49066265,2.13873971657));
#107450=CARTESIAN_POINT('',(-6.9277926318589,2.49144077988269,2.137332315355));
#107451=CARTESIAN_POINT('Origin',(0.193477601861138,2.55357126352284,-0.048909767983537));
#107452=CARTESIAN_POINT('Ctrl Pts',(-7.16657787288143,2.5308420210282,2.2113709751042));
#107453=CARTESIAN_POINT('Ctrl Pts',(-7.12675228698287,2.52458960837003,
2.19898347034696));
#107454=CARTESIAN_POINT('Ctrl Pts',(-7.08692087679801,2.51818504336427,
2.18661249604038));
#107455=CARTESIAN_POINT('Ctrl Pts',(-7.00733931618786,2.5050621488743,2.16193589866133));
#107456=CARTESIAN_POINT('Ctrl Pts',(-6.96754352551645,2.49833629938396,
2.14961612077613));
#107457=CARTESIAN_POINT('Ctrl Pts',(-6.92779263023784,2.49144078071947,
2.13733232013111));
#107458=CARTESIAN_POINT('Ctrl Pts',(-7.236629169,2.490655005,1.970075703));
#107459=CARTESIAN_POINT('Ctrl Pts',(-7.128772338,2.556411293,2.366263468));
#107460=CARTESIAN_POINT('Ctrl Pts',(-6.978309144,2.621296797,2.748308842));
#107461=CARTESIAN_POINT('Ctrl Pts',(-6.929189456,2.490655005,2.132799448));
#107462=CARTESIAN_POINT('Ctrl Pts',(-6.812423898,2.556411293,2.512155639));
#107463=CARTESIAN_POINT('Ctrl Pts',(-6.654942689,2.621296797,2.87649749));
#107464=CARTESIAN_POINT('Origin',(0.190164101466889,2.41076917337337,-0.0446170585626998));
#107465=CARTESIAN_POINT('Ctrl Pts',(-6.79534933510274,2.62578637467629,
3.17518495546536));
#107466=CARTESIAN_POINT('Ctrl Pts',(-6.78937137745835,2.62354158583815,
3.18785501350895));
#107467=CARTESIAN_POINT('Ctrl Pts',(-6.78339341981399,2.621296797,3.20052507155255));
#107468=CARTESIAN_POINT('Ctrl Pts',(-6.60947051893525,2.555986835,3.56914816665374));
#107469=CARTESIAN_POINT('Ctrl Pts',(-6.39662633629009,2.49066265,3.91675356870698));
#107470=CARTESIAN_POINT('Ctrl Pts',(-6.66568816340674,2.62578637467629,
2.85163721580644));
#107471=CARTESIAN_POINT('Ctrl Pts',(-6.6603154262033,2.62354158583815,2.86406735290325));
#107472=CARTESIAN_POINT('Ctrl Pts',(-6.65494268900001,2.621296797,2.87649749));
#107473=CARTESIAN_POINT('Ctrl Pts',(-6.498628092,2.555986835,3.238140317));
#107474=CARTESIAN_POINT('Ctrl Pts',(-6.304044932,2.49066265,3.580714662));
#107475=CARTESIAN_POINT('Ctrl Pts',(-6.66439419721497,2.62578637467629,
2.84840833987498));
#107476=CARTESIAN_POINT('Ctrl Pts',(-6.65902749986742,2.62354158583815,
2.86083608265752));
#107477=CARTESIAN_POINT('Ctrl Pts',(-6.65366080252,2.621296797,2.87326382544));
#107478=CARTESIAN_POINT('Ctrl Pts',(-6.49752192928999,2.555986835,3.23483699218));
#107479=CARTESIAN_POINT('Ctrl Pts',(-6.30312100693,2.49066265,3.57736112926));
#107480=CARTESIAN_POINT('',(-6.30636142167443,2.49144077994544,3.57663330547932));
#107481=CARTESIAN_POINT('Origin',(0.178440093734786,2.55357123951412,-0.0893582737754317));
#107482=CARTESIAN_POINT('Ctrl Pts',(-6.52364787265427,2.53084202104553,
3.70027275048277));
#107483=CARTESIAN_POINT('Ctrl Pts',(-6.48741633343293,2.5245896082618,3.67961353455242));
#107484=CARTESIAN_POINT('Ctrl Pts',(-6.45117555386211,2.5181850433564,3.65896921127779));
#107485=CARTESIAN_POINT('Ctrl Pts',(-6.37875930532489,2.5050621489458,3.61776185602896));
#107486=CARTESIAN_POINT('Ctrl Pts',(-6.34254230674421,2.4983362995596,3.59717518928135));
#107487=CARTESIAN_POINT('Ctrl Pts',(-6.30636141925216,2.49144078088254,
3.57663330943117));
#107488=CARTESIAN_POINT('Ctrl Pts',(-6.643932759,2.490655005,3.479677786));
#107489=CARTESIAN_POINT('Ctrl Pts',(-6.453428903,2.556411293,3.84341687));
#107490=CARTESIAN_POINT('Ctrl Pts',(-6.224354992,2.621296797,4.184185097));
#107491=CARTESIAN_POINT('Ctrl Pts',(-6.308700021,2.490655005,3.572506689));
#107492=CARTESIAN_POINT('Ctrl Pts',(-6.113114009,2.556411293,3.9178926));
#107493=CARTESIAN_POINT('Ctrl Pts',(-5.880991895,2.621296797,4.239862537));
#107494=CARTESIAN_POINT('Origin',(0.176126986800866,2.41076917395093,-0.0844537108595922));
#107495=CARTESIAN_POINT('Ctrl Pts',(-5.95390693584867,2.62578637476293,
4.56175013253003));
#107496=CARTESIAN_POINT('Ctrl Pts',(-5.94534505143132,2.62354158588146,
4.57283888770188));
#107497=CARTESIAN_POINT('Ctrl Pts',(-5.93678316701407,2.621296797,4.58392764287384));
#107498=CARTESIAN_POINT('Ctrl Pts',(-5.68768341845483,2.555986835,4.90654425278669));
#107499=CARTESIAN_POINT('Ctrl Pts',(-5.40509052821108,2.49066265,5.20026762634116));
#107500=CARTESIAN_POINT('Ctrl Pts',(-5.89683037055794,2.62578637476292,
4.2178934411378));
#107501=CARTESIAN_POINT('Ctrl Pts',(-5.88891113277903,2.62354158588146,
4.22887798906888));
#107502=CARTESIAN_POINT('Ctrl Pts',(-5.880991895,2.621296797,4.239862537));
#107503=CARTESIAN_POINT('Ctrl Pts',(-5.650589329,2.555986835,4.559447338));
#107504=CARTESIAN_POINT('Ctrl Pts',(-5.386912058,2.49066265,4.852182858));
#107505=CARTESIAN_POINT('Ctrl Pts',(-5.89626076945952,2.62578637476292,
4.21446189006023));
#107506=CARTESIAN_POINT('Ctrl Pts',(-5.88834794503479,2.62354158588146,
4.22544539804511));
#107507=CARTESIAN_POINT('Ctrl Pts',(-5.88043512061,2.621296797,4.23642890603));
#107508=CARTESIAN_POINT('Ctrl Pts',(-5.65021914495,2.555986835,4.5559834508));
#107509=CARTESIAN_POINT('Ctrl Pts',(-5.38673064420001,2.49066265,4.84870911242));
#107510=CARTESIAN_POINT('',(-5.39005175947313,2.49144077988329,4.848694897278));
#107511=CARTESIAN_POINT('Origin',(0.155058782873332,2.55357125459944,-0.125628383699805));
#107512=CARTESIAN_POINT('Ctrl Pts',(-5.57567934822786,2.53084202100795,
5.01615388492042));
#107513=CARTESIAN_POINT('Ctrl Pts',(-5.54473600627949,2.52458960887614,
4.98818896292234));
#107514=CARTESIAN_POINT('Ctrl Pts',(-5.51378043344695,2.51818504360533,
4.96023659441289));
#107515=CARTESIAN_POINT('Ctrl Pts',(-5.45191559857526,2.50506214888001,
4.90442529013533));
#107516=CARTESIAN_POINT('Ctrl Pts',(-5.42097085769936,2.49833629937661,
4.8765343436698));
#107517=CARTESIAN_POINT('Ctrl Pts',(-5.39005175646082,2.49144078071805,
4.84869490041678));
#107518=CARTESIAN_POINT('Ctrl Pts',(-5.740573438,2.490655005,4.826574003));
#107519=CARTESIAN_POINT('Ctrl Pts',(-5.476330305,2.556411293,5.140856372));
#107520=CARTESIAN_POINT('Ctrl Pts',(-5.179356919,2.621296797,5.424413508));
#107521=CARTESIAN_POINT('Ctrl Pts',(-5.393222785,2.490655005,4.845167489));
#107522=CARTESIAN_POINT('Ctrl Pts',(-5.12796170400001,2.556411293,5.140433258));
#107523=CARTESIAN_POINT('Ctrl Pts',(-4.832052457,2.621296797,5.404976323));
#107524=CARTESIAN_POINT('Origin',(0.153854054401565,2.41076917057774,-0.120341188345526));
#107525=CARTESIAN_POINT('Ctrl Pts',(-4.83406646628012,2.62578637475954,
5.73501294467684));
#107526=CARTESIAN_POINT('Ctrl Pts',(-4.82332099939218,2.62354158587977,
5.74400189885379));
#107527=CARTESIAN_POINT('Ctrl Pts',(-4.81257553250423,2.621296797,5.75299085303078));
#107528=CARTESIAN_POINT('Ctrl Pts',(-4.49994656305008,2.555986835,6.01451578350814));
#107529=CARTESIAN_POINT('Ctrl Pts',(-4.16081869483508,2.49066265,6.24062295031996));
#107530=CARTESIAN_POINT('Ctrl Pts',(-4.8522433440357,2.62578637475954,5.38692565646089));
#107531=CARTESIAN_POINT('Ctrl Pts',(-4.84214790051785,2.62354158587977,
5.39595098973051));
#107532=CARTESIAN_POINT('Ctrl Pts',(-4.832052457,2.621296797,5.404976323));
#107533=CARTESIAN_POINT('Ctrl Pts',(-4.538335289,2.555986835,5.667559668));
#107534=CARTESIAN_POINT('Ctrl Pts',(-4.217893162,2.49066265,5.896768375));
#107535=CARTESIAN_POINT('Ctrl Pts',(-4.85242474194361,2.62578637475954,
5.38345188573355));
#107536=CARTESIAN_POINT('Ctrl Pts',(-4.84233578539682,2.62354158587977,
5.39247758205185));
#107537=CARTESIAN_POINT('Ctrl Pts',(-4.83224682884999,2.621296797,5.40150327837001));
#107538=CARTESIAN_POINT('Ctrl Pts',(-4.538718393,2.555986835,5.66409718592));
#107539=CARTESIAN_POINT('Ctrl Pts',(-4.21846274216001,2.49066265,5.89333684504));
#107540=CARTESIAN_POINT('',(-4.22170926802651,2.49144077988097,5.89403690448083));
#107541=CARTESIAN_POINT('Origin',(0.1244271772488,2.55357125499674,-0.156024291756064));
#107542=CARTESIAN_POINT('Ctrl Pts',(-4.36699825526782,2.53084202105966,
6.09748523879666));
#107543=CARTESIAN_POINT('Ctrl Pts',(-4.34279002162134,2.52458961891928,
6.06352227161413));
#107544=CARTESIAN_POINT('Ctrl Pts',(-4.318567084774,2.5181850484725,6.02956885146575));
#107545=CARTESIAN_POINT('Ctrl Pts',(-4.27014637778942,2.50506214891138,
5.96176324873251));
#107546=CARTESIAN_POINT('Ctrl Pts',(-4.24592083658121,2.49833629941155,
5.92787217255079));
#107547=CARTESIAN_POINT('Ctrl Pts',(-4.22170926388744,2.49144078076664,
5.89403690726214));
#107548=CARTESIAN_POINT('Ctrl Pts',(-4.568791283,2.490655005,5.947784984));
#107549=CARTESIAN_POINT('Ctrl Pts',(-4.243164588,2.556411293,6.197915143));
#107550=CARTESIAN_POINT('Ctrl Pts',(-3.892177873,2.621296797,6.411002371));
#107551=CARTESIAN_POINT('Ctrl Pts',(-4.225564445,2.490655005,5.891273642));
#107552=CARTESIAN_POINT('Ctrl Pts',(-3.903031608,2.556411293,6.12261297));
#107553=CARTESIAN_POINT('Ctrl Pts',(-3.557171616,2.621296797,6.317359424));
#107554=CARTESIAN_POINT('Origin',(0.124387267833697,2.41076918495438,-0.150601809272185));
#107555=CARTESIAN_POINT('Ctrl Pts',(-3.48819042137609,2.6257863746852,6.64011292507194));
#107556=CARTESIAN_POINT('Ctrl Pts',(-3.47576381827505,2.6235415858426,6.64658176465048));
#107557=CARTESIAN_POINT('Ctrl Pts',(-3.463337215174,2.621296797,6.65305060422905));
#107558=CARTESIAN_POINT('Ctrl Pts',(-3.10179720708206,2.555986835,6.84125524024733));
#107559=CARTESIAN_POINT('Ctrl Pts',(-2.72199160358742,2.49066265,6.98917368021648));
#107560=CARTESIAN_POINT('Ctrl Pts',(-3.58077081065142,2.62578637468521,
6.30407121606756));
#107561=CARTESIAN_POINT('Ctrl Pts',(-3.56897121332571,2.6235415858426,6.31071532003383));
#107562=CARTESIAN_POINT('Ctrl Pts',(-3.557171616,2.621296797,6.317359424));
#107563=CARTESIAN_POINT('Ctrl Pts',(-3.213873735,2.555986835,6.51066320800001));
#107564=CARTESIAN_POINT('Ctrl Pts',(-2.851650271,2.49066265,6.66562755700001));
#107565=CARTESIAN_POINT('Ctrl Pts',(-3.58169472559192,2.62578637468521,
6.30071765536171));
#107566=CARTESIAN_POINT('Ctrl Pts',(-3.56990138553099,2.6235415858426,6.30736350839596));
#107567=CARTESIAN_POINT('Ctrl Pts',(-3.55810804547,2.621296797,6.31400936143));
#107568=CARTESIAN_POINT('Ctrl Pts',(-3.21499221354,2.555986835,6.50736403287));
#107569=CARTESIAN_POINT('Ctrl Pts',(-2.8529442122,2.49066265,6.6623986972));
#107570=CARTESIAN_POINT('',(-2.85596434332632,2.49144077993471,6.66378029754127));
#107571=CARTESIAN_POINT('Origin',(0.0879774927781977,2.55357123324615,-0.17912462577321));
#107572=CARTESIAN_POINT('Ctrl Pts',(-2.9541211766701,2.53084202101462,6.89370495986537));
#107573=CARTESIAN_POINT('Ctrl Pts',(-2.93777995225721,2.52458961891118,
6.85533197352984));
#107574=CARTESIAN_POINT('Ctrl Pts',(-2.9214223160308,2.51818504848243,6.81696515014835));
#107575=CARTESIAN_POINT('Ctrl Pts',(-2.88870985871748,2.50506214891889,
6.74033578394755));
#107576=CARTESIAN_POINT('Ctrl Pts',(-2.87233627702697,2.49833629948779,
6.70202928740089));
#107577=CARTESIAN_POINT('Ctrl Pts',(-2.85596433928416,2.49144078079788,
6.66378029911584));
#107578=CARTESIAN_POINT('Ctrl Pts',(-3.183377525,2.490655005,6.79088415));
#107579=CARTESIAN_POINT('Ctrl Pts',(-2.811593211,2.556411293,6.965166291));
#107580=CARTESIAN_POINT('Ctrl Pts',(-2.423004915,2.621296797,7.097819889));
#107581=CARTESIAN_POINT('Ctrl Pts',(-2.860323408,2.490655005,6.661910387));
#107582=CARTESIAN_POINT('Ctrl Pts',(-2.495600093,2.556411293,6.818506104));
#107583=CARTESIAN_POINT('Ctrl Pts',(-2.115961384,2.621296797,6.93434982));
#107584=CARTESIAN_POINT('Origin',(0.0891042866592537,2.41076916744523,-0.173820589646979));
#107585=CARTESIAN_POINT('Ctrl Pts',(-1.9792104682936,2.6257863746344,7.23472860556905));
#107586=CARTESIAN_POINT('Ctrl Pts',(-1.96568378315313,2.6235415858172,7.2383748548763));
#107587=CARTESIAN_POINT('Ctrl Pts',(-1.95215709801272,2.621296797,7.24202110418352));
#107588=CARTESIAN_POINT('Ctrl Pts',(-1.5586112616565,2.555986835,7.34810520522353));
#107589=CARTESIAN_POINT('Ctrl Pts',(-1.15588720928485,2.49066265,7.41091841655395));
#107590=CARTESIAN_POINT('Ctrl Pts',(-2.14186541422032,2.6257863746344,6.92644541242964));
#107591=CARTESIAN_POINT('Ctrl Pts',(-2.12891339911013,2.6235415858172,6.93039761621488));
#107592=CARTESIAN_POINT('Ctrl Pts',(-2.115961384,2.621296797,6.93434982));
#107593=CARTESIAN_POINT('Ctrl Pts',(-1.739135017,2.555986835,7.049335371));
#107594=CARTESIAN_POINT('Ctrl Pts',(-1.352067382,2.49066265,7.122809403));
#107595=CARTESIAN_POINT('Ctrl Pts',(-2.14348864497014,2.6257863746344,6.92336887051507));
#107596=CARTESIAN_POINT('Ctrl Pts',(-2.13054236483504,2.6235415858172,6.9273241276026));
#107597=CARTESIAN_POINT('Ctrl Pts',(-2.1175960847,2.621296797,6.93127938469));
#107598=CARTESIAN_POINT('Ctrl Pts',(-1.74093657126,2.555986835,7.04635376857));
#107599=CARTESIAN_POINT('Ctrl Pts',(-1.35402518099,2.49066265,7.11993419126));
#107600=CARTESIAN_POINT('',(-1.35667770051763,2.49144077987293,7.1219327287485));
#107601=CARTESIAN_POINT('Origin',(0.0474141679670559,2.5535712289894,-0.19384950688544));
#107602=CARTESIAN_POINT('Ctrl Pts',(-1.40311267532108,2.53084202106957,
7.36758269842034));
#107603=CARTESIAN_POINT('Ctrl Pts',(-1.39540254430667,2.52458960834639,
7.32659390134295));
#107604=CARTESIAN_POINT('Ctrl Pts',(-1.38767508043641,2.51818504337406,
7.2856077020964));
#107605=CARTESIAN_POINT('Ctrl Pts',(-1.37220047685122,2.50506214890662,
7.2037377083547));
#107606=CARTESIAN_POINT('Ctrl Pts',(-1.36444446486421,2.49833629945179,
7.16280696022082));
#107607=CARTESIAN_POINT('Ctrl Pts',(-1.35667769591991,2.49144078077239,
7.1219327294704));
#107608=CARTESIAN_POINT('Ctrl Pts',(-1.649112573,2.490655005,7.31644912000001));
#107609=CARTESIAN_POINT('Ctrl Pts',(-1.248554861,2.556411293,7.406734004));
#107610=CARTESIAN_POINT('Ctrl Pts',(-0.840534941,2.621296797,7.45275123800001));
#107611=CARTESIAN_POINT('Ctrl Pts',(-1.361336828,2.490655005,7.121043606));
#107612=CARTESIAN_POINT('Ctrl Pts',(-0.971477090999999,2.556411293,7.195573471));
#107613=CARTESIAN_POINT('Ctrl Pts',(-0.575811149,2.621296797,7.227097725));
#107614=CARTESIAN_POINT('Origin',(0.0496547889975075,2.4107691558232,-0.188911435488969));
#107615=CARTESIAN_POINT('Ctrl Pts',(-0.377684835313728,2.62578637475243,
7.49105641693586));
#107616=CARTESIAN_POINT('Ctrl Pts',(-0.363690560360698,2.62354158587621,
7.49170958152756));
#107617=CARTESIAN_POINT('Ctrl Pts',(-0.349696285407675,2.621296797,7.49236274611938));
#107618=CARTESIAN_POINT('Ctrl Pts',(0.0574536141148712,2.555986835,7.51136593841204));
#107619=CARTESIAN_POINT('Ctrl Pts',(0.464265185679254,2.49066265,7.48613684418663));
#107620=CARTESIAN_POINT('Ctrl Pts',(-0.602808772041866,2.62578637475243,
7.22494671878989));
#107621=CARTESIAN_POINT('Ctrl Pts',(-0.589309960520928,2.62354158587621,
7.226022221895));
#107622=CARTESIAN_POINT('Ctrl Pts',(-0.575811149000001,2.621296797,7.227097725));
#107623=CARTESIAN_POINT('Ctrl Pts',(-0.183076279,2.555986835,7.258388448));
#107624=CARTESIAN_POINT('Ctrl Pts',(0.210736675,2.49066265,7.246936598));
#107625=CARTESIAN_POINT('Ctrl Pts',(-0.60505541812148,2.62578637475243,
7.2222910513438));
#107626=CARTESIAN_POINT('Ctrl Pts',(-0.591561551125732,2.62354158587621,
7.22337076921702));
#107627=CARTESIAN_POINT('Ctrl Pts',(-0.57806768413,2.621296797,7.22445048709));
#107628=CARTESIAN_POINT('Ctrl Pts',(-0.18547667031,2.555986835,7.25586383469));
#107629=CARTESIAN_POINT('Ctrl Pts',(0.20820656273,2.49066265,7.24454947603));
#107630=CARTESIAN_POINT('Origin',(0.00463374273099309,2.55357126605449,
-0.199509935815785));
#107631=CARTESIAN_POINT('Ctrl Pts',(-1.34892079,3.267335925,7.123405976));
#107632=CARTESIAN_POINT('Ctrl Pts',(-0.962430673,3.331598135,7.19659351500001));
#107633=CARTESIAN_POINT('Ctrl Pts',(-0.57029087,3.396744076,7.227535425));
#107634=CARTESIAN_POINT('Ctrl Pts',(-1.153013899,3.267335925,7.410840637));
#107635=CARTESIAN_POINT('Ctrl Pts',(-0.750928622000001,3.331598135,7.47339898));
#107636=CARTESIAN_POINT('Ctrl Pts',(-0.344435225,3.396744076,7.492086784));
#107637=CARTESIAN_POINT('',(-0.574977342003353,3.39596551435623,7.22716410679017));
#107638=CARTESIAN_POINT('Ctrl Pts',(-0.574977341341557,3.39596551348928,
7.22716410851735));
#107639=CARTESIAN_POINT('Ctrl Pts',(-0.577947813433749,3.3891302450623,
7.26866336228872));
#107640=CARTESIAN_POINT('Ctrl Pts',(-0.580902909912182,3.38247027236386,
7.3102192791635));
#107641=CARTESIAN_POINT('Ctrl Pts',(-0.586879657064628,3.36926348332785,
7.39477921946042));
#107642=CARTESIAN_POINT('Ctrl Pts',(-0.589803775723335,3.36293886744668,
7.43643676797683));
#107643=CARTESIAN_POINT('Ctrl Pts',(-0.592606977972659,3.35698786876839,
7.47655114138138));
#107644=CARTESIAN_POINT('Origin',(0.001144562001206,3.48208295609875,-0.19502964771908));
#107645=CARTESIAN_POINT('Ctrl Pts',(-2.119693429,3.396737969,6.933209918));
#107646=CARTESIAN_POINT('Ctrl Pts',(-2.003146542,3.376870318,6.968841851));
#107647=CARTESIAN_POINT('Ctrl Pts',(-1.885467899,3.357142857,7.000536465));
#107648=CARTESIAN_POINT('Ctrl Pts',(-1.619528158,3.312561141,7.072162525));
#107649=CARTESIAN_POINT('Ctrl Pts',(-1.34892079,3.267335925,7.123405976));
#107650=CARTESIAN_POINT('Ctrl Pts',(-2.426824903,3.396737969,7.0965147));
#107651=CARTESIAN_POINT('Ctrl Pts',(-2.307532871,3.376870318,7.137309497));
#107652=CARTESIAN_POINT('Ctrl Pts',(-2.186937109,3.357142857,7.174071792));
#107653=CARTESIAN_POINT('Ctrl Pts',(-1.914405023,3.312561141,7.25715021));
#107654=CARTESIAN_POINT('Ctrl Pts',(-1.63635545,3.267335925,7.31931286700001));
#107655=CARTESIAN_POINT('',(-2.1151613392112,3.39596551386392,6.93459389680009));
#107656=CARTESIAN_POINT('Ctrl Pts',(-2.11516133429227,3.39596551252257,
6.93459389798702));
#107657=CARTESIAN_POINT('Ctrl Pts',(-2.03883838298854,3.38295904388416,
6.95787361101831));
#107658=CARTESIAN_POINT('Ctrl Pts',(-1.96225208742926,3.37001483652073,
6.97985603265297));
#107659=CARTESIAN_POINT('Ctrl Pts',(-1.88546790027978,3.35714285716407,
7.0005364649097));
#107660=CARTESIAN_POINT('Ctrl Pts',(-1.7428577927959,3.33323592504676,7.03894591890685));
#107661=CARTESIAN_POINT('Ctrl Pts',(-1.59858079503118,3.30907960191736,
7.07312617265287));
#107662=CARTESIAN_POINT('Ctrl Pts',(-1.45302067817422,3.2847386775838,7.1029029922699));
#107663=CARTESIAN_POINT('Ctrl Pts',(-1.41839143496263,3.27894788950982,
7.1099869981834));
#107664=CARTESIAN_POINT('Ctrl Pts',(-1.38368968313904,3.2731466708905,7.11682198006919));
#107665=CARTESIAN_POINT('Ctrl Pts',(-1.34892079120537,3.267335925,7.12340597682154));
#107666=CARTESIAN_POINT('Ctrl Pts',(-2.18598964688771,3.35698786872379,
7.17436054715959));
#107667=CARTESIAN_POINT('Ctrl Pts',(-2.174628554927,3.36293887920927,7.13578655462272));
#107668=CARTESIAN_POINT('Ctrl Pts',(-2.16281771494842,3.369263464767,7.09573172665881));
#107669=CARTESIAN_POINT('Ctrl Pts',(-2.13880288145924,3.38247021625705,
7.01443380632259));
#107670=CARTESIAN_POINT('Ctrl Pts',(-2.12698352521173,3.38913021761768,
6.97448451705911));
#107671=CARTESIAN_POINT('Ctrl Pts',(-2.11516134064853,3.3959655135504,6.93459389632039));
#107672=CARTESIAN_POINT('Ctrl Pts',(-2.84870549,3.267335925,6.666886607));
#107673=CARTESIAN_POINT('Ctrl Pts',(-2.486984455,3.331598135,6.821447013));
#107674=CARTESIAN_POINT('Ctrl Pts',(-2.110664259,3.396744076,6.935963984));
#107675=CARTESIAN_POINT('Ctrl Pts',(-2.719168749,3.267335925,6.989715396));
#107676=CARTESIAN_POINT('Ctrl Pts',(-2.339932197,3.331598135,7.137247609));
#107677=CARTESIAN_POINT('Ctrl Pts',(-1.946959715,3.396744076,7.242882566));
#107678=CARTESIAN_POINT('Origin',(0.0430438123304711,3.48208225451749,-0.190224481412699));
#107679=CARTESIAN_POINT('Ctrl Pts',(-3.560571363,3.396737969,6.315443893));
#107680=CARTESIAN_POINT('Ctrl Pts',(-3.45440909,3.376870318,6.375296907));
#107681=CARTESIAN_POINT('Ctrl Pts',(-3.346295113,3.357142857,6.431547949));
#107682=CARTESIAN_POINT('Ctrl Pts',(-3.101970381,3.312561141,6.558668615));
#107683=CARTESIAN_POINT('Ctrl Pts',(-2.84870549,3.267335925,6.666886607));
#107684=CARTESIAN_POINT('Ctrl Pts',(-3.895627974,3.396737969,6.408906513));
#107685=CARTESIAN_POINT('Ctrl Pts',(-3.787894599,3.376870318,6.47439181));
#107686=CARTESIAN_POINT('Ctrl Pts',(-3.678021106,3.357142857,6.536219148));
#107687=CARTESIAN_POINT('Ctrl Pts',(-3.429720073,3.312561141,6.67594158));
#107688=CARTESIAN_POINT('Ctrl Pts',(-3.171534278,3.267335925,6.796423348));
#107689=CARTESIAN_POINT('',(-3.55644274497419,3.39596551373282,6.31776978094853));
#107690=CARTESIAN_POINT('Ctrl Pts',(-3.55644274019271,3.39596551234443,
6.31776978329846));
#107691=CARTESIAN_POINT('Ctrl Pts',(-3.48690862792311,3.38295904375008,
6.35691240809697));
#107692=CARTESIAN_POINT('Ctrl Pts',(-3.41683844837133,3.37001483645008,
6.39484468269108));
#107693=CARTESIAN_POINT('Ctrl Pts',(-3.34629511471059,3.35714285726472,
6.43154794832714));
#107694=CARTESIAN_POINT('Ctrl Pts',(-3.21527588556531,3.3332358953807,6.49971645300047));
#107695=CARTESIAN_POINT('Ctrl Pts',(-3.08171957845639,3.30907954184599,
6.56411295660272));
#107696=CARTESIAN_POINT('Ctrl Pts',(-2.94596353678932,3.28473858662282,
6.62448479822373));
#107697=CARTESIAN_POINT('Ctrl Pts',(-2.91366692831899,3.27894782923934,
6.63884736881376));
#107698=CARTESIAN_POINT('Ctrl Pts',(-2.88124597494332,3.27314664142021,
6.65298232703042));
#107699=CARTESIAN_POINT('Ctrl Pts',(-2.84870549797431,3.26733592642396,
6.66688660359265));
#107700=CARTESIAN_POINT('Ctrl Pts',(-3.67715786822643,3.35698786876754,
6.53670482815668));
#107701=CARTESIAN_POINT('Ctrl Pts',(-3.65777016219896,3.36293886754113,
6.50147504251046));
#107702=CARTESIAN_POINT('Ctrl Pts',(-3.63762475105133,3.36926348416743,
6.4648954769089));
#107703=CARTESIAN_POINT('Ctrl Pts',(-3.59669478159549,3.38247021621516,
6.39066084503493));
#107704=CARTESIAN_POINT('Ctrl Pts',(-3.57656383913318,3.38913021755435,
6.35418636013907));
#107705=CARTESIAN_POINT('Ctrl Pts',(-3.55644274658362,3.3959655134553,6.31776978008172));
#107706=CARTESIAN_POINT('Ctrl Pts',(-4.215287887,3.267335925,5.89863103));
#107707=CARTESIAN_POINT('Ctrl Pts',(-3.895249607,3.331598135,6.127337229));
#107708=CARTESIAN_POINT('Ctrl Pts',(-3.552345332,3.396744076,6.320074576));
#107709=CARTESIAN_POINT('Ctrl Pts',(-4.15817829,3.267335925,6.241758831));
#107710=CARTESIAN_POINT('Ctrl Pts',(-3.819523143,3.331598135,6.467366471));
#107711=CARTESIAN_POINT('Ctrl Pts',(-3.458446532,3.396744076,6.65500921));
#107712=CARTESIAN_POINT('Origin',(0.082930151739517,3.48208255747605,-0.176524157443751));
#107713=CARTESIAN_POINT('Ctrl Pts',(-4.834960937,3.396737969,5.402374731));
#107714=CARTESIAN_POINT('Ctrl Pts',(-4.744147307,3.376870318,5.483650165));
#107715=CARTESIAN_POINT('Ctrl Pts',(-4.650653287,3.357142857,5.561827398));
#107716=CARTESIAN_POINT('Ctrl Pts',(-4.439367916,3.312561141,5.738498649));
#107717=CARTESIAN_POINT('Ctrl Pts',(-4.215287887,3.267335925,5.89863103000001));
#107718=CARTESIAN_POINT('Ctrl Pts',(-5.182275811,3.396737969,5.421624979));
#107719=CARTESIAN_POINT('Ctrl Pts',(-5.091138586,3.376870318,5.508738758));
#107720=CARTESIAN_POINT('Ctrl Pts',(-4.997124924,3.357142857,5.59274016));
#107721=CARTESIAN_POINT('Ctrl Pts',(-4.784665224,3.312561141,5.782573342));
#107722=CARTESIAN_POINT('Ctrl Pts',(-4.558415688,3.267335925,5.955740627));
#107723=CARTESIAN_POINT('',(-4.83142884097952,3.39596551373665,5.40553377166376));
#107724=CARTESIAN_POINT('Ctrl Pts',(-4.83142883691769,3.39596551243094,
5.40553377475887));
#107725=CARTESIAN_POINT('Ctrl Pts',(-4.77193490002935,3.38295904377871,
5.45870904546908));
#107726=CARTESIAN_POINT('Ctrl Pts',(-4.71165724017725,3.37001483644787,
5.51081750187918));
#107727=CARTESIAN_POINT('Ctrl Pts',(-4.65065328796363,3.35714285717796,
5.56182739730548));
#107728=CARTESIAN_POINT('Ctrl Pts',(-4.53735147580372,3.33323590524741,
5.65656738232091));
#107729=CARTESIAN_POINT('Ctrl Pts',(-4.42076103529562,3.30907956178187,
5.74816895335652));
#107730=CARTESIAN_POINT('Ctrl Pts',(-4.30115710773929,3.28473861678128,
5.83631283751082));
#107731=CARTESIAN_POINT('Ctrl Pts',(-4.27270305300004,3.27894784890599,
5.8572824741766));
#107732=CARTESIAN_POINT('Ctrl Pts',(-4.24407862990798,3.27314665055719,
5.87805654968572));
#107733=CARTESIAN_POINT('Ctrl Pts',(-4.21528788727099,3.267335925,5.89863103004511));
#107734=CARTESIAN_POINT('Ctrl Pts',(-4.99638627566226,3.3569878687369,5.59340005602189));
#107735=CARTESIAN_POINT('Ctrl Pts',(-4.96987847846357,3.36293886806068,
5.56316170399128));
#107736=CARTESIAN_POINT('Ctrl Pts',(-4.9423405379198,3.36926348296273,5.5317680247819));
#107737=CARTESIAN_POINT('Ctrl Pts',(-4.88640923164213,3.38247021622749,
5.46806768500484));
#107738=CARTESIAN_POINT('Ctrl Pts',(-4.85890800332103,3.38913021754945,
5.43677351095003));
#107739=CARTESIAN_POINT('Ctrl Pts',(-4.83142884220982,3.39596551347391,
5.40553377052408));
#107740=CARTESIAN_POINT('Ctrl Pts',(-5.38476810800001,3.267335925,4.854562022));
#107741=CARTESIAN_POINT('Ctrl Pts',(-5.121377218,3.331598135,5.14671996700001));
#107742=CARTESIAN_POINT('Ctrl Pts',(-4.827922686,3.396744076,5.408665504));
#107743=CARTESIAN_POINT('Ctrl Pts',(-5.402756036,3.267335925,5.201944561));
#107744=CARTESIAN_POINT('Ctrl Pts',(-5.120517432,3.331598135,5.49507846600001));
#107745=CARTESIAN_POINT('Ctrl Pts',(-4.808220234,3.396744076,5.755955019));
#107746=CARTESIAN_POINT('Origin',(0.11893884844377,3.48208255706764,-0.154569677558902));
#107747=CARTESIAN_POINT('Ctrl Pts',(-5.883273111,3.396737969,4.236696531));
#107748=CARTESIAN_POINT('Ctrl Pts',(-5.81205447,3.376870318,4.335594037));
#107749=CARTESIAN_POINT('Ctrl Pts',(-5.737552082,3.357142857,4.43204198));
#107750=CARTESIAN_POINT('Ctrl Pts',(-5.569185542,3.312561141,4.650002864));
#107751=CARTESIAN_POINT('Ctrl Pts',(-5.384768108,3.267335925,4.854562022));
#107752=CARTESIAN_POINT('Ctrl Pts',(-6.226606191,3.396737969,4.180834288));
#107753=CARTESIAN_POINT('Ctrl Pts',(-6.156326591,3.376870318,4.285503204));
#107754=CARTESIAN_POINT('Ctrl Pts',(-6.082568734,3.357142857,4.387750858));
#107755=CARTESIAN_POINT('Ctrl Pts',(-5.915884747,3.312561141,4.618818401));
#107756=CARTESIAN_POINT('Ctrl Pts',(-5.732150647,3.267335925,4.836574093));
#107757=CARTESIAN_POINT('',(-5.88050269384339,3.3959655137552,4.240541011126));
#107758=CARTESIAN_POINT('Ctrl Pts',(-5.88050269069937,3.39596551248106,
4.24054101494916));
#107759=CARTESIAN_POINT('Ctrl Pts',(-5.83383080093294,3.38295904381877,
4.30526251552692));
#107760=CARTESIAN_POINT('Ctrl Pts',(-5.78616417724815,3.37001483647222,
4.36911062035155));
#107761=CARTESIAN_POINT('Ctrl Pts',(-5.73755208286525,3.35714285718789,
4.43204197906141));
#107762=CARTESIAN_POINT('Ctrl Pts',(-5.64726547606571,3.33323589884546,
4.54892356737364));
#107763=CARTESIAN_POINT('Ctrl Pts',(-5.55309245898912,3.30907954889413,
4.66344707267108));
#107764=CARTESIAN_POINT('Ctrl Pts',(-5.45523310639709,3.28473859731843,
4.77524153924819));
#107765=CARTESIAN_POINT('Ctrl Pts',(-5.43195216929584,3.27894783590822,
4.8018376680362));
#107766=CARTESIAN_POINT('Ctrl Pts',(-5.40846280757583,3.27314664404836,
4.82827943229482));
#107767=CARTESIAN_POINT('Ctrl Pts',(-5.38476810818828,3.267335925,4.85456202199025));
#107768=CARTESIAN_POINT('Ctrl Pts',(-6.08198921329168,3.35698786876477,
4.38855411340845));
#107769=CARTESIAN_POINT('Ctrl Pts',(-6.04960074080444,3.36293887928365,
4.36472106532315));
#107770=CARTESIAN_POINT('Ctrl Pts',(-6.01595806662991,3.36926346429008,
4.33998131233127));
#107771=CARTESIAN_POINT('Ctrl Pts',(-5.9476406162827,3.38247021628422,4.28979375773227));
#107772=CARTESIAN_POINT('Ctrl Pts',(-5.91405502901164,3.38913021762073,
4.26514317521011));
#107773=CARTESIAN_POINT('Ctrl Pts',(-5.88050269485365,3.39596551352586,
4.2405410096845));
#107774=CARTESIAN_POINT('Ctrl Pts',(-6.30246255700001,3.267335925,3.583499089));
#107775=CARTESIAN_POINT('Ctrl Pts',(-6.108034921,3.331598135,3.9254478));
#107776=CARTESIAN_POINT('Ctrl Pts',(-5.877751741,3.396744076,4.244353245));
#107777=CARTESIAN_POINT('Ctrl Pts',(-6.39470691500001,3.267335925,3.918893144));
#107778=CARTESIAN_POINT('Ctrl Pts',(-6.182082017,3.331598135,4.265846698));
#107779=CARTESIAN_POINT('Ctrl Pts',(-5.933166901,3.396744076,4.58775876899999));
#107780=CARTESIAN_POINT('Origin',(0.149385868638626,3.48208259248333,-0.125387490683405));
#107781=CARTESIAN_POINT('Ctrl Pts',(-6.656489974,3.396737969,2.87291511));
#107782=CARTESIAN_POINT('Ctrl Pts',(-6.608196425,3.376870318,2.98481035));
#107783=CARTESIAN_POINT('Ctrl Pts',(-6.556169318,3.357142857,3.095019205));
#107784=CARTESIAN_POINT('Ctrl Pts',(-6.438594242,3.312561141,3.344078114));
#107785=CARTESIAN_POINT('Ctrl Pts',(-6.302462557,3.267335925,3.583499089));
#107786=CARTESIAN_POINT('Ctrl Pts',(-6.979787386,3.396737969,2.744552431));
#107787=CARTESIAN_POINT('Ctrl Pts',(-6.933651607,3.376870318,2.861882283));
#107788=CARTESIAN_POINT('Ctrl Pts',(-6.883598391,3.357142857,2.977595203));
#107789=CARTESIAN_POINT('Ctrl Pts',(-6.770484074,3.312561141,3.239092645));
#107790=CARTESIAN_POINT('Ctrl Pts',(-6.63785661200001,3.267335925,3.491254731));
#107791=CARTESIAN_POINT('',(-6.65461077676593,3.39596551374942,2.87726526625745));
#107792=CARTESIAN_POINT('Ctrl Pts',(-6.65461077492331,3.3959655124626,2.87726527063129));
#107793=CARTESIAN_POINT('Ctrl Pts',(-6.62294325708987,3.3829590439033,2.9505066947672));
#107794=CARTESIAN_POINT('Ctrl Pts',(-6.59011650753996,3.37001483656461,
3.02310898150559));
#107795=CARTESIAN_POINT('Ctrl Pts',(-6.55616931878919,3.35714285729924,
3.09501920332825));
#107796=CARTESIAN_POINT('Ctrl Pts',(-6.49311964373262,3.33323589670651,
3.228577129268));
#107797=CARTESIAN_POINT('Ctrl Pts',(-6.42576750106537,3.30907954446892,
3.36066756582076));
#107798=CARTESIAN_POINT('Ctrl Pts',(-6.35422854380943,3.28473859052526,
3.49088521988956));
#107799=CARTESIAN_POINT('Ctrl Pts',(-6.33720929007269,3.27894783137455,
3.52186424699044));
#107800=CARTESIAN_POINT('Ctrl Pts',(-6.31995330093824,3.27314664177974,
3.55273732373537));
#107801=CARTESIAN_POINT('Ctrl Pts',(-6.30246255717339,3.267335925,3.58349908895232));
#107802=CARTESIAN_POINT('Ctrl Pts',(-6.8832050949221,3.35698786871989,2.97850425893303));
#107803=CARTESIAN_POINT('Ctrl Pts',(-6.84645051598102,3.36293886794177,
2.96219100945032));
#107804=CARTESIAN_POINT('Ctrl Pts',(-6.80827589352812,3.3692634829752,2.94526175870117));
#107805=CARTESIAN_POINT('Ctrl Pts',(-6.73076693640478,3.38247021625307,
2.91093384222089));
#107806=CARTESIAN_POINT('Ctrl Pts',(-6.69266741499193,3.38913021757927,
2.89407948518823));
#107807=CARTESIAN_POINT('Ctrl Pts',(-6.65461077733531,3.39596551349355,
2.87726526486472));
#107808=CARTESIAN_POINT('Ctrl Pts',(-6.925460861,3.267335925,2.144875721));
#107809=CARTESIAN_POINT('Ctrl Pts',(-6.809087701,3.331598135,2.520626056));
#107810=CARTESIAN_POINT('Ctrl Pts',(-6.652743657,3.396744076,2.881579746));
#107811=CARTESIAN_POINT('Ctrl Pts',(-7.087648405,3.267335925,2.45259864));
#107812=CARTESIAN_POINT('Ctrl Pts',(-6.954579317,3.331598135,2.837148681));
#107813=CARTESIAN_POINT('Ctrl Pts',(-6.780685278,3.396744076,3.205044018));
#107814=CARTESIAN_POINT('Origin',(0.172847961265036,3.48208254856463,-0.0903424629903771));
#107815=CARTESIAN_POINT('Ctrl Pts',(-7.118456763,3.396737969,1.374799371));
#107816=CARTESIAN_POINT('Ctrl Pts',(-7.095346459,3.376870318,1.494460248));
#107817=CARTESIAN_POINT('Ctrl Pts',(-7.068227363,3.357142857,1.613276771));
#107818=CARTESIAN_POINT('Ctrl Pts',(-7.00694143000001,3.312561141,1.881787987));
#107819=CARTESIAN_POINT('Ctrl Pts',(-6.925460861,3.267335925,2.144875721));
#107820=CARTESIAN_POINT('Ctrl Pts',(-7.40660148,3.396737969,1.179938354));
#107821=CARTESIAN_POINT('Ctrl Pts',(-7.386766779,3.376870318,1.304442928));
#107822=CARTESIAN_POINT('Ctrl Pts',(-7.362758637,3.357142857,1.428210506));
#107823=CARTESIAN_POINT('Ctrl Pts',(-7.308503091,3.312561141,1.707910518));
#107824=CARTESIAN_POINT('Ctrl Pts',(-7.23318378,3.267335925,1.982688177));
#107825=CARTESIAN_POINT('',(-7.11755665579964,3.39596551374277,1.37945179519918));
#107826=CARTESIAN_POINT('Ctrl Pts',(-7.11755665457148,3.39596551231891,
1.37945180024207));
#107827=CARTESIAN_POINT('Ctrl Pts',(-7.10237424704946,3.38295904372266,
1.45778846079517));
#107828=CARTESIAN_POINT('Ctrl Pts',(-7.08592231402127,3.3700148364319,1.53575012695171));
#107829=CARTESIAN_POINT('Ctrl Pts',(-7.06822736368685,3.3571428571178,1.61327676996068));
#107830=CARTESIAN_POINT('Ctrl Pts',(-7.0353627534341,3.33323589104236,1.75726603526585));
#107831=CARTESIAN_POINT('Ctrl Pts',(-6.99798079655694,3.30907953327899,
1.90074702277125));
#107832=CARTESIAN_POINT('Ctrl Pts',(-6.95610731559513,3.28473857385227,
2.04329905286339));
#107833=CARTESIAN_POINT('Ctrl Pts',(-6.94614554674343,3.27894782023285,
2.07721241140201));
#107834=CARTESIAN_POINT('Ctrl Pts',(-6.93592980152675,3.27314663619637,
2.11107318782929));
#107835=CARTESIAN_POINT('Ctrl Pts',(-6.92546086189945,3.267335925,2.14487572052594));
#107836=CARTESIAN_POINT('Ctrl Pts',(-7.36256995641699,3.35698786876322,
1.42918285531943));
#107837=CARTESIAN_POINT('Ctrl Pts',(-7.32316781100546,3.36293886821889,
1.42115214801801));
#107838=CARTESIAN_POINT('Ctrl Pts',(-7.28224641027146,3.36926348187864,
1.41282511087487));
#107839=CARTESIAN_POINT('Ctrl Pts',(-7.19917007545255,3.38247021622246,
1.3959618950794));
#107840=CARTESIAN_POINT('Ctrl Pts',(-7.158338111131,3.38913021755116,1.38769185434494));
#107841=CARTESIAN_POINT('Ctrl Pts',(-7.11755665616871,3.39596551346862,
1.37945179314519));
#107842=CARTESIAN_POINT('Ctrl Pts',(-7.224632313,3.267335925,0.605960349000001));
#107843=CARTESIAN_POINT('Ctrl Pts',(-7.191755107,3.331598135,0.997942639));
#107844=CARTESIAN_POINT('Ctrl Pts',(-7.116660674,3.396744076,1.38406678));
#107845=CARTESIAN_POINT('Ctrl Pts',(-7.449179333,3.267335925,0.871623349000001));
#107846=CARTESIAN_POINT('Ctrl Pts',(-7.401888218,3.331598135,1.275788744));
#107847=CARTESIAN_POINT('Ctrl Pts',(-7.311146348,3.396744076,1.672464971));
#107848=CARTESIAN_POINT('Origin',(0.188227844185853,3.48208256576102,-0.0510731071993649));
#107849=CARTESIAN_POINT('Ctrl Pts',(-7.247572426,3.396737969,-0.187600458));
#107850=CARTESIAN_POINT('Ctrl Pts',(-7.25072598,3.376870318,-0.065769154));
#107851=CARTESIAN_POINT('Ctrl Pts',(-7.249782953,3.357142857,0.056099309));
#107852=CARTESIAN_POINT('Ctrl Pts',(-7.247651826,3.312561141,0.331507546));
#107853=CARTESIAN_POINT('Ctrl Pts',(-7.224632313,3.267335925,0.605960349000001));
#107854=CARTESIAN_POINT('Ctrl Pts',(-7.487091121,3.396737969,-0.43984833));
#107855=CARTESIAN_POINT('Ctrl Pts',(-7.494484947,3.376870318,-0.313990729));
#107856=CARTESIAN_POINT('Ctrl Pts',(-7.497644473,3.357142857,-0.187955727));
#107857=CARTESIAN_POINT('Ctrl Pts',(-7.504784626,3.312561141,0.0968683920000001));
#107858=CARTESIAN_POINT('Ctrl Pts',(-7.490295313,3.267335925,0.381413328));
#107859=CARTESIAN_POINT('',(-7.24769349608873,3.39596551376398,-0.182863309139555));
#107860=CARTESIAN_POINT('Ctrl Pts',(-7.2476934961534,3.39596551248093,-0.182863304051593));
#107861=CARTESIAN_POINT('Ctrl Pts',(-7.2497061112786,3.38295904386738,-0.103094342054963));
#107862=CARTESIAN_POINT('Ctrl Pts',(-7.25039826907839,3.37001483651852,
-0.0234186968749169));
#107863=CARTESIAN_POINT('Ctrl Pts',(-7.24978295327409,3.35714285717451,
0.0560993076602942));
#107864=CARTESIAN_POINT('Ctrl Pts',(-7.24864013544803,3.33323588073399,
0.203787167236864));
#107865=CARTESIAN_POINT('Ctrl Pts',(-7.24297631397189,3.30907951252702,
0.35194972910359));
#107866=CARTESIAN_POINT('Ctrl Pts',(-7.23272627583705,3.28473854237686,
0.500170597084882));
#107867=CARTESIAN_POINT('Ctrl Pts',(-7.23028778066582,3.27894779922121,
0.535432502074355));
#107868=CARTESIAN_POINT('Ctrl Pts',(-7.22758994432299,3.27314662567951,
0.570697651697861));
#107869=CARTESIAN_POINT('Ctrl Pts',(-7.22463231342918,3.267335925,0.605960348637243));
#107870=CARTESIAN_POINT('Ctrl Pts',(-7.49766922997614,3.35698786881975,
-0.186965550244216));
#107871=CARTESIAN_POINT('Ctrl Pts',(-7.4574619215761,3.3629388680623,-0.186338207434659));
#107872=CARTESIAN_POINT('Ctrl Pts',(-7.41570717295739,3.36926348177469,
-0.185673671628998));
#107873=CARTESIAN_POINT('Ctrl Pts',(-7.33094802269087,3.38247021627394,
-0.184283678323024));
#107874=CARTESIAN_POINT('Ctrl Pts',(-7.28929287292059,3.38913021757036,
-0.183582704619095));
#107875=CARTESIAN_POINT('Ctrl Pts',(-7.24769349602485,3.39596551350206,
-0.182863310345163));
#107876=CARTESIAN_POINT('Ctrl Pts',(-7.185987987,3.267335925,-0.961289056000001));
#107877=CARTESIAN_POINT('Ctrl Pts',(-7.238144037,3.331598135,-0.571403467));
#107878=CARTESIAN_POINT('Ctrl Pts',(-7.247810547,3.396744076,-0.17816361));
#107879=CARTESIAN_POINT('Ctrl Pts',(-7.462394915,3.267335925,-0.750108081));
#107880=CARTESIAN_POINT('Ctrl Pts',(-7.503093053,3.331598135,-0.345225657));
#107881=CARTESIAN_POINT('Ctrl Pts',(-7.49974634,3.396744076,0.0616833200000001));
#107882=CARTESIAN_POINT('Origin',(0.194806496690273,3.48208256695309,-0.0094156120496422));
#107883=CARTESIAN_POINT('Ctrl Pts',(-7.03779965700001,3.396737969,-1.741228298));
#107884=CARTESIAN_POINT('Ctrl Pts',(-7.067069611,3.376870318,-1.622923263));
#107885=CARTESIAN_POINT('Ctrl Pts',(-7.09234675,3.357142857,-1.503701295));
#107886=CARTESIAN_POINT('Ctrl Pts',(-7.149470077,3.312561141,-1.234273819));
#107887=CARTESIAN_POINT('Ctrl Pts',(-7.18598798700001,3.267335925,-0.961289056));
#107888=CARTESIAN_POINT('Ctrl Pts',(-7.217492702,3.396737969,-2.039068194));
#107889=CARTESIAN_POINT('Ctrl Pts',(-7.251769329,3.376870318,-1.917742529));
#107890=CARTESIAN_POINT('Ctrl Pts',(-7.281948786,3.357142857,-1.79533336));
#107891=CARTESIAN_POINT('Ctrl Pts',(-7.350150772,3.312561141,-1.518703192));
#107892=CARTESIAN_POINT('Ctrl Pts',(-7.397168962,3.267335925,-1.237695984));
#107893=CARTESIAN_POINT('',(-7.03893624368007,3.39596551376467,-1.73662792753749));
#107894=CARTESIAN_POINT('Ctrl Pts',(-7.03893624466455,3.39596551246643,
-1.73662792249366));
#107895=CARTESIAN_POINT('Ctrl Pts',(-7.05804977456909,3.38295904384934,
-1.65915656746975));
#107896=CARTESIAN_POINT('Ctrl Pts',(-7.07585365883465,3.37001483650869,
-1.58149248836743));
#107897=CARTESIAN_POINT('Ctrl Pts',(-7.09234674982968,3.35714285721031,
-1.50370129642354));
#107898=CARTESIAN_POINT('Ctrl Pts',(-7.1229791605006,3.33323589123215,-1.35922068675125));
#107899=CARTESIAN_POINT('Ctrl Pts',(-7.14929831789834,3.30907953349491,
-1.21330459259));
#107900=CARTESIAN_POINT('Ctrl Pts',(-7.17115101956385,3.28473857395464,
-1.06634565525889));
#107901=CARTESIAN_POINT('Ctrl Pts',(-7.17634981263611,3.27894782030931,
-1.03138388636658));
#107902=CARTESIAN_POINT('Ctrl Pts',(-7.1812960243595,3.27314663623902,-0.99636319779376));
#107903=CARTESIAN_POINT('Ctrl Pts',(-7.18598798717056,3.267335925,-0.961289056223232));
#107904=CARTESIAN_POINT('Ctrl Pts',(-7.28218582307141,3.35698786876996,
-1.79437165487534));
#107905=CARTESIAN_POINT('Ctrl Pts',(-7.24305332634517,3.36293887913784,
-1.78511557887735));
#107906=CARTESIAN_POINT('Ctrl Pts',(-7.20241782122286,3.36926346384614,
-1.77549058655937));
#107907=CARTESIAN_POINT('Ctrl Pts',(-7.11993850864496,3.38247029310111,
-1.75591223833854));
#107908=CARTESIAN_POINT('Ctrl Pts',(-7.07940817845462,3.38913025525282,
-1.74627308796842));
#107909=CARTESIAN_POINT('Ctrl Pts',(-7.0389362434003,3.39596551355439,-1.73662792952758));
#107910=CARTESIAN_POINT('Ctrl Pts',(-6.81133485,3.267335925,-2.483589653));
#107911=CARTESIAN_POINT('Ctrl Pts',(-6.946085397,3.331598135,-2.114031381));
#107912=CARTESIAN_POINT('Ctrl Pts',(-7.040060855,3.396744076,-1.732063268));
#107913=CARTESIAN_POINT('Ctrl Pts',(-7.126677204,3.267335925,-2.336765291));
#107914=CARTESIAN_POINT('Ctrl Pts',(-7.253461596,3.331598135,-1.950097689));
#107915=CARTESIAN_POINT('Ctrl Pts',(-7.337666529,3.396744076,-1.551982574));
#107916=CARTESIAN_POINT('Origin',(0.192275901926948,3.48208255376959,0.0326820931064098));
#107917=CARTESIAN_POINT('Ctrl Pts',(-6.498947198,3.396737969,-3.213438239));
#107918=CARTESIAN_POINT('Ctrl Pts',(-6.552964923,3.376870318,-3.104191285));
#107919=CARTESIAN_POINT('Ctrl Pts',(-6.603280295,3.357142857,-2.993190497));
#107920=CARTESIAN_POINT('Ctrl Pts',(-6.716987053,3.312561141,-2.742341913));
#107921=CARTESIAN_POINT('Ctrl Pts',(-6.81133485,3.267335925,-2.483589653));
#107922=CARTESIAN_POINT('Ctrl Pts',(-6.610412346,3.396737969,-3.542943496));
#107923=CARTESIAN_POINT('Ctrl Pts',(-6.669969036,3.376870318,-3.431822819));
#107924=CARTESIAN_POINT('Ctrl Pts',(-6.725757268,3.357142857,-3.3187632));
#107925=CARTESIAN_POINT('Ctrl Pts',(-6.851832038,3.312561141,-3.063261902));
#107926=CARTESIAN_POINT('Ctrl Pts',(-6.95815921200001,3.267335925,-2.798932008));
#107927=CARTESIAN_POINT('',(-6.50104615569751,3.39596551372471,-3.2091897545298));
#107928=CARTESIAN_POINT('Ctrl Pts',(-6.50104615793014,3.39596551236517,
-3.20918974991457));
#107929=CARTESIAN_POINT('Ctrl Pts',(-6.53636687541928,3.38295904389764,
-3.13763847664817));
#107930=CARTESIAN_POINT('Ctrl Pts',(-6.5704499960716,3.37001483658892,-3.06561744931968));
#107931=CARTESIAN_POINT('Ctrl Pts',(-6.60328029421643,3.35714285730722,
-2.99319049872864));
#107932=CARTESIAN_POINT('Ctrl Pts',(-6.66425557433981,3.33323589990589,
-2.85867287694132));
#107933=CARTESIAN_POINT('Ctrl Pts',(-6.72132703253208,3.30907955088029,
-2.72182611067045));
#107934=CARTESIAN_POINT('Ctrl Pts',(-6.77426064199191,3.28473860015761,
-2.5830007274313));
#107935=CARTESIAN_POINT('Ctrl Pts',(-6.78685365678872,3.27894783780932,
-2.54997388261299));
#107936=CARTESIAN_POINT('Ctrl Pts',(-6.79921266075128,3.27314664500316,
-2.51683519774265));
#107937=CARTESIAN_POINT('Ctrl Pts',(-6.81133485011412,3.267335925,-2.48358965324511));
#107938=CARTESIAN_POINT('Ctrl Pts',(-6.72619550123133,3.35698786876473,
-3.31787493432137));
#107939=CARTESIAN_POINT('Ctrl Pts',(-6.68996775206939,3.3629388678247,-3.30042296335432));
#107940=CARTESIAN_POINT('Ctrl Pts',(-6.65235119061501,3.36926348312789,
-3.28228747871531));
#107941=CARTESIAN_POINT('Ctrl Pts',(-6.57600906312393,3.38247029531356,
-3.24543629492914));
#107942=CARTESIAN_POINT('Ctrl Pts',(-6.53849844885975,3.38913025630653,
-3.22730968299859));
#107943=CARTESIAN_POINT('Ctrl Pts',(-6.50104615482508,3.39596551351214,
-3.20918975625285));
#107944=CARTESIAN_POINT('Ctrl Pts',(-6.118191265,3.267335925,-3.889760358));
#107945=CARTESIAN_POINT('Ctrl Pts',(-6.329235524,3.331598135,-3.557809538));
#107946=CARTESIAN_POINT('Ctrl Pts',(-6.503125741,3.396744076,-3.204973572));
#107947=CARTESIAN_POINT('Ctrl Pts',(-6.45772398800001,3.267335925,-3.814157953));
#107948=CARTESIAN_POINT('Ctrl Pts',(-6.664666336,3.331598135,-3.463785321));
#107949=CARTESIAN_POINT('Ctrl Pts',(-6.832485586,3.396744076,-3.093079487));
#107950=CARTESIAN_POINT('Origin',(0.180754990267068,3.48208253270065,0.0732516867238425));
#107951=CARTESIAN_POINT('Ctrl Pts',(-5.656211191,3.396737969,-4.535391379));
#107952=CARTESIAN_POINT('Ctrl Pts',(-5.732450877,3.376870318,-4.440310772));
#107953=CARTESIAN_POINT('Ctrl Pts',(-5.805451792,3.357142857,-4.342721438));
#107954=CARTESIAN_POINT('Ctrl Pts',(-5.97042518,3.312561141,-4.122181147));
#107955=CARTESIAN_POINT('Ctrl Pts',(-6.118191265,3.267335925,-3.889760358));
#107956=CARTESIAN_POINT('Ctrl Pts',(-5.694236456,3.396737969,-4.881154698));
#107957=CARTESIAN_POINT('Ctrl Pts',(-5.776288404,3.376870318,-4.785434889));
#107958=CARTESIAN_POINT('Ctrl Pts',(-5.855076814,3.357142857,-4.687011361));
#107959=CARTESIAN_POINT('Ctrl Pts',(-6.033129253,3.312561141,-4.464585891));
#107960=CARTESIAN_POINT('Ctrl Pts',(-6.19379367,3.267335925,-4.229293082));
#107961=CARTESIAN_POINT('',(-5.65917437486607,3.39596551372921,-4.5316934355077));
#107962=CARTESIAN_POINT('Ctrl Pts',(-5.6591743779949,3.39596551235788,-4.53169343152599));
#107963=CARTESIAN_POINT('Ctrl Pts',(-5.70905072577702,3.38295904374474,
-4.469407896851));
#107964=CARTESIAN_POINT('Ctrl Pts',(-5.75781939387318,3.37001483644105,
-4.40639754447334));
#107965=CARTESIAN_POINT('Ctrl Pts',(-5.80545179132042,3.35714285719604,
-4.34272143928784));
#107966=CARTESIAN_POINT('Ctrl Pts',(-5.89391873234071,3.33323592234731,
-4.22445675947104));
#107967=CARTESIAN_POINT('Ctrl Pts',(-5.97907382423562,3.3090795962726,-4.1030781881729));
#107968=CARTESIAN_POINT('Ctrl Pts',(-6.06061315891376,3.28473866884692,
-3.97887774869767));
#107969=CARTESIAN_POINT('Ctrl Pts',(-6.08001162970604,3.27894788368063,
-3.94933006343559));
#107970=CARTESIAN_POINT('Ctrl Pts',(-6.09920560139156,3.27314666797384,
-3.91962284618732));
#107971=CARTESIAN_POINT('Ctrl Pts',(-6.11819126506037,3.267335925,-3.88976035827113));
#107972=CARTESIAN_POINT('Ctrl Pts',(-5.85569575257732,3.35698786875252,
-4.68623807017156));
#107973=CARTESIAN_POINT('Ctrl Pts',(-5.82406658291608,3.36293887966387,
-4.66140617195981));
#107974=CARTESIAN_POINT('Ctrl Pts',(-5.79122822973608,3.36926346374271,
-4.63560836239597));
#107975=CARTESIAN_POINT('Ctrl Pts',(-5.72459315521993,3.38247021623446,
-4.58320767478909));
#107976=CARTESIAN_POINT('Ctrl Pts',(-5.69185599036889,3.38913021755001,
-4.5574410118512));
#107977=CARTESIAN_POINT('Ctrl Pts',(-5.65917437376494,3.3959655134616,-4.53169343683433));
#107978=CARTESIAN_POINT('Ctrl Pts',(-5.138967857,3.267335925,-5.114050192));
#107979=CARTESIAN_POINT('Ctrl Pts',(-5.416437632,3.331598135,-4.835228475));
#107980=CARTESIAN_POINT('Ctrl Pts',(-5.662111695,3.396744076,-4.528022874));
#107981=CARTESIAN_POINT('Ctrl Pts',(-5.486814776,3.267335925,-5.11320482800001));
#107982=CARTESIAN_POINT('Ctrl Pts',(-5.764238685,3.331598135,-4.815510201));
#107983=CARTESIAN_POINT('Ctrl Pts',(-6.007825211,3.396744076,-4.489547442));
#107984=CARTESIAN_POINT('Origin',(0.160782004737559,3.48208256640899,0.110395990657645));
#107985=CARTESIAN_POINT('Ctrl Pts',(-4.548997036,3.396737969,-5.64527465800001));
#107986=CARTESIAN_POINT('Ctrl Pts',(-4.6438938,3.376870318,-5.568806262));
#107987=CARTESIAN_POINT('Ctrl Pts',(-4.736166816,3.357142857,-5.489191552));
#107988=CARTESIAN_POINT('Ctrl Pts',(-4.944692861,3.312561141,-5.309271772));
#107989=CARTESIAN_POINT('Ctrl Pts',(-5.138967857,3.267335925,-5.114050192));
#107990=CARTESIAN_POINT('Ctrl Pts',(-4.511804397,3.396737969,-5.991128531));
#107991=CARTESIAN_POINT('Ctrl Pts',(-4.612514947,3.376870318,-5.915285341));
#107992=CARTESIAN_POINT('Ctrl Pts',(-4.710619476,3.357142857,-5.83610008));
#107993=CARTESIAN_POINT('Ctrl Pts',(-4.93232405,3.312561141,-5.657150805));
#107994=CARTESIAN_POINT('Ctrl Pts',(-5.139813221,3.267335925,-5.461897111));
#107995=CARTESIAN_POINT('',(-4.55268589075781,3.39596551376344,-5.64230016798178));
#107996=CARTESIAN_POINT('Ctrl Pts',(-4.55268589439774,3.39596551241353,
-5.64230016474708));
#107997=CARTESIAN_POINT('Ctrl Pts',(-4.61478570966965,3.38295904375274,
-5.59219277144712));
#107998=CARTESIAN_POINT('Ctrl Pts',(-4.67595955649415,3.37001483642585,
-5.54113938813364));
#107999=CARTESIAN_POINT('Ctrl Pts',(-4.73616681521636,3.35714285716618,
-5.48919155275715));
#108000=CARTESIAN_POINT('Ctrl Pts',(-4.84798885387433,3.33323592329174,
-5.39270961640222));
#108001=CARTESIAN_POINT('Ctrl Pts',(-4.95724586759288,3.30907959821499,
-5.29247464058025));
#108002=CARTESIAN_POINT('Ctrl Pts',(-5.06357827707533,3.28473867183283,
-5.18870648985122));
#108003=CARTESIAN_POINT('Ctrl Pts',(-5.0888751057795,3.27894788567283,-5.16401970670844));
#108004=CARTESIAN_POINT('Ctrl Pts',(-5.11400651106192,3.27314666897044,
-5.13913316002725));
#108005=CARTESIAN_POINT('Ctrl Pts',(-5.13896785700169,3.267335925,-5.114050192696));
#108006=CARTESIAN_POINT('Ctrl Pts',(-4.71139017880485,3.35698786875269,
-5.83547792184127));
#108007=CARTESIAN_POINT('Ctrl Pts',(-4.68583860689359,3.36293887935722,
-5.80442724467471));
#108008=CARTESIAN_POINT('Ctrl Pts',(-4.65931375765883,3.36926346474903,
-5.77217329178179));
#108009=CARTESIAN_POINT('Ctrl Pts',(-4.60550117740311,3.38247021619481,
-5.70667313699998));
#108010=CARTESIAN_POINT('Ctrl Pts',(-4.57906846021727,3.3891302175044,-5.67447136160083));
#108011=CARTESIAN_POINT('Ctrl Pts',(-4.55268588945475,3.39596551344277,
-5.64230016898225));
#108012=CARTESIAN_POINT('Ctrl Pts',(-3.919452023,3.267335925,-6.09921272300001));
#108013=CARTESIAN_POINT('Ctrl Pts',(-4.250373136,3.331598135,-5.886557502));
#108014=CARTESIAN_POINT('Ctrl Pts',(-4.5563436,3.396744076,-5.639346859));
#108015=CARTESIAN_POINT('Ctrl Pts',(-4.259348203,3.267335925,-6.173163928));
#108016=CARTESIAN_POINT('Ctrl Pts',(-4.59428164,3.331598135,-5.942067176));
#108017=CARTESIAN_POINT('Ctrl Pts',(-4.902245606,3.396744076,-5.676089148));
#108018=CARTESIAN_POINT('Origin',(0.133291327431939,3.48208259557583,0.142378644240245));
#108019=CARTESIAN_POINT('Ctrl Pts',(-3.229076835,3.396737969,-6.49119116900001));
#108020=CARTESIAN_POINT('Ctrl Pts',(-3.33819341,3.376870318,-6.436910561));
#108021=CARTESIAN_POINT('Ctrl Pts',(-3.445423944,3.357142857,-6.378993169));
#108022=CARTESIAN_POINT('Ctrl Pts',(-3.6877522,3.312561141,-6.248106749));
#108023=CARTESIAN_POINT('Ctrl Pts',(-3.919452023,3.267335925,-6.09921272300001));
#108024=CARTESIAN_POINT('Ctrl Pts',(-3.11840538,3.396737969,-6.820963853));
#108025=CARTESIAN_POINT('Ctrl Pts',(-3.233065417,3.376870318,-6.768543626));
#108026=CARTESIAN_POINT('Ctrl Pts',(-3.345898807,3.357142857,-6.712299246));
#108027=CARTESIAN_POINT('Ctrl Pts',(-3.600888855,3.312561141,-6.585193635));
#108028=CARTESIAN_POINT('Ctrl Pts',(-3.845500817,3.267335925,-6.439108903));
#108029=CARTESIAN_POINT('',(-3.23331887358448,3.39596551379113,-6.48907921538511));
#108030=CARTESIAN_POINT('Ctrl Pts',(-3.23331887791266,3.39596551246019,
-6.48907921306364));
#108031=CARTESIAN_POINT('Ctrl Pts',(-3.30473844184022,3.38295904388523,
-6.45349292782824));
#108032=CARTESIAN_POINT('Ctrl Pts',(-3.37545704658702,3.37001483654186,
-6.41678371308469));
#108033=CARTESIAN_POINT('Ctrl Pts',(-3.44542394259196,3.35714285725904,
-6.37899316976051));
#108034=CARTESIAN_POINT('Ctrl Pts',(-3.57537225490592,3.33323595160592,
-6.3088054431801));
#108035=CARTESIAN_POINT('Ctrl Pts',(-3.70362230820437,3.30907965522593,
-6.23440102649535));
#108036=CARTESIAN_POINT('Ctrl Pts',(-3.82977566596386,3.28473875800089,
-6.15591734453168));
#108037=CARTESIAN_POINT('Ctrl Pts',(-3.85978814753651,3.2789479432148,-6.13724570470757));
#108038=CARTESIAN_POINT('Ctrl Pts',(-3.88968201527148,3.27314669778425,
-6.11834340825996));
#108039=CARTESIAN_POINT('Ctrl Pts',(-3.91945202291905,3.267335925,-6.09921272337206));
#108040=CARTESIAN_POINT('Ctrl Pts',(-3.34678523697663,3.3569878687276,-6.71185731173205));
#108041=CARTESIAN_POINT('Ctrl Pts',(-3.32850605734561,3.36293886864128,
-6.67603981394387));
#108042=CARTESIAN_POINT('Ctrl Pts',(-3.30953490584486,3.36926348259368,
-6.63883771552335));
#108043=CARTESIAN_POINT('Ctrl Pts',(-3.27106108269111,3.38247021625425,
-6.56330090580448));
#108044=CARTESIAN_POINT('Ctrl Pts',(-3.25216877742182,3.38913021759946,
-6.52616973707086));
#108045=CARTESIAN_POINT('Ctrl Pts',(-3.23331887183457,3.39596551355691,
-6.48907921623128));
#108046=CARTESIAN_POINT('Ctrl Pts',(-2.516666969,3.267335925,-6.79918284600001));
#108047=CARTESIAN_POINT('Ctrl Pts',(-2.885565917,3.331598135,-6.662637643));
#108048=CARTESIAN_POINT('Ctrl Pts',(-3.237525941,3.396744076,-6.486981253));
#108049=CARTESIAN_POINT('Ctrl Pts',(-2.832719242,3.267335925,-6.94447274400001));
#108050=CARTESIAN_POINT('Ctrl Pts',(-3.209501092,3.331598135,-6.790779694));
#108051=CARTESIAN_POINT('Ctrl Pts',(-3.567442445,3.396744076,-6.597223234));
#108052=CARTESIAN_POINT('Origin',(0.099567748023463,3.48208258641656,0.167703371500352));
#108053=CARTESIAN_POINT('Ctrl Pts',(-1.758168589,3.396737969,-7.033586796));
#108054=CARTESIAN_POINT('Ctrl Pts',(-1.876402807,3.376870318,-7.004032076));
#108055=CARTESIAN_POINT('Ctrl Pts',(-1.993576877,3.357142857,-6.970520155));
#108056=CARTESIAN_POINT('Ctrl Pts',(-2.258376345,3.312561141,-6.894787199));
#108057=CARTESIAN_POINT('Ctrl Pts',(-2.516666969,3.267335925,-6.799182846));
#108058=CARTESIAN_POINT('Ctrl Pts',(-1.579193193,3.396737969,-7.331858486));
#108059=CARTESIAN_POINT('Ctrl Pts',(-1.702441341,3.376870318,-7.305312333));
#108060=CARTESIAN_POINT('Ctrl Pts',(-1.824727629,3.357142857,-7.274638759));
#108061=CARTESIAN_POINT('Ctrl Pts',(-2.1010801,3.312561141,-7.20532013));
#108062=CARTESIAN_POINT('Ctrl Pts',(-2.37137707,3.267335925,-7.115235119));
#108063=CARTESIAN_POINT('',(-1.76276545951291,3.39596551375301,-7.0324361311284));
#108064=CARTESIAN_POINT('Ctrl Pts',(-1.76276546417588,3.39596551234759,
-7.03243612999851));
#108065=CARTESIAN_POINT('Ctrl Pts',(-1.84016527804476,3.38295904390363,
-7.01303492728227));
#108066=CARTESIAN_POINT('Ctrl Pts',(-1.91712191713628,3.37001483660174,
-6.99238636288139));
#108067=CARTESIAN_POINT('Ctrl Pts',(-1.99357687556294,3.35714285721626,
-6.97052015564213));
#108068=CARTESIAN_POINT('Ctrl Pts',(-2.13557595262986,3.33323585096109,
-6.92990825481634));
#108069=CARTESIAN_POINT('Ctrl Pts',(-2.27682293005017,3.30907945238249,
-6.88481313408911));
#108070=CARTESIAN_POINT('Ctrl Pts',(-2.41689914240186,3.28473845141959,
-6.83528335471055));
#108071=CARTESIAN_POINT('Ctrl Pts',(-2.45022320893918,3.27894773847801,
-6.82350024296103));
#108072=CARTESIAN_POINT('Ctrl Pts',(-2.48348102141939,3.27314659526071,
-6.81146637762032));
#108073=CARTESIAN_POINT('Ctrl Pts',(-2.516666969,3.267335925,-6.799182846));
#108074=CARTESIAN_POINT('Ctrl Pts',(-1.82568833719241,3.35698786877967,
-7.27439771327727));
#108075=CARTESIAN_POINT('Ctrl Pts',(-1.81553619967536,3.36293887933007,
-7.23548805576183));
#108076=CARTESIAN_POINT('Ctrl Pts',(-1.80500598344178,3.36926346353021,
-7.19507767308363));
#108077=CARTESIAN_POINT('Ctrl Pts',(-1.78366980731412,3.38247021627563,
-7.11303601874255));
#108078=CARTESIAN_POINT('Ctrl Pts',(-1.77320129741808,3.38913021757011,
-7.07271166924245));
#108079=CARTESIAN_POINT('Ctrl Pts',(-1.76276545739149,3.39596551349533,
-7.03243613163435));
#108080=CARTESIAN_POINT('Ctrl Pts',(-0.996205363999999,3.267335925,-7.181230735));
#108081=CARTESIAN_POINT('Ctrl Pts',(-1.385832842,3.331598135,-7.127180253));
#108082=CARTESIAN_POINT('Ctrl Pts',(-1.767325168,3.396744076,-7.031291613));
#108083=CARTESIAN_POINT('Ctrl Pts',(-1.273635477,3.267335925,-7.391065733));
#108084=CARTESIAN_POINT('Ctrl Pts',(-1.674647839,3.331598135,-7.321962901));
#108085=CARTESIAN_POINT('Ctrl Pts',(-2.065829641,3.396744076,-7.209878494));
#108086=CARTESIAN_POINT('Origin',(0.0611886336607825,3.48208255128803,0.185186683605522));
#108087=CARTESIAN_POINT('Ctrl Pts',(-0.205050335,3.396737969,-7.247099721));
#108088=CARTESIAN_POINT('Ctrl Pts',(-0.326873693,3.376870318,-7.243652835));
#108089=CARTESIAN_POINT('Ctrl Pts',(-0.448512371,3.357142857,-7.236113367));
#108090=CARTESIAN_POINT('Ctrl Pts',(-0.723401321,3.312561141,-7.21907506300001));
#108091=CARTESIAN_POINT('Ctrl Pts',(-0.996205364,3.267335925,-7.181230735));
#108092=CARTESIAN_POINT('Ctrl Pts',(0.033860313,3.396737969,-7.499923565));
#108093=CARTESIAN_POINT('Ctrl Pts',(-0.092213001,3.376870318,-7.500492755));
#108094=CARTESIAN_POINT('Ctrl Pts',(-0.218234215,3.357142857,-7.496824249));
#108095=CARTESIAN_POINT('Ctrl Pts',(-0.503027175,3.312561141,-7.488533863));
#108096=CARTESIAN_POINT('Ctrl Pts',(-0.786370366,3.267335925,-7.458660848));
#108097=CARTESIAN_POINT('',(-0.209787091585121,3.39596551378162,-7.24696414902478));
#108098=CARTESIAN_POINT('Ctrl Pts',(-0.209787096109259,3.39596551248188,
-7.24696414920313));
#108099=CARTESIAN_POINT('Ctrl Pts',(-0.28954803098352,3.38295904384088,
-7.24465520746408));
#108100=CARTESIAN_POINT('Ctrl Pts',(-0.369144297527101,3.37001483649756,
-7.24103279796689));
#108101=CARTESIAN_POINT('Ctrl Pts',(-0.448512369281491,3.35714285725138,
-7.23611336728682));
#108102=CARTESIAN_POINT('Ctrl Pts',(-0.595921292197588,3.33323595691704,
-7.22697659379603));
#108103=CARTESIAN_POINT('Ctrl Pts',(-0.743559459221487,3.30907966593021,
-7.21329977761382));
#108104=CARTESIAN_POINT('Ctrl Pts',(-0.891007556090164,3.2847387741694,
-7.19504034292312));
#108105=CARTESIAN_POINT('Ctrl Pts',(-0.926086197406635,3.27894795401279,
-7.19069633188629));
#108106=CARTESIAN_POINT('Ctrl Pts',(-0.961154037905286,3.27314670319171,
-7.18609317742572));
#108107=CARTESIAN_POINT('Ctrl Pts',(-0.996205363815112,3.267335925,-7.18123073524444));
#108108=CARTESIAN_POINT('Ctrl Pts',(-0.219224279818265,3.35698786879476,
-7.49679536283724));
#108109=CARTESIAN_POINT('Ctrl Pts',(-0.217673919736165,3.36293888004325,
-7.45661297729563));
#108110=CARTESIAN_POINT('Ctrl Pts',(-0.216076931763992,3.36926346459429,
-7.41488367955715));
#108111=CARTESIAN_POINT('Ctrl Pts',(-0.212876114293901,3.38247021622806,
-7.33017347319156));
#108112=CARTESIAN_POINT('Ctrl Pts',(-0.211320895472024,3.38913021760024,
-7.28854146381554));
#108113=CARTESIAN_POINT('Ctrl Pts',(-0.209787090011592,3.39596551352973,
-7.24696414904142));
#108114=CARTESIAN_POINT('Ctrl Pts',(0.570837696,3.267335925,-7.227492257));
#108115=CARTESIAN_POINT('Ctrl Pts',(0.178700236,3.331598135,-7.258463836));
#108116=CARTESIAN_POINT('Ctrl Pts',(-0.214486235,3.396744076,-7.246826592));
#108117=CARTESIAN_POINT('Ctrl Pts',(0.345002067,3.267335925,-7.492060703));
#108118=CARTESIAN_POINT('Ctrl Pts',(-0.061489915,3.331598135,-7.510779261));
#108119=CARTESIAN_POINT('Ctrl Pts',(-0.467620938,3.396744076,-7.485407848));
#108120=CARTESIAN_POINT('Origin',(0.0199484237424318,3.48208257448395,0.19401088831975));
#108121=CARTESIAN_POINT('Ctrl Pts',(1.357655845,3.396737969,-7.121746317));
#108122=CARTESIAN_POINT('Ctrl Pts',(1.237939671,3.376870318,-7.14456843900001));
#108123=CARTESIAN_POINT('Ctrl Pts',(1.117524075,3.357142857,-7.163353959));
#108124=CARTESIAN_POINT('Ctrl Pts',(0.845399144,3.312561141,-7.205807));
#108125=CARTESIAN_POINT('Ctrl Pts',(0.570837696,3.267335925,-7.227492257));
#108126=CARTESIAN_POINT('Ctrl Pts',(1.645330548,3.396737969,-7.317300553));
#108127=CARTESIAN_POINT('Ctrl Pts',(1.522327117,3.376870318,-7.344958472));
#108128=CARTESIAN_POINT('Ctrl Pts',(1.398463589,3.357142857,-7.36846657));
#108129=CARTESIAN_POINT('Ctrl Pts',(1.118546742,3.312561141,-7.421592076));
#108130=CARTESIAN_POINT('Ctrl Pts',(0.835406142,3.267335925,-7.45332788600001));
#108131=CARTESIAN_POINT('',(1.35300068757869,3.39596551374153,-7.12263217768761));
#108132=CARTESIAN_POINT('Ctrl Pts',(1.35300068233051,3.39596551240205,-7.12263217854008));
#108133=CARTESIAN_POINT('Ctrl Pts',(1.2746081595671,3.38295904372139,-7.13752346249768));
#108134=CARTESIAN_POINT('Ctrl Pts',(1.19609409861221,3.37001483640097,-7.15109658726971));
#108135=CARTESIAN_POINT('Ctrl Pts',(1.11752407593566,3.35714285712236,-7.1633539590213));
#108136=CARTESIAN_POINT('Ctrl Pts',(0.97159705154719,3.33323590700525,-7.18611940684339));
#108137=CARTESIAN_POINT('Ctrl Pts',(0.824470163904568,3.30907956542225,
-7.20450021779076));
#108138=CARTESIAN_POINT('Ctrl Pts',(0.676543772340042,3.28473862232611,
-7.21836467120363));
#108139=CARTESIAN_POINT('Ctrl Pts',(0.641351723076271,3.27894785260945,
-7.22166305847827));
#108140=CARTESIAN_POINT('Ctrl Pts',(0.60611451475454,3.27314665241224,-7.22470604357414));
#108141=CARTESIAN_POINT('Ctrl Pts',(0.570837696373458,3.267335925,-7.22749225731879));
#108142=CARTESIAN_POINT('Ctrl Pts',(1.39749046141673,3.35698786879297,-7.36865119366902));
#108143=CARTESIAN_POINT('Ctrl Pts',(1.39036656336943,3.36293886876702,-7.32907504330461));
#108144=CARTESIAN_POINT('Ctrl Pts',(1.38295561590671,3.36926348197299,-7.28797786324346));
#108145=CARTESIAN_POINT('Ctrl Pts',(1.3678713393157,3.38247029533229,-7.20455966330532));
#108146=CARTESIAN_POINT('Ctrl Pts',(1.36044059487445,3.38913025632477,-7.16356692879642));
#108147=CARTESIAN_POINT('Ctrl Pts',(1.35300068947362,3.39596551352698,-7.12263217749919));
#108148=CARTESIAN_POINT('Ctrl Pts',(2.11118902,3.267335925,-6.935804274));
#108149=CARTESIAN_POINT('Ctrl Pts',(1.73487749,3.331598135,-7.050349716));
#108150=CARTESIAN_POINT('Ctrl Pts',(1.348381837,3.396744076,-7.123508014));
#108151=CARTESIAN_POINT('Ctrl Pts',(1.947507698,3.267335925,-7.242735241));
#108152=CARTESIAN_POINT('Ctrl Pts',(1.554543209,3.331598135,-7.34839993));
#108153=CARTESIAN_POINT('Ctrl Pts',(1.1524532,3.396744076,-7.410927852));
#108154=CARTESIAN_POINT('Origin',(-0.0222246156226963,3.48208256333927,
0.193763563776748));
#108155=CARTESIAN_POINT('Ctrl Pts',(2.856879547,3.396737969,-6.663387971));
#108156=CARTESIAN_POINT('Ctrl Pts',(2.744868352,3.376870318,-6.711411963));
#108157=CARTESIAN_POINT('Ctrl Pts',(2.631306337,3.357142857,-6.755644082));
#108158=CARTESIAN_POINT('Ctrl Pts',(2.374669684,3.312561141,-6.855603411));
#108159=CARTESIAN_POINT('Ctrl Pts',(2.11118902,3.267335925,-6.93580427400001));
#108160=CARTESIAN_POINT('Ctrl Pts',(3.179866955,3.396737969,-6.792528701));
#108161=CARTESIAN_POINT('Ctrl Pts',(3.065684911,3.376870318,-6.845982094));
#108162=CARTESIAN_POINT('Ctrl Pts',(2.94977079,3.357142857,-6.895567583));
#108163=CARTESIAN_POINT('Ctrl Pts',(2.687818656,3.312561141,-7.007624892));
#108164=CARTESIAN_POINT('Ctrl Pts',(2.418119987,3.267335925,-7.099485596));
#108165=CARTESIAN_POINT('',(2.85252365818121,3.39596551374359,-6.66525384216208));
#108166=CARTESIAN_POINT('Ctrl Pts',(2.852523653046,3.39596551231933,-6.66525384416588));
#108167=CARTESIAN_POINT('Ctrl Pts',(2.77916509043875,3.38295904377301,-6.69664905294925));
#108168=CARTESIAN_POINT('Ctrl Pts',(2.70540446510206,3.37001483648196,-6.72678304782433));
#108169=CARTESIAN_POINT('Ctrl Pts',(2.63130633853808,3.35714285723369,-6.75564408156074));
#108170=CARTESIAN_POINT('Ctrl Pts',(2.49368487690778,3.33323590224748,-6.80924729363336));
#108171=CARTESIAN_POINT('Ctrl Pts',(2.3539490363617,3.30907955566733,-6.85882631280321));
#108172=CARTESIAN_POINT('Ctrl Pts',(2.21246149976698,3.28473860750851,-6.90416643206194));
#108173=CARTESIAN_POINT('Ctrl Pts',(2.17880130540959,3.27894784271333,-6.91495294558227));
#108174=CARTESIAN_POINT('Ctrl Pts',(2.14504210403852,3.27314664745598,-6.92549973634016));
#108175=CARTESIAN_POINT('Ctrl Pts',(2.1111890205697,3.267335925,-6.93580427430381));
#108176=CARTESIAN_POINT('Ctrl Pts',(2.94886010157405,3.35698786876897,-6.89595708377018));
#108177=CARTESIAN_POINT('Ctrl Pts',(2.93339505702865,3.36293886751201,-6.85883763699597));
#108178=CARTESIAN_POINT('Ctrl Pts',(2.91732268763635,3.36926348341502,-6.82029440453799));
#108179=CARTESIAN_POINT('Ctrl Pts',(2.88465882512692,3.38247021619802,-6.74206962658919));
#108180=CARTESIAN_POINT('Ctrl Pts',(2.86858947662251,3.38913021753449,-6.70363241886973));
#108181=CARTESIAN_POINT('Ctrl Pts',(2.85252365959883,3.39596551344807,-6.66525384151601));
#108182=CARTESIAN_POINT('Ctrl Pts',(3.552823492,3.267335925,-6.319805791));
#108183=CARTESIAN_POINT('Ctrl Pts',(3.2099338,3.331598135,-6.51256908));
#108184=CARTESIAN_POINT('Ctrl Pts',(2.848201072,3.396744076,-6.667102118));
#108185=CARTESIAN_POINT('Ctrl Pts',(3.458950033,3.267335925,-6.65474752900001));
#108186=CARTESIAN_POINT('Ctrl Pts',(3.09788762,3.331598135,-6.842417585));
#108187=CARTESIAN_POINT('Ctrl Pts',(2.718639907,3.396744076,-6.989921105));
#108188=CARTESIAN_POINT('Origin',(-0.0633584572675827,3.48208260128073,
0.18445584139668));
#108189=CARTESIAN_POINT('Ctrl Pts',(4.222518736,3.396737969,-5.89345701));
#108190=CARTESIAN_POINT('Ctrl Pts',(4.123450039,3.376870318,-5.964437323));
#108191=CARTESIAN_POINT('Ctrl Pts',(4.022051639,3.357142857,-6.032047796));
#108192=CARTESIAN_POINT('Ctrl Pts',(3.79290331,3.312561141,-6.184839426));
#108193=CARTESIAN_POINT('Ctrl Pts',(3.552823492,3.267335925,-6.319805791));
#108194=CARTESIAN_POINT('Ctrl Pts',(4.565716317,3.396737969,-5.950145755));
#108195=CARTESIAN_POINT('Ctrl Pts',(4.465694686,3.376870318,-6.026895202));
#108196=CARTESIAN_POINT('Ctrl Pts',(4.363149987,3.357142857,-6.100239519));
#108197=CARTESIAN_POINT('Ctrl Pts',(4.131411158,3.312561141,-6.265988957));
#108198=CARTESIAN_POINT('Ctrl Pts',(3.88776523,3.267335925,-6.41367925));
#108199=CARTESIAN_POINT('',(4.21866579244059,3.39596551376989,-5.89621564499187));
#108200=CARTESIAN_POINT('Ctrl Pts',(4.21866578869482,3.39596551246601,-5.89621564797497));
#108201=CARTESIAN_POINT('Ctrl Pts',(4.15377134973309,3.38295904378691,-5.94264677680636));
#108202=CARTESIAN_POINT('Ctrl Pts',(4.08821312497822,3.37001483644987,-5.98793260973008));
#108203=CARTESIAN_POINT('Ctrl Pts',(4.02205164047476,3.35714285719441,-6.03204779542876));
#108204=CARTESIAN_POINT('Ctrl Pts',(3.8991708216098,3.33323590672447,-6.11398232501675));
#108205=CARTESIAN_POINT('Ctrl Pts',(3.77335997481717,3.30907956474255,-6.19244127511079));
#108206=CARTESIAN_POINT('Ctrl Pts',(3.644927148364,3.28473862118571,-6.26713699279031));
#108207=CARTESIAN_POINT('Ctrl Pts',(3.61437266836811,3.27894785185105,-6.28490728465918));
#108208=CARTESIAN_POINT('Ctrl Pts',(3.58366996254106,3.27314665203412,-6.30246474160323));
#108209=CARTESIAN_POINT('Ctrl Pts',(3.55282349211638,3.267335925,-6.31980579103262));
#108210=CARTESIAN_POINT('Ctrl Pts',(4.36234432158474,3.35698786875377,-6.10081568471984));
#108211=CARTESIAN_POINT('Ctrl Pts',(4.33926125519902,3.36293886804972,-6.06788859433876));
#108212=CARTESIAN_POINT('Ctrl Pts',(4.31527899933772,3.36926348229613,-6.03370157477921));
#108213=CARTESIAN_POINT('Ctrl Pts',(4.2665627804133,3.38247021623225,-5.96432740782836));
#108214=CARTESIAN_POINT('Ctrl Pts',(4.24260626070832,3.38913021759041,-5.93024327565408));
#108215=CARTESIAN_POINT('Ctrl Pts',(4.21866579364629,3.3959655135348,-5.89621564409636));
#108216=CARTESIAN_POINT('Ctrl Pts',(4.828331886,3.267335925,-5.408300213));
#108217=CARTESIAN_POINT('Ctrl Pts',(4.534897174,3.331598135,-5.670267952));
#108218=CARTESIAN_POINT('Ctrl Pts',(4.214841591,3.396744076,-5.89894993700001));
#108219=CARTESIAN_POINT('Ctrl Pts',(4.808655709,3.267335925,-5.755591218));
#108220=CARTESIAN_POINT('Ctrl Pts',(4.49637825,3.331598135,-6.016491399));
#108221=CARTESIAN_POINT('Ctrl Pts',(4.157706034,3.396744076,-6.242073416));
#108222=CARTESIAN_POINT('Origin',(-0.101529668806381,3.48208256172017,0.166523092993265));
#108223=CARTESIAN_POINT('Ctrl Pts',(5.39071764200001,3.396737969,-4.847954548));
#108224=CARTESIAN_POINT('Ctrl Pts',(5.309223786,3.376870318,-4.93857222300001));
#108225=CARTESIAN_POINT('Ctrl Pts',(5.224730277,3.357142857,-5.026399659));
#108226=CARTESIAN_POINT('Ctrl Pts',(5.033784992,3.312561141,-5.224879222));
#108227=CARTESIAN_POINT('Ctrl Pts',(4.828331886,3.267335925,-5.40830021300001));
#108228=CARTESIAN_POINT('Ctrl Pts',(5.73807786,3.396737969,-4.829540607));
#108229=CARTESIAN_POINT('Ctrl Pts',(5.656893541,3.376870318,-4.92599738900001));
#108230=CARTESIAN_POINT('Ctrl Pts',(5.57251314,3.357142857,-5.019671036));
#108231=CARTESIAN_POINT('Ctrl Pts',(5.38182346500001,3.312561141,-5.231362342));
#108232=CARTESIAN_POINT('Ctrl Pts',(5.17562289100001,3.267335925,-5.42797639));
#108233=CARTESIAN_POINT('',(5.38754780316155,3.39596551374977,-4.85147695721432));
#108234=CARTESIAN_POINT('Ctrl Pts',(5.38754779964328,3.39596551235192,-4.85147696088385));
#108235=CARTESIAN_POINT('Ctrl Pts',(5.33415187731936,3.38295904377502,-4.91077294193955));
#108236=CARTESIAN_POINT('Ctrl Pts',(5.27986148300074,3.37001483647243,-4.9690930976777));
#108237=CARTESIAN_POINT('Ctrl Pts',(5.22473027794813,3.35714285719587,-5.02639965812588));
#108238=CARTESIAN_POINT('Ctrl Pts',(5.12233584940433,3.33323590746412,-5.13283434396295));
#108239=CARTESIAN_POINT('Ctrl Pts',(5.01633274907877,3.30907956627202,-5.23650457710434));
#108240=CARTESIAN_POINT('Ctrl Pts',(4.90695998635107,3.28473862356702,-5.33706320852209));
#108241=CARTESIAN_POINT('Ctrl Pts',(4.88093993712966,3.27894785343848,-5.36098635422923));
#108242=CARTESIAN_POINT('Ctrl Pts',(4.85472937426329,3.27314665282757,-5.38473350510159));
#108243=CARTESIAN_POINT('Ctrl Pts',(4.82833188668483,3.267335925,-5.4083002130388));
#108244=CARTESIAN_POINT('Ctrl Pts',(5.57185016888731,3.35698786876255,-5.02040692549819));
#108245=CARTESIAN_POINT('Ctrl Pts',(5.54222842210733,3.36293886778275,-4.99321183034349));
#108246=CARTESIAN_POINT('Ctrl Pts',(5.51145765308973,3.36926348336969,-4.96497955430138));
#108247=CARTESIAN_POINT('Ctrl Pts',(5.4489666271509,3.38247029552344,-4.90769952435259));
#108248=CARTESIAN_POINT('Ctrl Pts',(5.41824331752566,3.38913025642266,-4.87956238800544));
#108249=CARTESIAN_POINT('Ctrl Pts',(5.38754780472075,3.39596551353952,-4.85147695545905));
#108250=CARTESIAN_POINT('Ctrl Pts',(5.878072847,3.267335925,-4.243908529));
#108251=CARTESIAN_POINT('Ctrl Pts',(5.647813796,3.331598135,-4.562831397));
#108252=CARTESIAN_POINT('Ctrl Pts',(5.384400802,3.396744076,-4.854969413));
#108253=CARTESIAN_POINT('Ctrl Pts',(5.933513989,3.267335925,-4.587309859));
#108254=CARTESIAN_POINT('Ctrl Pts',(5.684623229,3.331598135,-4.909240762));
#108255=CARTESIAN_POINT('Ctrl Pts',(5.402362448,3.396744076,-5.202353312));
#108256=CARTESIAN_POINT('Origin',(-0.134953372141405,3.48208259745366,0.140803901079568));
#108257=CARTESIAN_POINT('Ctrl Pts',(6.306852583,3.396737969,-3.575767121));
#108258=CARTESIAN_POINT('Ctrl Pts',(6.246744129,3.376870318,-3.681784975));
#108259=CARTESIAN_POINT('Ctrl Pts',(6.183106334,3.357142857,-3.785722661));
#108260=CARTESIAN_POINT('Ctrl Pts',(6.039292483,3.312561141,-4.020609474));
#108261=CARTESIAN_POINT('Ctrl Pts',(5.878072847,3.267335925,-4.243908529));
#108262=CARTESIAN_POINT('Ctrl Pts',(6.642133258,3.396737969,-3.483111508));
#108263=CARTESIAN_POINT('Ctrl Pts',(6.58358234,3.376870318,-3.594765413));
#108264=CARTESIAN_POINT('Ctrl Pts',(6.521311771,3.357142857,-3.704388314));
#108265=CARTESIAN_POINT('Ctrl Pts',(6.380587689,3.312561141,-3.952123038));
#108266=CARTESIAN_POINT('Ctrl Pts',(6.221474178,3.267335925,-4.188467387));
#108267=CARTESIAN_POINT('',(6.30451406690207,3.3959655137755,-3.5798885989803));
#108268=CARTESIAN_POINT('Ctrl Pts',(6.30451406510151,3.39596551257587,-3.57988860303183));
#108269=CARTESIAN_POINT('Ctrl Pts',(6.2651133921919,3.38295904390818,-3.64927682231007));
#108270=CARTESIAN_POINT('Ctrl Pts',(6.22462938630305,3.37001483653199,-3.71790431544402));
#108271=CARTESIAN_POINT('Ctrl Pts',(6.18310633484167,3.35714285725499,-3.78572265965193));
#108272=CARTESIAN_POINT('Ctrl Pts',(6.10598607637181,3.33323588697773,-3.91168084524802));
#108273=CARTESIAN_POINT('Ctrl Pts',(6.02474723190066,3.30907952487959,-4.03571496374845));
#108274=CARTESIAN_POINT('Ctrl Pts',(5.93954859646137,3.2847385609158,-4.15743460203448));
#108275=CARTESIAN_POINT('Ctrl Pts',(5.91927972212827,3.27894781160174,-4.18639187393878));
#108276=CARTESIAN_POINT('Ctrl Pts',(5.89878695617026,3.27314663187857,-4.21521822142582));
#108277=CARTESIAN_POINT('Ctrl Pts',(5.87807284737279,3.267335925,-4.24390852893982));
#108278=CARTESIAN_POINT('Ctrl Pts',(6.52082249472828,3.35698786878879,-3.70524951776723));
#108279=CARTESIAN_POINT('Ctrl Pts',(6.48604707793,3.36293887951342,-3.6850579891456));
#108280=CARTESIAN_POINT('Ctrl Pts',(6.44992678160999,3.36926346437347,-3.66410067488437));
#108281=CARTESIAN_POINT('Ctrl Pts',(6.3765835824589,3.38247021627534,-3.62159373779551));
#108282=CARTESIAN_POINT('Ctrl Pts',(6.34052967847699,3.38913021762558,-3.60071889880902));
#108283=CARTESIAN_POINT('Ctrl Pts',(6.30451406744253,3.39596551355646,-3.57988859797397));
#108284=CARTESIAN_POINT('Ctrl Pts',(6.652961655,3.267335925,-2.881076398));
#108285=CARTESIAN_POINT('Ctrl Pts',(6.496644922,3.331598135,-3.242041916));
#108286=CARTESIAN_POINT('Ctrl Pts',(6.302191415,3.396744076,-3.583975916));
#108287=CARTESIAN_POINT('Ctrl Pts',(6.780927749,3.267335925,-3.20453099));
#108288=CARTESIAN_POINT('Ctrl Pts',(6.607061545,3.331598135,-3.572439483));
#108289=CARTESIAN_POINT('Ctrl Pts',(6.394410397,3.396744076,-3.919376949));
#108290=CARTESIAN_POINT('Origin',(-0.162067079264793,3.48208259603613,0.108501079889591));
#108291=CARTESIAN_POINT('Ctrl Pts',(6.928086106,3.396737969,-2.136380796));
#108292=CARTESIAN_POINT('Ctrl Pts',(6.892173659,3.376870318,-2.252841553));
#108293=CARTESIAN_POINT('Ctrl Pts',(6.852367211,3.357142857,-2.368029478));
#108294=CARTESIAN_POINT('Ctrl Pts',(6.76240936900001,3.312561141,-2.628340495));
#108295=CARTESIAN_POINT('Ctrl Pts',(6.652961655,3.267335925,-2.881076398));
#108296=CARTESIAN_POINT('Ctrl Pts',(7.235609888,3.396737969,-1.973815986));
#108297=CARTESIAN_POINT('Ctrl Pts',(7.202430147,3.376870318,-2.095446201));
#108298=CARTESIAN_POINT('Ctrl Pts',(7.165181113,3.357142857,-2.215892511));
#108299=CARTESIAN_POINT('Ctrl Pts',(7.081002724,3.312561141,-2.488086853));
#108300=CARTESIAN_POINT('Ctrl Pts',(6.976416247,3.267335925,-2.753110305));
#108301=CARTESIAN_POINT('',(6.92668825921923,3.39596551374539,-2.14090862877695));
#108302=CARTESIAN_POINT('Ctrl Pts',(6.92668825783294,3.39596551239671,-2.14090863337104));
#108303=CARTESIAN_POINT('Ctrl Pts',(6.90312516711708,3.38295904390286,-2.21714457406198));
#108304=CARTESIAN_POINT('Ctrl Pts',(6.87834053751168,3.37001483658745,-2.29287045883608));
#108305=CARTESIAN_POINT('Ctrl Pts',(6.85236721145235,3.35714285722418,-2.36802947669104));
#108306=CARTESIAN_POINT('Ctrl Pts',(6.80412723414096,3.33323587011083,-2.50762150427388));
#108307=CARTESIAN_POINT('Ctrl Pts',(6.75145133814406,3.30907949095744,-2.64621982014326));
#108308=CARTESIAN_POINT('Ctrl Pts',(6.69441067811292,3.28473850983767,-2.78340900225841));
#108309=CARTESIAN_POINT('Ctrl Pts',(6.68084067475151,3.27894777748228,-2.81604638165472));
#108310=CARTESIAN_POINT('Ctrl Pts',(6.66702387080435,3.2731466147879,-2.84860402807476));
#108311=CARTESIAN_POINT('Ctrl Pts',(6.65296165575154,3.267335925,-2.88107639770267));
#108312=CARTESIAN_POINT('Ctrl Pts',(7.16488840890112,3.35698786873672,-2.21683876059868));
#108313=CARTESIAN_POINT('Ctrl Pts',(7.12658551330807,3.36293886811032,-2.20459500866856));
#108314=CARTESIAN_POINT('Ctrl Pts',(7.08680430148347,3.36926348261331,-2.19189240174846));
#108315=CARTESIAN_POINT('Ctrl Pts',(7.0060376629728,3.38247030444418,-2.16614573658246));
#108316=CARTESIAN_POINT('Ctrl Pts',(6.96633949484734,3.38913026076675,-2.15350955557203));
#108317=CARTESIAN_POINT('Ctrl Pts',(6.92668826046996,3.39596551347636,-2.1409086266833));
#108318=CARTESIAN_POINT('Ctrl Pts',(7.116765371,3.267335925,-1.383528337));
#108319=CARTESIAN_POINT('Ctrl Pts',(7.041700152,3.331598135,-1.769658159));
#108320=CARTESIAN_POINT('Ctrl Pts',(6.925298563,3.396744076,-2.145399688));
#108321=CARTESIAN_POINT('Ctrl Pts',(7.311272864,3.267335925,-1.671911813));
#108322=CARTESIAN_POINT('Ctrl Pts',(7.220561006,3.331598135,-2.068594904));
#108323=CARTESIAN_POINT('Ctrl Pts',(7.087462824,3.396744076,-2.453134876));
#108324=CARTESIAN_POINT('Origin',(-0.181602625130144,3.48208254599677,0.0711247740124582));
#108325=CARTESIAN_POINT('Ctrl Pts',(7.225370023,3.396737969,-0.597099681));
#108326=CARTESIAN_POINT('Ctrl Pts',(7.21533281000001,3.376870318,-0.718557763));
#108327=CARTESIAN_POINT('Ctrl Pts',(7.201219013,3.357142857,-0.839609869));
#108328=CARTESIAN_POINT('Ctrl Pts',(7.16932351,3.312561141,-1.113173236));
#108329=CARTESIAN_POINT('Ctrl Pts',(7.116765371,3.267335925,-1.383528337));
#108330=CARTESIAN_POINT('Ctrl Pts',(7.490757441,3.396737969,-0.372227023));
#108331=CARTESIAN_POINT('Ctrl Pts',(7.484500325,3.376870318,-0.498146254));
#108332=CARTESIAN_POINT('Ctrl Pts',(7.474014549,3.357142857,-0.623784038));
#108333=CARTESIAN_POINT('Ctrl Pts',(7.45031794100001,3.312561141,-0.907710493));
#108334=CARTESIAN_POINT('Ctrl Pts',(7.405148846,3.267335925,-1.189020844));
#108335=CARTESIAN_POINT('',(7.22497820777076,3.39596551374994,-0.601822150741499));
#108336=CARTESIAN_POINT('Ctrl Pts',(7.2249782070017,3.39596551246352,-0.601822155609413));
#108337=CARTESIAN_POINT('Ctrl Pts',(7.21835448240688,3.38295904386693,-0.681341109866494));
#108338=CARTESIAN_POINT('Ctrl Pts',(7.21042813046328,3.37001483652023,-0.760624528247004));
#108339=CARTESIAN_POINT('Ctrl Pts',(7.20121901317613,3.35714285724619,-0.839609867489352));
#108340=CARTESIAN_POINT('Ctrl Pts',(7.18411505685797,3.33323592201497,-0.986308161852371));
#108341=CARTESIAN_POINT('Ctrl Pts',(7.16246529151479,3.30907959556797,-1.13298957017443));
#108342=CARTESIAN_POINT('Ctrl Pts',(7.13624990595926,3.2847386677418,-1.27923308736274));
#108343=CARTESIAN_POINT('Ctrl Pts',(7.13001318165582,3.27894788294406,-1.31402488914406));
#108344=CARTESIAN_POINT('Ctrl Pts',(7.12351828192882,3.2731466676059,-1.3487918764834));
#108345=CARTESIAN_POINT('Ctrl Pts',(7.11676537203918,3.267335925,-1.38352833629909));
#108346=CARTESIAN_POINT('Ctrl Pts',(7.47393210366752,3.35698786876155,-0.624771087536086));
#108347=CARTESIAN_POINT('Ctrl Pts',(7.43389266565902,3.36293886785064,-0.621047578195738));
#108348=CARTESIAN_POINT('Ctrl Pts',(7.39231082795146,3.36926348285857,-0.617193735242564));
#108349=CARTESIAN_POINT('Ctrl Pts',(7.30789826191457,3.38247021624306,-0.609411504751938));
#108350=CARTESIAN_POINT('Ctrl Pts',(7.26641150751208,3.389130217592,-0.605604655336773));
#108351=CARTESIAN_POINT('Ctrl Pts',(7.22497820790518,3.39596551351833,-0.601822148850575));
#108352=CARTESIAN_POINT('Ctrl Pts',(7.247797047,3.267335925,0.178711971));
#108353=CARTESIAN_POINT('Ctrl Pts',(7.257493309,3.331598135,-0.214527153));
#108354=CARTESIAN_POINT('Ctrl Pts',(7.224586446,3.396744076,-0.606506955));
#108355=CARTESIAN_POINT('Ctrl Pts',(7.499750986,3.267335925,-0.061115898));
#108356=CARTESIAN_POINT('Ctrl Pts',(7.496435059,3.331598135,-0.468025127));
#108357=CARTESIAN_POINT('Ctrl Pts',(7.449113366,3.396744076,-0.872186943));
#108358=CARTESIAN_POINT('Origin',(-0.192646482398922,3.4820825457969,0.0304227050463073));
#108359=CARTESIAN_POINT('Ctrl Pts',(7.184803668,3.396737969,0.970101153));
#108360=CARTESIAN_POINT('Ctrl Pts',(7.201111017,3.376870318,0.849324988));
#108361=CARTESIAN_POINT('Ctrl Pts',(7.213349817,3.357142857,0.728068964));
#108362=CARTESIAN_POINT('Ctrl Pts',(7.241008051,3.312561141,0.454044767));
#108363=CARTESIAN_POINT('Ctrl Pts',(7.247797047,3.267335925,0.178711971));
#108364=CARTESIAN_POINT('Ctrl Pts',(7.395645502,3.396737969,1.246766863));
#108365=CARTESIAN_POINT('Ctrl Pts',(7.416603586,3.376870318,1.122446458));
#108366=CARTESIAN_POINT('Ctrl Pts',(7.433371371,3.357142857,0.997491884));
#108367=CARTESIAN_POINT('Ctrl Pts',(7.471264572,3.312561141,0.715109402));
#108368=CARTESIAN_POINT('Ctrl Pts',(7.487624915,3.267335925,0.43066591));
#108369=CARTESIAN_POINT('',(7.18543620481062,3.39596551373394,0.965404863303355));
#108370=CARTESIAN_POINT('Ctrl Pts',(7.18543620520418,3.39596551236943,0.965404858045346));
#108371=CARTESIAN_POINT('Ctrl Pts',(7.19606156435663,3.3829590437794,0.886321106970015));
#108372=CARTESIAN_POINT('Ctrl Pts',(7.20536411729142,3.37001483646942,0.807187359173183));
#108373=CARTESIAN_POINT('Ctrl Pts',(7.21334981711854,3.35714285715552,0.728068965219242));
#108374=CARTESIAN_POINT('Ctrl Pts',(7.22818155036869,3.33323590368426,0.58112343890167));
#108375=CARTESIAN_POINT('Ctrl Pts',(7.2385701157649,3.30907955877851,0.43321718806126));
#108376=CARTESIAN_POINT('Ctrl Pts',(7.24440566172763,3.28473861229339,0.284757116497334));
#108377=CARTESIAN_POINT('Ctrl Pts',(7.24579395134919,3.27894784591094,0.249438128713763));
#108378=CARTESIAN_POINT('Ctrl Pts',(7.24692476879664,3.27314664905907,0.214087875340147));
#108379=CARTESIAN_POINT('Ctrl Pts',(7.24779704733703,3.267335925,0.178711971354076));
#108380=CARTESIAN_POINT('Ctrl Pts',(7.43350303989333,3.35698786876789,0.996510188147964));
#108381=CARTESIAN_POINT('Ctrl Pts',(7.39359918051022,3.36293887930503,0.991539338669348));
#108382=CARTESIAN_POINT('Ctrl Pts',(7.35216123765737,3.36926346403428,0.98636423935489));
#108383=CARTESIAN_POINT('Ctrl Pts',(7.26804866643108,3.38247028762204,0.975818247058842));
#108384=CARTESIAN_POINT('Ctrl Pts',(7.22671373276374,3.38913025251371,0.970617699024864));
#108385=CARTESIAN_POINT('Ctrl Pts',(7.18543620457005,3.39596551344063,0.965404864874389));
#108386=CARTESIAN_POINT('Ctrl Pts',(7.039929788,3.267335925,1.732595906));
#108387=CARTESIAN_POINT('Ctrl Pts',(7.133934145,3.331598135,1.350634904));
#108388=CARTESIAN_POINT('Ctrl Pts',(7.186060697,3.396744076,0.960745369));
#108389=CARTESIAN_POINT('Ctrl Pts',(7.337549087,3.267335925,1.552537729));
#108390=CARTESIAN_POINT('Ctrl Pts',(7.421784141,3.331598135,1.154428985));
#108391=CARTESIAN_POINT('Ctrl Pts',(7.462451646,3.396744076,0.749543483));
#108392=CARTESIAN_POINT('Origin',(-0.194682376371735,3.48208258157526,-0.0117018368190408));
#108393=CARTESIAN_POINT('Ctrl Pts',(6.808283879,3.396737969,2.491941134));
#108394=CARTESIAN_POINT('Ctrl Pts',(6.850173276,3.376870318,2.377494247));
#108395=CARTESIAN_POINT('Ctrl Pts',(6.888192401,3.357142857,2.261704102));
#108396=CARTESIAN_POINT('Ctrl Pts',(6.974111103,3.312561141,2.00003214));
#108397=CARTESIAN_POINT('Ctrl Pts',(7.039929788,3.267335925,1.732595906));
#108398=CARTESIAN_POINT('Ctrl Pts',(6.954721399,3.396737969,2.807463316));
#108399=CARTESIAN_POINT('Ctrl Pts',(7.001914706,3.376870318,2.690554822));
#108400=CARTESIAN_POINT('Ctrl Pts',(7.04515201,3.357142857,2.572126194));
#108401=CARTESIAN_POINT('Ctrl Pts',(7.142863175,3.312561141,2.304491575));
#108402=CARTESIAN_POINT('Ctrl Pts',(7.219987966,3.267335925,2.030215204));
#108403=CARTESIAN_POINT('',(6.80991119073934,3.39596551375276,2.48749061769332));
#108404=CARTESIAN_POINT('Ctrl Pts',(6.80991119222407,3.39596551241334,2.48749061268678));
#108405=CARTESIAN_POINT('Ctrl Pts',(6.83728880486597,3.38295904379503,2.41253993402923));
#108406=CARTESIAN_POINT('Ctrl Pts',(6.86338528591401,3.37001483647005,2.33725606338888));
#108407=CARTESIAN_POINT('Ctrl Pts',(6.88819240069204,3.35714285718407,2.26170410317289));
#108408=CARTESIAN_POINT('Ctrl Pts',(6.93426633835587,3.3332358944779,2.12138241075397));
#108409=CARTESIAN_POINT('Ctrl Pts',(6.97620751152916,3.30907954004391,1.97916730415587));
#108410=CARTESIAN_POINT('Ctrl Pts',(7.01382116403914,3.2847385838048,1.83543255897252));
#108411=CARTESIAN_POINT('Ctrl Pts',(7.02276951907545,3.27894782689033,1.80123780666515));
#108412=CARTESIAN_POINT('Ctrl Pts',(7.03147314347654,3.27314663953617,1.76695717111046));
#108413=CARTESIAN_POINT('Ctrl Pts',(7.03992978840013,3.267335925,1.73259590666138));
#108414=CARTESIAN_POINT('Ctrl Pts',(7.045491636111,3.35698786875769,2.57119575441533));
#108415=CARTESIAN_POINT('Ctrl Pts',(7.00758936241169,3.36293886830875,2.55776299522492));
#108416=CARTESIAN_POINT('Ctrl Pts',(6.96823253199427,3.36926348165724,2.54380089152843));
#108417=CARTESIAN_POINT('Ctrl Pts',(6.88835362328747,3.38247029190796,2.51541977092196));
#108418=CARTESIAN_POINT('Ctrl Pts',(6.84910305541214,3.38913025463968,2.5014550247814));
#108419=CARTESIAN_POINT('Ctrl Pts',(6.80991119013386,3.39596551352048,2.48749061958343));
#108420=CARTESIAN_POINT('Ctrl Pts',(6.502883238,3.267335925,3.205465582));
#108421=CARTESIAN_POINT('Ctrl Pts',(6.676800149,3.331598135,2.852642774));
#108422=CARTESIAN_POINT('Ctrl Pts',(6.811522736,3.396744076,2.483074308));
#108423=CARTESIAN_POINT('Ctrl Pts',(6.832251548,3.267335925,3.093596417));
#108424=CARTESIAN_POINT('Ctrl Pts',(7.000098845,3.331598135,2.722903281));
#108425=CARTESIAN_POINT('Ctrl Pts',(7.126853981,3.396744076,2.336226088));
#108426=CARTESIAN_POINT('Origin',(-0.187615177368009,3.48208256415948,-0.0532791725642151));
#108427=CARTESIAN_POINT('Ctrl Pts',(6.113416303,3.396737969,3.897260718));
#108428=CARTESIAN_POINT('Ctrl Pts',(6.178929047,3.376870318,3.794494518));
#108429=CARTESIAN_POINT('Ctrl Pts',(6.240950764,3.357142857,3.68958447));
#108430=CARTESIAN_POINT('Ctrl Pts',(6.381112471,3.312561141,3.452500234));
#108431=CARTESIAN_POINT('Ctrl Pts',(6.502883238,3.267335925,3.205465582));
#108432=CARTESIAN_POINT('Ctrl Pts',(6.188602252,3.396737969,4.236885904));
#108433=CARTESIAN_POINT('Ctrl Pts',(6.259824077,3.376870318,4.132855832));
#108434=CARTESIAN_POINT('Ctrl Pts',(6.327509171,3.357142857,4.026490742));
#108435=CARTESIAN_POINT('Ctrl Pts',(6.480469435,3.312561141,3.786118284));
#108436=CARTESIAN_POINT('Ctrl Pts',(6.614752403,3.267335925,3.534833892));
#108437=CARTESIAN_POINT('',(6.11596229868539,3.39596551374412,3.89326407617423));
#108438=CARTESIAN_POINT('Ctrl Pts',(6.11596230129545,3.39596551235726,3.89326407151603));
#108439=CARTESIAN_POINT('Ctrl Pts',(6.15881202082059,3.3829590437766,3.82595107545144));
#108440=CARTESIAN_POINT('Ctrl Pts',(6.20048218733259,3.37001483646751,3.75803727209581));
#108441=CARTESIAN_POINT('Ctrl Pts',(6.24095076366032,3.35714285712456,3.68958447086456));
#108442=CARTESIAN_POINT('Ctrl Pts',(6.31611262983619,3.33323586399187,3.5624477948108));
#108443=CARTESIAN_POINT('Ctrl Pts',(6.38764537173352,3.30907947870888,3.43257354309568));
#108444=CARTESIAN_POINT('Ctrl Pts',(6.45527843514372,3.28473849130112,3.3002848860287));
#108445=CARTESIAN_POINT('Ctrl Pts',(6.47136835562607,3.27894776510738,3.26881338576536));
#108446=CARTESIAN_POINT('Ctrl Pts',(6.48723773182478,3.27314660859326,3.23720540176058));
#108447=CARTESIAN_POINT('Ctrl Pts',(6.502883238,3.267335925,3.205465582));
#108448=CARTESIAN_POINT('Ctrl Pts',(6.32804087382115,3.35698786876481,4.02565506518012));
#108449=CARTESIAN_POINT('Ctrl Pts',(6.29391238080765,3.36293886823552,4.00438848822485));
#108450=CARTESIAN_POINT('Ctrl Pts',(6.25847712951975,3.36926348181522,3.98229225475981));
#108451=CARTESIAN_POINT('Ctrl Pts',(6.18656726015517,3.38247021623562,3.93740332255877));
#108452=CARTESIAN_POINT('Ctrl Pts',(6.15123613580125,3.38913021753919,3.91532721514912));
#108453=CARTESIAN_POINT('Ctrl Pts',(6.11596229760619,3.39596551350274,3.89326407782484));
#108454=CARTESIAN_POINT('Ctrl Pts',(5.66176909400001,3.267335925,4.528451251));
#108455=CARTESIAN_POINT('Ctrl Pts',(5.907466399,3.331598135,4.221264238));
#108456=CARTESIAN_POINT('Ctrl Pts',(6.11848554200001,3.396744076,3.889297452));
#108457=CARTESIAN_POINT('Ctrl Pts',(6.00748552,3.267335925,4.490001975));
#108458=CARTESIAN_POINT('Ctrl Pts',(6.251096707,3.331598135,4.164057646));
#108459=CARTESIAN_POINT('Ctrl Pts',(6.458012545,3.396744076,3.813669358));
#108460=CARTESIAN_POINT('Origin',(-0.171775537985642,3.48208257530023,-0.0923653531614632));
#108461=CARTESIAN_POINT('Ctrl Pts',(5.132692175,3.396737969,5.120348722));
#108462=CARTESIAN_POINT('Ctrl Pts',(5.218764963,3.376870318,5.03406844200001));
#108463=CARTESIAN_POINT('Ctrl Pts',(5.301889206,3.357142857,4.944943968));
#108464=CARTESIAN_POINT('Ctrl Pts',(5.489740113,3.312561141,4.743533254));
#108465=CARTESIAN_POINT('Ctrl Pts',(5.661769094,3.267335925,4.52845125));
#108466=CARTESIAN_POINT('Ctrl Pts',(5.133110943,3.396737969,5.468196417));
#108467=CARTESIAN_POINT('Ctrl Pts',(5.22503103100001,3.376870318,5.381909097));
#108468=CARTESIAN_POINT('Ctrl Pts',(5.313999035,3.357142857,5.292581058));
#108469=CARTESIAN_POINT('Ctrl Pts',(5.51505614700001,3.312561141,5.09071031));
#108470=CARTESIAN_POINT('Ctrl Pts',(5.70021837,3.267335925,4.874167676));
#108471=CARTESIAN_POINT('',(5.13603780693678,3.39596551375112,5.11699283301184));
#108472=CARTESIAN_POINT('Ctrl Pts',(5.13603781027852,3.39596551232431,5.11699282926967));
#108473=CARTESIAN_POINT('Ctrl Pts',(5.19235603125485,3.38295904386035,5.06046499702263));
#108474=CARTESIAN_POINT('Ctrl Pts',(5.24765143270648,3.37001483656328,5.0030968345882));
#108475=CARTESIAN_POINT('Ctrl Pts',(5.30188920504041,3.35714285723109,4.9449439694496));
#108476=CARTESIAN_POINT('Ctrl Pts',(5.40262434824966,3.33323588965341,4.8369373737601));
#108477=CARTESIAN_POINT('Ctrl Pts',(5.50040371818527,3.30907953040397,4.72547705731968));
#108478=CARTESIAN_POINT('Ctrl Pts',(5.59489361499051,3.28473856932848,4.61082047448819));
#108479=CARTESIAN_POINT('Ctrl Pts',(5.61737290688907,3.27894781722051,4.58354349694134));
#108480=CARTESIAN_POINT('Ctrl Pts',(5.63966614902101,3.27314663469309,4.55608581445833));
#108481=CARTESIAN_POINT('Ctrl Pts',(5.6617690941662,3.267335925,4.52845125149442));
#108482=CARTESIAN_POINT('Ctrl Pts',(5.31469795297972,3.35698786870842,5.29187921908844));
#108483=CARTESIAN_POINT('Ctrl Pts',(5.28593899785827,3.36293887909632,5.26377317423017));
#108484=CARTESIAN_POINT('Ctrl Pts',(5.25608237635442,3.36926346364826,5.23457613979773));
#108485=CARTESIAN_POINT('Ctrl Pts',(5.19550343018046,3.38247021624225,5.17527810805215));
#108486=CARTESIAN_POINT('Ctrl Pts',(5.165744038557,3.38913021751788,5.14612298051144));
#108487=CARTESIAN_POINT('Ctrl Pts',(5.13603780535955,3.39596551346047,5.11699283455206));
#108488=CARTESIAN_POINT('Ctrl Pts',(4.55591692,3.267335925,5.639691571));
#108489=CARTESIAN_POINT('Ctrl Pts',(4.861906086,3.331598135,5.392504079));
#108490=CARTESIAN_POINT('Ctrl Pts',(5.139354765,3.396744076,5.113661369));
#108491=CARTESIAN_POINT('Ctrl Pts',(4.901816146,3.267335925,5.67646003));
#108492=CARTESIAN_POINT('Ctrl Pts',(5.209800235,3.331598135,5.410505303));
#108493=CARTESIAN_POINT('Ctrl Pts',(5.48720162,3.396744076,5.112789687));
#108494=CARTESIAN_POINT('Origin',(-0.147903616601148,3.48208256703089,-0.127132486034253));
#108495=CARTESIAN_POINT('Ctrl Pts',(3.911969065,3.396737969,6.104014911));
#108496=CARTESIAN_POINT('Ctrl Pts',(4.014577229,3.376870318,6.03825492));
#108497=CARTESIAN_POINT('Ctrl Pts',(4.114917201,3.357142857,5.969083383));
#108498=CARTESIAN_POINT('Ctrl Pts',(4.341673608,3.312561141,5.812763932));
#108499=CARTESIAN_POINT('Ctrl Pts',(4.55591692,3.267335925,5.639691571));
#108500=CARTESIAN_POINT('Ctrl Pts',(3.837601071,3.396737969,6.44382014200001));
#108501=CARTESIAN_POINT('Ctrl Pts',(3.945921342,3.376870318,6.379310274));
#108502=CARTESIAN_POINT('Ctrl Pts',(4.052012211,3.357142857,6.311196166));
#108503=CARTESIAN_POINT('Ctrl Pts',(4.291764963,3.312561141,6.157266379));
#108504=CARTESIAN_POINT('Ctrl Pts',(4.519148461,3.267335925,5.985590797));
#108505=CARTESIAN_POINT('',(3.91595789500395,3.39596551384657,6.10145669215797));
#108506=CARTESIAN_POINT('Ctrl Pts',(3.91595789925708,3.39596551228061,6.10145668921002));
#108507=CARTESIAN_POINT('Ctrl Pts',(3.98311124483374,3.38295904374827,6.05835719870953));
#108508=CARTESIAN_POINT('Ctrl Pts',(4.04944632971667,3.37001483646856,6.01421714884346));
#108509=CARTESIAN_POINT('Ctrl Pts',(4.11491719996409,3.35714285720156,5.9690833837649));
#108510=CARTESIAN_POINT('Ctrl Pts',(4.23651531527283,3.3332359135643,5.88525708363404));
#108511=CARTESIAN_POINT('Ctrl Pts',(4.35596921437483,3.30907957859659,5.79742241323709));
#108512=CARTESIAN_POINT('Ctrl Pts',(4.4728976542248,3.28473864218913,5.70575907122463));
#108513=CARTESIAN_POINT('Ctrl Pts',(4.50071525452162,3.27894786587584,5.68395210780971));
#108514=CARTESIAN_POINT('Ctrl Pts',(4.52838999981166,3.27314665905663,5.66192866720594));
#108515=CARTESIAN_POINT('Ctrl Pts',(4.55591691995108,3.267335925,5.63969157146022));
#108516=CARTESIAN_POINT('Ctrl Pts',(4.05284566323258,3.35698786873722,6.31066098193971));
#108517=CARTESIAN_POINT('Ctrl Pts',(4.03080108981236,3.36293886711398,6.27702978340556));
#108518=CARTESIAN_POINT('Ctrl Pts',(4.00791888511499,3.36926348337905,6.24209689463089));
#108519=CARTESIAN_POINT('Ctrl Pts',(3.96150363406496,3.38247021623708,6.17116264113993));
#108520=CARTESIAN_POINT('Ctrl Pts',(3.93870749073462,3.38913021755258,6.13629175453415));
#108521=CARTESIAN_POINT('Ctrl Pts',(3.91595789307705,3.39596551346942,6.10145669334236));
#108522=CARTESIAN_POINT('Ctrl Pts',(3.237035134,3.267335925,6.487226182));
#108523=CARTESIAN_POINT('Ctrl Pts',(3.589008448,3.331598135,6.311596421));
#108524=CARTESIAN_POINT('Ctrl Pts',(3.919913471,3.396744076,6.098916164));
#108525=CARTESIAN_POINT('Ctrl Pts',(3.566943297,3.267335925,6.597493124));
#108526=CARTESIAN_POINT('Ctrl Pts',(3.924899294,3.331598135,6.403963745));
#108527=CARTESIAN_POINT('Ctrl Pts',(4.259815245,3.396744076,6.172841653));
#108528=CARTESIAN_POINT('Origin',(-0.11711599026234,3.48208228754832,-0.155955219364179));
#108529=CARTESIAN_POINT('Ctrl Pts',(2.50832663,3.396737969,6.802264146));
#108530=CARTESIAN_POINT('Ctrl Pts',(2.622672326,3.376870318,6.76009931));
#108531=CARTESIAN_POINT('Ctrl Pts',(2.735536241,3.357142857,6.714115092));
#108532=CARTESIAN_POINT('Ctrl Pts',(2.99059527,3.312561141,6.610196228));
#108533=CARTESIAN_POINT('Ctrl Pts',(3.237035134,3.267335925,6.487226182));
#108534=CARTESIAN_POINT('Ctrl Pts',(2.362649238,3.396737969,7.118138));
#108535=CARTESIAN_POINT('Ctrl Pts',(2.482304756,3.376870318,7.078421992));
#108536=CARTESIAN_POINT('Ctrl Pts',(2.600557799,3.357142857,7.034706755));
#108537=CARTESIAN_POINT('Ctrl Pts',(2.867795619,3.312561141,6.935915516));
#108538=CARTESIAN_POINT('Ctrl Pts',(3.126768193,3.267335925,6.817134344));
#108539=CARTESIAN_POINT('',(2.51277214475068,3.39596551375339,6.80062321798605));
#108540=CARTESIAN_POINT('Ctrl Pts',(2.51277214949544,3.39596551225138,6.80062321598465));
#108541=CARTESIAN_POINT('Ctrl Pts',(2.58762060356924,3.38295904370181,6.77296735215514));
#108542=CARTESIAN_POINT('Ctrl Pts',(2.66189361690341,3.37001483643105,6.74411935425174));
#108543=CARTESIAN_POINT('Ctrl Pts',(2.73553623993914,3.3571428571487,6.71411509284571));
#108544=CARTESIAN_POINT('Ctrl Pts',(2.87231202328787,3.33323584566299,6.65838844796532));
#108545=CARTESIAN_POINT('Ctrl Pts',(3.00785539350867,3.30907944181061,6.598286178192));
#108546=CARTESIAN_POINT('Ctrl Pts',(3.1417553897474,3.28473843554526,6.53390182583033));
#108547=CARTESIAN_POINT('Ctrl Pts',(3.17361009877579,3.27894772834719,6.51858483652433));
#108548=CARTESIAN_POINT('Ctrl Pts',(3.2053718310647,3.27314659089702,6.50302572734794));
#108549=CARTESIAN_POINT('Ctrl Pts',(3.23703512624063,3.26733592642395,6.48722618587181));
#108550=CARTESIAN_POINT('Ctrl Pts',(2.60148681409268,3.35698786873481,7.03436325144702));
#108551=CARTESIAN_POINT('Ctrl Pts',(2.58718731604156,3.36293887879503,6.99677932612183));
#108552=CARTESIAN_POINT('Ctrl Pts',(2.57234969575745,3.36926346386341,6.9577443421693));
#108553=CARTESIAN_POINT('Ctrl Pts',(2.54226833099559,3.38247021621572,6.87849046822266));
#108554=CARTESIAN_POINT('Ctrl Pts',(2.52750135875675,3.38913021753285,6.83953434665205));
#108555=CARTESIAN_POINT('Ctrl Pts',(2.51277214241879,3.39596551346009,6.80062321881723));
#108556=CARTESIAN_POINT('Ctrl Pts',(1.766793184,3.267335925,7.031425307));
#108557=CARTESIAN_POINT('Ctrl Pts',(2.148292764,3.331598135,6.93556553));
#108558=CARTESIAN_POINT('Ctrl Pts',(2.51718138,3.396744076,6.798992418));
#108559=CARTESIAN_POINT('Ctrl Pts',(2.065284143,3.267335925,7.21003477200001));
#108560=CARTESIAN_POINT('Ctrl Pts',(2.456474424,3.331598135,7.097979961));
#108561=CARTESIAN_POINT('Ctrl Pts',(2.833244645,3.396744076,6.944258404));
#108562=CARTESIAN_POINT('Origin',(-0.0808521869256668,3.48208254633516,
-0.177485595265519));
#108563=CARTESIAN_POINT('Ctrl Pts',(0.98739763,3.396737969,7.182447071));
#108564=CARTESIAN_POINT('Ctrl Pts',(1.10813418,3.376870318,7.165848969));
#108565=CARTESIAN_POINT('Ctrl Pts',(1.228244647,3.357142857,7.145202243));
#108566=CARTESIAN_POINT('Ctrl Pts',(1.499680022,3.312561141,7.098543095));
#108567=CARTESIAN_POINT('Ctrl Pts',(1.766793184,3.267335925,7.031425307));
#108568=CARTESIAN_POINT('Ctrl Pts',(0.777222552,3.396737969,7.459619635));
#108569=CARTESIAN_POINT('Ctrl Pts',(0.902618358,3.376870318,7.446554566));
#108570=CARTESIAN_POINT('Ctrl Pts',(1.027504195,3.357142857,7.429282275));
#108571=CARTESIAN_POINT('Ctrl Pts',(1.309731339,3.312561141,7.390248953));
#108572=CARTESIAN_POINT('Ctrl Pts',(1.588183719,3.267335925,7.329916267));
#108573=CARTESIAN_POINT('',(0.992091960819354,3.3959655138041,7.18180016023131));
#108574=CARTESIAN_POINT('Ctrl Pts',(0.992091965201248,3.39596551263151,
7.18180016009836));
#108575=CARTESIAN_POINT('Ctrl Pts',(1.07113569834774,3.38295904380298,7.17088107956549));
#108576=CARTESIAN_POINT('Ctrl Pts',(1.14987371695153,3.37001483640952,7.15867403457068));
#108577=CARTESIAN_POINT('Ctrl Pts',(1.22824464557595,3.35714285718804,7.14520224359184));
#108578=CARTESIAN_POINT('Ctrl Pts',(1.3738017716988,3.33323592741606,7.12018129133799));
#108579=CARTESIAN_POINT('Ctrl Pts',(1.51909593195878,3.30907960644241,7.09062211347458));
#108580=CARTESIAN_POINT('Ctrl Pts',(1.663705666322,3.28473868418063,7.05652771971352));
#108581=CARTESIAN_POINT('Ctrl Pts',(1.69810882624232,3.27894789392113,7.04841654458334));
#108582=CARTESIAN_POINT('Ctrl Pts',(1.73247323072682,3.27314667310194,7.04004891557619));
#108583=CARTESIAN_POINT('Ctrl Pts',(1.766793184,3.267335925,7.031425307));
#108584=CARTESIAN_POINT('Ctrl Pts',(1.02848533315043,3.35698786876585,7.4291465131798));
#108585=CARTESIAN_POINT('Ctrl Pts',(1.02259958178645,3.36293887945333,7.38936730565414));
#108586=CARTESIAN_POINT('Ctrl Pts',(1.01650022449133,3.36926346446715,7.34805528870315));
#108587=CARTESIAN_POINT('Ctrl Pts',(1.00415932290298,3.38247028390876,7.26418729613533));
#108588=CARTESIAN_POINT('Ctrl Pts',(0.99811204299841,3.38913025079369,7.22296771414462));
#108589=CARTESIAN_POINT('Ctrl Pts',(0.992091959548617,3.39596551362997,
7.18180016038823));
#108590=CARTESIAN_POINT('Ctrl Pts',(0.213937947,3.267335925,7.246842799));
#108591=CARTESIAN_POINT('Ctrl Pts',(0.607125298,3.331598135,7.235235304));
#108592=CARTESIAN_POINT('Ctrl Pts',(0.996748685,3.396744076,7.181155343));
#108593=CARTESIAN_POINT('Ctrl Pts',(0.467054599,3.267335925,7.485443207));
#108594=CARTESIAN_POINT('Ctrl Pts',(0.87318754,3.331598135,7.460102522));
#108595=CARTESIAN_POINT('Ctrl Pts',(1.274194673,3.396744076,7.39096935));
#108596=CARTESIAN_POINT('Origin',(-0.0408077614185605,3.48208260746332,
-0.190716837355268));
#108597=CARTESIAN_POINT('Ctrl Pts',(-0.579700987,3.396737969,7.226786752));
#108598=CARTESIAN_POINT('Ctrl Pts',(-0.458219089,3.376870318,7.236531495));
#108599=CARTESIAN_POINT('Ctrl Pts',(-0.336478302,3.357142857,7.242187677));
#108600=CARTESIAN_POINT('Ctrl Pts',(-0.061358598,3.312561141,7.254969977));
#108601=CARTESIAN_POINT('Ctrl Pts',(0.213937947,3.267335925,7.24684279900001));
#108602=CARTESIAN_POINT('Ctrl Pts',(-0.844546196,3.396737969,7.452297748));
#108603=CARTESIAN_POINT('Ctrl Pts',(-0.71927347,3.376870318,7.46649452400001));
#108604=CARTESIAN_POINT('Ctrl Pts',(-0.593594363,3.357142857,7.476472814));
#108605=CARTESIAN_POINT('Ctrl Pts',(-0.309574522,3.312561141,7.499022561));
#108606=CARTESIAN_POINT('Ctrl Pts',(-0.02466246,3.267335925,7.499959451));
#108607=CARTESIAN_POINT('Ctrl Pts',(-0.574977340788912,3.39596551522583,
7.22716410353705));
#108608=CARTESIAN_POINT('Ctrl Pts',(-0.455851638000001,3.376486685,7.23664148900001));
#108609=CARTESIAN_POINT('Ctrl Pts',(-0.336478302,3.357142857,7.242187677));
#108610=CARTESIAN_POINT('Ctrl Pts',(-0.0613585965077572,3.31256114087447,
7.25496997652748));
#108611=CARTESIAN_POINT('Ctrl Pts',(0.213937950575229,3.26733592689007,
7.24684279957603));
#108612=CARTESIAN_POINT('Ctrl Pts',(0.178686009732229,2.48690656550041,
7.24784936885964));
#108613=CARTESIAN_POINT('Ctrl Pts',(0.192365848366114,2.48917367225018,
7.24746042942977));
#108614=CARTESIAN_POINT('Ctrl Pts',(0.206045687,2.491440779,7.24707149000001));
#108615=CARTESIAN_POINT('Ctrl Pts',(0.602789375,2.557191576,7.23579144));
#108616=CARTESIAN_POINT('Ctrl Pts',(0.995930671,2.622066995,7.18126883600001));
#108617=CARTESIAN_POINT('Ctrl Pts',(0.4311616098954,2.48690656550041,7.48817560011827));
#108618=CARTESIAN_POINT('Ctrl Pts',(0.445293291484062,2.48917367225018,
7.48730837266027));
#108619=CARTESIAN_POINT('Ctrl Pts',(0.459424973072718,2.491440779,7.48644114520224));
#108620=CARTESIAN_POINT('Ctrl Pts',(0.869273043739099,2.557191576,7.46128975056695));
#108621=CARTESIAN_POINT('Ctrl Pts',(1.27392616352466,2.622066995,7.39154817726272));
#108622=CARTESIAN_POINT('',(0.458902333983518,2.4914407798504,7.4859474130173));
#108623=CARTESIAN_POINT('',(1.02398864463363,2.58208164081247,7.42976765664733));
#108624=CARTESIAN_POINT('Origin',(0.001328250839037,2.41074793646468,-0.189950586860783));
#108625=CARTESIAN_POINT('Ctrl Pts',(0.991263375970751,2.62129679704272,
7.18191457174322));
#108626=CARTESIAN_POINT('Ctrl Pts',(0.996664707245066,2.61444751350223,
7.22317185246287));
#108627=CARTESIAN_POINT('Ctrl Pts',(1.00209692939513,2.60775977698502,7.26447633270777));
#108628=CARTESIAN_POINT('Ctrl Pts',(1.01300518115998,2.59469807325527,7.34708108552444));
#108629=CARTESIAN_POINT('Ctrl Pts',(1.0184871761395,2.58831697879642,7.38842649747231));
#108630=CARTESIAN_POINT('Ctrl Pts',(1.02398863945874,2.58208164077288,7.42976764544215));
#108631=CARTESIAN_POINT('',(0.332473999383933,2.49144078146678,7.36650945118224));
#108632=CARTESIAN_POINT('Origin',(2.89210929510508E-14,2.58316965300033,
2.78423117894278E-13));
#108633=CARTESIAN_POINT('',(1.02346990113142,2.40074633455656,7.42983912063183));
#108634=CARTESIAN_POINT('Origin',(-0.00170106791189131,2.55355106829602,
-0.190812554157955));
#108635=CARTESIAN_POINT('',(1.58020016870039,2.49144077881204,7.33164152797676));
#108636=CARTESIAN_POINT('Origin',(-0.0278993116906279,2.41071458311704,
-0.19085055781879));
#108637=CARTESIAN_POINT('Origin',(-0.0308560152959829,2.55357125325729,
-0.190428015594565));
#108638=CARTESIAN_POINT('Ctrl Pts',(0.9866149,2.622074631,7.182554632));
#108639=CARTESIAN_POINT('Ctrl Pts',(1.376928915,2.556767114,7.128940056));
#108640=CARTESIAN_POINT('Ctrl Pts',(1.759134602,2.491440779,7.033345253));
#108641=CARTESIAN_POINT('Ctrl Pts',(0.776409618,2.622074631,7.459704291));
#108642=CARTESIAN_POINT('Ctrl Pts',(1.181784486,2.556767114,7.417512679));
#108643=CARTESIAN_POINT('Ctrl Pts',(1.580200173,2.491440779,7.331641522));
#108644=CARTESIAN_POINT('Ctrl Pts',(0.77430756518,2.622074631,7.46247578759));
#108645=CARTESIAN_POINT('Ctrl Pts',(1.17983304171,2.556767114,7.42039840523));
#108646=CARTESIAN_POINT('Ctrl Pts',(1.57841082871,2.491440779,7.33462448469001));
#108647=CARTESIAN_POINT('',(1.6696673844688,2.49144077849314,7.18249338820464));
#108648=CARTESIAN_POINT('Ctrl Pts',(1.73258179986369,2.48690656552405,7.03998646724969));
#108649=CARTESIAN_POINT('Ctrl Pts',(1.74585820093184,2.489173672262,7.03666586012479));
#108650=CARTESIAN_POINT('Ctrl Pts',(1.759134602,2.491440779,7.033345253));
#108651=CARTESIAN_POINT('Ctrl Pts',(2.144177766,2.557191576,6.93704076));
#108652=CARTESIAN_POINT('Ctrl Pts',(2.516406889,2.622066995,6.799279107));
#108653=CARTESIAN_POINT('Ctrl Pts',(2.03081769670521,2.48690656552405,7.22041921463527));
#108654=CARTESIAN_POINT('Ctrl Pts',(2.04443255908916,2.489173672262,7.21653436867755));
#108655=CARTESIAN_POINT('Ctrl Pts',(2.05804742147311,2.491440779,7.21264952271985));
#108656=CARTESIAN_POINT('Ctrl Pts',(2.45290666554322,2.557191576,7.09998093342908));
#108657=CARTESIAN_POINT('Ctrl Pts',(2.83310684298389,2.622066995,6.94488142061167));
#108658=CARTESIAN_POINT('',(2.05743086091823,2.49144077985044,7.21227968580291));
#108659=CARTESIAN_POINT('',(2.59722878304874,2.58208164080325,7.03593652810296));
#108660=CARTESIAN_POINT('Origin',(-0.0395365885006085,2.41074795151913,
-0.185795251756038));
#108661=CARTESIAN_POINT('Ctrl Pts',(2.51198752636068,2.62129679696105,6.80091307643713));
#108662=CARTESIAN_POINT('Ctrl Pts',(2.52613167332026,2.61444751340273,6.84004465842731));
#108663=CARTESIAN_POINT('Ctrl Pts',(2.54031613545444,2.60775977687909,6.879215695743));
#108664=CARTESIAN_POINT('Ctrl Pts',(2.56872693491772,2.5946980747769,6.95754423388337));
#108665=CARTESIAN_POINT('Ctrl Pts',(2.58296880150041,2.58831698191966,6.99674453567385));
#108666=CARTESIAN_POINT('Ctrl Pts',(2.59722877560764,2.58208164077717,7.03593651817469));
#108667=CARTESIAN_POINT('',(1.908282721884,2.49144078146678,7.1228124714158));
#108668=CARTESIAN_POINT('Origin',(7.42678488152571E-13,2.58316965300044,
2.05521363816352E-12));
#108669=CARTESIAN_POINT('',(2.59673753012003,2.40074633453864,7.0361178357593));
#108670=CARTESIAN_POINT('Origin',(-0.0426803276019039,2.55355106469629,
-0.185985695722827));
#108671=CARTESIAN_POINT('',(3.119342175801,2.4914407788122,6.82053549638486));
#108672=CARTESIAN_POINT('Origin',(-0.0682743477746839,2.41071456818591,
-0.180391257391022));
#108673=CARTESIAN_POINT('Origin',(-0.071070994550492,2.55357129094536,-0.179342759647155));
#108674=CARTESIAN_POINT('Ctrl Pts',(2.507585323,2.622074631,6.802537457));
#108675=CARTESIAN_POINT('Ctrl Pts',(2.877248464,2.556767114,6.666270384));
#108676=CARTESIAN_POINT('Ctrl Pts',(3.229968338,2.491440779,6.49074761));
#108677=CARTESIAN_POINT('Ctrl Pts',(2.361873508,2.622074631,7.118395433));
#108678=CARTESIAN_POINT('Ctrl Pts',(2.748700987,2.556767114,6.990046624));
#108679=CARTESIAN_POINT('Ctrl Pts',(3.119342177,2.491440779,6.820535491));
#108680=CARTESIAN_POINT('Ctrl Pts',(2.36041638985,2.622074631,7.12155401276));
#108681=CARTESIAN_POINT('Ctrl Pts',(2.74741551223,2.556767114,6.9932843864));
#108682=CARTESIAN_POINT('Ctrl Pts',(3.11823591539,2.491440779,6.82383336981));
#108683=CARTESIAN_POINT('',(3.17465525469772,2.49144077849433,6.65564155183665));
#108684=CARTESIAN_POINT('Ctrl Pts',(3.2054639914271,2.48690656571219,6.50294162341348));
#108685=CARTESIAN_POINT('Ctrl Pts',(3.21771616471352,2.48917367235607,6.49684461670674));
#108686=CARTESIAN_POINT('Ctrl Pts',(3.229968338,2.491440779,6.49074761));
#108687=CARTESIAN_POINT('Ctrl Pts',(3.585306787,2.557191576,6.313921764));
#108688=CARTESIAN_POINT('Ctrl Pts',(3.919218717,2.622066995,6.099362643));
#108689=CARTESIAN_POINT('Ctrl Pts',(3.53551500587727,2.4869065657122,6.61504405117166));
#108690=CARTESIAN_POINT('Ctrl Pts',(3.54797643276839,2.48917367235607,6.60832323804217));
#108691=CARTESIAN_POINT('Ctrl Pts',(3.56043785965957,2.491440779,6.6016024249127));
#108692=CARTESIAN_POINT('Ctrl Pts',(3.92184509740445,2.557191576,6.40668489823342));
#108693=CARTESIAN_POINT('Ctrl Pts',(4.25981459571951,2.622066995,6.17347972708782));
#108694=CARTESIAN_POINT('',(3.55975620996069,2.49144077985043,6.60137377688286));
#108695=CARTESIAN_POINT('',(4.04902538988259,2.58208164076325,6.31311282687116));
#108696=CARTESIAN_POINT('Origin',(-0.0785528899479215,2.41074794720924,
-0.172952521176576));
#108697=CARTESIAN_POINT('Ctrl Pts',(3.91525393165237,2.62129679694602,6.10190844352683));
#108698=CARTESIAN_POINT('Ctrl Pts',(3.93747952956042,2.61444751341348,6.13708457730189));
#108699=CARTESIAN_POINT('Ctrl Pts',(3.95975298189506,2.60775977689882,6.17229057739767));
#108700=CARTESIAN_POINT('Ctrl Pts',(4.00433788126619,2.59469807234326,6.24268036890378));
#108701=CARTESIAN_POINT('Ctrl Pts',(4.02667369633177,2.5883169770036,6.27790262364398));
#108702=CARTESIAN_POINT('Ctrl Pts',(4.0490253804682,2.58208164071723,6.31311281894294));
#108703=CARTESIAN_POINT('',(3.39486226506754,2.49144078146677,6.54606069746623));
#108704=CARTESIAN_POINT('Origin',(7.0906822080552E-14,2.58316965300056,
1.24032728532342E-13));
#108705=CARTESIAN_POINT('',(4.04858459835607,2.40074633454437,6.31339550070062));
#108706=CARTESIAN_POINT('Origin',(-0.081663894348511,2.55355105428733,-0.172462402234757));
#108707=CARTESIAN_POINT('',(4.51262720696831,2.4914407788122,5.99050880554589));
#108708=CARTESIAN_POINT('Origin',(-0.105456859430594,2.41071461865303,-0.161496726585507));
#108709=CARTESIAN_POINT('Origin',(-0.10796268082271,2.55357129252955,-0.159871514079931));
#108710=CARTESIAN_POINT('Ctrl Pts',(3.911303843,2.622074631,6.104441191));
#108711=CARTESIAN_POINT('Ctrl Pts',(4.243031073,2.556767114,5.891893318));
#108712=CARTESIAN_POINT('Ctrl Pts',(4.549772344,2.491440779,5.644649822));
#108713=CARTESIAN_POINT('Ctrl Pts',(3.836898817,2.622074631,6.444238315));
#108714=CARTESIAN_POINT('Ctrl Pts',(4.187091285,2.556767114,6.235733757));
#108715=CARTESIAN_POINT('Ctrl Pts',(4.512627207,2.491440779,5.99050880000001));
#108716=CARTESIAN_POINT('Ctrl Pts',(3.83615476674,2.622074631,6.44763628624));
#108717=CARTESIAN_POINT('Ctrl Pts',(4.18653188712,2.556767114,6.23917216139));
#108718=CARTESIAN_POINT('Ctrl Pts',(4.51225575563,2.491440779,5.99396738978001));
#108719=CARTESIAN_POINT('',(4.53119977305058,2.49144077849433,5.8175793129078));
#108720=CARTESIAN_POINT('Ctrl Pts',(4.52846224709165,2.48690656555413,5.66182645693944));
#108721=CARTESIAN_POINT('Ctrl Pts',(4.53911729554583,2.48917367227704,5.6532381394697));
#108722=CARTESIAN_POINT('Ctrl Pts',(4.549772344,2.491440779,5.644649822));
#108723=CARTESIAN_POINT('Ctrl Pts',(4.85879084800001,2.557191576,5.395570803));
#108724=CARTESIAN_POINT('Ctrl Pts',(5.138772234,2.622066995,5.114246761));
#108725=CARTESIAN_POINT('Ctrl Pts',(4.87489556037499,2.48690656555413,5.70035678045006));
#108726=CARTESIAN_POINT('Ctrl Pts',(4.88562087025615,2.48917367227704,5.69111425748587));
#108727=CARTESIAN_POINT('Ctrl Pts',(4.89634618013719,2.491440779,5.68187173452161));
#108728=CARTESIAN_POINT('Ctrl Pts',(5.20740241124098,2.557191576,5.41381939934162));
#108729=CARTESIAN_POINT('Ctrl Pts',(5.48733815209132,2.622066995,5.11341298321399));
#108730=CARTESIAN_POINT('',(4.89563131445871,2.49144077985042,5.6817949666801));
#108731=CARTESIAN_POINT('',(5.31149407010535,2.58208164084134,5.29509498696339));
#108732=CARTESIAN_POINT('Origin',(-0.113895876282957,2.41074793632891,-0.15202226988008));
#108733=CARTESIAN_POINT('Ctrl Pts',(5.13544741496347,2.62129679693993,5.11758535379643));
#108734=CARTESIAN_POINT('Ctrl Pts',(5.16471521985902,2.61444751339497,5.14716124259995));
#108735=CARTESIAN_POINT('Ctrl Pts',(5.19403618067066,2.6077597768829,5.17675601218363));
#108736=CARTESIAN_POINT('Ctrl Pts',(5.25271042576565,2.59469807426784,5.23591568543397));
#108737=CARTESIAN_POINT('Ctrl Pts',(5.28209577596687,2.5883169808747,5.26551291392302));
#108738=CARTESIAN_POINT('Ctrl Pts',(5.31149405920984,2.58208164081004,5.29509498109586));
#108739=CARTESIAN_POINT('',(4.72270182137915,2.49144078146676,5.66322240019092));
#108740=CARTESIAN_POINT('Origin',(-6.40546643504436E-13,2.58316965300033,
-6.43148728718401E-13));
#108741=CARTESIAN_POINT('',(5.31112435035526,2.40074633451093,5.29546580931694));
#108742=CARTESIAN_POINT('Origin',(-0.116828924643203,2.55355111047958,-0.1508749981619));
#108743=CARTESIAN_POINT('',(5.69490680501467,2.49144077881248,4.8803725837289));
#108744=CARTESIAN_POINT('Origin',(-0.137708370212528,2.41071459951173,-0.135050933525499));
#108745=CARTESIAN_POINT('Origin',(-0.139806310418847,2.55357127476894,-0.132925095633139));
#108746=CARTESIAN_POINT('Ctrl Pts',(5.132134143,2.622074631,5.120908039));
#108747=CARTESIAN_POINT('Ctrl Pts',(5.410414265,2.556767114,4.842017869));
#108748=CARTESIAN_POINT('Ctrl Pts',(5.656834052,2.491440779,4.534614483));
#108749=CARTESIAN_POINT('Ctrl Pts',(5.132515003,2.622074631,5.468755777));
#108750=CARTESIAN_POINT('Ctrl Pts',(5.429697849,2.556767114,5.18984491));
#108751=CARTESIAN_POINT('Ctrl Pts',(5.694906805,2.491440779,4.880372576));
#108752=CARTESIAN_POINT('Ctrl Pts',(5.1325188116,2.622074631,5.47223425438));
#108753=CARTESIAN_POINT('Ctrl Pts',(5.42989068484001,2.556767114,5.19332318041001));
#108754=CARTESIAN_POINT('Ctrl Pts',(5.69528753253,2.491440779,4.88383015693));
#108755=CARTESIAN_POINT('',(5.67587042651797,2.49144077849433,4.70749353188976));
#108756=CARTESIAN_POINT('Ctrl Pts',(5.63971464197941,2.4869065655115,4.55597057888841));
#108757=CARTESIAN_POINT('Ctrl Pts',(5.64827434698972,2.48917367225572,4.54529253094417));
#108758=CARTESIAN_POINT('Ctrl Pts',(5.65683405200001,2.491440779,4.534614483));
#108759=CARTESIAN_POINT('Ctrl Pts',(5.905083248,2.557191576,4.224928949));
#108760=CARTESIAN_POINT('Ctrl Pts',(6.118042472,2.622066995,3.889994385));
#108761=CARTESIAN_POINT('Ctrl Pts',(5.98633141772411,2.4869065655115,4.51912716241547));
#108762=CARTESIAN_POINT('Ctrl Pts',(5.99481910667497,2.48917367225572,4.50779509979886));
#108763=CARTESIAN_POINT('Ctrl Pts',(6.00330679562579,2.491440779,4.49646303718222));
#108764=CARTESIAN_POINT('Ctrl Pts',(6.24946737655826,2.557191576,4.1678097214174));
#108765=CARTESIAN_POINT('Ctrl Pts',(6.45827987534397,2.622066995,3.81424873074632));
#108766=CARTESIAN_POINT('',(6.00259214027373,2.49144077985043,4.49654173912977));
#108767=CARTESIAN_POINT('',(6.32560319063832,2.5820816408139,4.02948439011544));
#108768=CARTESIAN_POINT('Origin',(-0.14391329291115,2.41074795037636,-0.123983781589465));
#108769=CARTESIAN_POINT('Ctrl Pts',(6.11551308426914,2.6212967969781,3.89396966096671));
#108770=CARTESIAN_POINT('Ctrl Pts',(6.15045456600537,2.61444751341353,3.91656236895765));
#108771=CARTESIAN_POINT('Ctrl Pts',(6.18545201972378,2.60775977688574,3.93916208936406));
#108772=CARTESIAN_POINT('Ctrl Pts',(6.25547208577829,2.59469807216963,3.98432542110109));
#108773=CARTESIAN_POINT('Ctrl Pts',(6.29053296465008,2.58831697663297,4.00691370917541));
#108774=CARTESIAN_POINT('Ctrl Pts',(6.32560317876756,2.58208164076528,4.02948438689549));
#108775=CARTESIAN_POINT('',(5.82971308973407,2.49144078146677,4.51557811846253));
#108776=CARTESIAN_POINT('Origin',(1.00527225432856E-12,2.58316965300022,
6.98876720384156E-13));
#108777=CARTESIAN_POINT('',(6.3253218305668,2.4007463345075,4.02992602189079));
#108778=CARTESIAN_POINT('Origin',(-0.146531164652753,2.553551096683,-0.122232832307339));
#108779=CARTESIAN_POINT('',(6.61089889168057,2.49144077881248,3.54203556251265));
#108780=CARTESIAN_POINT('Origin',(-0.163520847235297,2.41071460928183,-0.102290334524298));
#108781=CARTESIAN_POINT('Origin',(-0.16511287802337,2.55357127486387,-0.0997632859032118));
#108782=CARTESIAN_POINT('Ctrl Pts',(6.11299155399999,2.622074631,3.897926919));
#108783=CARTESIAN_POINT('Ctrl Pts',(6.324812498,2.556767114,3.565735045));
#108784=CARTESIAN_POINT('Ctrl Pts',(6.499388487,2.491440779,3.21254561));
#108785=CARTESIAN_POINT('Ctrl Pts',(6.188140491,2.622074631,4.237560296));
#108786=CARTESIAN_POINT('Ctrl Pts',(6.418417775,2.556767114,3.901284683));
#108787=CARTESIAN_POINT('Ctrl Pts',(6.61089889,2.491440779,3.542035555));
#108788=CARTESIAN_POINT('Ctrl Pts',(6.18889198036999,2.622074631,4.24095662977));
#108789=CARTESIAN_POINT('Ctrl Pts',(6.41935382777,2.556767114,3.90464017938));
#108790=CARTESIAN_POINT('Ctrl Pts',(6.61201399403,2.491440779,3.54533045445));
#108791=CARTESIAN_POINT('',(6.55514368707803,2.49144077849433,3.37729058525997));
#108792=CARTESIAN_POINT('Ctrl Pts',(6.48726024865665,2.48690656555131,3.23708257910937));
#108793=CARTESIAN_POINT('Ctrl Pts',(6.49332436782831,2.48917367227563,3.22481409455469));
#108794=CARTESIAN_POINT('Ctrl Pts',(6.499388487,2.491440779,3.21254561));
#108795=CARTESIAN_POINT('Ctrl Pts',(6.67526052,2.557191576,2.856734113));
#108796=CARTESIAN_POINT('Ctrl Pts',(6.81123984400001,2.622066995,2.483850194));
#108797=CARTESIAN_POINT('Ctrl Pts',(6.817853071007,2.48690656555132,3.12658818021115));
#108798=CARTESIAN_POINT('Ctrl Pts',(6.82370626395992,2.48917367227563,3.11369645281647));
#108799=CARTESIAN_POINT('Ctrl Pts',(6.829559456913,2.491440779,3.10080472542187));
#108800=CARTESIAN_POINT('Ctrl Pts',(6.99931419211015,2.557191576,2.72691789345473));
#108801=CARTESIAN_POINT('Ctrl Pts',(7.12723960977484,2.622066995,2.33673444670107));
#108802=CARTESIAN_POINT('',(6.82887843004262,2.4914407798504,3.10103521501192));
#108803=CARTESIAN_POINT('',(7.04393413620837,2.58208164078061,2.5754595818908));
#108804=CARTESIAN_POINT('Origin',(-0.1672016121272,2.41074790913348,-0.0901480503329738));
#108805=CARTESIAN_POINT('Ctrl Pts',(6.8096241586967,2.6212967969834,2.48827627384362));
#108806=CARTESIAN_POINT('Ctrl Pts',(6.84860541200244,2.61444752754034,2.50282936134758));
#108807=CARTESIAN_POINT('Ctrl Pts',(6.88764282530724,2.6077598055919,2.51737726108904));
#108808=CARTESIAN_POINT('Ctrl Pts',(6.96573480727117,2.59469807329946,2.5464325162797));
#108809=CARTESIAN_POINT('Ctrl Pts',(7.00483178883872,2.58831697892964,2.56095564735769));
#108810=CARTESIAN_POINT('Ctrl Pts',(7.04393412388175,2.58208164074236,2.57545958120439));
#108811=CARTESIAN_POINT('',(6.66413345302227,2.49144078146678,3.15679042217479));
#108812=CARTESIAN_POINT('Origin',(-1.67834496300756E-12,2.58316965299956,
-6.07586897460877E-13));
#108813=CARTESIAN_POINT('',(7.04375429213915,2.40074633454149,2.57595137240142));
#108814=CARTESIAN_POINT('Origin',(-0.169381858058412,2.55355109385969,-0.0878752584789577));
#108815=CARTESIAN_POINT('',(7.21777269325484,2.49144077881249,2.03807689497822));
#108816=CARTESIAN_POINT('Origin',(-0.181687328975315,2.41071460036769,-0.0647467316436268));
#108817=CARTESIAN_POINT('Origin',(-0.18269865670645,2.55357127027427,-0.061936443737653));
#108818=CARTESIAN_POINT('Ctrl Pts',(6.808012274,2.622074631,2.492683068));
#108819=CARTESIAN_POINT('Ctrl Pts',(6.943469529,2.556767114,2.122722415));
#108820=CARTESIAN_POINT('Ctrl Pts',(7.03803874,2.491440779,1.740261674));
#108821=CARTESIAN_POINT('Ctrl Pts',(6.954415407,2.622074631,2.808221206));
#108822=CARTESIAN_POINT('Ctrl Pts',(7.10701962,2.556767114,2.430304721));
#108823=CARTESIAN_POINT('Ctrl Pts',(7.21777269,2.491440779,2.038076888));
#108824=CARTESIAN_POINT('Ctrl Pts',(6.95587943833001,2.622074631,2.81137658738));
#108825=CARTESIAN_POINT('Ctrl Pts',(7.10865512091,2.556767114,2.43338054406));
#108826=CARTESIAN_POINT('Ctrl Pts',(7.2195700295,2.491440779,2.04105504014));
#108827=CARTESIAN_POINT('',(7.12790571420459,2.49144077849433,1.88916928400112));
#108828=CARTESIAN_POINT('Ctrl Pts',(7.03146877638639,2.48690656567176,1.76683219441741));
#108829=CARTESIAN_POINT('Ctrl Pts',(7.03475375819324,2.48917367233585,1.7535469342087));
#108830=CARTESIAN_POINT('Ctrl Pts',(7.03803874,2.491440779,1.740261674));
#108831=CARTESIAN_POINT('Ctrl Pts',(7.133310028,2.557191576,1.354961564));
#108832=CARTESIAN_POINT('Ctrl Pts',(7.18595121099999,2.622066995,0.961563929));
#108833=CARTESIAN_POINT('Ctrl Pts',(7.33057949286396,2.48690656567176,1.58785340997492));
#108834=CARTESIAN_POINT('Ctrl Pts',(7.33352450100962,2.48917367233585,1.5740048208671));
#108835=CARTESIAN_POINT('Ctrl Pts',(7.33646950915533,2.491440779,1.56015623175923));
#108836=CARTESIAN_POINT('Ctrl Pts',(7.42188085561533,2.557191576,1.15851841490154));
#108837=CARTESIAN_POINT('Ctrl Pts',(7.46293754093156,2.622066995,0.749957057554851));
#108838=CARTESIAN_POINT('',(7.33585395163772,2.49144077985043,1.56052773568837));
#108839=CARTESIAN_POINT('',(7.43289855053669,2.58208164078526,1.00100914581307));
#108840=CARTESIAN_POINT('Origin',(-0.182671872314275,2.4107479441789,-0.0520970523417763));
#108841=CARTESIAN_POINT('Ctrl Pts',(7.18532477592665,2.62129679696926,0.96623385415251));
#108842=CARTESIAN_POINT('Ctrl Pts',(7.22652323753413,2.61444751346219,0.972066893244294));
#108843=CARTESIAN_POINT('Ctrl Pts',(7.26777544245234,2.6077597769625,0.97788279460163));
#108844=CARTESIAN_POINT('Ctrl Pts',(7.35028750978922,2.59469807451361,0.989471259813259));
#108845=CARTESIAN_POINT('Ctrl Pts',(7.39159246099731,2.58831698137499,0.995250151657246));
#108846=CARTESIAN_POINT('Ctrl Pts',(7.43289853829811,2.58208164075722,1.0010091477115));
#108847=CARTESIAN_POINT('',(7.18694634311339,2.49144078146678,1.65039471424761));
#108848=CARTESIAN_POINT('Origin',(9.08995101411847E-13,2.583169653,1.07634170673498E-13));
#108849=CARTESIAN_POINT('',(7.43282863131921,2.40074633450192,1.00152810022529));
#108850=CARTESIAN_POINT('Origin',(-0.184312290055271,2.55355107458263,-0.0494086632345077));
#108851=CARTESIAN_POINT('',(7.48715146569616,2.4914407788124,0.438820016134038));
#108852=CARTESIAN_POINT('Origin',(-0.191357879378022,2.41071461740584,-0.0241755478479756));
#108853=CARTESIAN_POINT('Origin',(-0.191741974367537,2.55357130245492,-0.0212136133590121));
#108854=CARTESIAN_POINT('Ctrl Pts',(7.184697907,2.622074631,0.970884128));
#108855=CARTESIAN_POINT('Ctrl Pts',(7.237457642,2.556767114,0.580453643));
#108856=CARTESIAN_POINT('Ctrl Pts',(7.247598124,2.491440779,0.186605037));
#108857=CARTESIAN_POINT('Ctrl Pts',(7.395509589,2.622074631,1.247572813));
#108858=CARTESIAN_POINT('Ctrl Pts',(7.46330512600001,2.556767114,0.845686411));
#108859=CARTESIAN_POINT('Ctrl Pts',(7.487151461,2.491440779,0.43882001));
#108860=CARTESIAN_POINT('Ctrl Pts',(7.39761770582,2.622074631,1.25033969985));
#108861=CARTESIAN_POINT('Ctrl Pts',(7.46556360084,2.556767114,0.84833873868));
#108862=CARTESIAN_POINT('Ctrl Pts',(7.48954699437,2.491440779,0.44134215973));
#108863=CARTESIAN_POINT('',(7.36737479236834,2.49144077849433,0.312712526601943));
#108864=CARTESIAN_POINT('Ctrl Pts',(7.24689363902624,2.48690656569715,0.213966701214266));
#108865=CARTESIAN_POINT('Ctrl Pts',(7.24724588151317,2.48917367234855,0.200285869107131));
#108866=CARTESIAN_POINT('Ctrl Pts',(7.247598124,2.491440779,0.186605037));
#108867=CARTESIAN_POINT('Ctrl Pts',(7.257813887,2.557191576,-0.210167481));
#108868=CARTESIAN_POINT('Ctrl Pts',(7.224655486,2.622066995,-0.605683996));
#108869=CARTESIAN_POINT('Ctrl Pts',(7.500536164337,2.48690656569716,-0.0251276215615274));
#108870=CARTESIAN_POINT('Ctrl Pts',(7.50043528254417,2.48917367234855,-0.0392855279489237));
#108871=CARTESIAN_POINT('Ctrl Pts',(7.50033440075132,2.491440779,-0.0534434343363214));
#108872=CARTESIAN_POINT('Ctrl Pts',(7.49740861943488,2.557191576,-0.464052096364095));
#108873=CARTESIAN_POINT('Ctrl Pts',(7.44967680768896,2.622066995,-0.871887489814411));
#108874=CARTESIAN_POINT('',(7.49981309758335,2.4914407798504,-0.05294829189469));
#108875=CARTESIAN_POINT('',(7.47430888983564,2.58208164080481,-0.620247365094564));
#108876=CARTESIAN_POINT('Origin',(-0.189600407854941,2.41074793233023,-0.011610007931523));
#108877=CARTESIAN_POINT('Ctrl Pts',(7.22504759239769,2.62129679701665,-0.600988586287213));
#108878=CARTESIAN_POINT('Ctrl Pts',(7.26653670335673,2.61444752746288,-0.604148365421792));
#108879=CARTESIAN_POINT('Ctrl Pts',(7.30807460570636,2.60775980536993,-0.607336433764565));
#108880=CARTESIAN_POINT('Ctrl Pts',(7.39114895381358,2.59469807312342,-0.613756570528413));
#108881=CARTESIAN_POINT('Ctrl Pts',(7.43273051931852,2.58831697852743,-0.616992130316176));
#108882=CARTESIAN_POINT('Ctrl Pts',(7.47430887837775,2.58208164076432,-0.620247360527366));
#108883=CARTESIAN_POINT('',(7.37370560986287,2.49144078146676,0.0668283836306943));
#108884=CARTESIAN_POINT('Origin',(-5.95010152260045E-13,2.58316965300044,
1.45659173741639E-13));
#108885=CARTESIAN_POINT('',(7.47435216511153,2.40074633456696,-0.619725513626632));
#108886=CARTESIAN_POINT('Origin',(-0.190624814482888,2.55355107517748,-0.00863181457063135));
#108887=CARTESIAN_POINT('',(7.40643935690458,2.49144077881248,-1.18095559800117));
#108888=CARTESIAN_POINT('Origin',(-0.192081249505737,2.41071462784453,0.0175259825687855));
#108889=CARTESIAN_POINT('Origin',(-0.191819194414465,2.55357127695176,0.0205011828761191));
#108890=CARTESIAN_POINT('Ctrl Pts',(7.225435051,2.622074631,-0.596312275));
#108891=CARTESIAN_POINT('Ctrl Pts',(7.19303028,2.556767114,-0.988956496));
#108892=CARTESIAN_POINT('Ctrl Pts',(7.118267874,2.491440779,-1.375777044));
#108893=CARTESIAN_POINT('Ctrl Pts',(7.490797961,2.622074631,-0.371410698));
#108894=CARTESIAN_POINT('Ctrl Pts',(7.47061478,2.556767114,-0.778475256));
#108895=CARTESIAN_POINT('Ctrl Pts',(7.406439351,2.491440779,-1.180955603));
#108896=CARTESIAN_POINT('Ctrl Pts',(7.49345159010001,2.622074631,-0.36916168223));
#108897=CARTESIAN_POINT('Ctrl Pts',(7.473390625,2.556767114,-0.7763704436));
#108898=CARTESIAN_POINT('Ctrl Pts',(7.40932106577,2.491440779,-1.17900738859));
#108899=CARTESIAN_POINT('',(7.26235361303824,2.49144077849433,-1.27836632044227));
#108900=CARTESIAN_POINT('Ctrl Pts',(7.1234618085242,2.48690656562793,-1.34890363637193));
#108901=CARTESIAN_POINT('Ctrl Pts',(7.12086484126211,2.48917367231394,-1.36234034018596));
#108902=CARTESIAN_POINT('Ctrl Pts',(7.118267874,2.491440779,-1.375777044));
#108903=CARTESIAN_POINT('Ctrl Pts',(7.042950436,2.557191576,-1.765469329));
#108904=CARTESIAN_POINT('Ctrl Pts',(6.925542901,2.622066995,-2.144610811));
#108905=CARTESIAN_POINT('Ctrl Pts',(7.31977610096884,2.48690656562794,-1.63693371243211));
#108906=CARTESIAN_POINT('Ctrl Pts',(7.31663404633257,2.48917367231394,-1.65073892846223));
#108907=CARTESIAN_POINT('Ctrl Pts',(7.31349199169623,2.491440779,-1.66454414449235));
#108908=CARTESIAN_POINT('Ctrl Pts',(7.22236588906184,2.557191576,-2.06492404823634));
#108909=CARTESIAN_POINT('Ctrl Pts',(7.08807746581271,2.622066995,-2.45296354767138));
#108910=CARTESIAN_POINT('',(7.31308931728985,2.49144077985038,-1.66394851343346));
#108911=CARTESIAN_POINT('',(7.16622885233626,2.58208164074841,-2.21250179872927));
#108912=CARTESIAN_POINT('Origin',(-0.187663248092902,2.41074796270394,0.029419856961789));
#108913=CARTESIAN_POINT('Ctrl Pts',(6.92693521466089,2.62129679693166,-2.14010946824839));
#108914=CARTESIAN_POINT('Ctrl Pts',(6.96677515560324,2.6144475133313,-2.15211433059853));
#108915=CARTESIAN_POINT('Ctrl Pts',(7.00665667656492,2.60775977678319,-2.16415731290675));
#108916=CARTESIAN_POINT('Ctrl Pts',(7.08640817575413,2.59469812265093,-2.1882857354475));
#108917=CARTESIAN_POINT('Ctrl Pts',(7.12632169586457,2.58831707916653,-2.20038435307007));
#108918=CARTESIAN_POINT('Ctrl Pts',(7.16622884238419,2.58208164067141,-2.21250179179743));
#108919=CARTESIAN_POINT('',(7.21567859711874,2.49144078146676,-1.51986276769353));
#108920=CARTESIAN_POINT('Origin',(8.62157567560473E-13,2.58316965299989,
-2.5576329248933E-13));
#108921=CARTESIAN_POINT('',(7.16638329838829,2.40074633454233,-2.21200145070765));
#108922=CARTESIAN_POINT('Origin',(-0.188023568116957,2.55355108735271,0.0325486569326483));
#108923=CARTESIAN_POINT('',(6.97941037431554,2.49144077881229,-2.74551104348949));
#108924=CARTESIAN_POINT('Origin',(-0.183822865911698,2.41071459369151,0.0584079944944987));
#108925=CARTESIAN_POINT('Origin',(-0.182927537906269,2.55357125929785,0.0612573726347116));
#108926=CARTESIAN_POINT('Ctrl Pts',(6.928318882,2.622074631,-2.135625779));
#108927=CARTESIAN_POINT('Ctrl Pts',(6.812264815,2.556767114,-2.512124128));
#108928=CARTESIAN_POINT('Ctrl Pts',(6.65609533,2.491440779,-2.873829319));
#108929=CARTESIAN_POINT('Ctrl Pts',(7.235824946,2.622074631,-1.973027457));
#108930=CARTESIAN_POINT('Ctrl Pts',(7.128606789,2.556767114,-2.366236285));
#108931=CARTESIAN_POINT('Ctrl Pts',(6.979410369,2.491440779,-2.745511045));
#108932=CARTESIAN_POINT('Ctrl Pts',(7.23890000664,2.622074631,-1.97140147378));
#108933=CARTESIAN_POINT('Ctrl Pts',(7.13177020874,2.556767114,-2.36477740657));
#108934=CARTESIAN_POINT('Ctrl Pts',(6.98264351939001,2.491440779,-2.74422786226));
#108935=CARTESIAN_POINT('',(6.81775285068297,2.49144077849433,-2.80967017912947));
#108936=CARTESIAN_POINT('Ctrl Pts',(6.66694482167319,2.48690656554502,-2.848700738649));
#108937=CARTESIAN_POINT('Ctrl Pts',(6.66152007583659,2.48917367227249,-2.86126502882453));
#108938=CARTESIAN_POINT('Ctrl Pts',(6.65609533,2.491440779,-2.873829319));
#108939=CARTESIAN_POINT('Ctrl Pts',(6.49876645,2.557191576,-3.238219792));
#108940=CARTESIAN_POINT('Ctrl Pts',(6.302599626,2.622066995,-3.583258008));
#108941=CARTESIAN_POINT('Ctrl Pts',(6.79675144311513,2.48690656554502,-3.17219860169431));
#108942=CARTESIAN_POINT('Ctrl Pts',(6.79071513448913,2.48917367227249,-3.18500561081046));
#108943=CARTESIAN_POINT('Ctrl Pts',(6.78467882586311,2.491440779,-3.19781261992669));
#108944=CARTESIAN_POINT('Ctrl Pts',(6.60961335660931,2.557191576,-3.56924244559905));
#108945=CARTESIAN_POINT('Ctrl Pts',(6.39504749997121,2.622066995,-3.91934175583024));
#108946=CARTESIAN_POINT('',(6.78441360938226,2.49144077985043,-3.19714434868294));
#108947=CARTESIAN_POINT('',(6.52306391845758,2.58208164080626,-3.70130210716894));
#108948=CARTESIAN_POINT('Origin',(-0.176951405087596,2.41074795767547,0.0690740987240757));
#108949=CARTESIAN_POINT('Ctrl Pts',(6.30492704362086,2.6212967969752,-3.57916121053907));
#108950=CARTESIAN_POINT('Ctrl Pts',(6.34125478323769,2.6144475275756,-3.59944977361168));
#108951=CARTESIAN_POINT('Ctrl Pts',(6.3776149261663,2.60775980566249,-3.61978449806117));
#108952=CARTESIAN_POINT('Ctrl Pts',(6.45031541722462,2.59469807337158,-3.66049326997677));
#108953=CARTESIAN_POINT('Ctrl Pts',(6.48669524604243,2.58831697904106,-3.68088942978343));
#108954=CARTESIAN_POINT('Ctrl Pts',(6.52306390997007,2.58208164076785,-3.70130209819832));
#108955=CARTESIAN_POINT('',(6.72025447322876,2.49144078146676,-3.03548682471018));
#108956=CARTESIAN_POINT('Origin',(4.43655528981068E-13,2.583169653,-2.21610924056037E-13));
#108957=CARTESIAN_POINT('',(6.52332231405131,2.40074633455023,-3.70084665820525));
#108958=CARTESIAN_POINT('Origin',(-0.176630612761898,2.55355109588944,0.0722071555427695));
#108959=CARTESIAN_POINT('',(6.22603192246307,2.49144077881206,-4.18168943993897));
#108960=CARTESIAN_POINT('Origin',(-0.166969114515872,2.41071458448309,0.0965588810765111));
#108961=CARTESIAN_POINT('Origin',(-0.165482309762637,2.55357128393338,0.0991492473481255));
#108962=CARTESIAN_POINT('Ctrl Pts',(6.307242223,2.622074631,-3.575079795));
#108963=CARTESIAN_POINT('Ctrl Pts',(6.11296542,2.556767114,-3.917827629));
#108964=CARTESIAN_POINT('Ctrl Pts',(5.882691166,2.491440779,-4.23750453));
#108965=CARTESIAN_POINT('Ctrl Pts',(6.642512799,2.622074631,-3.482387646));
#108966=CARTESIAN_POINT('Ctrl Pts',(6.453273068,2.556767114,-3.843354735));
#108967=CARTESIAN_POINT('Ctrl Pts',(6.226031915,2.491440779,-4.181689442));
#108968=CARTESIAN_POINT('Ctrl Pts',(6.64586550476001,2.622074631,-3.48146072451));
#108969=CARTESIAN_POINT('Ctrl Pts',(6.45667614448,2.556767114,-3.84261000606));
#108970=CARTESIAN_POINT('Ctrl Pts',(6.22946532249,2.491440779,-4.18113129112));
#108971=CARTESIAN_POINT('',(6.05436154227657,2.49144077849314,-4.2095969834449));
#108972=CARTESIAN_POINT('Ctrl Pts',(5.89868890436543,2.48690656560986,-4.2152957621876));
#108973=CARTESIAN_POINT('Ctrl Pts',(5.89069003518275,2.48917367230491,-4.2264001460938));
#108974=CARTESIAN_POINT('Ctrl Pts',(5.882691166,2.491440779,-4.23750453));
#108975=CARTESIAN_POINT('Ctrl Pts',(5.650707367,2.557191576,-4.559554698));
#108976=CARTESIAN_POINT('Ctrl Pts',(5.384953798,2.622066995,-4.854356043));
#108977=CARTESIAN_POINT('Ctrl Pts',(5.95591824127479,2.48690656560986,-4.55913501163647));
#108978=CARTESIAN_POINT('Ctrl Pts',(5.94726992991814,2.48917367230491,-4.57034497191049));
#108979=CARTESIAN_POINT('Ctrl Pts',(5.9386216185615,2.491440779,-4.58155493218466));
#108980=CARTESIAN_POINT('Ctrl Pts',(5.68780264932776,2.557191576,-4.90666703386099));
#108981=CARTESIAN_POINT('Ctrl Pts',(5.4029922208282,2.622066995,-5.20245589976416));
#108982=CARTESIAN_POINT('',(5.93850626126276,2.49144077985043,-4.58084527104709));
#108983=CARTESIAN_POINT('',(5.57488776576028,2.58208164079198,-5.01703364292958));
#108984=CARTESIAN_POINT('Origin',(-0.157965533946155,2.41074797302503,0.105498548043241));
#108985=CARTESIAN_POINT('Ctrl Pts',(5.38810749188006,2.62129679706164,-4.85085535278));
#108986=CARTESIAN_POINT('Ctrl Pts',(5.41922446827193,2.61444752753297,-4.87847897090086));
#108987=CARTESIAN_POINT('Ctrl Pts',(5.4503631671097,2.60775980550092,-4.90615463707291));
#108988=CARTESIAN_POINT('Ctrl Pts',(5.51261277153886,2.59469807464639,-4.96154011084877));
#108989=CARTESIAN_POINT('Ctrl Pts',(5.54375748182496,2.58831698163702,-4.98928000146014));
#108990=CARTESIAN_POINT('Ctrl Pts',(5.57488775926951,2.58208164076488,-5.01703363236939));
#108991=CARTESIAN_POINT('',(5.91059871904757,2.49144078146676,-4.40917489237154));
#108992=CARTESIAN_POINT('Origin',(8.06646416329215E-14,2.58316965300056,
-3.07913416985883E-14));
#108993=CARTESIAN_POINT('',(5.57523802806608,2.40074633456092,-5.01664438946));
#108994=CARTESIAN_POINT('Origin',(-0.156978674655573,2.55355110431272,0.108489348300177));
#108995=CARTESIAN_POINT('',(5.18153113441456,2.49144077881227,-5.42233668988284));
#108996=CARTESIAN_POINT('Origin',(-0.142308321068101,2.41071463315435,0.130194957196538));
#108997=CARTESIAN_POINT('Origin',(-0.140299164977355,2.55357126531762,0.132404891235678));
#108998=CARTESIAN_POINT('Ctrl Pts',(5.391245927,2.622074631,-4.847367054));
#108999=CARTESIAN_POINT('Ctrl Pts',(5.127830556,2.556767114,-5.14033786300001));
#109000=CARTESIAN_POINT('Ctrl Pts',(4.834218902,2.491440779,-5.403038739));
#109001=CARTESIAN_POINT('Ctrl Pts',(5.738604136,2.622074631,-4.828915258));
#109002=CARTESIAN_POINT('Ctrl Pts',(5.476191471,2.556767114,-5.14076219));
#109003=CARTESIAN_POINT('Ctrl Pts',(5.181531129,2.491440779,-5.422336689));
#109004=CARTESIAN_POINT('Ctrl Pts',(5.74207771809,2.622074631,-4.82873074004));
#109005=CARTESIAN_POINT('Ctrl Pts',(5.47967508015,2.556767114,-5.14076643327));
#109006=CARTESIAN_POINT('Ctrl Pts',(5.18500425127001,2.491440779,-5.4225296685));
#109007=CARTESIAN_POINT('',(5.00787501777898,2.49144077849432,-5.41268771189147));
#109008=CARTESIAN_POINT('Ctrl Pts',(4.85461685026215,2.48690656571168,-5.38478824115059));
#109009=CARTESIAN_POINT('Ctrl Pts',(4.84441787613114,2.48917367235581,-5.3939134900753));
#109010=CARTESIAN_POINT('Ctrl Pts',(4.834218902,2.491440779,-5.403038739));
#109011=CARTESIAN_POINT('Ctrl Pts',(4.538427489,2.557191576,-5.667689893));
#109012=CARTESIAN_POINT('Ctrl Pts',(4.215513515,2.622066995,-5.898469785));
#109013=CARTESIAN_POINT('Ctrl Pts',(4.83659292192365,2.48690656571168,-5.73289133567628));
#109014=CARTESIAN_POINT('Ctrl Pts',(4.82573699343333,2.48917367235581,-5.74198008177738));
#109015=CARTESIAN_POINT('Ctrl Pts',(4.81488106494289,2.491440779,-5.75106882787834));
#109016=CARTESIAN_POINT('Ctrl Pts',(4.50003661232125,2.557191576,-6.01466132424542));
#109017=CARTESIAN_POINT('Ctrl Pts',(4.15829902993438,2.622066995,-6.24230898857749));
#109018=CARTESIAN_POINT('',(4.81492095921965,2.49144077985039,-5.75035096193016));
#109019=CARTESIAN_POINT('',(4.36603605687917,2.58208164081465,-6.09817426156109));
#109020=CARTESIAN_POINT('Origin',(-0.131593410693618,2.41074792150729,0.136990085206607));
#109021=CARTESIAN_POINT('Ctrl Pts',(4.21934602251979,2.62129679699324,-5.89572888979408));
#109022=CARTESIAN_POINT('Ctrl Pts',(4.2437972900956,2.61444751343298,-5.92939598223856));
#109023=CARTESIAN_POINT('Ctrl Pts',(4.26825859004058,2.60775977690531,-5.96311858498214));
#109024=CARTESIAN_POINT('Ctrl Pts',(4.31714649608614,2.59469807212449,-6.03059086746435));
#109025=CARTESIAN_POINT('Ctrl Pts',(4.34159981442992,2.58831697653239,-6.06437742162148));
#109026=CARTESIAN_POINT('Ctrl Pts',(4.36603605302416,2.58208164076558,-6.09817424988061));
#109027=CARTESIAN_POINT('',(4.82456993844327,2.49144078146676,-5.57669484260008));
#109028=CARTESIAN_POINT('Origin',(2.52185425320128E-13,2.58316965299956,
-3.40873163029443E-13));
#109029=CARTESIAN_POINT('',(4.3664618082785,2.40074633452804,-6.09786940478252));
#109030=CARTESIAN_POINT('Origin',(-0.12998675156063,2.55355109067572,0.139698914534188));
#109031=CARTESIAN_POINT('',(3.89474771260811,2.49144077881251,-6.40944149926319));
#109032=CARTESIAN_POINT('Origin',(-0.110993050041865,2.41071459137445,0.157742983199087));
#109033=CARTESIAN_POINT('Origin',(-0.108555880427218,2.55357126078289,0.159469471285793));
#109034=CARTESIAN_POINT('Ctrl Pts',(4.223160964,2.622074631,-5.892996816));
#109035=CARTESIAN_POINT('Ctrl Pts',(3.902924033,2.556767114,-6.122491612));
#109036=CARTESIAN_POINT('Ctrl Pts',(3.559703934,2.491440779,-6.315932861));
#109037=CARTESIAN_POINT('Ctrl Pts',(4.566364721,2.622074631,-5.94964816));
#109038=CARTESIAN_POINT('Ctrl Pts',(4.243049246,2.556767114,-6.197793318));
#109039=CARTESIAN_POINT('Ctrl Pts',(3.894747705,2.491440779,-6.409441498));
#109040=CARTESIAN_POINT('Ctrl Pts',(4.56979675856999,2.622074631,-5.95021467344));
#109041=CARTESIAN_POINT('Ctrl Pts',(4.24645049813,2.556767114,-6.19854633505999));
#109042=CARTESIAN_POINT('Ctrl Pts',(3.89809814271,2.491440779,-6.41037658437));
#109043=CARTESIAN_POINT('',(3.72722582217897,2.49144077849432,-6.36268717793067));
#109044=CARTESIAN_POINT('Ctrl Pts',(3.58354830709371,2.4869065657146,-6.30249400556225));
#109045=CARTESIAN_POINT('Ctrl Pts',(3.57162612054686,2.48917367235727,-6.30921343328113));
#109046=CARTESIAN_POINT('Ctrl Pts',(3.559703934,2.491440779,-6.315932861));
#109047=CARTESIAN_POINT('Ctrl Pts',(3.213935785,2.557191576,-6.510810208));
#109048=CARTESIAN_POINT('Ctrl Pts',(2.848960505,2.622066995,-6.666777635));
#109049=CARTESIAN_POINT('Ctrl Pts',(3.49111389272047,2.4869065657146,-6.63858403102125));
#109050=CARTESIAN_POINT('Ctrl Pts',(3.47855795805834,2.48917367235727,-6.64512658357427));
#109051=CARTESIAN_POINT('Ctrl Pts',(3.46600202339621,2.491440779,-6.65166913612718));
#109052=CARTESIAN_POINT('Ctrl Pts',(3.1018538639937,2.557191576,-6.84141673629003));
#109053=CARTESIAN_POINT('Ctrl Pts',(2.71916839820034,2.622066995,-6.99027864614378));
#109054=CARTESIAN_POINT('',(3.46619530490013,2.49144077985039,-6.65097662960528));
#109055=CARTESIAN_POINT('',(2.9530333546921,2.58208164077412,-6.89417102909293));
#109056=CARTESIAN_POINT('Origin',(-0.0990679971332942,2.41074794347386,
0.162075993420773));
#109057=CARTESIAN_POINT('Ctrl Pts',(2.85329262184866,2.62129679704082,-6.66492469624666));
#109058=CARTESIAN_POINT('Ctrl Pts',(2.86993476900124,2.6144475273861,-6.70306089312993));
#109059=CARTESIAN_POINT('Ctrl Pts',(2.88657477658767,2.60775980518931,-6.74125344879505));
#109060=CARTESIAN_POINT('Ctrl Pts',(2.91981523095929,2.59469807424988,-6.8176578743698));
#109061=CARTESIAN_POINT('Ctrl Pts',(2.93643372789784,2.58831698082537,-6.8559112442663));
#109062=CARTESIAN_POINT('Ctrl Pts',(2.95303335326477,2.58208164074392,-6.89417101679466));
#109063=CARTESIAN_POINT('',(3.51294962880404,2.49144078146678,-6.48345473929143));
#109064=CARTESIAN_POINT('Origin',(-5.87637577487143E-14,2.583169653,3.06178693509906E-13));
#109065=CARTESIAN_POINT('',(2.95351468760116,2.40074633455062,-6.8939648237853));
#109066=CARTESIAN_POINT('Origin',(-0.096916549270849,2.55355105557019,0.16437603281196));
#109067=CARTESIAN_POINT('',(2.42585021516617,2.49144077881249,-7.09684794887307));
#109068=CARTESIAN_POINT('Origin',(-0.0744880397869285,2.4107146057847,0.177915339574071));
#109069=CARTESIAN_POINT('Origin',(-0.0717367755555178,2.55357127143605,
0.179077716464044));
#109070=CARTESIAN_POINT('Ctrl Pts',(2.857605688,2.622074631,-6.663076597));
#109071=CARTESIAN_POINT('Ctrl Pts',(2.495521121,2.556767114,-6.818364458));
#109072=CARTESIAN_POINT('Ctrl Pts',(2.118741167,2.491440779,-6.933500982));
#109073=CARTESIAN_POINT('Ctrl Pts',(3.180607168,2.622074631,-6.792182127));
#109074=CARTESIAN_POINT('Ctrl Pts',(2.811506755,2.556767114,-6.96502251800001));
#109075=CARTESIAN_POINT('Ctrl Pts',(2.425850208,2.491440779,-7.096847946));
#109076=CARTESIAN_POINT('Ctrl Pts',(3.1838371828,2.622074631,-6.79347318230001));
#109077=CARTESIAN_POINT('Ctrl Pts',(2.81466661134,2.556767114,-6.96648909860001));
#109078=CARTESIAN_POINT('Ctrl Pts',(2.42892129841,2.491440779,-7.09848141564));
#109079=CARTESIAN_POINT('',(2.27229569045365,2.49144077849433,-7.01517446304328));
#109080=CARTESIAN_POINT('Ctrl Pts',(2.14491702998573,2.48690656547073,-6.92550215446538));
#109081=CARTESIAN_POINT('Ctrl Pts',(2.1318290984929,2.48917367223534,-6.92950156823269));
#109082=CARTESIAN_POINT('Ctrl Pts',(2.118741167,2.491440779,-6.933500982));
#109083=CARTESIAN_POINT('Ctrl Pts',(1.739164016,2.557191576,-7.049492274));
#109084=CARTESIAN_POINT('Ctrl Pts',(1.349193269,2.622066995,-7.123354373));
#109085=CARTESIAN_POINT('Ctrl Pts',(1.98239426019606,2.48690656547073,-7.23386391516343));
#109086=CARTESIAN_POINT('Ctrl Pts',(1.96872542015212,2.48917367223534,-7.23755435190902));
#109087=CARTESIAN_POINT('Ctrl Pts',(1.95505658010818,2.491440779,-7.24124478865457));
#109088=CARTESIAN_POINT('Ctrl Pts',(1.55863187661946,2.557191576,-7.34827510636233));
#109089=CARTESIAN_POINT('Ctrl Pts',(1.15289247451102,2.622066995,-7.41139064303918));
#109090=CARTESIAN_POINT('',(1.95539421362746,2.49144077968687,-7.24061002108648));
#109091=CARTESIAN_POINT('',(1.40195009493992,2.58208164075595,-7.36780402184064));
#109092=CARTESIAN_POINT('Origin',(-0.0619102066622512,2.41074799745518,
0.179583077257681));
#109093=CARTESIAN_POINT('Ctrl Pts',(1.35382243093522,2.62129679694517,-7.12247603196643));
#109094=CARTESIAN_POINT('Ctrl Pts',(1.36187735507601,2.61444751336702,-7.1632982784614));
#109095=CARTESIAN_POINT('Ctrl Pts',(1.36991807621742,2.60775977682948,-7.20417511712516));
#109096=CARTESIAN_POINT('Ctrl Pts',(1.3859566607698,2.59469807297325,-7.28593879530451));
#109097=CARTESIAN_POINT('Ctrl Pts',(1.39396328432408,2.58831697829252,-7.32687031691883));
#109098=CARTESIAN_POINT('Ctrl Pts',(1.401950096276,2.58208164071552,-7.36780400958062));
#109099=CARTESIAN_POINT('',(2.03706769954258,2.49144078146677,-7.08705549831995));
#109100=CARTESIAN_POINT('Origin',(9.30245463992563E-14,2.58316965299978,
-5.59014640133526E-13));
#109101=CARTESIAN_POINT('',(1.40246450238646,2.40074633473875,-7.36770610983971));
#109102=CARTESIAN_POINT('Origin',(-0.0593146844469267,2.55355108193507,
0.181367093158652));
#109103=CARTESIAN_POINT('',(0.843522657377911,2.49144077881244,-7.45241367635275));
#109104=CARTESIAN_POINT('Origin',(-0.0345000262588741,2.41071456861255,
0.189768554694382));
#109105=CARTESIAN_POINT('Origin',(-0.0315631804266333,2.55357129110865,
0.190312136075104));
#109106=CARTESIAN_POINT('Ctrl Pts',(1.358431946,2.622074631,-7.121598321));
#109107=CARTESIAN_POINT('Ctrl Pts',(0.971430415,2.556767114,-7.19541816));
#109108=CARTESIAN_POINT('Ctrl Pts',(0.578708417,2.491440779,-7.226866303));
#109109=CARTESIAN_POINT('Ctrl Pts',(1.646127958,2.622074631,-7.317121206));
#109110=CARTESIAN_POINT('Ctrl Pts',(1.248501333,2.556767114,-7.406575007));
#109111=CARTESIAN_POINT('Ctrl Pts',(0.843522651,2.491440779,-7.452413672));
#109112=CARTESIAN_POINT('Ctrl Pts',(1.64900491812,2.622074631,-7.31907643485));
#109113=CARTESIAN_POINT('Ctrl Pts',(1.25127204218,2.556767114,-7.40868657547001));
#109114=CARTESIAN_POINT('Ctrl Pts',(0.84617079334,2.491440779,-7.45466914569));
#109115=CARTESIAN_POINT('',(0.711115537090266,2.49144077849433,-7.33963998720059));
#109116=CARTESIAN_POINT('Ctrl Pts',(0.589268654989089,2.48968577857207,
-7.22602066694827));
#109117=CARTESIAN_POINT('Ctrl Pts',(0.583988535994544,2.49056327878603,
-7.22644348497414));
#109118=CARTESIAN_POINT('Ctrl Pts',(0.578708417,2.491440779,-7.226866303));
#109119=CARTESIAN_POINT('Ctrl Pts',(0.18307087,2.557191576,-7.258547916));
#109120=CARTESIAN_POINT('Ctrl Pts',(-0.213660746,2.622066995,-7.246850977));
#109121=CARTESIAN_POINT('Ctrl Pts',(0.363928115288176,2.48968577857207,
-7.49137659932231));
#109122=CARTESIAN_POINT('Ctrl Pts',(0.358454361982624,2.49056327878603,
-7.49163449528042));
#109123=CARTESIAN_POINT('Ctrl Pts',(0.352980608677072,2.491440779,-7.49189239123853));
#109124=CARTESIAN_POINT('Ctrl Pts',(-0.057165892363825,2.557191576,-7.51121644896398));
#109125=CARTESIAN_POINT('Ctrl Pts',(-0.466970758744476,2.622066995,-7.48565195764118));
#109126=CARTESIAN_POINT('Ctrl Pts',(-0.208950993496339,2.62129679688656,
-7.24698830400573));
#109127=CARTESIAN_POINT('Ctrl Pts',(-0.209859963272608,2.61444752746582,
-7.28858763389194));
#109128=CARTESIAN_POINT('Ctrl Pts',(-0.210794539299999,2.60775980554242,
-7.3302372148635));
#109129=CARTESIAN_POINT('Ctrl Pts',(-0.212707705721166,2.59469807423041,
-7.41353730072241));
#109130=CARTESIAN_POINT('Ctrl Pts',(-0.213687339137458,2.58831698335809,
-7.45523302806801));
#109131=CARTESIAN_POINT('Ctrl Pts',(-0.214686788682326,2.58208164328187,
-7.49692665879079));
#109132=CARTESIAN_POINT('',(0.465934748101219,2.49144078146678,-7.3592734190439));
#109133=CARTESIAN_POINT('Ctrl Pts',(-0.204260564,2.622074631,-7.247122023));
#109134=CARTESIAN_POINT('Ctrl Pts',(-0.598083297,2.556767114,-7.23602210600001));
#109135=CARTESIAN_POINT('Ctrl Pts',(-0.988384095,2.491440779,-7.182311389));
#109136=CARTESIAN_POINT('Ctrl Pts',(0.034677634,2.622074631,-7.49991983));
#109137=CARTESIAN_POINT('Ctrl Pts',(-0.372882624,2.556767114,-7.501804281));
#109138=CARTESIAN_POINT('Ctrl Pts',(-0.778247087,2.491440779,-7.459512817));
#109139=CARTESIAN_POINT('Ctrl Pts',(0.03706701598,2.622074631,-7.50244780807));
#109140=CARTESIAN_POINT('Ctrl Pts',(-0.37063061727,2.556767114,-7.50446210275));
#109141=CARTESIAN_POINT('Ctrl Pts',(-0.77614571692,2.491440779,-7.46228483128));
#109142=CARTESIAN_POINT('',(-0.88331558791762,2.49144077849433,-7.32091210337191));
#109143=CARTESIAN_POINT('Ctrl Pts',(-0.961268905873276,2.48690656566808,
-7.18604280921463));
#109144=CARTESIAN_POINT('Ctrl Pts',(-0.974826500436638,2.48917367233402,
-7.18417709910731));
#109145=CARTESIAN_POINT('Ctrl Pts',(-0.988384095,2.491440779,-7.182311389));
#109146=CARTESIAN_POINT('Ctrl Pts',(-1.381582466,2.557191576,-7.128201925));
#109147=CARTESIAN_POINT('Ctrl Pts',(-1.766524221,2.622066995,-7.031492884));
#109148=CARTESIAN_POINT('Ctrl Pts',(-1.23824831884656,2.48690656566808,
-7.39766282396809));
#109149=CARTESIAN_POINT('Ctrl Pts',(-1.2522033956195,2.48917367233402,-7.39527277674135));
#109150=CARTESIAN_POINT('Ctrl Pts',(-1.26615847239241,2.491440779,-7.39288272951463));
#109151=CARTESIAN_POINT('Ctrl Pts',(-1.67088465214717,2.557191576,-7.32356640118142));
#109152=CARTESIAN_POINT('Ctrl Pts',(-2.06562528673817,2.622066995,-7.21048295863567));
#109153=CARTESIAN_POINT('',(-1.26558551255393,2.49144077985043,-7.39244839868839));
#109154=CARTESIAN_POINT('',(-1.82128516547444,2.58208164082782,-7.27550139284704));
#109155=CARTESIAN_POINT('Origin',(0.0192168786179955,2.41074796101253,0.188980975291886));
#109156=CARTESIAN_POINT('Ctrl Pts',(-1.76195410109266,2.62129679686244,
-7.03263945803568));
#109157=CARTESIAN_POINT('Ctrl Pts',(-1.77178446640157,2.6144475132992,-7.07307090047985));
#109158=CARTESIAN_POINT('Ctrl Pts',(-1.78165064464794,2.60775977678226,
-7.11354592569115));
#109159=CARTESIAN_POINT('Ctrl Pts',(-1.80142609344871,2.59469807529347,
-7.19448704266161));
#109160=CARTESIAN_POINT('Ctrl Pts',(-1.81134617464545,2.58831698297699,
-7.23499736360396));
#109161=CARTESIAN_POINT('Ctrl Pts',(-1.82128515921039,2.58208164080564,
-7.27550138211921));
#109162=CARTESIAN_POINT('',(-1.12698479404631,2.49144078146678,-7.28737989481257));
#109163=CARTESIAN_POINT('Origin',(2.65629532258949E-13,2.58316965300011,
9.47592698752331E-13));
#109164=CARTESIAN_POINT('',(-1.82077718939072,2.40074633449375,-7.2756285243275));
#109165=CARTESIAN_POINT('Origin',(0.0223215638672389,2.55355104571884,0.189510060974852));
#109166=CARTESIAN_POINT('',(-2.36362685302965,2.49144077881259,-7.11781344061047));
#109167=CARTESIAN_POINT('Origin',(0.0483703533929128,2.41071457610894,0.186715408605023));
#109168=CARTESIAN_POINT('Origin',(0.051264056983934,2.55357123384883,0.18597571480012));
#109169=CARTESIAN_POINT('Ctrl Pts',(-1.757402077,2.622074631,-7.033778354));
#109170=CARTESIAN_POINT('Ctrl Pts',(-2.1396313,2.556767114,-6.938277701));
#109171=CARTESIAN_POINT('Ctrl Pts',(-2.509260865,2.491440779,-6.801919576));
#109172=CARTESIAN_POINT('Ctrl Pts',(-1.578394177,2.622074631,-7.332030539));
#109173=CARTESIAN_POINT('Ctrl Pts',(-1.976831005,2.556767114,-7.246257523));
#109174=CARTESIAN_POINT('Ctrl Pts',(-2.363626857,2.491440779,-7.117813434));
#109175=CARTESIAN_POINT('Ctrl Pts',(-1.576604098,2.622074631,-7.33501306085001));
#109176=CARTESIAN_POINT('Ctrl Pts',(-1.97520300205,2.556767114,-7.24933732122));
#109177=CARTESIAN_POINT('Ctrl Pts',(-2.36217051692,2.491440779,-7.12097237258));
#109178=CARTESIAN_POINT('',(-2.43644385806959,2.49144077849432,-6.95986650602585));
#109179=CARTESIAN_POINT('Ctrl Pts',(-2.48358175836414,2.48690656555699,
-6.81139272207903));
#109180=CARTESIAN_POINT('Ctrl Pts',(-2.49642131168206,2.48917367227847,
-6.80665614903953));
#109181=CARTESIAN_POINT('Ctrl Pts',(-2.509260865,2.491440779,-6.801919576));
#109182=CARTESIAN_POINT('Ctrl Pts',(-2.881634541,2.557191576,-6.664549134));
#109183=CARTESIAN_POINT('Ctrl Pts',(-3.236786987,2.622066995,-6.487349998));
#109184=CARTESIAN_POINT('Ctrl Pts',(-2.79957759473554,2.48690656555699,
-6.95852279157715));
#109185=CARTESIAN_POINT('Ctrl Pts',(-2.8126926203869,2.48917367227847,-6.95318869321943));
#109186=CARTESIAN_POINT('Ctrl Pts',(-2.82580764603826,2.491440779,-6.94785459486179));
#109187=CARTESIAN_POINT('Ctrl Pts',(-3.20617059104897,2.557191576,-6.79315467934256));
#109188=CARTESIAN_POINT('Ctrl Pts',(-3.56737281157474,2.622066995,-6.59785749653093));
#109189=CARTESIAN_POINT('',(-2.82515471339926,2.49144077985043,-6.94755358787023));
#109190=CARTESIAN_POINT('',(-3.34272226778266,2.58208164079413,-6.71388173945941));
#109191=CARTESIAN_POINT('Origin',(0.059392855570275,2.4107479566335,0.180431512122942));
#109192=CARTESIAN_POINT('Ctrl Pts',(-3.23257019409512,2.62129679699428,
-6.4894522060673));
#109193=CARTESIAN_POINT('Ctrl Pts',(-3.25086225817596,2.61444752746025,
-6.52682506928392));
#109194=CARTESIAN_POINT('Ctrl Pts',(-3.26919866182157,2.60775980540329,
-6.56423278756611));
#109195=CARTESIAN_POINT('Ctrl Pts',(-3.30591180070054,2.59469807479607,
-6.63903057594865));
#109196=CARTESIAN_POINT('Ctrl Pts',(-3.32430847897031,2.58831698194924,
-6.67646126717085));
#109197=CARTESIAN_POINT('Ctrl Pts',(-3.34272225931077,2.58208164076833,
-6.71388173038885));
#109198=CARTESIAN_POINT('',(-2.66720777989305,2.49144078146678,-6.87473658497311));
#109199=CARTESIAN_POINT('Origin',(7.11236625150491E-14,2.58316965300056,
1.9298798670242E-13));
#109200=CARTESIAN_POINT('',(-3.34225349745921,2.40074633454216,-6.71411509886202));
#109201=CARTESIAN_POINT('Origin',(0.0625387514614029,2.55355110413983,0.180280971376496));
#109202=CARTESIAN_POINT('',(-3.83848606137291,2.49144077881225,-6.44329301049446));
#109203=CARTESIAN_POINT('Origin',(0.0873777332257386,2.41071459753082,0.171951807332024));
#109204=CARTESIAN_POINT('Origin',(0.0900447143229784,2.55357127459312,0.170607277916298));
#109205=CARTESIAN_POINT('Ctrl Pts',(-3.228369423,2.622074631,-6.491543027));
#109206=CARTESIAN_POINT('Ctrl Pts',(-3.581132521,2.556767114,-6.316107141));
#109207=CARTESIAN_POINT('Ctrl Pts',(-3.912807385,2.491440779,-6.103477563));
#109208=CARTESIAN_POINT('Ctrl Pts',(-3.117662031,2.622074631,-6.821303648));
#109209=CARTESIAN_POINT('Ctrl Pts',(-3.488344964,2.556767114,-6.65188381800001));
#109210=CARTESIAN_POINT('Ctrl Pts',(-3.838486062,2.491440779,-6.44329300500001));
#109211=CARTESIAN_POINT('Ctrl Pts',(-3.11655495708,2.622074631,-6.82460125420999));
#109212=CARTESIAN_POINT('Ctrl Pts',(-3.48741708843,2.556767114,-6.65524158477));
#109213=CARTESIAN_POINT('Ctrl Pts',(-3.83774284877,2.491440779,-6.44669115942001));
#109214=CARTESIAN_POINT('',(-3.87564672085863,2.49144077849432,-6.27338528563182));
#109215=CARTESIAN_POINT('Ctrl Pts',(-3.88976508816575,2.48690656560517,
-6.11824948085734));
#109216=CARTESIAN_POINT('Ctrl Pts',(-3.90128623658284,2.48917367230256,
-6.11086352192864));
#109217=CARTESIAN_POINT('Ctrl Pts',(-3.912807385,2.491440779,-6.103477563));
#109218=CARTESIAN_POINT('Ctrl Pts',(-4.246944588,2.557191576,-5.889269433));
#109219=CARTESIAN_POINT('Ctrl Pts',(-4.555701191,2.622066995,-5.639865837));
#109220=CARTESIAN_POINT('Ctrl Pts',(-4.23000173462422,2.48690656560517,
-6.19400996793768));
#109221=CARTESIAN_POINT('Ctrl Pts',(-4.24166346466579,2.48917367230256,
-6.18598123507829));
#109222=CARTESIAN_POINT('Ctrl Pts',(-4.25332519470735,2.491440779,-6.17795250221879));
#109223=CARTESIAN_POINT('Ctrl Pts',(-4.59153955643061,2.557191576,-5.94510259488557));
#109224=CARTESIAN_POINT('Ctrl Pts',(-4.9023139484091,2.622066995,-5.67672355130975));
#109225=CARTESIAN_POINT('',(-4.25262281964114,2.49144077985043,-6.17779889382796));
#109226=CARTESIAN_POINT('',(-4.70785739189339,2.58208164078621,-5.83832843814145));
#109227=CARTESIAN_POINT('Origin',(0.0967917407034796,2.41074795623055,0.16344543293264));
#109228=CARTESIAN_POINT('Ctrl Pts',(-4.5520348968241,2.62129679694249,-5.64282538264453));
#109229=CARTESIAN_POINT('Ctrl Pts',(-4.57793341658891,2.61444751335628,
-5.67539230278681));
#109230=CARTESIAN_POINT('Ctrl Pts',(-4.60388273930677,2.60775977681687,
-5.70798374014004));
#109231=CARTESIAN_POINT('Ctrl Pts',(-4.65581675711939,2.59469807182015,
-5.77314043040226));
#109232=CARTESIAN_POINT('Ctrl Pts',(-4.68182983665765,2.58831697595684,
-5.80574128731554));
#109233=CARTESIAN_POINT('Ctrl Pts',(-4.70785738166523,2.58208164073532,
-5.83832843131991));
#109234=CARTESIAN_POINT('',(-4.08271509389942,2.49144078146678,-6.14063823337773));
#109235=CARTESIAN_POINT('Origin',(8.67361737988404E-15,2.58316965300056,
3.38271077815477E-14));
#109236=CARTESIAN_POINT('',(-4.70744974629859,2.4007463345217,-5.83865711346281));
#109237=CARTESIAN_POINT('Origin',(0.0998316725259318,2.55355109009625,0.162622053385927));
#109238=CARTESIAN_POINT('',(-5.13386192418331,2.49144077881253,-5.46749136466001));
#109239=CARTESIAN_POINT('Origin',(0.122299545908611,2.41071455200006,0.1491481746298));
#109240=CARTESIAN_POINT('Origin',(0.124615097880485,2.55357125344024,0.147261696059101));
#109241=CARTESIAN_POINT('Ctrl Pts',(-4.548381802,2.622074631,-5.645770362));
#109242=CARTESIAN_POINT('Ctrl Pts',(-4.85518396500001,2.556767114,-5.398602432));
#109243=CARTESIAN_POINT('Ctrl Pts',(-5.13339538200001,2.491440779,-5.119643723));
#109244=CARTESIAN_POINT('Ctrl Pts',(-4.511151473,2.622074631,-5.99162018));
#109245=CARTESIAN_POINT('Ctrl Pts',(-4.83674779000001,2.556767114,-5.746475418));
#109246=CARTESIAN_POINT('Ctrl Pts',(-5.133861925,2.491440779,-5.46749135700001));
#109247=CARTESIAN_POINT('Ctrl Pts',(-4.51077916970999,2.622074631,-5.99507867818));
#109248=CARTESIAN_POINT('Ctrl Pts',(-4.83656342825001,2.556767114,-5.74995414786));
#109249=CARTESIAN_POINT('Ctrl Pts',(-5.13386659043,2.491440779,-5.47096983334));
#109250=CARTESIAN_POINT('',(-5.13362865127118,2.49144077849432,-5.29356754216149));
#109251=CARTESIAN_POINT('Ctrl Pts',(-5.11406732737489,2.48690656569176,
-5.13902369391064));
#109252=CARTESIAN_POINT('Ctrl Pts',(-5.12373135468741,2.48917367234586,
-5.12933370845532));
#109253=CARTESIAN_POINT('Ctrl Pts',(-5.133395382,2.491440779,-5.119643723));
#109254=CARTESIAN_POINT('Ctrl Pts',(-5.413672226,2.557191576,-4.838614039));
#109255=CARTESIAN_POINT('Ctrl Pts',(-5.66159587,2.622066995,-4.528667818));
#109256=CARTESIAN_POINT('Ctrl Pts',(-5.46263569378407,2.48690656569176,
-5.13987212188714));
#109257=CARTESIAN_POINT('Ctrl Pts',(-5.47229883864984,2.48917367234586,
-5.12952416929416));
#109258=CARTESIAN_POINT('Ctrl Pts',(-5.4819619835156,2.491440779,-5.11917621670133));
#109259=CARTESIAN_POINT('Ctrl Pts',(-5.76221323472681,2.557191576,-4.81906412049436));
#109260=CARTESIAN_POINT('Ctrl Pts',(-6.00802833355053,2.622066995,-4.49015232227628));
#109261=CARTESIAN_POINT('',(-5.48124301056672,2.49144077985039,-5.11917718797777));
#109262=CARTESIAN_POINT('',(-5.85285833666219,2.5820816407985,-4.68978138803624));
#109263=CARTESIAN_POINT('Origin',(0.12966479496718,2.41074795964312,0.138816861836842));
#109264=CARTESIAN_POINT('Ctrl Pts',(-5.6586515066873,2.62129679699947,-4.53234631572041));
#109265=CARTESIAN_POINT('Ctrl Pts',(-5.69094539166984,2.61444752760817,
-4.55858436875302));
#109266=CARTESIAN_POINT('Ctrl Pts',(-5.72329415329283,2.60775980571505,
-4.58483543755505));
#109267=CARTESIAN_POINT('Ctrl Pts',(-5.78802088432703,2.59469807261756,
-4.63730463473079));
#109268=CARTESIAN_POINT('Ctrl Pts',(-5.82043400878806,2.58831697755227,
-4.663551255023));
#109269=CARTESIAN_POINT('Ctrl Pts',(-5.85285832520197,2.58208164075407,
-4.68978138350754));
#109270=CARTESIAN_POINT('',(-5.30731918799508,2.49144078146676,-5.11941046289051));
#109271=CARTESIAN_POINT('Origin',(7.45931094670027E-14,2.58316965299933,
4.16333634234434E-14));
#109272=CARTESIAN_POINT('',(-5.85253087724993,2.40074633455269,-4.6901900103424));
#109273=CARTESIAN_POINT('Origin',(0.132456444858018,2.55355106810776,0.137359050767329));
#109274=CARTESIAN_POINT('',(-6.18918411085228,2.49144077881255,-4.23603589763637));
#109275=CARTESIAN_POINT('Origin',(0.151502940283521,2.41071459750532,0.119370561588326));
#109276=CARTESIAN_POINT('Origin',(0.153358491952575,2.55357124787777,0.117030173352617));
#109277=CARTESIAN_POINT('Ctrl Pts',(-5.65571690300001,2.622074631,-4.536007751));
#109278=CARTESIAN_POINT('Ctrl Pts',(-5.902212403,2.556767114,-4.228665073));
#109279=CARTESIAN_POINT('Ctrl Pts',(-6.113951515,2.491440779,-3.896421033));
#109280=CARTESIAN_POINT('Ctrl Pts',(-5.693704486,2.622074631,-4.88177521199999));
#109281=CARTESIAN_POINT('Ctrl Pts',(-5.958989665,2.556767114,-4.572368215));
#109282=CARTESIAN_POINT('Ctrl Pts',(-6.18918411,2.491440779,-4.23603589));
#109283=CARTESIAN_POINT('Ctrl Pts',(-5.69408436183001,2.622074631,-4.88523288661));
#109284=CARTESIAN_POINT('Ctrl Pts',(-5.95955743762001,2.556767114,-4.57580524642));
#109285=CARTESIAN_POINT('Ctrl Pts',(-6.18993643594999,2.491440779,-4.23943203857));
#109286=CARTESIAN_POINT('',(-6.15156781078794,2.49144077849432,-4.06622846409008));
#109287=CARTESIAN_POINT('Ctrl Pts',(-6.09924145970536,2.48690656548447,
-3.91950287244791));
#109288=CARTESIAN_POINT('Ctrl Pts',(-6.10659648735274,2.48917367224221,
-3.90796195272396));
#109289=CARTESIAN_POINT('Ctrl Pts',(-6.113951515,2.491440779,-3.896421033));
#109290=CARTESIAN_POINT('Ctrl Pts',(-6.327262568,2.557191576,-3.56171043));
#109291=CARTESIAN_POINT('Ctrl Pts',(-6.502760619,2.622066995,-3.205714324));
#109292=CARTESIAN_POINT('Ctrl Pts',(-6.43984287951191,2.48690656548447,
-3.84539956878979));
#109293=CARTESIAN_POINT('Ctrl Pts',(-6.44705560182278,2.48917367224221,
-3.83321625452855));
#109294=CARTESIAN_POINT('Ctrl Pts',(-6.45426832413366,2.491440779,-3.82103294026727));
#109295=CARTESIAN_POINT('Ctrl Pts',(-6.66345222729634,2.557191576,-3.46769156362974));
#109296=CARTESIAN_POINT('Ctrl Pts',(-6.83281399032402,2.622066995,-3.09362655994177));
#109297=CARTESIAN_POINT('',(-6.45356636728458,2.49144077985042,-3.82118844870344));
#109298=CARTESIAN_POINT('',(-6.72418613066418,2.58208164076895,-3.32194537211322));
#109299=CARTESIAN_POINT('Origin',(0.156474591155465,2.4107479616494,0.107697166367046));
#109300=CARTESIAN_POINT('Ctrl Pts',(-6.5006758616883,2.62129679701399,-3.20993977145643));
#109301=CARTESIAN_POINT('Ctrl Pts',(-6.53785521611478,2.61444751350204,
-3.22862220123853));
#109302=CARTESIAN_POINT('Ctrl Pts',(-6.57509097269971,2.60775977699807,
-3.24730555074524));
#109303=CARTESIAN_POINT('Ctrl Pts',(-6.64958357449561,2.5946980755614,-3.28463362300767));
#109304=CARTESIAN_POINT('Ctrl Pts',(-6.68688112675005,2.58831698350122,
-3.30329873896052));
#109305=CARTESIAN_POINT('Ctrl Pts',(-6.72418611842758,2.58208164075017,
-3.32194536991413));
#109306=CARTESIAN_POINT('',(-6.28375893558179,2.49144078146676,-3.85880474889419));
#109307=CARTESIAN_POINT('Origin',(-1.77722420113824E-12,2.583169653,-9.55832635263221E-13));
#109308=CARTESIAN_POINT('',(-6.72395416877965,2.40074633454126,-3.32241483495408));
#109309=CARTESIAN_POINT('Origin',(0.158887903390401,2.55355108009206,0.105673490532908));
#109310=CARTESIAN_POINT('',(-6.95510692647806,2.4914407788125,-2.80650809933182));
#109311=CARTESIAN_POINT('Origin',(0.173621591640072,2.41071463550373,0.0840108764685926));
#109312=CARTESIAN_POINT('Origin',(0.174931003160467,2.55357126558374,0.0813264799573265));
#109313=CARTESIAN_POINT('Ctrl Pts',(-6.498596968,2.622074631,-3.214146458));
#109314=CARTESIAN_POINT('Ctrl Pts',(-6.67325995,2.556767114,-2.861000035));
#109315=CARTESIAN_POINT('Ctrl Pts',(-6.808626071,2.491440779,-2.491006026));
#109316=CARTESIAN_POINT('Ctrl Pts',(-6.610026206,2.622074631,-3.543663861));
#109317=CARTESIAN_POINT('Ctrl Pts',(-6.80259580600001,2.556767114,-3.184462156));
#109318=CARTESIAN_POINT('Ctrl Pts',(-6.955106924,2.491440779,-2.806508092));
#109319=CARTESIAN_POINT('Ctrl Pts',(-6.61114049838,2.622074631,-3.54695903503));
#109320=CARTESIAN_POINT('Ctrl Pts',(-6.80388916456,2.556767114,-3.18769677721));
#109321=CARTESIAN_POINT('Ctrl Pts',(-6.95657173253,2.491440779,-2.80966311266));
#109322=CARTESIAN_POINT('',(-6.88186649638476,2.49144077849432,-2.64875706189757));
#109323=CARTESIAN_POINT('Ctrl Pts',(-6.79922184204682,2.48690656561667,
-2.51671045117644));
#109324=CARTESIAN_POINT('Ctrl Pts',(-6.80392395652347,2.48917367230831,
-2.5038582385882));
#109325=CARTESIAN_POINT('Ctrl Pts',(-6.808626071,2.491440779,-2.491006026));
#109326=CARTESIAN_POINT('Ctrl Pts',(-6.944997145,2.557191576,-2.1182652));
#109327=CARTESIAN_POINT('Ctrl Pts',(-7.039863509,2.622066995,-1.732865192));
#109328=CARTESIAN_POINT('Ctrl Pts',(-7.11593016962833,2.48690656561667,
-2.37112040446412));
#109329=CARTESIAN_POINT('Ctrl Pts',(-7.12035520993026,2.48917367230831,
-2.35767140762744));
#109330=CARTESIAN_POINT('Ctrl Pts',(-7.12478025023214,2.491440779,-2.34422241079084));
#109331=CARTESIAN_POINT('Ctrl Pts',(-7.25311559839781,2.557191576,-1.9541736036031));
#109332=CARTESIAN_POINT('Ctrl Pts',(-7.33810486046178,2.622066995,-1.55244625913541));
#109333=CARTESIAN_POINT('',(-7.12412813449252,2.49144077985043,-2.34452518347534));
#109334=CARTESIAN_POINT('',(-7.28109845461218,2.58208164083062,-1.79877888269512));
#109335=CARTESIAN_POINT('Origin',(0.175968276889885,2.41074793770117,0.0715419416780225));
#109336=CARTESIAN_POINT('Ctrl Pts',(-7.03873583834957,2.62129679700212,
-1.7374400121656));
#109337=CARTESIAN_POINT('Ctrl Pts',(-7.07906204740106,2.61444752758852,
-1.74769317383412));
#109338=CARTESIAN_POINT('Ctrl Pts',(-7.11944352632008,2.60775980565941,
-1.75793510623339));
#109339=CARTESIAN_POINT('Ctrl Pts',(-7.20021915405798,2.5946980736025,-1.77837680933423));
#109340=CARTESIAN_POINT('Ctrl Pts',(-7.24065717235596,2.58831697949574,
-1.78858767743524));
#109341=CARTESIAN_POINT('Ctrl Pts',(-7.28109844228063,2.58208164079368,
-1.79877888333402));
#109342=CARTESIAN_POINT('',(-6.96637709903875,2.49144078146678,-2.41776561379499));
#109343=CARTESIAN_POINT('Origin',(-6.28837260041593E-13,2.58316965300011,
-9.69276742202041E-14));
#109344=CARTESIAN_POINT('',(-7.2809728364116,2.40074633457368,-1.79928723503158));
#109345=CARTESIAN_POINT('Origin',(0.177890141013355,2.55355108091248,0.0690467838518782));
#109346=CARTESIAN_POINT('',(-7.39581667399581,2.49144077881244,-1.24575110158275));
#109347=CARTESIAN_POINT('Origin',(0.18762263744327,2.41071458012096,0.0447233372678933));
#109348=CARTESIAN_POINT('Origin',(0.188324448607427,2.55357128732538,0.041820229100871));
#109349=CARTESIAN_POINT('Ctrl Pts',(-7.037609861,2.622074631,-1.741995249));
#109350=CARTESIAN_POINT('Ctrl Pts',(-7.132273277,2.556767114,-1.359557815));
#109351=CARTESIAN_POINT('Ctrl Pts',(-7.184936839,2.491440779,-0.969114346));
#109352=CARTESIAN_POINT('Ctrl Pts',(-7.21727044700001,2.622074631,-2.039854725));
#109353=CARTESIAN_POINT('Ctrl Pts',(-7.328120127,2.556767114,-1.647654185));
#109354=CARTESIAN_POINT('Ctrl Pts',(-7.39581667,2.491440779,-1.245751095));
#109355=CARTESIAN_POINT('Ctrl Pts',(-7.21906705286,2.622074631,-2.04283331976));
#109356=CARTESIAN_POINT('Ctrl Pts',(-7.3300785955,2.556767114,-1.6505351487));
#109357=CARTESIAN_POINT('Ctrl Pts',(-7.39792546831,2.491440779,-1.24851746249));
#109358=CARTESIAN_POINT('',(-7.29037675403372,2.49144077849432,-1.10743272356957));
#109359=CARTESIAN_POINT('Ctrl Pts',(-7.18127816726304,2.48690656553082,
-0.9962394477905));
#109360=CARTESIAN_POINT('Ctrl Pts',(-7.18310750313154,2.48917367226538,
-0.982676896895252));
#109361=CARTESIAN_POINT('Ctrl Pts',(-7.184936839,2.491440779,-0.969114346));
#109362=CARTESIAN_POINT('Ctrl Pts',(-7.237991373,2.557191576,-0.575772243));
#109363=CARTESIAN_POINT('Ctrl Pts',(-7.247790206,2.622066995,-0.178989209));
#109364=CARTESIAN_POINT('Ctrl Pts',(-7.45928447412705,2.48690656553082,
-0.785970285862701));
#109365=CARTESIAN_POINT('Ctrl Pts',(-7.46071492270005,2.48917367226538,
-0.771884465993628));
#109366=CARTESIAN_POINT('Ctrl Pts',(-7.46214537127316,2.491440779,-0.757798646124541));
#109367=CARTESIAN_POINT('Ctrl Pts',(-7.50363134646488,2.557191576,-0.349280657688787));
#109368=CARTESIAN_POINT('Ctrl Pts',(-7.50027410217251,2.622066995,0.0613247038400555));
#109369=CARTESIAN_POINT('',(-7.46157358879537,2.49144077985042,-0.758234525785307));
#109370=CARTESIAN_POINT('',(-7.49755470733861,2.58208164080026,-0.191503492201462));
#109371=CARTESIAN_POINT('Origin',(0.187233531968248,2.41074792168317,0.032041345118505));
#109372=CARTESIAN_POINT('Ctrl Pts',(-7.24767235074776,2.62129679697139,
-0.183699488456621));
#109373=CARTESIAN_POINT('Ctrl Pts',(-7.2892598818894,2.61444752755311,-0.185043994028461));
#109374=CARTESIAN_POINT('Ctrl Pts',(-7.33089897670836,2.60775980564852,
-0.186365651459866));
#109375=CARTESIAN_POINT('Ctrl Pts',(-7.41418046610708,2.59469807529747,
-0.188965066345878));
#109376=CARTESIAN_POINT('Ctrl Pts',(-7.45586808822642,2.58831698299861,
-0.19024423107201));
#109377=CARTESIAN_POINT('Ctrl Pts',(-7.49755469532192,2.58208164077877,
-0.191503495362631));
#109378=CARTESIAN_POINT('',(-7.32325521222775,2.49144078146676,-0.863674445527217));
#109379=CARTESIAN_POINT('Origin',(9.00321484031963E-13,2.58316965299956,
9.75781955236954E-16));
#109380=CARTESIAN_POINT('',(-7.49754130651673,2.40074633455664,-0.192026963734102));
#109381=CARTESIAN_POINT('Origin',(0.188574016816311,2.55355108770253,0.0291913730601223));
#109382=CARTESIAN_POINT('',(-7.49070625230964,2.49144077881258,0.373255832402669));
#109383=CARTESIAN_POINT('Origin',(0.192850144084868,2.41071460097831,0.00334440390496821));
#109384=CARTESIAN_POINT('Origin',(0.192911317040971,2.55357123636567,0.000358288584547154));
#109385=CARTESIAN_POINT('Ctrl Pts',(-7.24755193900001,2.622074631,-0.188390278));
#109386=CARTESIAN_POINT('Ctrl Pts',(-7.257789433,2.556767114,0.205455817));
#109387=CARTESIAN_POINT('Ctrl Pts',(-7.225287946,2.491440779,0.598092044));
#109388=CARTESIAN_POINT('Ctrl Pts',(-7.487043143,2.622074631,-0.440664251));
#109389=CARTESIAN_POINT('Ctrl Pts',(-7.510989697,2.556767114,-0.033803736));
#109390=CARTESIAN_POINT('Ctrl Pts',(-7.490706247,2.491440779,0.373255838));
#109391=CARTESIAN_POINT('Ctrl Pts',(-7.48943805504001,2.622074631,-0.44318699073));
#109392=CARTESIAN_POINT('Ctrl Pts',(-7.51352169964,2.556767114,-0.0361963315300001));
#109393=CARTESIAN_POINT('Ctrl Pts',(-7.49336043001,2.491440779,0.37100747594));
#109394=CARTESIAN_POINT('',(-7.35799709670449,2.49144077849432,0.485673937901959));
#109395=CARTESIAN_POINT('Ctrl Pts',(-7.22754590707776,2.48690656539367,
0.570814604899168));
#109396=CARTESIAN_POINT('Ctrl Pts',(-7.22641692653879,2.48917367219681,
0.584453324449584));
#109397=CARTESIAN_POINT('Ctrl Pts',(-7.225287946,2.491440779,0.598092044));
#109398=CARTESIAN_POINT('Ctrl Pts',(-7.19254517,2.557191576,0.993643183999999));
#109399=CARTESIAN_POINT('Ctrl Pts',(-7.116818287,2.622066995,1.38325611));
#109400=CARTESIAN_POINT('Ctrl Pts',(-7.4538509263014,2.48690656539367,0.835930928125738));
#109401=CARTESIAN_POINT('Ctrl Pts',(-7.45221989685616,2.48917367219681,
0.849994933965902));
#109402=CARTESIAN_POINT('Ctrl Pts',(-7.45058886741099,2.491440779,0.864058939806079));
#109403=CARTESIAN_POINT('Ctrl Pts',(-7.40328563237933,2.557191576,1.27194426382674));
#109404=CARTESIAN_POINT('Ctrl Pts',(-7.31173886259761,2.622066995,1.6722281922973));
#109405=CARTESIAN_POINT('',(-7.45012415412549,2.49144077985042,0.863510334451682));
#109406=CARTESIAN_POINT('',(-7.36343363451669,2.58208164079611,1.42472638913831));
#109407=CARTESIAN_POINT('Origin',(0.189743853020058,2.41074793455603,-0.00895740390180852));
#109408=CARTESIAN_POINT('Ctrl Pts',(-7.11771575797403,2.62129679704776,
1.37863061942135));
#109409=CARTESIAN_POINT('Ctrl Pts',(-7.15862010913201,2.61444751349351,
1.38625765323444));
#109410=CARTESIAN_POINT('Ctrl Pts',(-7.19956991822297,2.60775977696405,
1.39391808802037));
#109411=CARTESIAN_POINT('Ctrl Pts',(-7.28146295658397,2.59469807427698,
1.40928247184832));
#109412=CARTESIAN_POINT('Ctrl Pts',(-7.32245093530049,2.58831698089371,
1.41699482114407));
#109413=CARTESIAN_POINT('Ctrl Pts',(-7.36343362353817,2.58208164076581,
1.42472638341801));
#109414=CARTESIAN_POINT('',(-7.33770605049959,2.49144078146676,0.73080117944313));
#109415=CARTESIAN_POINT('Origin',(5.68121938382404E-13,2.583169653,-6.21247844834194E-14));
#109416=CARTESIAN_POINT('',(-7.363533078059,2.40074633454557,1.42421227530058));
#109417=CARTESIAN_POINT('Origin',(0.190440384937789,2.55355104710757,-0.0120289222636236));
#109418=CARTESIAN_POINT('',(-7.23533873239084,2.49144077881247,1.97480973969609));
#109419=CARTESIAN_POINT('Origin',(0.189060473731137,2.4107145792923,-0.0381908852372392));
#109420=CARTESIAN_POINT('Origin',(0.188478046561856,2.55357127601239,-0.041120270749862));
#109421=CARTESIAN_POINT('Ctrl Pts',(-7.118606543,2.622074631,1.374023613));
#109422=CARTESIAN_POINT('Ctrl Pts',(-7.043939422,2.556767114,1.760862564));
#109423=CARTESIAN_POINT('Ctrl Pts',(-6.927792619,2.491440779,2.137332315));
#109424=CARTESIAN_POINT('Ctrl Pts',(-7.406730022,2.622074631,1.179131195));
#109425=CARTESIAN_POINT('Ctrl Pts',(-7.342653736,2.556767114,1.581627338));
#109426=CARTESIAN_POINT('Ctrl Pts',(-7.235338726,2.491440779,1.974809744));
#109427=CARTESIAN_POINT('Ctrl Pts',(-7.40961125679,2.622074631,1.17718227082));
#109428=CARTESIAN_POINT('Ctrl Pts',(-7.34564087914,2.556767114,1.57983498574));
#109429=CARTESIAN_POINT('Ctrl Pts',(-7.23841418707,2.491440779,1.97318451829));
#109430=CARTESIAN_POINT('',(-7.08156567336569,2.49144077849432,2.05607102651835));
#109431=CARTESIAN_POINT('Ctrl Pts',(-6.93586163280649,2.48690656567579,
2.11117800379407));
#109432=CARTESIAN_POINT('Ctrl Pts',(-6.93182712590332,2.48917367233787,
2.12425515939704));
#109433=CARTESIAN_POINT('Ctrl Pts',(-6.92779261899999,2.491440779,2.137332315));
#109434=CARTESIAN_POINT('Ctrl Pts',(-6.810783548,2.557191576,2.51659696));
#109435=CARTESIAN_POINT('Ctrl Pts',(-6.653071856,2.622066995,2.880821911));
#109436=CARTESIAN_POINT('Ctrl Pts',(-7.09988359422218,2.48690656567579,
2.41874494454143));
#109437=CARTESIAN_POINT('Ctrl Pts',(-7.09526735207894,2.48917367233787,
2.43212951777117));
#109438=CARTESIAN_POINT('Ctrl Pts',(-7.09065110993579,2.491440779,2.44551409100092));
#109439=CARTESIAN_POINT('Ctrl Pts',(-6.95677050999374,2.557191576,2.83369448500872));
#109440=CARTESIAN_POINT('Ctrl Pts',(-6.78131484150381,2.622066995,3.20494014823205));
#109441=CARTESIAN_POINT('',(-7.09031519534277,2.49144077985042,2.44487841211678));
#109442=CARTESIAN_POINT('',(-6.88500658986866,2.58208164074794,2.97433764640151));
#109443=CARTESIAN_POINT('Origin',(0.183382424378213,2.41074792779091,-0.0495374053930203));
#109444=CARTESIAN_POINT('Ctrl Pts',(-6.65494268860644,2.6212967969372,2.87649749092932));
#109445=CARTESIAN_POINT('Ctrl Pts',(-6.69325113231692,2.61444751332667,
2.89273943554867));
#109446=CARTESIAN_POINT('Ctrl Pts',(-6.73159679081763,2.60775977676549,
2.90902377224826));
#109447=CARTESIAN_POINT('Ctrl Pts',(-6.80827173775859,2.59469817447579,
2.94163327719176));
#109448=CARTESIAN_POINT('Ctrl Pts',(-6.84664284917639,2.58831718441713,
2.95797623595795));
#109449=CARTESIAN_POINT('Ctrl Pts',(-6.88500658063842,2.58208164062072,
2.97433763948164));
#109450=CARTESIAN_POINT('',(-7.00905390970131,2.49144078146676,2.29110535411757));
#109451=CARTESIAN_POINT('Ctrl Pts',(-6.656803017,2.622074631,2.872189686));
#109452=CARTESIAN_POINT('Ctrl Pts',(-6.500722632,2.556767114,3.233933334));
#109453=CARTESIAN_POINT('Ctrl Pts',(-6.306361409,2.491440779,3.576633302));
#109454=CARTESIAN_POINT('Ctrl Pts',(-6.980086438,2.622074631,2.743791776));
#109455=CARTESIAN_POINT('Ctrl Pts',(-6.830983446,2.556767114,3.123103275));
#109456=CARTESIAN_POINT('Ctrl Pts',(-6.641654807,2.491440779,3.48402374));
#109457=CARTESIAN_POINT('Ctrl Pts',(-6.98331927221,2.622074631,2.7425077969));
#109458=CARTESIAN_POINT('Ctrl Pts',(-6.83428605413999,2.556767114,3.12199497441));
#109459=CARTESIAN_POINT('Ctrl Pts',(-6.64500774098,2.491440779,3.48309764438));
#109460=CARTESIAN_POINT('',(-6.6416548109875,2.49144077881208,3.48402374074511));
#109461=CARTESIAN_POINT('Origin',(0.175232140450808,2.55357127254053,-0.0806762294126564));
#109462=CARTESIAN_POINT('',(-6.4740081094864,2.49144077849433,3.5303285182742));
#109463=CARTESIAN_POINT('Origin',(-2.90999863095109E-13,2.58316965299956,
1.45283091113058E-13));
#109464=CARTESIAN_POINT('',(-6.88521422698715,2.40074633447349,2.97385693108466));
#109465=CARTESIAN_POINT('Origin',(0.183402177679237,2.55355105024397,-0.052686769679634));
#109466=CARTESIAN_POINT('Origin',(0.176430275859584,2.41071461896874,-0.0779403562094694));
#109467=CARTESIAN_POINT('Ctrl Pts',(-6.31986417766011,2.48690656564425,
3.55282506333069));
#109468=CARTESIAN_POINT('Ctrl Pts',(-6.31311279333012,2.4891736723221,3.56472918266534));
#109469=CARTESIAN_POINT('Ctrl Pts',(-6.306361409,2.491440779,3.576633302));
#109470=CARTESIAN_POINT('Ctrl Pts',(-6.110557257,2.557191576,3.921877459));
#109471=CARTESIAN_POINT('Ctrl Pts',(-5.87823517799999,2.622066995,4.243683681));
#109472=CARTESIAN_POINT('Ctrl Pts',(-6.41393359556659,2.48690656564425,
3.8884611333781));
#109473=CARTESIAN_POINT('Ctrl Pts',(-6.40654799092982,2.4891736723221,3.90054042721907));
#109474=CARTESIAN_POINT('Ctrl Pts',(-6.39916238629304,2.491440779,3.9126197210601));
#109475=CARTESIAN_POINT('Ctrl Pts',(-6.18496452964555,2.557191576,4.26294430216168));
#109476=CARTESIAN_POINT('Ctrl Pts',(-5.93380407379803,2.622066995,4.58779266501244));
#109477=CARTESIAN_POINT('',(-6.39897097736251,2.49144077985043,3.91192669229793));
#109478=CARTESIAN_POINT('',(-6.35266619768326,2.49144078146678,3.74427998846434));
#109479=CARTESIAN_POINT('',(-6.08464428739668,2.58208164078499,4.38487218380399));
#109480=CARTESIAN_POINT('Origin',(0.168445965700353,2.41074796746151,-0.0878010593493334));
#109481=CARTESIAN_POINT('Ctrl Pts',(-5.88099189403263,2.62129679694873,
4.23986253723593));
#109482=CARTESIAN_POINT('Ctrl Pts',(-5.9149131694583,2.61444751339891,4.26395993721713));
#109483=CARTESIAN_POINT('Ctrl Pts',(-5.94886167659632,2.60775977687749,
4.28810673828796));
#109484=CARTESIAN_POINT('Ctrl Pts',(-6.01673444503164,2.59469807475853,
4.33643706788972));
#109485=CARTESIAN_POINT('Ctrl Pts',(-6.05069579275439,2.58831698187106,
4.36064701015502));
#109486=CARTESIAN_POINT('Ctrl Pts',(-6.08464427979713,2.58208164075899,
4.3848721740135));
#109487=CARTESIAN_POINT('Origin',(1.04170144732407E-12,2.58316965300044,
-7.54171031180917E-13));
#109488=CARTESIAN_POINT('',(-5.73741449653065,2.49144077881202,4.83032865927712));
#109489=CARTESIAN_POINT('Origin',(0.153792080296967,2.5535713027714,-0.116459622361033));
#109490=CARTESIAN_POINT('',(-6.08495041118466,2.40074633452799,4.38444734227674));
#109491=CARTESIAN_POINT('Origin',(0.167788274850221,2.55355109662838,-0.0908810363877111));
#109492=CARTESIAN_POINT('Origin',(0.155550450071232,2.41071458854319,-0.114045366558431));
#109493=CARTESIAN_POINT('Ctrl Pts',(-5.88373478,2.622074631,4.236055362));
#109494=CARTESIAN_POINT('Ctrl Pts',(-5.653539277,2.556767114,4.555788976));
#109495=CARTESIAN_POINT('Ctrl Pts',(-5.390051748,2.491440779,4.848694892));
#109496=CARTESIAN_POINT('Ctrl Pts',(-6.22706177,2.622074631,4.180155704));
#109497=CARTESIAN_POINT('Ctrl Pts',(-5.999903964,2.556767114,4.518546375));
#109498=CARTESIAN_POINT('Ctrl Pts',(-5.737414491,2.491440779,4.830328659));
#109499=CARTESIAN_POINT('Ctrl Pts',(-6.23049503989999,2.622074631,4.17959670742));
#109500=CARTESIAN_POINT('Ctrl Pts',(-6.00336761087,2.556767114,4.51817394899));
#109501=CARTESIAN_POINT('Ctrl Pts',(-5.74088811843,2.491440779,4.83014499667));
#109502=CARTESIAN_POINT('',(-5.56373312153948,2.49144077849386,4.83951177315532));
#109503=CARTESIAN_POINT('Ctrl Pts',(-5.40835689678428,2.48690656569021,
4.82834597309885));
#109504=CARTESIAN_POINT('Ctrl Pts',(-5.39920432239215,2.48917367234508,
4.83852043254936));
#109505=CARTESIAN_POINT('Ctrl Pts',(-5.390051748,2.491440779,4.848694892));
#109506=CARTESIAN_POINT('Ctrl Pts',(-5.1246081,2.557191576,5.143775327));
#109507=CARTESIAN_POINT('Ctrl Pts',(-4.828538757,2.622066995,5.408115519));
#109508=CARTESIAN_POINT('Ctrl Pts',(-5.42807519093172,2.48690656569021,
5.17635720151946));
#109509=CARTESIAN_POINT('Ctrl Pts',(-5.41826556660759,2.48917367234508,
5.18656640138796));
#109510=CARTESIAN_POINT('Ctrl Pts',(-5.40845594228348,2.491440779,5.19677560125659));
#109511=CARTESIAN_POINT('Ctrl Pts',(-5.12395648294661,2.557191576,5.49286358046064));
#109512=CARTESIAN_POINT('Ctrl Pts',(-4.80883522364381,2.622066995,5.75612509553517));
#109513=CARTESIAN_POINT('',(-5.40841798908711,2.49144077985043,5.19605762786303));
#109514=CARTESIAN_POINT('',(-4.99977078188444,2.58208164079232,5.59037496954931));
#109515=CARTESIAN_POINT('Origin',(0.145633230011868,2.41074796083966,-0.121959297299493));
#109516=CARTESIAN_POINT('Ctrl Pts',(-4.83205245536802,2.62129679697757,
5.40497632402769));
#109517=CARTESIAN_POINT('Ctrl Pts',(-4.86000044148469,2.61444751346176,
5.43580241133959));
#109518=CARTESIAN_POINT('Ctrl Pts',(-4.88796440292578,2.60775977695734,
5.46668259888027));
#109519=CARTESIAN_POINT('Ctrl Pts',(-4.94386075122956,2.59469807493931,
5.52847363037815));
#109520=CARTESIAN_POINT('Ctrl Pts',(-4.97182367878698,2.58831698223328,
5.55941824246101));
#109521=CARTESIAN_POINT('Ctrl Pts',(-4.99977077658195,2.58208164076771,
5.590374958319));
#109522=CARTESIAN_POINT('',(-5.39923487480582,2.49144078146676,5.02237625242088));
#109523=CARTESIAN_POINT('Origin',(-3.58220397789211E-13,2.58316965299911,
3.24826970876657E-13));
#109524=CARTESIAN_POINT('',(-5.00016107681822,2.40074633453083,5.5900258682109));
#109525=CARTESIAN_POINT('Origin',(0.144328703502746,2.5535510911766,-0.124825772307806));
#109526=CARTESIAN_POINT('',(-4.56489905870438,2.49144077881237,5.95077277843231));
#109527=CARTESIAN_POINT('Origin',(0.127397609975873,2.41071461307179,-0.144818061835398));
#109528=CARTESIAN_POINT('Origin',(0.125161223023721,2.5535712640916,-0.146797725607393));
#109529=CARTESIAN_POINT('Ctrl Pts',(-4.835549645,2.622074631,5.401847798));
#109530=CARTESIAN_POINT('Ctrl Pts',(-4.542002709,2.556767114,5.664620989));
#109531=CARTESIAN_POINT('Ctrl Pts',(-4.221709258,2.491440779,5.894036897));
#109532=CARTESIAN_POINT('Ctrl Pts',(-5.182866615,2.622074631,5.421060196));
#109533=CARTESIAN_POINT('Ctrl Pts',(-4.88827564,2.556767114,5.702707268));
#109534=CARTESIAN_POINT('Ctrl Pts',(-4.564899051,2.491440779,5.95077277800001));
#109535=CARTESIAN_POINT('Ctrl Pts',(-5.1863397847,2.622074631,5.42125231998));
#109536=CARTESIAN_POINT('Ctrl Pts',(-4.89173836931,2.556767114,5.70308813079));
#109537=CARTESIAN_POINT('Ctrl Pts',(-4.56833094893,2.491440779,5.95134013681001));
#109538=CARTESIAN_POINT('',(-4.39330415699558,2.49144077849392,5.92240483564876));
#109539=CARTESIAN_POINT('Ctrl Pts',(-4.24396085842985,2.48690656573101,
5.878098790588));
#109540=CARTESIAN_POINT('Ctrl Pts',(-4.23283505821495,2.48917367236547,
5.88606784379398));
#109541=CARTESIAN_POINT('Ctrl Pts',(-4.221709258,2.491440779,5.894036897));
#109542=CARTESIAN_POINT('Ctrl Pts',(-3.899037964,2.557191576,6.125155977));
#109543=CARTESIAN_POINT('Ctrl Pts',(-3.553065231,2.622066995,6.31966988600001));
#109544=CARTESIAN_POINT('Ctrl Pts',(-4.18840602291764,2.486906565731,6.22221255992507));
#109545=CARTESIAN_POINT('Ctrl Pts',(-4.17663106608019,2.48917367236548,
6.23007429505655));
#109546=CARTESIAN_POINT('Ctrl Pts',(-4.16485610924274,2.491440779,6.23793603018786));
#109547=CARTESIAN_POINT('Ctrl Pts',(-3.82335792608898,2.557191576,6.46594266332069));
#109548=CARTESIAN_POINT('Ctrl Pts',(-3.45901058282517,2.622066995,6.65530751465221));
#109549=CARTESIAN_POINT('',(-4.16497338460572,2.49144077985039,6.23722668575043));
#109550=CARTESIAN_POINT('',(-3.6811135513713,2.58208164079298,6.53447803534407));
#109551=CARTESIAN_POINT('Origin',(0.116010728969889,2.41074796290915,-0.150414734490522));
#109552=CARTESIAN_POINT('Ctrl Pts',(-3.55717161529104,2.62129679695473,
6.31735942486863));
#109553=CARTESIAN_POINT('Ctrl Pts',(-3.57783949549941,2.61444751335948,
6.35347280667645));
#109554=CARTESIAN_POINT('Ctrl Pts',(-3.59851134755322,2.60775977681711,
6.38964245789835));
#109555=CARTESIAN_POINT('Ctrl Pts',(-3.6398176296258,2.59469807329828,6.46200492028157));
#109556=CARTESIAN_POINT('Ctrl Pts',(-3.66047462828288,2.58831697893288,
6.49823727743706));
#109557=CARTESIAN_POINT('Ctrl Pts',(-3.68111354872381,2.58208164075444,
6.53447802327984));
#109558=CARTESIAN_POINT('',(-4.19334132994659,2.49144078146676,6.06563178439533));
#109559=CARTESIAN_POINT('Origin',(-6.54858112181245E-14,2.58316965300011,
-2.73218947466347E-14));
#109560=CARTESIAN_POINT('',(-3.68156976764956,2.40074633450494,6.53422099774582));
#109561=CARTESIAN_POINT('Origin',(0.114120472869241,2.55355107061601,-0.152933734037438));
#109562=CARTESIAN_POINT('',(-3.17893401143449,2.49144077881209,6.79296537807907));
#109563=CARTESIAN_POINT('Origin',(0.0932874242503334,2.41071459168756,-0.16881882010749));
#109564=CARTESIAN_POINT('Origin',(0.0906779232206405,2.55357127085558,-0.170271772113147));
#109565=CARTESIAN_POINT('Ctrl Pts',(-3.561259582,2.622074631,6.315055834));
#109566=CARTESIAN_POINT('Ctrl Pts',(-3.218087142,2.556767114,6.50858162));
#109567=CARTESIAN_POINT('Ctrl Pts',(-2.855964336,2.491440779,6.663780287));
#109568=CARTESIAN_POINT('Ctrl Pts',(-3.896326377,2.622074631,6.408481939));
#109569=CARTESIAN_POINT('Ctrl Pts',(-3.54807698,2.556767114,6.620215907));
#109570=CARTESIAN_POINT('Ctrl Pts',(-3.178934004,2.491440779,6.792965376));
#109571=CARTESIAN_POINT('Ctrl Pts',(-3.89967704495,2.622074631,6.40941620005));
#109572=CARTESIAN_POINT('Ctrl Pts',(-3.55137687838,2.556767114,6.62133224987001));
#109573=CARTESIAN_POINT('Ctrl Pts',(-3.18216370068,2.491440779,6.79425722688999));
#109574=CARTESIAN_POINT('',(-3.01744917283955,2.49144077849314,6.72837283022655));
#109575=CARTESIAN_POINT('Ctrl Pts',(-2.88112192769865,2.48690656581069,
6.65299824113503));
#109576=CARTESIAN_POINT('Ctrl Pts',(-2.86854313184929,2.48917367240532,
6.65838926406759));
#109577=CARTESIAN_POINT('Ctrl Pts',(-2.855964336,2.491440779,6.663780287));
#109578=CARTESIAN_POINT('Ctrl Pts',(-2.491153147,2.557191576,6.820131142));
#109579=CARTESIAN_POINT('Ctrl Pts',(-2.111454323,2.622066995,6.935723513));
#109580=CARTESIAN_POINT('Ctrl Pts',(-2.75289164418675,2.48690656581069,
6.97712417427914));
#109581=CARTESIAN_POINT('Ctrl Pts',(-2.73970193885012,2.48917367240532,
6.98227083867556));
#109582=CARTESIAN_POINT('Ctrl Pts',(-2.72651223351355,2.491440779,6.98741750307182));
#109583=CARTESIAN_POINT('Ctrl Pts',(-2.34398340133904,2.557191576,7.1366814533166));
#109584=CARTESIAN_POINT('Ctrl Pts',(-1.94744645129448,2.622066995,7.24329515151907));
#109585=CARTESIAN_POINT('',(-2.72677925511041,2.49144077985039,6.9867499534755));
#109586=CARTESIAN_POINT('',(-2.1903315421454,2.58208164079196,7.17303617095425));
#109587=CARTESIAN_POINT('Origin',(0.0809637820517822,2.41074797514361,-0.171837106840123));
#109588=CARTESIAN_POINT('Ctrl Pts',(-2.11596138345152,2.62129679691413,
6.93434982023637));
#109589=CARTESIAN_POINT('Ctrl Pts',(-2.1283827246779,2.61444752758119,6.97406179194022));
#109590=CARTESIAN_POINT('Ctrl Pts',(-2.14079584527957,2.60775980576447,
7.01382956018076));
#109591=CARTESIAN_POINT('Ctrl Pts',(-2.16558067114611,2.59469807468317,
7.09338002604718));
#109592=CARTESIAN_POINT('Ctrl Pts',(-2.17796583179262,2.58831698174837,
7.13320592542989));
#109593=CARTESIAN_POINT('Ctrl Pts',(-2.1903315420636,2.58208164076534,7.17303615854577));
#109594=CARTESIAN_POINT('',(-2.7913718055054,2.49144078146677,6.82526511527213));
#109595=CARTESIAN_POINT('Origin',(4.62737487216813E-13,2.58316965300044,
-1.26721549920106E-12));
#109596=CARTESIAN_POINT('',(-2.19083234810414,2.40074633453921,7.17288321534959));
#109597=CARTESIAN_POINT('Origin',(0.0785761618095226,2.55355108003917,-0.173890731842352));
#109598=CARTESIAN_POINT('',(-1.64432554279914,2.4914407788121,7.31752646662564));
#109599=CARTESIAN_POINT('Origin',(0.0548153802276763,2.41071457910362,-0.184926017836832));
#109600=CARTESIAN_POINT('Origin',(0.0519544797054261,2.55357126758846,-0.185783815545175));
#109601=CARTESIAN_POINT('Ctrl Pts',(-2.12044898,2.622074631,6.932978878));
#109602=CARTESIAN_POINT('Ctrl Pts',(-1.743697397,2.556767114,7.048208208));
#109603=CARTESIAN_POINT('Ctrl Pts',(-1.356677695,2.491440779,7.121932718));
#109604=CARTESIAN_POINT('Ctrl Pts',(-2.427598248,2.622074631,7.096250189));
#109605=CARTESIAN_POINT('Ctrl Pts',(-2.041974184,2.556767114,7.228170609));
#109606=CARTESIAN_POINT('Ctrl Pts',(-1.644325536,2.491440779,7.317526463));
#109607=CARTESIAN_POINT('Ctrl Pts',(-2.43066974068,2.622074631,7.09788290211));
#109608=CARTESIAN_POINT('Ctrl Pts',(-2.04495695187,2.556767114,7.22997023301));
#109609=CARTESIAN_POINT('Ctrl Pts',(-1.64720201441,2.491440779,7.31948240044999));
#109610=CARTESIAN_POINT('',(-1.50050161854692,2.49144077849314,7.21972958986675));
#109611=CARTESIAN_POINT('Ctrl Pts',(-1.38356493859898,2.48690656559387,
7.1168108876931));
#109612=CARTESIAN_POINT('Ctrl Pts',(-1.37012131679948,2.48917367229691,
7.11937180234655));
#109613=CARTESIAN_POINT('Ctrl Pts',(-1.356677695,2.491440779,7.121932717));
#109614=CARTESIAN_POINT('Ctrl Pts',(-0.966784777,2.557191576,7.196204554));
#109615=CARTESIAN_POINT('Ctrl Pts',(-0.571114157,2.622066995,7.227470416));
#109616=CARTESIAN_POINT('Ctrl Pts',(-1.18865511346413,2.48690656559387,
7.40579321700299));
#109617=CARTESIAN_POINT('Ctrl Pts',(-1.17466739474133,2.48917367229691,
7.40798415859763));
#109618=CARTESIAN_POINT('Ctrl Pts',(-1.16067967601852,2.491440779,7.41017510019224));
#109619=CARTESIAN_POINT('Ctrl Pts',(-0.755006818633824,2.557191576,7.47371695105929));
#109620=CARTESIAN_POINT('Ctrl Pts',(-0.344821887789227,2.622066995,7.49259435609274));
#109621=CARTESIAN_POINT('',(-1.16108395826105,2.49144077985039,7.40958055924775));
#109622=CARTESIAN_POINT('',(-0.597132064662066,2.58208164077664,7.47619110706454));
#109623=CARTESIAN_POINT('Origin',(0.0421309546760995,2.41074796189775,-0.185224158370121));
#109624=CARTESIAN_POINT('Ctrl Pts',(-0.575811147771544,2.62129679698884,
7.22709772421984));
#109625=CARTESIAN_POINT('Ctrl Pts',(-0.579405185147711,2.61444752745383,
7.26855147446483));
#109626=CARTESIAN_POINT('Ctrl Pts',(-0.582979199524533,2.60775980541408,
7.31005794984184));
#109627=CARTESIAN_POINT('Ctrl Pts',(-0.590083571131229,2.59469807517952,
7.39307656959251));
#109628=CARTESIAN_POINT('Ctrl Pts',(-0.593617782357874,2.58831698274238,
7.43463380158057));
#109629=CARTESIAN_POINT('Ctrl Pts',(-0.597132067174118,2.58208164075448,
7.47619109490713));
#109630=CARTESIAN_POINT('',(-1.25888083740932,2.49144078146678,7.26575663541678));
#109631=CARTESIAN_POINT('Origin',(-1.6554411921138E-14,2.58316965300056,
5.00467722819309E-13));
#109632=CARTESIAN_POINT('',(-0.597654043017649,2.4007463345303,7.47614938614282));
#109633=CARTESIAN_POINT('Origin',(0.0393577243934989,2.55355107526744,-0.186716797871721));
#109634=CARTESIAN_POINT('',(-0.03283023986312,2.49144077881205,7.4999281500093));
#109635=CARTESIAN_POINT('Origin',(0.0137802080897542,2.41071457200419,-0.192386363698522));
#109636=CARTESIAN_POINT('Origin',(0.010801788896734,2.55357128359452,-0.192608996550105));
#109637=CARTESIAN_POINT('Ctrl Pts',(-0.580488539,2.622074631,7.226723535));
#109638=CARTESIAN_POINT('Ctrl Pts',(-0.1877743,2.556767114,7.258268414));
#109639=CARTESIAN_POINT('Ctrl Pts',(0.206045687,2.491440779,7.24707149));
#109640=CARTESIAN_POINT('Ctrl Pts',(-0.845358323000001,2.622074631,7.452205667));
#109641=CARTESIAN_POINT('Ctrl Pts',(-0.440390945,2.556767114,7.498144086));
#109642=CARTESIAN_POINT('Ctrl Pts',(-0.032830234,2.491440779,7.499928145));
#109643=CARTESIAN_POINT('Ctrl Pts',(-0.848007020840001,2.622074631,7.45446048832));
#109644=CARTESIAN_POINT('Ctrl Pts',(-0.44291711145,2.556767114,7.50054284272));
#109645=CARTESIAN_POINT('Ctrl Pts',(-0.03521899321,2.491440779,7.50245671154999));
#109646=CARTESIAN_POINT('',(0.086607723388183,2.49144077849314,7.37349981753655));
#109647=CARTESIAN_POINT('Ctrl Pts',(-1.641068979,3.266573167,7.318257484));
#109648=CARTESIAN_POINT('Ctrl Pts',(-1.244023089,3.330825242,7.407292298));
#109649=CARTESIAN_POINT('Ctrl Pts',(-0.839675095000001,3.395965514,7.452848163));
#109650=CARTESIAN_POINT('Ctrl Pts',(-1.353508207,3.266573167,7.122535752));
#109651=CARTESIAN_POINT('Ctrl Pts',(-0.967081035,3.330825242,7.195969198));
#109652=CARTESIAN_POINT('Ctrl Pts',(-0.574977339,3.395965514,7.227164109));
#109653=CARTESIAN_POINT('',(-0.839675102516549,3.39596551397696,7.45284816193034));
#109654=CARTESIAN_POINT('',(-0.707326224613764,3.39596551522583,7.3400061352663));
#109655=CARTESIAN_POINT('',(-1.39547228497567,3.30628897739669,7.36903366125719));
#109656=CARTESIAN_POINT('Origin',(0.00745224377008552,3.48210502434058,
-0.189556297375185));
#109657=CARTESIAN_POINT('Ctrl Pts',(-1.34892078857225,3.26733592495805,
7.12340597695071));
#109658=CARTESIAN_POINT('Ctrl Pts',(-1.35655738881502,3.27415053067158,
7.16430599565868));
#109659=CARTESIAN_POINT('Ctrl Pts',(-1.36426297460565,3.28079893120748,
7.20524768819475));
#109660=CARTESIAN_POINT('Ctrl Pts',(-1.3797808582022,3.29377261882018,7.28710885345242));
#109661=CARTESIAN_POINT('Ctrl Pts',(-1.38760239032622,3.30010561499173,
7.3280769990597));
#109662=CARTESIAN_POINT('Ctrl Pts',(-1.39547228151228,3.30628897727386,
7.36903366194122));
#109663=CARTESIAN_POINT('Ctrl Pts',(-1.95959162658564,3.39726054241129,
7.23947982964322));
#109664=CARTESIAN_POINT('Ctrl Pts',(-1.95562373629282,3.39661302820565,
7.24054919782161));
#109665=CARTESIAN_POINT('Ctrl Pts',(-1.951655846,3.395965514,7.241618566));
#109666=CARTESIAN_POINT('Ctrl Pts',(-1.832291891,3.376486685,7.273787806));
#109667=CARTESIAN_POINT('Ctrl Pts',(-1.711932572,3.357142857,7.302005674));
#109668=CARTESIAN_POINT('Ctrl Pts',(-1.432141907,3.31217565,7.367601728));
#109669=CARTESIAN_POINT('Ctrl Pts',(-1.148152096,3.266554913,7.411595426));
#109670=CARTESIAN_POINT('Ctrl Pts',(-2.12276066440802,3.39726054241129,
6.93227598202677));
#109671=CARTESIAN_POINT('Ctrl Pts',(-2.11896100170401,3.39661302820565,
6.93343493951338));
#109672=CARTESIAN_POINT('Ctrl Pts',(-2.115161339,3.395965514,6.934593897));
#109673=CARTESIAN_POINT('Ctrl Pts',(-2.000858086,3.376486685,6.969458205));
#109674=CARTESIAN_POINT('Ctrl Pts',(-1.885467899,3.357142857,7.000536465));
#109675=CARTESIAN_POINT('Ctrl Pts',(-1.617228618,3.31217565,7.072781865));
#109676=CARTESIAN_POINT('Ctrl Pts',(-1.344247503,3.266554913,7.124289344));
#109677=CARTESIAN_POINT('',(-1.95165584931786,3.39596551355058,7.24161856620618));
#109678=CARTESIAN_POINT('Ctrl Pts',(-1.39547228792016,3.30628897830869,
7.36903366077302));
#109679=CARTESIAN_POINT('Ctrl Pts',(-1.50164913379404,3.32334891375385,
7.34892697479509));
#109680=CARTESIAN_POINT('Ctrl Pts',(-1.60718233601057,3.34030767936807,
7.3265640420645));
#109681=CARTESIAN_POINT('Ctrl Pts',(-1.71193257096189,3.35714285683316,
7.30200567424338));
#109682=CARTESIAN_POINT('Ctrl Pts',(-1.79202337301739,3.37001483643651,
7.28322863481056));
#109683=CARTESIAN_POINT('Ctrl Pts',(-1.87195374174027,3.38295904433187,
7.26309871975793));
#109684=CARTESIAN_POINT('Ctrl Pts',(-1.95165584885848,3.39596551444773,
7.24161856504488));
#109685=CARTESIAN_POINT('',(-2.03340860029504,3.3959655126796,7.08810622926379));
#109686=CARTESIAN_POINT('Origin',(4.20670442924376E-14,3.48737837500078,
-6.15826833971767E-13));
#109687=CARTESIAN_POINT('',(-1.4027848099639,3.4862983196521,7.36764513069795));
#109688=CARTESIAN_POINT('Origin',(0.0563618769074783,3.62489370122117,-0.177672047855243));
#109689=CARTESIAN_POINT('Origin',(0.0367081618178045,3.48214200415296,-0.189266476659903));
#109690=CARTESIAN_POINT('Ctrl Pts',(-3.175910731,3.266573167,6.794379371));
#109691=CARTESIAN_POINT('Ctrl Pts',(-2.807287406,3.330825242,6.96668573));
#109692=CARTESIAN_POINT('Ctrl Pts',(-2.422186008,3.395965514,7.098099389));
#109693=CARTESIAN_POINT('Ctrl Pts',(-2.852998583,3.266573167,6.66505056900001));
#109694=CARTESIAN_POINT('Ctrl Pts',(-2.491391884,3.330825242,6.819837601));
#109695=CARTESIAN_POINT('Ctrl Pts',(-2.115161339,3.395965514,6.934593897));
#109696=CARTESIAN_POINT('',(-2.42218601520096,3.39596551397697,7.09809938660105));
#109697=CARTESIAN_POINT('',(-2.26867368077813,3.39596551522584,7.01634664064668));
#109698=CARTESIAN_POINT('',(-2.94697132857873,3.30628897732248,6.89676445798204));
#109699=CARTESIAN_POINT('Origin',(0.0480269488321092,3.48210505014218,-0.183522448319748));
#109700=CARTESIAN_POINT('Ctrl Pts',(-2.84870548848616,3.26733592487573,
6.6668866075392));
#109701=CARTESIAN_POINT('Ctrl Pts',(-2.86495564557713,3.27415044722697,
6.70518829485233));
#109702=CARTESIAN_POINT('Ctrl Pts',(-2.88128210332557,3.28079876150916,
6.74351578730517));
#109703=CARTESIAN_POINT('Ctrl Pts',(-2.91403550111338,3.29377268004841,
6.82012856164089));
#109704=CARTESIAN_POINT('Ctrl Pts',(-2.93048128834732,3.30010573966433,
6.85845790751624));
#109705=CARTESIAN_POINT('Ctrl Pts',(-2.94697132493218,3.30628897718608,
6.89676445955767));
#109706=CARTESIAN_POINT('Ctrl Pts',(-3.47005162939067,3.39726054241129,
6.64897053993111));
#109707=CARTESIAN_POINT('Ctrl Pts',(-3.46640638869534,3.39661302820565,
6.65086788596556));
#109708=CARTESIAN_POINT('Ctrl Pts',(-3.462761148,3.395965514,6.652765232));
#109709=CARTESIAN_POINT('Ctrl Pts',(-3.353103291,3.376486685,6.709842094));
#109710=CARTESIAN_POINT('Ctrl Pts',(-3.241623914,3.357142857,6.763273941));
#109711=CARTESIAN_POINT('Ctrl Pts',(-2.982475812,3.31217565,6.887483117));
#109712=CARTESIAN_POINT('Ctrl Pts',(-2.71458287,3.266554913,6.991497682));
#109713=CARTESIAN_POINT('Ctrl Pts',(-3.56336611914593,3.39726054241129,
6.31387242722714));
#109714=CARTESIAN_POINT('Ctrl Pts',(-3.55990443207297,3.39661302820565,
6.31582110411357));
#109715=CARTESIAN_POINT('Ctrl Pts',(-3.556442745,3.395965514,6.317769781));
#109716=CARTESIAN_POINT('Ctrl Pts',(-3.452306635,3.376486685,6.376390802));
#109717=CARTESIAN_POINT('Ctrl Pts',(-3.346295113,3.357142857,6.431547949));
#109718=CARTESIAN_POINT('Ctrl Pts',(-3.099857743,3.31217565,6.55976780700001));
#109719=CARTESIAN_POINT('Ctrl Pts',(-2.84433136,3.266554913,6.66875394));
#109720=CARTESIAN_POINT('',(-3.46276115493587,3.39596551397716,6.65276522825413));
#109721=CARTESIAN_POINT('Ctrl Pts',(-2.94697133156129,3.3062889783089,6.89676445651874));
#109722=CARTESIAN_POINT('Ctrl Pts',(-3.04634347853802,3.32334891375403,
6.85430297046257));
#109723=CARTESIAN_POINT('Ctrl Pts',(-3.14460200356063,3.34030767936782,
6.80977635198074));
#109724=CARTESIAN_POINT('Ctrl Pts',(-3.24162391269816,3.35714285675915,
6.76327394139216));
#109725=CARTESIAN_POINT('Ctrl Pts',(-3.3158057287211,3.37001483655547,6.72771874213896));
#109726=CARTESIAN_POINT('Ctrl Pts',(-3.38954003520254,3.38295904483435,
6.69087678604438));
#109727=CARTESIAN_POINT('Ctrl Pts',(-3.46276115484867,3.39596551520491,
6.652765228235));
#109728=CARTESIAN_POINT('',(-3.50960195363195,3.39596551267963,6.48526750264044));
#109729=CARTESIAN_POINT('Origin',(-2.74736830507827E-13,3.48737837500022,
8.58254439739525E-13));
#109730=CARTESIAN_POINT('',(-2.95381439771736,3.48629831963313,6.89383641367548));
#109731=CARTESIAN_POINT('Origin',(0.093238293760558,3.62489371327987,-0.161401769541824));
#109732=CARTESIAN_POINT('Origin',(0.076536543906639,3.48214199689222,-0.176950158017798));
#109733=CARTESIAN_POINT('Ctrl Pts',(-4.56225042700001,3.266573167,5.952803629));
#109734=CARTESIAN_POINT('Ctrl Pts',(-4.239286085,3.330825242,6.20032467900001));
#109735=CARTESIAN_POINT('Ctrl Pts',(-3.891438196,3.395965514,6.411451378));
#109736=CARTESIAN_POINT('Ctrl Pts',(-4.219085917,3.266573167,5.895915029));
#109737=CARTESIAN_POINT('Ctrl Pts',(-3.899208018,3.330825242,6.124817978));
#109738=CARTESIAN_POINT('Ctrl Pts',(-3.556442745,3.395965514,6.317769781));
#109739=CARTESIAN_POINT('',(-3.89143820237509,3.39596551397697,6.41145137387599));
#109740=CARTESIAN_POINT('',(-3.72394047710203,3.39596551522583,6.36461057563715));
#109741=CARTESIAN_POINT('',(-4.36067326829594,3.306288977333,6.10201021368914));
#109742=CARTESIAN_POINT('Origin',(0.0863561497287396,3.48210502566653,-0.168907609084561));
#109743=CARTESIAN_POINT('Ctrl Pts',(-4.2152878865285,3.26733592487922,5.89863103039522));
#109744=CARTESIAN_POINT('Ctrl Pts',(-4.23939214923398,3.27415053058325,
5.9325443570056));
#109745=CARTESIAN_POINT('Ctrl Pts',(-4.26357651993798,3.28079893111318,
5.96646653943243));
#109746=CARTESIAN_POINT('Ctrl Pts',(-4.31203278075909,3.29377261872553,
6.03424593089019));
#109747=CARTESIAN_POINT('Ctrl Pts',(-4.33633348893587,3.30010561490405,
6.0681434368539));
#109748=CARTESIAN_POINT('Ctrl Pts',(-4.36067326513809,3.3062889771908,6.10201021589449));
#109749=CARTESIAN_POINT('Ctrl Pts',(-4.81825587435657,3.3972605424113,5.74756277776071));
#109750=CARTESIAN_POINT('Ctrl Pts',(-4.81510373067828,3.39661302820565,
5.75019938388036));
#109751=CARTESIAN_POINT('Ctrl Pts',(-4.811951587,3.395965514,5.75283599));
#109752=CARTESIAN_POINT('Ctrl Pts',(-4.717127308,3.376486685,5.832151624));
#109753=CARTESIAN_POINT('Ctrl Pts',(-4.619740525,3.357142857,5.908299035));
#109754=CARTESIAN_POINT('Ctrl Pts',(-4.393352463,3.31217565,6.085313451));
#109755=CARTESIAN_POINT('Ctrl Pts',(-4.154082765,3.266554913,6.244485277));
#109756=CARTESIAN_POINT('Ctrl Pts',(-4.83735253472087,3.3972605424113,5.40023921543882));
#109757=CARTESIAN_POINT('Ctrl Pts',(-4.83439068786043,3.39661302820565,
5.40288649371941));
#109758=CARTESIAN_POINT('Ctrl Pts',(-4.831428841,3.395965514,5.405533772));
#109759=CARTESIAN_POINT('Ctrl Pts',(-4.742329161,3.376486685,5.485170451));
#109760=CARTESIAN_POINT('Ctrl Pts',(-4.650653287,3.357142857,5.561827398));
#109761=CARTESIAN_POINT('Ctrl Pts',(-4.437540965,3.31217565,5.740026298));
#109762=CARTESIAN_POINT('Ctrl Pts',(-4.211417444,3.266554913,5.901395014));
#109763=CARTESIAN_POINT('',(-4.81195159120568,3.39596551354713,5.7528359871114));
#109764=CARTESIAN_POINT('Ctrl Pts',(-4.36067327090021,3.30628897830886,
6.10201021177672));
#109765=CARTESIAN_POINT('Ctrl Pts',(-4.44859418812871,3.32334891375399,
6.03917937748522));
#109766=CARTESIAN_POINT('Ctrl Pts',(-4.5349835767243,3.34030767936764,5.9745710882284));
#109767=CARTESIAN_POINT('Ctrl Pts',(-4.61974052367493,3.3571428567285,5.90829903560032));
#109768=CARTESIAN_POINT('Ctrl Pts',(-4.68454469282505,3.37001483650127,
5.85762819936046));
#109769=CARTESIAN_POINT('Ctrl Pts',(-4.74863520074109,3.3829590448342,5.80579689162175));
#109770=CARTESIAN_POINT('Ctrl Pts',(-4.81195159287912,3.39596551520488,
5.75283598485012));
#109771=CARTESIAN_POINT('',(-4.82169022013556,3.39596551267962,5.57918487569748));
#109772=CARTESIAN_POINT('Origin',(-3.33283747822044E-13,3.48737837499933,
3.5301622736128E-13));
#109773=CARTESIAN_POINT('',(-4.36672690753549,3.48629831964532,6.09767956787773));
#109774=CARTESIAN_POINT('Origin',(0.125755312071149,3.62489371866856,-0.137585200598519));
#109775=CARTESIAN_POINT('Origin',(0.112786245811037,3.48214197539546,-0.156360099239026));
#109776=CARTESIAN_POINT('Ctrl Pts',(-5.735264364,3.266573167,4.832881405));
#109777=CARTESIAN_POINT('Ctrl Pts',(-5.473060458,3.330825242,5.144043338));
#109778=CARTESIAN_POINT('Ctrl Pts',(-5.178731058,3.395965514,5.425011025));
#109779=CARTESIAN_POINT('Ctrl Pts',(-5.387893482,3.266573167,4.851093055));
#109780=CARTESIAN_POINT('Ctrl Pts',(-5.124701518,3.330825242,5.143408673));
#109781=CARTESIAN_POINT('Ctrl Pts',(-4.831428841,3.395965514,5.40553377200001));
#109782=CARTESIAN_POINT('',(-5.17873106354357,3.39596551397697,5.42501101981538));
#109783=CARTESIAN_POINT('',(-5.00507995511728,3.39596551522583,5.41527239330822));
#109784=CARTESIAN_POINT('',(-5.57047497242684,3.30628897733851,5.02193275359628));
#109785=CARTESIAN_POINT('Origin',(0.120647090505832,3.4821050288845,-0.146394402571267));
#109786=CARTESIAN_POINT('Ctrl Pts',(-5.38476810741094,3.26733592498887,
4.85456202254788));
#109787=CARTESIAN_POINT('Ctrl Pts',(-5.41559918872214,3.27415053066729,
4.88250077028925));
#109788=CARTESIAN_POINT('Ctrl Pts',(-5.44651040880628,3.28079893117115,
4.91043094599988));
#109789=CARTESIAN_POINT('Ctrl Pts',(-5.50840435484866,3.2937726187527,4.96620902910849));
#109790=CARTESIAN_POINT('Ctrl Pts',(-5.5394238877264,3.30010561491808,4.99409009625292));
#109791=CARTESIAN_POINT('Ctrl Pts',(-5.57047496986067,3.30628897720077,
5.02193275641807));
#109792=CARTESIAN_POINT('Ctrl Pts',(-5.9411638298455,3.3972605424113,4.5774053670745));
#109793=CARTESIAN_POINT('Ctrl Pts',(-5.93865217392275,3.39661302820565,
4.58065794853726));
#109794=CARTESIAN_POINT('Ctrl Pts',(-5.936140518,3.395965514,4.58391053));
#109795=CARTESIAN_POINT('Ctrl Pts',(-5.860583695,3.376486685,4.681756226));
#109796=CARTESIAN_POINT('Ctrl Pts',(-5.781843203,3.357142857,4.777058632));
#109797=CARTESIAN_POINT('Ctrl Pts',(-5.598800835,3.31217565,4.998601291));
#109798=CARTESIAN_POINT('Ctrl Pts',(-5.39934236800001,3.266554913,5.205487681));
#109799=CARTESIAN_POINT('Ctrl Pts',(-5.88514972182881,3.3972605424113,4.23409681912444));
#109800=CARTESIAN_POINT('Ctrl Pts',(-5.88282620791441,3.39661302820565,
4.23731891506222));
#109801=CARTESIAN_POINT('Ctrl Pts',(-5.880502694,3.395965514,4.240541011));
#109802=CARTESIAN_POINT('Ctrl Pts',(-5.810605648,3.376486685,4.337469627));
#109803=CARTESIAN_POINT('Ctrl Pts',(-5.737552082,3.357142857,4.43204198));
#109804=CARTESIAN_POINT('Ctrl Pts',(-5.567729703,3.31217565,4.651887538));
#109805=CARTESIAN_POINT('Ctrl Pts',(-5.381582328,3.266554913,4.858093417));
#109806=CARTESIAN_POINT('',(-5.93614052278745,3.39596551397716,4.58391052373854));
#109807=CARTESIAN_POINT('Ctrl Pts',(-5.57047497456071,3.3062889783089,5.02193275120465));
#109808=CARTESIAN_POINT('Ctrl Pts',(-5.64283357730374,3.32334891375403,
4.94167046845604));
#109809=CARTESIAN_POINT('Ctrl Pts',(-5.71331435752237,3.34030767936776,
4.86000152005898));
#109810=CARTESIAN_POINT('Ctrl Pts',(-5.78184320195352,3.3571428567475,4.77705863309879));
#109811=CARTESIAN_POINT('Ctrl Pts',(-5.83423955398265,3.37001483653487,
4.71364147256023));
#109812=CARTESIAN_POINT('Ctrl Pts',(-5.88568946219912,3.38295904483425,
4.64924438689859));
#109813=CARTESIAN_POINT('Ctrl Pts',(-5.93614052263486,3.39596551520492,
4.58391052370727));
#109814=CARTESIAN_POINT('',(-5.90832161085222,3.39596551267962,4.41222576400249));
#109815=CARTESIAN_POINT('Origin',(1.10415149245924E-12,3.48737837500033,
-1.05644659686988E-12));
#109816=CARTESIAN_POINT('',(-5.5754561197949,3.48629831964252,5.01640200242548));
#109817=CARTESIAN_POINT('Origin',(0.152391677636978,3.62489374132545,-0.107334577125267));
#109818=CARTESIAN_POINT('Origin',(0.143762229393116,3.48214198317769,-0.128458831607123));
#109819=CARTESIAN_POINT('Ctrl Pts',(-6.640103713,3.266573167,3.486979019));
#109820=CARTESIAN_POINT('Ctrl Pts',(-6.450920607,3.330825242,3.847232247));
#109821=CARTESIAN_POINT('Ctrl Pts',(-6.223872212,3.395965514,4.184903187));
#109822=CARTESIAN_POINT('Ctrl Pts',(-6.304769136,3.266573167,3.579439362));
#109823=CARTESIAN_POINT('Ctrl Pts',(-6.110569671,3.330825242,3.921499296));
#109824=CARTESIAN_POINT('Ctrl Pts',(-5.880502694,3.395965514,4.240541011));
#109825=CARTESIAN_POINT('',(-6.22387221623639,3.39596551397697,4.1849031807028));
#109826=CARTESIAN_POINT('',(-6.05218745736987,3.39596551522583,4.21272209272205));
#109827=CARTESIAN_POINT('',(-6.51980745789167,3.3062889773493,3.70703529982725));
#109828=CARTESIAN_POINT('Origin',(0.149296895945722,3.48210497061754,-0.117036208815399));
#109829=CARTESIAN_POINT('Ctrl Pts',(-6.30246255588907,3.26733592487402,
3.58349908979831));
#109830=CARTESIAN_POINT('Ctrl Pts',(-6.33857882863868,3.27415053057877,
3.60415687415245));
#109831=CARTESIAN_POINT('Ctrl Pts',(-6.37477152392552,3.28079893112066,
3.62478905937302));
#109832=CARTESIAN_POINT('Ctrl Pts',(-6.4472090632051,3.29377261874503,3.66595771307224));
#109833=CARTESIAN_POINT('Ctrl Pts',(-6.48349698199461,3.30010561492302,
3.68651865366252));
#109834=CARTESIAN_POINT('Ctrl Pts',(-6.51980745608699,3.30628897722029,
3.70703530306007));
#109835=CARTESIAN_POINT('Ctrl Pts',(-6.78626956786007,3.3972605424113,3.19321356957691));
#109836=CARTESIAN_POINT('Ctrl Pts',(-6.78451584193003,3.39661302820565,
3.19693003928845));
#109837=CARTESIAN_POINT('Ctrl Pts',(-6.78276211600001,3.395965514,3.200646509));
#109838=CARTESIAN_POINT('Ctrl Pts',(-6.730005702,3.376486685,3.312447111));
#109839=CARTESIAN_POINT('Ctrl Pts',(-6.673593319,3.357142857,3.422448278));
#109840=CARTESIAN_POINT('Ctrl Pts',(-6.542455503,3.31217565,3.678160091));
#109841=CARTESIAN_POINT('Ctrl Pts',(-6.392134722,3.266554913,3.923087266));
#109842=CARTESIAN_POINT('Ctrl Pts',(-6.65776384915911,3.3972605424113,2.86997276216926));
#109843=CARTESIAN_POINT('Ctrl Pts',(-6.65618731307956,3.39661302820565,
2.87361901408463));
#109844=CARTESIAN_POINT('Ctrl Pts',(-6.65461077700001,3.395965514,2.877265266));
#109845=CARTESIAN_POINT('Ctrl Pts',(-6.60718467200001,3.376486685,2.986953543));
#109846=CARTESIAN_POINT('Ctrl Pts',(-6.556169318,3.357142857,3.095019205));
#109847=CARTESIAN_POINT('Ctrl Pts',(-6.437577588,3.31217565,3.346231687));
#109848=CARTESIAN_POINT('Ctrl Pts',(-6.300110404,3.266554913,3.58763277));
#109849=CARTESIAN_POINT('',(-6.78276211930252,3.39596551397715,3.20064650184279));
#109850=CARTESIAN_POINT('Ctrl Pts',(-6.51980745952236,3.30628897830886,
3.70703529715327));
#109851=CARTESIAN_POINT('Ctrl Pts',(-6.57322034014727,3.32334891375399,
3.61309454144891));
#109852=CARTESIAN_POINT('Ctrl Pts',(-6.62449690909045,3.34030767936783,
3.5181836834444));
#109853=CARTESIAN_POINT('Ctrl Pts',(-6.67359331829069,3.35714285676664,
3.4224482792469));
#109854=CARTESIAN_POINT('Ctrl Pts',(-6.71113185794451,3.3700148365687,3.34925010973637));
#109855=CARTESIAN_POINT('Ctrl Pts',(-6.74753542590834,3.38295904483419,
3.27529838263715));
#109856=CARTESIAN_POINT('Ctrl Pts',(-6.78276211917339,3.39596551520488,
3.20064650185762));
#109857=CARTESIAN_POINT('',(-6.71868644984201,3.39596551267962,3.03895588011132));
#109858=CARTESIAN_POINT('Origin',(-2.38090797077817E-13,3.48737837499967,
5.50774703622636E-14));
#109859=CARTESIAN_POINT('',(-6.52348320100086,3.48629831963772,3.7005630546879));
#109860=CARTESIAN_POINT('Origin',(0.171902718338477,3.62489370565627,-0.0720655235974765));
#109861=CARTESIAN_POINT('Origin',(0.168016080065133,3.48214198897817,-0.0945509470315842));
#109862=CARTESIAN_POINT('Ctrl Pts',(-7.23445919300001,3.266573167,1.978029369));
#109863=CARTESIAN_POINT('Ctrl Pts',(-7.127142877,3.330825242,2.370528853));
#109864=CARTESIAN_POINT('Ctrl Pts',(-6.97799201900001,3.395965514,2.749113927));
#109865=CARTESIAN_POINT('Ctrl Pts',(-6.926840792,3.266573167,2.140415062));
#109866=CARTESIAN_POINT('Ctrl Pts',(-6.810714378,3.330825242,2.516224969));
#109867=CARTESIAN_POINT('Ctrl Pts',(-6.654610777,3.395965514,2.877265266));
#109868=CARTESIAN_POINT('',(-6.97799202168079,3.39596551397697,2.74911391989859));
#109869=CARTESIAN_POINT('',(-6.81630140091813,3.39596551522583,2.81318958942943));
#109870=CARTESIAN_POINT('',(-7.16428099291218,3.30628897730615,2.21880099504165));
#109871=CARTESIAN_POINT('Origin',(0.170965953034417,3.48210502415779,-0.0822056236155499));
#109872=CARTESIAN_POINT('Ctrl Pts',(-6.92546086104984,3.26733592499053,
2.14487572213753));
#109873=CARTESIAN_POINT('Ctrl Pts',(-6.96517356826331,3.27415053065529,
2.15728660792526));
#109874=CARTESIAN_POINT('Ctrl Pts',(-7.00495540816731,3.28079893115101,
2.16965606448942));
#109875=CARTESIAN_POINT('Ctrl Pts',(-7.08454944149771,3.29377261873339,
2.19429028833485));
#109876=CARTESIAN_POINT('Ctrl Pts',(-7.12440896325153,3.30010561488432,
2.20656969571793));
#109877=CARTESIAN_POINT('Ctrl Pts',(-7.16428099180961,3.30628897717171,
2.21880099870381));
#109878=CARTESIAN_POINT('Ctrl Pts',(-7.3140568833428,3.39726054241129,1.65971065413928));
#109879=CARTESIAN_POINT('Ctrl Pts',(-7.31314308967141,3.39661302820565,
1.66371723406964));
#109880=CARTESIAN_POINT('Ctrl Pts',(-7.312229296,3.395965514,1.667723814));
#109881=CARTESIAN_POINT('Ctrl Pts',(-7.284740122,3.376486685,1.788251649));
#109882=CARTESIAN_POINT('Ctrl Pts',(-7.253293629,3.357142857,1.907808045));
#109883=CARTESIAN_POINT('Ctrl Pts',(-7.180192223,3.31217565,2.185732212));
#109884=CARTESIAN_POINT('Ctrl Pts',(-7.086037961,3.266554913,2.457247651));
#109885=CARTESIAN_POINT('Ctrl Pts',(-7.11906833833695,3.39726054241129,
1.37165196852683));
#109886=CARTESIAN_POINT('Ctrl Pts',(-7.11831249716847,3.39661302820565,
1.37555188176341));
#109887=CARTESIAN_POINT('Ctrl Pts',(-7.117556656,3.395965514,1.379451795));
#109888=CARTESIAN_POINT('Ctrl Pts',(-7.094819084,3.376486685,1.496770832));
#109889=CARTESIAN_POINT('Ctrl Pts',(-7.068227363,3.357142857,1.613276771));
#109890=CARTESIAN_POINT('Ctrl Pts',(-7.006411501,3.31217565,1.884109762));
#109891=CARTESIAN_POINT('Ctrl Pts',(-6.92405232,3.266554913,2.149418403));
#109892=CARTESIAN_POINT('',(-7.31222929770336,3.39596551397716,1.6677238063043));
#109893=CARTESIAN_POINT('Ctrl Pts',(-7.16428099403738,3.30628897830889,
2.21880099199275));
#109894=CARTESIAN_POINT('Ctrl Pts',(-7.19625062562276,3.32334891375402,
2.11557432831844));
#109895=CARTESIAN_POINT('Ctrl Pts',(-7.22592534802315,3.3403076793677,2.01185948673362));
#109896=CARTESIAN_POINT('Ctrl Pts',(-7.25329362833298,3.35714285673703,
1.90780804624414));
#109897=CARTESIAN_POINT('Ctrl Pts',(-7.27421909452139,3.37001483651634,
1.82825153253987));
#109898=CARTESIAN_POINT('Ctrl Pts',(-7.29387413230536,3.38295904483434,
1.74820306499536));
#109899=CARTESIAN_POINT('Ctrl Pts',(-7.31222929756424,3.39596551520491,
1.66772380634285));
#109900=CARTESIAN_POINT('',(-7.21489297767553,3.39596551267961,1.52358779656558));
#109901=CARTESIAN_POINT('Origin',(4.46257614195034E-13,3.48737837499967,
-1.83555427801796E-13));
#109902=CARTESIAN_POINT('',(-7.16647945764019,3.48629831962515,2.21168989156009));
#109903=CARTESIAN_POINT('Origin',(0.183375927394167,3.62489371453121,-0.0334267439120248));
#109904=CARTESIAN_POINT('Origin',(0.184413422376409,3.48214204626776,-0.0562218677092333));
#109905=CARTESIAN_POINT('Ctrl Pts',(-7.490539402,3.266573167,0.376589264));
#109906=CARTESIAN_POINT('Ctrl Pts',(-7.470107869,3.330825242,0.782982164));
#109907=CARTESIAN_POINT('Ctrl Pts',(-7.405828674,3.395965514,1.184779155));
#109908=CARTESIAN_POINT('Ctrl Pts',(-7.225021072,3.266573167,0.601307333));
#109909=CARTESIAN_POINT('Ctrl Pts',(-7.19239765,3.330825242,0.993294759999999));
#109910=CARTESIAN_POINT('Ctrl Pts',(-7.117556656,3.395965514,1.379451795));
#109911=CARTESIAN_POINT('',(-7.40582867522515,3.39596551397696,1.1847791475097));
#109912=CARTESIAN_POINT('',(-7.26169266632994,3.39596551522583,1.28211546746747));
#109913=CARTESIAN_POINT('',(-7.47376071103804,3.30628897732951,0.626818022433091));
#109914=CARTESIAN_POINT('Origin',(0.184640406146561,3.48210501342017,-0.0435310537882508));
#109915=CARTESIAN_POINT('Ctrl Pts',(-7.22463231302281,3.26733592498612,
0.605960349825525));
#109916=CARTESIAN_POINT('Ctrl Pts',(-7.26608453277289,3.2741505306695,0.609544017994957));
#109917=CARTESIAN_POINT('Ctrl Pts',(-7.30759536288584,3.28079893118097,
0.613072364018514));
#109918=CARTESIAN_POINT('Ctrl Pts',(-7.39062455165567,3.29377267969189,
0.620020321807375));
#109919=CARTESIAN_POINT('Ctrl Pts',(-7.43219233249536,3.30010573881294,
0.623444059561667));
#109920=CARTESIAN_POINT('Ctrl Pts',(-7.47376071072472,3.30628897719416,
0.626818026364407));
#109921=CARTESIAN_POINT('Ctrl Pts',(-7.49984702782103,3.3972605424113,0.0486015141103514));
#109922=CARTESIAN_POINT('Ctrl Pts',(-7.49981589441051,3.39661302820565,
0.0527108610551757));
#109923=CARTESIAN_POINT('Ctrl Pts',(-7.499784761,3.395965514,0.056820208));
#109924=CARTESIAN_POINT('Ctrl Pts',(-7.498848191,3.376486685,0.180439529));
#109925=CARTESIAN_POINT('Ctrl Pts',(-7.49383799,3.357142857,0.303960829));
#109926=CARTESIAN_POINT('Ctrl Pts',(-7.482191134,3.31217565,0.591101925));
#109927=CARTESIAN_POINT('Ctrl Pts',(-7.44860594,3.266554913,0.876509867));
#109928=CARTESIAN_POINT('Ctrl Pts',(-7.24749310390195,3.3972605424113,-0.190805746883935));
#109929=CARTESIAN_POINT('Ctrl Pts',(-7.24759329995098,3.39661302820565,
-0.186834527941968));
#109930=CARTESIAN_POINT('Ctrl Pts',(-7.247693496,3.395965514,-0.182863309));
#109931=CARTESIAN_POINT('Ctrl Pts',(-7.250707641,3.376486685,-0.06339922));
#109932=CARTESIAN_POINT('Ctrl Pts',(-7.249782953,3.357142857,0.056099309));
#109933=CARTESIAN_POINT('Ctrl Pts',(-7.247633398,3.31217565,0.333888958));
#109934=CARTESIAN_POINT('Ctrl Pts',(-7.224233245,3.266554913,0.61069962));
#109935=CARTESIAN_POINT('',(-7.49978476208606,3.39596551355058,0.0568202048562634));
#109936=CARTESIAN_POINT('Ctrl Pts',(-7.47376071114191,3.30628897830889,
0.626818019136488));
#109937=CARTESIAN_POINT('Ctrl Pts',(-7.48279222925345,3.32334891375402,
0.519132211709427));
#109938=CARTESIAN_POINT('Ctrl Pts',(-7.48947754816551,3.34030767936767,
0.411462977315972));
#109939=CARTESIAN_POINT('Ctrl Pts',(-7.49383798972126,3.35714285673008,
0.303960830511502));
#109940=CARTESIAN_POINT('Ctrl Pts',(-7.497171931789,3.37001483625442,0.221765949147783));
#109941=CARTESIAN_POINT('Ctrl Pts',(-7.49915939119715,3.38295904433211,
0.139363719624729));
#109942=CARTESIAN_POINT('Ctrl Pts',(-7.49978476084517,3.39596551444813,
0.0568202049882929));
#109943=CARTESIAN_POINT('',(-7.37373912843069,3.3959655126796,-0.0630215586091557));
#109944=CARTESIAN_POINT('Origin',(1.33270131041918E-12,3.48737837500044,
-9.09103521629095E-14));
#109945=CARTESIAN_POINT('',(-7.47437910004273,3.48629831962699,0.619400567520625));
#109946=CARTESIAN_POINT('Origin',(0.186274213854775,3.62489373218069,0.00677518458523894));
#109947=CARTESIAN_POINT('Origin',(0.19218808190701,3.48214199745557,-0.0152639929471668));
#109948=CARTESIAN_POINT('Ctrl Pts',(-7.396370313,3.266573167,-1.242459737));
#109949=CARTESIAN_POINT('Ctrl Pts',(-7.463778918,3.330825242,-0.841175901));
#109950=CARTESIAN_POINT('Ctrl Pts',(-7.487377012,3.395965514,-0.434954574));
#109951=CARTESIAN_POINT('Ctrl Pts',(-7.185367396,3.266573167,-0.965916859000001));
#109952=CARTESIAN_POINT('Ctrl Pts',(-7.237772401,3.330825242,-0.576080809));
#109953=CARTESIAN_POINT('Ctrl Pts',(-7.247693496,3.395965514,-0.182863309));
#109954=CARTESIAN_POINT('',(-7.48737701144181,3.39596551397696,-0.434954581569916));
#109955=CARTESIAN_POINT('',(-7.36753525367957,3.39596551522583,-0.30890894914232));
#109956=CARTESIAN_POINT('',(-7.43377568527516,3.30628897737924,-0.994474264932722));
#109957=CARTESIAN_POINT('Origin',(0.189681805221984,3.48210505004052,-0.00282106332404317));
#109958=CARTESIAN_POINT('Ctrl Pts',(-7.18598798705034,3.2673359249808,-0.961289055455298));
#109959=CARTESIAN_POINT('Ctrl Pts',(-7.22724145968924,3.27415053066413,
-0.966700173467491));
#109960=CARTESIAN_POINT('Ctrl Pts',(-7.26854027983182,3.28079893118089,
-0.972177919707717));
#109961=CARTESIAN_POINT('Ctrl Pts',(-7.35112151021921,3.29377261878279,
-0.983241170704317));
#109962=CARTESIAN_POINT('Ctrl Pts',(-7.39245302187789,3.30010561495841,
-0.988833261135669));
#109963=CARTESIAN_POINT('Ctrl Pts',(-7.43377568577855,3.30628897725429,
-0.994474261382158));
#109964=CARTESIAN_POINT('Ctrl Pts',(-7.33495266083656,3.3972605424113,-1.5647801799305));
#109965=CARTESIAN_POINT('Ctrl Pts',(-7.33580564341827,3.39661302820565,
-1.56076021446525));
#109966=CARTESIAN_POINT('Ctrl Pts',(-7.33665862600001,3.395965514,-1.556740249));
#109967=CARTESIAN_POINT('Ctrl Pts',(-7.362318452,3.376486685,-1.435809744));
#109968=CARTESIAN_POINT('Ctrl Pts',(-7.383978815,3.357142857,-1.314099258));
#109969=CARTESIAN_POINT('Ctrl Pts',(-7.43433110500001,3.31217565,-1.031167631));
#109970=CARTESIAN_POINT('Ctrl Pts',(-7.462885385,3.266554913,-0.745212545));
#109971=CARTESIAN_POINT('Ctrl Pts',(-7.03703314764056,3.3972605424113,-1.74434159666193));
#109972=CARTESIAN_POINT('Ctrl Pts',(-7.03798469582028,3.39661302820565,
-1.74048476183097));
#109973=CARTESIAN_POINT('Ctrl Pts',(-7.038936244,3.395965514,-1.736627927));
#109974=CARTESIAN_POINT('Ctrl Pts',(-7.067561167,3.376486685,-1.620604795));
#109975=CARTESIAN_POINT('Ctrl Pts',(-7.09234675,3.357142857,-1.503701295));
#109976=CARTESIAN_POINT('Ctrl Pts',(-7.149964013,3.31217565,-1.231944122));
#109977=CARTESIAN_POINT('Ctrl Pts',(-7.18661705200001,3.266554913,-0.956574799));
#109978=CARTESIAN_POINT('',(-7.33665862544624,3.39596551354713,-1.55674025405169));
#109979=CARTESIAN_POINT('Ctrl Pts',(-7.43377568496655,3.30628897830885,
-0.994474267950553));
#109980=CARTESIAN_POINT('Ctrl Pts',(-7.4194467856062,3.32334891375399,-1.1015839503658));
#109981=CARTESIAN_POINT('Ctrl Pts',(-7.40283010245738,3.34030767936774,
-1.20817308388293));
#109982=CARTESIAN_POINT('Ctrl Pts',(-7.38397881522136,3.3571428567508,-1.31409925646954));
#109983=CARTESIAN_POINT('Ctrl Pts',(-7.36956534156352,3.3700148365407,-1.39508916791251));
#109984=CARTESIAN_POINT('Ctrl Pts',(-7.35379229118658,3.3829590448342,-1.4759921258145));
#109985=CARTESIAN_POINT('Ctrl Pts',(-7.33665862420373,3.39596551520488,
-1.55674025660656));
#109986=CARTESIAN_POINT('',(-7.18779743318909,3.3959655126796,-1.64668409590467));
#109987=CARTESIAN_POINT('Origin',(-8.54351311918577E-14,3.48737837500022,
1.29291109068896E-14));
#109988=CARTESIAN_POINT('',(-7.4327850829995,3.4862983196318,-1.00185123922132));
#109989=CARTESIAN_POINT('Origin',(0.18046278988964,3.62489369570797,0.0466602352497604));
#109990=CARTESIAN_POINT('Origin',(0.190975911410668,3.48214202383925,0.0264075856926274));
#109991=CARTESIAN_POINT('Ctrl Pts',(-6.956355169,3.266573167,-2.8034127));
#109992=CARTESIAN_POINT('Ctrl Pts',(-7.108451961,3.330825242,-2.426001516));
#109993=CARTESIAN_POINT('Ctrl Pts',(-7.218823922,3.395965514,-2.03435031));
#109994=CARTESIAN_POINT('Ctrl Pts',(-6.80973392700001,3.266573167,-2.487975852));
#109995=CARTESIAN_POINT('Ctrl Pts',(-6.94471696,3.330825242,-2.118519479));
#109996=CARTESIAN_POINT('Ctrl Pts',(-7.03893624400001,3.395965514,-1.736627927));
#109997=CARTESIAN_POINT('',(-7.21882391984119,3.39596551397696,-2.03435031727704));
#109998=CARTESIAN_POINT('',(-7.12888008104419,3.39596551522583,-1.88548912589476));
#109999=CARTESIAN_POINT('',(-7.04619557022418,3.3062889773588,-2.56926604054269));
#110000=CARTESIAN_POINT('Origin',(0.185853545006802,3.48210500655179,0.0380208618339362));
#110001=CARTESIAN_POINT('Ctrl Pts',(-6.81133485030236,3.26733592504445,
-2.48358965276559));
#110002=CARTESIAN_POINT('Ctrl Pts',(-6.85046060920791,3.27415053069601,
-2.49774253882626));
#110003=CARTESIAN_POINT('Ctrl Pts',(-6.88961633227399,3.28079893118911,
-2.51197024378488));
#110004=CARTESIAN_POINT('Ctrl Pts',(-6.96788858726607,3.29377261876151,
-2.54052736533596));
#110005=CARTESIAN_POINT('Ctrl Pts',(-7.00705165692539,3.3001056149326,-2.55487376898962));
#110006=CARTESIAN_POINT('Ctrl Pts',(-7.04619557146458,3.30628897721914,
-2.56926603699822));
#110007=CARTESIAN_POINT('Ctrl Pts',(-6.82708405989074,3.39726054241129,
-3.1049944917374));
#110008=CARTESIAN_POINT('Ctrl Pts',(-6.82878127394537,3.39661302820565,
-3.1012518768687));
#110009=CARTESIAN_POINT('Ctrl Pts',(-6.830478488,3.395965514,-3.097509262));
#110010=CARTESIAN_POINT('Ctrl Pts',(-6.881534885,3.376486685,-2.984922149));
#110011=CARTESIAN_POINT('Ctrl Pts',(-6.928852998,3.357142857,-2.870713524));
#110012=CARTESIAN_POINT('Ctrl Pts',(-7.038850015,3.31217565,-2.605220935));
#110013=CARTESIAN_POINT('Ctrl Pts',(-7.128208603,3.266554913,-2.332089646));
#110014=CARTESIAN_POINT('Ctrl Pts',(-6.49752934201089,3.39726054241129,
-3.21631397286633));
#110015=CARTESIAN_POINT('Ctrl Pts',(-6.49928774900545,3.39661302820565,
-3.21275186343316));
#110016=CARTESIAN_POINT('Ctrl Pts',(-6.501046156,3.395965514,-3.209189754));
#110017=CARTESIAN_POINT('Ctrl Pts',(-6.553943388,3.376486685,-3.102032691));
#110018=CARTESIAN_POINT('Ctrl Pts',(-6.603280295,3.357142857,-2.993190497));
#110019=CARTESIAN_POINT('Ctrl Pts',(-6.71797025700001,3.31217565,-2.740172865));
#110020=CARTESIAN_POINT('Ctrl Pts',(-6.812962634,3.266554913,-2.479120843));
#110021=CARTESIAN_POINT('',(-6.83047848634386,3.39596551354713,-3.09750926682452));
#110022=CARTESIAN_POINT('Ctrl Pts',(-7.04619556909987,3.30628897830889,
-2.56926604348342));
#110023=CARTESIAN_POINT('Ctrl Pts',(-7.0091762559016,3.32334891375402,-2.67079127129904));
#110024=CARTESIAN_POINT('Ctrl Pts',(-6.97003454879645,3.34030767936774,
-2.77131631447829));
#110025=CARTESIAN_POINT('Ctrl Pts',(-6.92885299822154,3.35714285674388,
-2.87071352264016));
#110026=CARTESIAN_POINT('Ctrl Pts',(-6.89736606607387,3.37001483652846,
-2.94671146444352));
#110027=CARTESIAN_POINT('Ctrl Pts',(-6.86457003692198,3.38295904483433,
-3.02233221654559));
#110028=CARTESIAN_POINT('Ctrl Pts',(-6.83047848461137,3.39596551520491,
-3.09750926904244));
#110029=CARTESIAN_POINT('',(-6.66576231853218,3.39596551267961,-3.15334951533053));
#110030=CARTESIAN_POINT('Origin',(2.94902990916057E-14,3.48737837499956,
5.46437894932694E-14));
#110031=CARTESIAN_POINT('',(-7.04364229628584,3.48629831963653,-2.57625759529346));
#110032=CARTESIAN_POINT('Origin',(0.166213305170159,3.62489367230267,0.0843635729055464));
#110033=CARTESIAN_POINT('Origin',(0.180834155856733,3.48214200407374,0.0668443663325308));
#110034=CARTESIAN_POINT('Ctrl Pts',(-6.191068588,3.266573167,-4.233281202));
#110035=CARTESIAN_POINT('Ctrl Pts',(-6.420741691,3.330825242,-3.897389996));
#110036=CARTESIAN_POINT('Ctrl Pts',(-6.61272664900001,3.395965514,-3.538622086));
#110037=CARTESIAN_POINT('Ctrl Pts',(-6.115684868,3.266573167,-3.893699859));
#110038=CARTESIAN_POINT('Ctrl Pts',(-6.326934271,3.330825242,-3.561898533));
#110039=CARTESIAN_POINT('Ctrl Pts',(-6.501046156,3.395965514,-3.209189754));
#110040=CARTESIAN_POINT('',(-6.6127266453021,3.39596551397696,-3.5386220926291));
#110041=CARTESIAN_POINT('',(-6.55688639900026,3.39596551522583,-3.37390592680144));
#110042=CARTESIAN_POINT('',(-6.32914318155958,3.3062889773532,-4.02392179185992));
#110043=CARTESIAN_POINT('Origin',(0.173334860569169,3.48210500429325,0.0770848768754384));
#110044=CARTESIAN_POINT('Ctrl Pts',(-6.11819126530476,3.2673359249502,-3.88976035761938));
#110045=CARTESIAN_POINT('Ctrl Pts',(-6.15335983356358,3.27415053064474,
-3.91199323889897));
#110046=CARTESIAN_POINT('Ctrl Pts',(-6.18854158161075,3.28079893116152,
-3.93430563116583));
#110047=CARTESIAN_POINT('Ctrl Pts',(-6.25884493789794,3.29377261876225,
-3.9790213243313));
#110048=CARTESIAN_POINT('Ctrl Pts',(-6.29400834408267,3.30010561492991,
-4.00145121935033));
#110049=CARTESIAN_POINT('Ctrl Pts',(-6.32914318354082,3.30628897721165,
-4.02392178863842));
#110050=CARTESIAN_POINT('Ctrl Pts',(-5.99998859553901,3.39726054241129,
-4.50002271153911));
#110051=CARTESIAN_POINT('Ctrl Pts',(-6.00245068126951,3.39661302820565,
-4.49673244776956));
#110052=CARTESIAN_POINT('Ctrl Pts',(-6.004912767,3.395965514,-4.493442184));
#110053=CARTESIAN_POINT('Ctrl Pts',(-6.078978396,3.376486685,-4.394462911));
#110054=CARTESIAN_POINT('Ctrl Pts',(-6.149741715,3.357142857,-4.293096416));
#110055=CARTESIAN_POINT('Ctrl Pts',(-6.314240122,3.31217565,-4.057457004));
#110056=CARTESIAN_POINT('Ctrl Pts',(-6.460224709,3.266554913,-3.809920827));
#110057=CARTESIAN_POINT('Ctrl Pts',(-5.65420828564301,3.39726054241129,
-4.5378950825258));
#110058=CARTESIAN_POINT('Ctrl Pts',(-5.65669133032151,3.39661302820565,
-4.5347942587629));
#110059=CARTESIAN_POINT('Ctrl Pts',(-5.659174375,3.395965514,-4.53169343500001));
#110060=CARTESIAN_POINT('Ctrl Pts',(-5.733870501,3.376486685,-4.438412986));
#110061=CARTESIAN_POINT('Ctrl Pts',(-5.805451792,3.357142857,-4.342721438));
#110062=CARTESIAN_POINT('Ctrl Pts',(-5.971851679,3.31217565,-4.12027417));
#110063=CARTESIAN_POINT('Ctrl Pts',(-6.120741654,3.266554913,-3.885745952));
#110064=CARTESIAN_POINT('',(-6.00491276436094,3.39596551354713,-4.49344218835395));
#110065=CARTESIAN_POINT('Ctrl Pts',(-6.32914317981192,3.30628897830886,
-4.02392179450353));
#110066=CARTESIAN_POINT('Ctrl Pts',(-6.2711644346662,3.32334891375399,-4.11511536091147));
#110067=CARTESIAN_POINT('Ctrl Pts',(-6.21132792606103,3.3403076793678,-4.20487587433852));
#110068=CARTESIAN_POINT('Ctrl Pts',(-6.1497417158695,3.35714285676231,-4.29309641475446));
#110069=CARTESIAN_POINT('Ctrl Pts',(-6.10265362077076,3.37001483656105,
-4.3605488071224));
#110070=CARTESIAN_POINT('Ctrl Pts',(-6.05436811763914,3.38295904483433,
-4.42735141118742));
#110071=CARTESIAN_POINT('Ctrl Pts',(-6.00491276217618,3.39596551520488,
-4.49344219014927));
#110072=CARTESIAN_POINT('',(-5.8320435660374,3.39596551267961,-4.51256781591366));
#110073=CARTESIAN_POINT('Origin',(-9.02489888376934E-13,3.487378375,-6.71554825637521E-13));
#110074=CARTESIAN_POINT('',(-6.32514662437651,3.48629831963453,-4.03020100929146));
#110075=CARTESIAN_POINT('Origin',(0.144191659664066,3.62489375334973,0.118122165331142));
#110076=CARTESIAN_POINT('Origin',(0.162236844850232,3.48214202030952,0.10415561729928));
#110077=CARTESIAN_POINT('Ctrl Pts',(-5.13629452100001,3.266573167,-5.46520618000001));
#110078=CARTESIAN_POINT('Ctrl Pts',(-5.432804675,3.330825242,-5.186540851));
#110079=CARTESIAN_POINT('Ctrl Pts',(-5.697425627,3.395965514,-4.877431827));
#110080=CARTESIAN_POINT('Ctrl Pts',(-5.135673182,3.266573167,-5.117358788));
#110081=CARTESIAN_POINT('Ctrl Pts',(-5.413311169,3.330825242,-4.83872717));
#110082=CARTESIAN_POINT('Ctrl Pts',(-5.659174375,3.395965514,-4.531693435));
#110083=CARTESIAN_POINT('',(-5.69742562195829,3.39596551397696,-4.87743183267498));
#110084=CARTESIAN_POINT('',(-5.67829999611997,3.39596551522583,-4.70456263689008));
#110085=CARTESIAN_POINT('',(-5.31614709217801,3.30628897737121,-5.29042343252636));
#110086=CARTESIAN_POINT('Origin',(0.152711476053585,3.48210502425196,0.112544600522418));
#110087=CARTESIAN_POINT('Ctrl Pts',(-5.13896785745178,3.26733592494318,
-5.11405019183392));
#110088=CARTESIAN_POINT('Ctrl Pts',(-5.16853479175912,3.27415053063135,
-5.1433234832491));
#110089=CARTESIAN_POINT('Ctrl Pts',(-5.19809750522736,3.28079893115591,
-5.1726772600891));
#110090=CARTESIAN_POINT('Ctrl Pts',(-5.25714465569619,3.29377261877121,
-5.23146066871708));
#110091=CARTESIAN_POINT('Ctrl Pts',(-5.28666419646867,3.30010561494333,
-5.26092525818259));
#110092=CARTESIAN_POINT('Ctrl Pts',(-5.31614709470979,3.30628897724565,
-5.29042343002221));
#110093=CARTESIAN_POINT('Ctrl Pts',(-4.89234033307211,3.3972605424113,-5.68463487117339));
#110094=CARTESIAN_POINT('Ctrl Pts',(-4.89545216603606,3.39661302820565,
-5.6819508075867));
#110095=CARTESIAN_POINT('Ctrl Pts',(-4.898563999,3.395965514,-5.679266744));
#110096=CARTESIAN_POINT('Ctrl Pts',(-4.992175632,3.376486685,-5.598523472));
#110097=CARTESIAN_POINT('Ctrl Pts',(-5.083075345,3.357142857,-5.514738891));
#110098=CARTESIAN_POINT('Ctrl Pts',(-5.29438337900001,3.31217565,-5.319970893));
#110099=CARTESIAN_POINT('Ctrl Pts',(-5.490167888,3.266554913,-5.109604345));
#110100=CARTESIAN_POINT('Ctrl Pts',(-4.54650273517165,3.3972605424113,-5.64728926211416));
#110101=CARTESIAN_POINT('Ctrl Pts',(-4.54959431308582,3.39661302820565,
-5.64479471505708));
#110102=CARTESIAN_POINT('Ctrl Pts',(-4.552685891,3.395965514,-5.64230016800001));
#110103=CARTESIAN_POINT('Ctrl Pts',(-4.645688202,3.376486685,-5.567258022));
#110104=CARTESIAN_POINT('Ctrl Pts',(-4.736166816,3.357142857,-5.489191552));
#110105=CARTESIAN_POINT('Ctrl Pts',(-4.946495953,3.31217565,-5.30771603400001));
#110106=CARTESIAN_POINT('Ctrl Pts',(-5.142321598,3.266554913,-5.110677899));
#110107=CARTESIAN_POINT('',(-4.89856399292942,3.39596551397715,-5.67926674902997));
#110108=CARTESIAN_POINT('Ctrl Pts',(-5.31614709017629,3.30628897830889,
-5.29042343480269));
#110109=CARTESIAN_POINT('Ctrl Pts',(-5.23991993481122,3.32334891375402,
-5.3670212298921));
#110110=CARTESIAN_POINT('Ctrl Pts',(-5.16218651342885,3.340307679368,-5.44182011168093));
#110111=CARTESIAN_POINT('Ctrl Pts',(-5.08307534592634,3.35714285679733,
-5.51473889012026));
#110112=CARTESIAN_POINT('Ctrl Pts',(-5.02258787301562,3.370014836623,-5.57049173472499));
#110113=CARTESIAN_POINT('Ctrl Pts',(-4.96107067312144,3.38295904483426,
-5.62535257504625));
#110114=CARTESIAN_POINT('Ctrl Pts',(-4.89856399296705,3.39596551520491,
-5.67926674896868));
#110115=CARTESIAN_POINT('',(-4.72562493877464,3.3959655126796,-5.66078346119694));
#110116=CARTESIAN_POINT('Origin',(-1.6826817716975E-13,3.48737837500044,
-2.05131051034257E-13));
#110117=CARTESIAN_POINT('',(-5.31089412610486,3.48629831962543,-5.29569670366415));
#110118=CARTESIAN_POINT('Origin',(0.115427610360891,3.62489372344857,0.146357328935068));
#110119=CARTESIAN_POINT('Origin',(0.1360537206532,3.4821420105048,0.13659692597751));
#110120=CARTESIAN_POINT('Ctrl Pts',(-3.841353031,3.266573167,-6.441584191));
#110121=CARTESIAN_POINT('Ctrl Pts',(-4.190835751,3.330825242,-6.233174821));
#110122=CARTESIAN_POINT('Ctrl Pts',(-4.515719315,3.395965514,-5.988178277));
#110123=CARTESIAN_POINT('Ctrl Pts',(-3.915523125,3.266573167,-6.101735708));
#110124=CARTESIAN_POINT('Ctrl Pts',(-4.246567652,3.330825242,-5.889302302));
#110125=CARTESIAN_POINT('Ctrl Pts',(-4.552685891,3.395965514,-5.642300168));
#110126=CARTESIAN_POINT('',(-4.51571930876571,3.39596551397696,-5.98817828133813));
#110127=CARTESIAN_POINT('',(-4.53420259696787,3.39596551522583,-5.81523922720331));
#110128=CARTESIAN_POINT('',(-4.05457387323724,3.30628897737472,-6.30955075328127));
#110129=CARTESIAN_POINT('Origin',(0.124947428463476,3.48210504497436,0.142741857003189));
#110130=CARTESIAN_POINT('Ctrl Pts',(-3.91945202346168,3.26733592500564,
-6.09921272262872));
#110131=CARTESIAN_POINT('Ctrl Pts',(-3.9420348069806,3.27415053068454,-6.13415763776697));
#110132=CARTESIAN_POINT('Ctrl Pts',(-3.96459616635793,3.28079893119255,
-6.16918024915714));
#110133=CARTESIAN_POINT('Ctrl Pts',(-4.00962613217553,3.29377261878804,
-6.23928272632204));
#110134=CARTESIAN_POINT('Ctrl Pts',(-4.03212150681201,3.30010561495652,
-6.27440427875316));
#110135=CARTESIAN_POINT('Ctrl Pts',(-4.05457387631763,3.306288977244,-6.30955075129799));
#110136=CARTESIAN_POINT('Ctrl Pts',(-3.5559316742459,3.3972605424113,-6.60343982105814));
#110137=CARTESIAN_POINT('Ctrl Pts',(-3.55954774862295,3.39661302820565,
-6.60148746152907));
#110138=CARTESIAN_POINT('Ctrl Pts',(-3.563163823,3.395965514,-6.599535102));
#110139=CARTESIAN_POINT('Ctrl Pts',(-3.671944285,3.376486685,-6.540803298));
#110140=CARTESIAN_POINT('Ctrl Pts',(-3.778730021,3.357142857,-6.478518305));
#110141=CARTESIAN_POINT('Ctrl Pts',(-4.026967153,3.31217565,-6.333728855));
#110142=CARTESIAN_POINT('Ctrl Pts',(-4.263396918,3.266554913,-6.170368443));
#110143=CARTESIAN_POINT('Ctrl Pts',(-3.22620776921482,3.3972605424113,-6.49262247109658));
#110144=CARTESIAN_POINT('Ctrl Pts',(-3.22976332160741,3.39661302820565,
-6.4908508430483));
#110145=CARTESIAN_POINT('Ctrl Pts',(-3.233318874,3.395965514,-6.489079215));
#110146=CARTESIAN_POINT('Ctrl Pts',(-3.340278685,3.376486685,-6.435784261));
#110147=CARTESIAN_POINT('Ctrl Pts',(-3.445423944,3.357142857,-6.378993169));
#110148=CARTESIAN_POINT('Ctrl Pts',(-3.689847575,3.31217565,-6.246974995));
#110149=CARTESIAN_POINT('Ctrl Pts',(-3.923452299,3.266554913,-6.096640227));
#110150=CARTESIAN_POINT('',(-3.56316381609284,3.39596551397714,-6.59953510579764));
#110151=CARTESIAN_POINT('Ctrl Pts',(-4.05457387064305,3.30628897830886,
-6.30955075494452));
#110152=CARTESIAN_POINT('Ctrl Pts',(-3.96366260214418,3.32334891375399,
-6.36797115091668));
#110153=CARTESIAN_POINT('Ctrl Pts',(-3.87166699641581,3.34030767936791,
-6.42431088867839));
#110154=CARTESIAN_POINT('Ctrl Pts',(-3.77873002219183,3.3571428567841,-6.47851830430484));
#110155=CARTESIAN_POINT('Ctrl Pts',(-3.70767149963447,3.37001483659959,
-6.51996465985505));
#110156=CARTESIAN_POINT('Ctrl Pts',(-3.63579907860465,3.38295904483422,
-6.56031850441926));
#110157=CARTESIAN_POINT('Ctrl Pts',(-3.56316381603993,3.39596551520488,
-6.59953510555543));
#110158=CARTESIAN_POINT('',(-3.39824134130304,3.39596551267961,-6.54430716223715));
#110159=CARTESIAN_POINT('Origin',(6.85215773010839E-13,3.48737837500089,
1.19869392189997E-12));
#110160=CARTESIAN_POINT('',(-4.04831012106115,3.48629831963159,-6.31357150582533));
#110161=CARTESIAN_POINT('Origin',(0.0812663912945105,3.62489370994011,0.167748984259999));
#110162=CARTESIAN_POINT('Origin',(0.10350851005091,3.48214198135497,0.162650836534864));
#110163=CARTESIAN_POINT('Ctrl Pts',(-2.366794143,3.266573167,-7.116760884));
#110164=CARTESIAN_POINT('Ctrl Pts',(-2.752908005,3.330825242,-6.988352464));
#110165=CARTESIAN_POINT('Ctrl Pts',(-3.122862986,3.395965514,-6.81892416500001));
#110166=CARTESIAN_POINT('Ctrl Pts',(-2.512287559,3.266573167,-6.800802248));
#110167=CARTESIAN_POINT('Ctrl Pts',(-2.881259352,3.330825242,-6.664500205));
#110168=CARTESIAN_POINT('Ctrl Pts',(-3.233318874,3.395965514,-6.489079215));
#110169=CARTESIAN_POINT('',(-3.12286297908662,3.39596551397696,-6.81892416813198));
#110170=CARTESIAN_POINT('',(-3.17809092309782,3.39596551522583,-6.65400169329663));
#110171=CARTESIAN_POINT('',(-2.60341328610598,3.30628897734022,-7.03365049340117));
#110172=CARTESIAN_POINT('Origin',(0.0913408454317249,3.48210503010585,0.166264369373738));
#110173=CARTESIAN_POINT('Ctrl Pts',(-2.5166669693812,3.26733592496633,-6.79918284502861));
#110174=CARTESIAN_POINT('Ctrl Pts',(-2.53120965623776,3.27415053064923,
-6.83816539843916));
#110175=CARTESIAN_POINT('Ctrl Pts',(-2.54571471740442,3.2807989311671,-6.87721922612769));
#110176=CARTESIAN_POINT('Ctrl Pts',(-2.57462194719662,3.29377261875497,
-6.95536285802594));
#110177=CARTESIAN_POINT('Ctrl Pts',(-2.58904129683186,3.3001056149235,-6.99449912875471));
#110178=CARTESIAN_POINT('Ctrl Pts',(-2.603413289663,3.30628897720744,-7.03365049210116));
#110179=CARTESIAN_POINT('Ctrl Pts',(-2.05325160269057,3.39726054241129,
-7.21347526574445));
#110180=CARTESIAN_POINT('Ctrl Pts',(-2.05720283484529,3.39661302820565,
-7.21234590037222));
#110181=CARTESIAN_POINT('Ctrl Pts',(-2.061154067,3.395965514,-7.21121653500001));
#110182=CARTESIAN_POINT('Ctrl Pts',(-2.180016904,3.376486685,-7.177242431));
#110183=CARTESIAN_POINT('Ctrl Pts',(-2.297695481,3.357142857,-7.139369403));
#110184=CARTESIAN_POINT('Ctrl Pts',(-2.571254418,3.31217565,-7.05132869600001));
#110185=CARTESIAN_POINT('Ctrl Pts',(-2.837274247,3.266554913,-6.94261297));
#110186=CARTESIAN_POINT('Ctrl Pts',(-1.75505891355549,3.39726054241129,
-7.03436787041624));
#110187=CARTESIAN_POINT('Ctrl Pts',(-1.75891218677775,3.39661302820565,
-7.03340200070812));
#110188=CARTESIAN_POINT('Ctrl Pts',(-1.76276546,3.395965514,-7.032436131));
#110189=CARTESIAN_POINT('Ctrl Pts',(-1.87868145,3.376486685,-7.003380381));
#110190=CARTESIAN_POINT('Ctrl Pts',(-1.993576877,3.357142857,-6.970520155));
#110191=CARTESIAN_POINT('Ctrl Pts',(-2.260666024,3.31217565,-6.894132348));
#110192=CARTESIAN_POINT('Ctrl Pts',(-2.521126731,3.266554913,-6.797530434));
#110193=CARTESIAN_POINT('',(-2.0611540593741,3.39596551397715,-7.21121653699979));
#110194=CARTESIAN_POINT('Ctrl Pts',(-2.60341328311995,3.30628897830887,
-7.03365049452299));
#110195=CARTESIAN_POINT('Ctrl Pts',(-2.50206881124079,3.32334891375401,
-7.07116181866411));
#110196=CARTESIAN_POINT('Ctrl Pts',(-2.40011263349957,3.34030767936808,
-7.10640802868447));
#110197=CARTESIAN_POINT('Ctrl Pts',(-2.29769548211474,3.35714285681676,
-7.13936940264124));
#110198=CARTESIAN_POINT('Ctrl Pts',(-2.21938852700798,3.37001483665733,
-7.16457128373588));
#110199=CARTESIAN_POINT('Ctrl Pts',(-2.14052155993246,3.38295904483429,
-7.18853123205442));
#110200=CARTESIAN_POINT('Ctrl Pts',(-2.06115405943867,3.39596551520489,
-7.21121653697635));
#110201=CARTESIAN_POINT('',(-1.91195975566792,3.39596551267961,-7.12182633510264));
#110202=CARTESIAN_POINT('Origin',(-4.25657772917809E-13,3.48737837499945,
-1.36305897124878E-12));
#110203=CARTESIAN_POINT('',(-2.59643163431783,3.48629831961912,-7.03623072141385));
#110204=CARTESIAN_POINT('Origin',(0.0433053581522996,3.62489369331728,0.181296946656153));
#110205=CARTESIAN_POINT('Origin',(0.0661234053702608,3.48214199777855,0.181099351764563));
#110206=CARTESIAN_POINT('Ctrl Pts',(-0.781566591,3.266573167,-7.459165749));
#110207=CARTESIAN_POINT('Ctrl Pts',(-1.18625734,3.330825242,-7.416762512));
#110208=CARTESIAN_POINT('Ctrl Pts',(-1.583985056,3.395965514,-7.330824738));
#110209=CARTESIAN_POINT('Ctrl Pts',(-0.991580219,3.266573167,-7.181870833));
#110210=CARTESIAN_POINT('Ctrl Pts',(-1.381226566,3.330825242,-7.128073485));
#110211=CARTESIAN_POINT('Ctrl Pts',(-1.76276546,3.395965514,-7.032436131));
#110212=CARTESIAN_POINT('',(-1.58398504857742,3.39596551397696,-7.33082473958187));
#110213=CARTESIAN_POINT('',(-1.67337525055052,3.39596551522583,-7.18163043623579));
#110214=CARTESIAN_POINT('',(-1.03051998746748,3.30628897732933,-7.42886455333183));
#110215=CARTESIAN_POINT('Origin',(0.0534634752718685,3.4821050195673,0.182013100375262));
#110216=CARTESIAN_POINT('Ctrl Pts',(-0.996205364753573,3.26733592494251,
-7.18123073465414));
#110217=CARTESIAN_POINT('Ctrl Pts',(-1.00202795503195,3.27415053062055,
-7.22242814541734));
#110218=CARTESIAN_POINT('Ctrl Pts',(-1.00779847745467,3.2807989311329,-7.26368707561806));
#110219=CARTESIAN_POINT('Ctrl Pts',(-1.01923135518573,3.29377267967181,
-7.34621834033066));
#110220=CARTESIAN_POINT('Ctrl Pts',(-1.02490050608604,3.30010573880957,
-7.38753980110302));
#110221=CARTESIAN_POINT('Ctrl Pts',(-1.03051999137626,3.30628897719394,
-7.42886455280585));
#110222=CARTESIAN_POINT('Ctrl Pts',(-0.454563767573316,3.3972605424113,
-7.48621662364792));
#110223=CARTESIAN_POINT('Ctrl Pts',(-0.458665402286658,3.39661302820565,
-7.48596306032396));
#110224=CARTESIAN_POINT('Ctrl Pts',(-0.462767037,3.395965514,-7.48570949700001));
#110225=CARTESIAN_POINT('Ctrl Pts',(-0.586154355,3.376486685,-7.478081685));
#110226=CARTESIAN_POINT('Ctrl Pts',(-0.709223254,3.357142857,-7.466391523));
#110227=CARTESIAN_POINT('Ctrl Pts',(-0.995312685000001,3.31217565,-7.439216243));
#110228=CARTESIAN_POINT('Ctrl Pts',(-1.278483785,3.266554913,-7.39022863000001));
#110229=CARTESIAN_POINT('Ctrl Pts',(-0.201845453451928,3.3972605424113,
-7.24719404571963));
#110230=CARTESIAN_POINT('Ctrl Pts',(-0.205816272725964,3.39661302820565,
-7.24707909735982));
#110231=CARTESIAN_POINT('Ctrl Pts',(-0.209787092,3.395965514,-7.246964149));
#110232=CARTESIAN_POINT('Ctrl Pts',(-0.329239158,3.376486685,-7.243506218));
#110233=CARTESIAN_POINT('Ctrl Pts',(-0.448512371,3.357142857,-7.236113367));
#110234=CARTESIAN_POINT('Ctrl Pts',(-0.725778243,3.31217565,-7.21892773600001));
#110235=CARTESIAN_POINT('Ctrl Pts',(-1.000916079,3.266554913,-7.180575673));
#110236=CARTESIAN_POINT('',(-0.462767033893976,3.39596551355056,-7.48570949824636));
#110237=CARTESIAN_POINT('Ctrl Pts',(-1.03051998418126,3.30628897830881,
-7.42886455361434));
#110238=CARTESIAN_POINT('Ctrl Pts',(-0.923481063958462,3.32334891375394,
-7.44371281826105));
#110239=CARTESIAN_POINT('Ctrl Pts',(-0.816331671680277,3.3403076793679,
-7.45621742731177));
#110240=CARTESIAN_POINT('Ctrl Pts',(-0.709223255344492,3.35714285678867,
-7.46639152287229));
#110241=CARTESIAN_POINT('Ctrl Pts',(-0.627329415421036,3.37001483635925,
-7.47417051711955));
#110242=CARTESIAN_POINT('Ctrl Pts',(-0.545155634773015,3.38295904433458,
-7.48061622843096));
#110243=CARTESIAN_POINT('Ctrl Pts',(-0.462767033959746,3.39596551445183,
-7.48570949700878));
#110244=CARTESIAN_POINT('',(-0.336277056399031,3.39596551267961,-7.36633682336981));
#110245=CARTESIAN_POINT('Origin',(1.66262403150652E-13,3.48737837499922,
1.2862974574368E-12));
#110246=CARTESIAN_POINT('',(-1.02314689010349,3.48629831963628,-7.42988360835676));
#110247=CARTESIAN_POINT('Origin',(0.00331945825586336,3.62489370198345,
0.186367959974886));
#110248=CARTESIAN_POINT('Origin',(0.025646474010152,3.48214201755016,0.191079869937566));
#110249=CARTESIAN_POINT('Ctrl Pts',(0.840206145999999,3.266573167,-7.452788313));
#110250=CARTESIAN_POINT('Ctrl Pts',(0.4358614,3.330825242,-7.498372989));
#110251=CARTESIAN_POINT('Ctrl Pts',(0.028958256,3.395965514,-7.499944094));
#110252=CARTESIAN_POINT('Ctrl Pts',(0.57549231,3.266573167,-7.227123121));
#110253=CARTESIAN_POINT('Ctrl Pts',(0.183390838,3.330825242,-7.258345971));
#110254=CARTESIAN_POINT('Ctrl Pts',(-0.209787092,3.395965514,-7.246964149));
#110255=CARTESIAN_POINT('',(0.0289582635899049,3.39596551397696,-7.49994409402047));
#110256=CARTESIAN_POINT('',(-0.0904144103515404,3.39596551522583,-7.37345412159378));
#110257=CARTESIAN_POINT('',(0.590559280491092,3.30628897736223,-7.47671316417767));
#110258=CARTESIAN_POINT('Origin',(0.0130861047795402,3.48210501151378,0.189250681594911));
#110259=CARTESIAN_POINT('Ctrl Pts',(0.570837695264029,3.26733592494405,
-7.22749225733758));
#110260=CARTESIAN_POINT('Ctrl Pts',(0.574007459370702,3.2741505306344,-7.26897818017597));
#110261=CARTESIAN_POINT('Ctrl Pts',(0.577241298962552,3.28079893115661,
-7.3105129911894));
#110262=CARTESIAN_POINT('Ctrl Pts',(0.583817467099475,3.29377261875627,
-7.39357206124346));
#110263=CARTESIAN_POINT('Ctrl Pts',(0.587163713369376,3.30010561493485,
-7.43514570629488));
#110264=CARTESIAN_POINT('Ctrl Pts',(0.590559276754091,3.30628897722236,
-7.47671316441908));
#110265=CARTESIAN_POINT('Ctrl Pts',(1.16537896377315,3.3972605424113,-7.40891081180722));
#110266=CARTESIAN_POINT('Ctrl Pts',(1.16131871438658,3.39661302820565,-7.40954490690361));
#110267=CARTESIAN_POINT('Ctrl Pts',(1.157258465,3.395965514,-7.410179002));
#110268=CARTESIAN_POINT('Ctrl Pts',(1.03511612,3.376486685,-7.429254151));
#110269=CARTESIAN_POINT('Ctrl Pts',(0.912411464,3.357142857,-7.444293474));
#110270=CARTESIAN_POINT('Ctrl Pts',(0.627168763,3.31217565,-7.479254308));
#110271=CARTESIAN_POINT('Ctrl Pts',(0.340087157,3.266554913,-7.492285414));
#110272=CARTESIAN_POINT('Ctrl Pts',(1.36080607551578,3.3972605424113,-7.12114948230861));
#110273=CARTESIAN_POINT('Ctrl Pts',(1.35690338125789,3.39661302820565,-7.12189083015431));
#110274=CARTESIAN_POINT('Ctrl Pts',(1.353000687,3.395965514,-7.12263217800001));
#110275=CARTESIAN_POINT('Ctrl Pts',(1.23559799,3.376486685,-7.144933755));
#110276=CARTESIAN_POINT('Ctrl Pts',(1.117524075,3.357142857,-7.163353959));
#110277=CARTESIAN_POINT('Ctrl Pts',(0.843046122,3.31217565,-7.206174085));
#110278=CARTESIAN_POINT('Ctrl Pts',(0.566096296,3.266554913,-7.227865175));
#110279=CARTESIAN_POINT('',(1.1572584727817,3.39596551397715,-7.41017900074624));
#110280=CARTESIAN_POINT('Ctrl Pts',(0.590559283615143,3.30628897830888,
-7.47671316387715));
#110281=CARTESIAN_POINT('Ctrl Pts',(0.69828763140258,3.32334891375402,-7.46820408056629));
#110282=CARTESIAN_POINT('Ctrl Pts',(0.805620051771964,3.340307679368,-7.45738238676489));
#110283=CARTESIAN_POINT('Ctrl Pts',(0.912411462719141,3.35714285679808,
-7.44429347415699));
#110284=CARTESIAN_POINT('Ctrl Pts',(0.994062925744556,3.37001483662431,
-7.43428584474713));
#110285=CARTESIAN_POINT('Ctrl Pts',(1.07570116794024,3.3829590448342,-7.42291592453298));
#110286=CARTESIAN_POINT('Ctrl Pts',(1.15725847269244,3.39596551520491,-7.41017900061876));
#110287=CARTESIAN_POINT('',(1.25512958399112,3.3959655126796,-7.26640558861969));
#110288=CARTESIAN_POINT('Origin',(-1.14874608306628E-13,3.48737837499989,
1.91990520703733E-12));
#110289=CARTESIAN_POINT('',(0.597979065930149,3.48629831963031,-7.47612339603309));
#110290=CARTESIAN_POINT('Origin',(-0.0368217379796355,3.62489368320795,
0.18272430210277));
#110291=CARTESIAN_POINT('Origin',(-0.0160296329366373,3.48214204465331,
0.192125554458964));
#110292=CARTESIAN_POINT('Ctrl Pts',(2.422691778,3.266573167,-7.097926778));
#110293=CARTESIAN_POINT('Ctrl Pts',(2.037599744,3.330825242,-7.229367878));
#110294=CARTESIAN_POINT('Ctrl Pts',(1.640547511,3.395965514,-7.3183744));
#110295=CARTESIAN_POINT('Ctrl Pts',(2.115655458,3.266573167,-6.934443163));
#110296=CARTESIAN_POINT('Ctrl Pts',(1.739433091,3.330825242,-7.049226266));
#110297=CARTESIAN_POINT('Ctrl Pts',(1.353000687,3.395965514,-7.122632178));
#110298=CARTESIAN_POINT('',(1.64054751841347,3.39596551397696,-7.31837439837307));
#110299=CARTESIAN_POINT('',(1.4967741064898,3.39596551522583,-7.2205032874474));
#110300=CARTESIAN_POINT('',(2.18402465294681,3.30628897734932,-7.17495897641274));
#110301=CARTESIAN_POINT('Origin',(-0.0279031602769891,3.48210505020889,
0.18763928548272));
#110302=CARTESIAN_POINT('Ctrl Pts',(2.11118901980916,3.26733592496051,-6.93580427423557));
#110303=CARTESIAN_POINT('Ctrl Pts',(2.12320292378257,3.27415053065322,-6.97563887355951));
#110304=CARTESIAN_POINT('Ctrl Pts',(2.13528991457471,3.28079893116479,-7.01550744370506));
#110305=CARTESIAN_POINT('Ctrl Pts',(2.15956758027455,3.29377261876942,-7.09521095702699));
#110306=CARTESIAN_POINT('Ctrl Pts',(2.17177269778662,3.30010561493228,-7.13509328920972));
#110307=CARTESIAN_POINT('Ctrl Pts',(2.18402464941342,3.30628897722014,-7.1749589775187));
#110308=CARTESIAN_POINT('Ctrl Pts',(2.73082986964228,3.39726054241129,-6.98517256627893));
#110309=CARTESIAN_POINT('Ctrl Pts',(2.72700085832114,3.39661302820565,-6.98666467013947));
#110310=CARTESIAN_POINT('Ctrl Pts',(2.723171847,3.395965514,-6.988156774));
#110311=CARTESIAN_POINT('Ctrl Pts',(2.607985715,3.376486685,-7.03304294900001));
#110312=CARTESIAN_POINT('Ctrl Pts',(2.491382836,3.357142857,-7.074108535));
#110313=CARTESIAN_POINT('Ctrl Pts',(2.220324497,3.31217565,-7.169570753));
#110314=CARTESIAN_POINT('Ctrl Pts',(1.942756002,3.266554913,-7.244011259));
#110315=CARTESIAN_POINT('Ctrl Pts',(2.85982782510034,3.39726054241129,-6.66212788310328));
#110316=CARTESIAN_POINT('Ctrl Pts',(2.85617574155017,3.39661302820565,-6.66369086255164));
#110317=CARTESIAN_POINT('Ctrl Pts',(2.852523658,3.395965514,-6.665253842));
#110318=CARTESIAN_POINT('Ctrl Pts',(2.742659951,3.376486685,-6.71227213));
#110319=CARTESIAN_POINT('Ctrl Pts',(2.631306337,3.357142857,-6.755644082));
#110320=CARTESIAN_POINT('Ctrl Pts',(2.372450588,3.31217565,-6.856467744));
#110321=CARTESIAN_POINT('Ctrl Pts',(2.106638638,3.266554913,-6.937187734));
#110322=CARTESIAN_POINT('',(2.72317185034836,3.39596551355056,-6.9881567738227));
#110323=CARTESIAN_POINT('Ctrl Pts',(2.18402465597099,3.3062889783089,-7.17495897559197));
#110324=CARTESIAN_POINT('Ctrl Pts',(2.287405173422,3.32334891375403,-7.14349041942547));
#110325=CARTESIAN_POINT('Ctrl Pts',(2.3899018770918,3.34030767936787,-7.1098484331051));
#110326=CARTESIAN_POINT('Ctrl Pts',(2.49138283465962,3.35714285677056,-7.07410853538993));
#110327=CARTESIAN_POINT('Ctrl Pts',(2.5689739854683,3.37001483632763,-7.04678222827701));
#110328=CARTESIAN_POINT('Ctrl Pts',(2.64625937286991,3.38295904433555,-7.01812832265671));
#110329=CARTESIAN_POINT('Ctrl Pts',(2.72317184976995,3.39596551445312,-6.98815677273005));
#110330=CARTESIAN_POINT('',(2.78784776000748,3.39596551267962,-6.82670530493414));
#110331=CARTESIAN_POINT('Origin',(-4.47450236584768E-13,3.48737837500022,
1.14795326022765E-12));
#110332=CARTESIAN_POINT('',(2.19114418520372,3.48629831963248,-7.17278796251029));
#110333=CARTESIAN_POINT('Origin',(-0.0752411761832097,3.62489372401122,
0.170536642326012));
#110334=CARTESIAN_POINT('Origin',(-0.0569562512824762,3.48214202558383,
0.18418808260192));
#110335=CARTESIAN_POINT('Ctrl Pts',(3.891895034,3.266573167,-6.411174077));
#110336=CARTESIAN_POINT('Ctrl Pts',(3.54406219,3.330825242,-6.622325561));
#110337=CARTESIAN_POINT('Ctrl Pts',(3.175426589,3.395965514,-6.794605653));
#110338=CARTESIAN_POINT('Ctrl Pts',(3.556892909,3.266573167,-6.31751635));
#110339=CARTESIAN_POINT('Ctrl Pts',(3.214141385,3.330825242,-6.510492576));
#110340=CARTESIAN_POINT('Ctrl Pts',(2.852523658,3.395965514,-6.665253842));
#110341=CARTESIAN_POINT('',(3.17542659581968,3.39596551397696,-6.7946056496667));
#110342=CARTESIAN_POINT('',(3.01397513048093,3.39596551522583,-6.72992974437362));
#110343=CARTESIAN_POINT('',(3.67536745979543,3.30628897733966,-6.53771168204423));
#110344=CARTESIAN_POINT('Origin',(-0.0675876810856374,3.48210503795346,
0.177253988013014));
#110345=CARTESIAN_POINT('Ctrl Pts',(3.55282349146402,3.26733592496364,-6.31980579117285));
#110346=CARTESIAN_POINT('Ctrl Pts',(3.57311977824477,3.27415053065783,-6.35612644571022));
#110347=CARTESIAN_POINT('Ctrl Pts',(3.5934947459802,3.28079893117787,-6.39246456534641));
#110348=CARTESIAN_POINT('Ctrl Pts',(3.63433871271115,3.29377261876238,-6.46508567454925));
#110349=CARTESIAN_POINT('Ctrl Pts',(3.65483200398093,3.30010561492691,-6.5014118406284));
#110350=CARTESIAN_POINT('Ctrl Pts',(3.67536745644001,3.30628897719833,-6.53771168388222));
#110351=CARTESIAN_POINT('Ctrl Pts',(4.16859020585149,3.3972605424113,-6.2348154138769));
#110352=CARTESIAN_POINT('Ctrl Pts',(4.16517147292575,3.39661302820565,-6.23709575743844));
#110353=CARTESIAN_POINT('Ctrl Pts',(4.16175274,3.395965514,-6.239376101));
#110354=CARTESIAN_POINT('Ctrl Pts',(4.058908797,3.376486685,-6.307974476));
#110355=CARTESIAN_POINT('Ctrl Pts',(3.953859916,3.357142857,-6.373146144));
#110356=CARTESIAN_POINT('Ctrl Pts',(3.709660325,3.31217565,-6.52464603900001));
#110357=CARTESIAN_POINT('Ctrl Pts',(3.454583735,3.266554913,-6.657015188));
#110358=CARTESIAN_POINT('Ctrl Pts',(4.2251272029383,3.3972605424113,-5.89159258926902));
#110359=CARTESIAN_POINT('Ctrl Pts',(4.22189649746915,3.39661302820565,-5.89390411713451));
#110360=CARTESIAN_POINT('Ctrl Pts',(4.218665792,3.395965514,-5.896215645));
#110361=CARTESIAN_POINT('Ctrl Pts',(4.12147818,3.376486685,-5.965752121));
#110362=CARTESIAN_POINT('Ctrl Pts',(4.022051639,3.357142857,-6.032047796));
#110363=CARTESIAN_POINT('Ctrl Pts',(3.7909219,3.31217565,-6.186160591));
#110364=CARTESIAN_POINT('Ctrl Pts',(3.548676898,3.266554913,-6.322135104));
#110365=CARTESIAN_POINT('',(4.16175274448907,3.39596551354713,-6.23937609860885));
#110366=CARTESIAN_POINT('Ctrl Pts',(3.67536746257195,3.30628897830886,-6.53771168043497));
#110367=CARTESIAN_POINT('Ctrl Pts',(3.76956619177034,3.32334891375399,-6.48475508644378));
#110368=CARTESIAN_POINT('Ctrl Pts',(3.86243454701094,3.34030767936762,-6.42986586961159));
#110369=CARTESIAN_POINT('Ctrl Pts',(3.95385991457985,3.35714285672509,-6.37314614456213));
#110370=CARTESIAN_POINT('Ctrl Pts',(4.02376268007051,3.37001483649523,-6.32977890632933));
#110371=CARTESIAN_POINT('Ctrl Pts',(4.0930814367508,3.38295904483422,-6.28518083842415));
#110372=CARTESIAN_POINT('Ctrl Pts',(4.16175274640143,3.39596551520488,-6.23937609651593));
#110373=CARTESIAN_POINT('',(4.19020927267297,3.3959655126796,-6.06779586839188));
#110374=CARTESIAN_POINT('Origin',(-3.25260651745651E-14,3.48737837500033,
1.47451495458029E-14));
#110375=CARTESIAN_POINT('',(3.68185383757783,3.48629831961797,-6.53406093588961));
#110376=CARTESIAN_POINT('Origin',(-0.110142518670112,3.62489370752314,0.150375150523643));
#110377=CARTESIAN_POINT('Origin',(-0.095219468594035,3.48214199609701,0.167637657977258));
#110378=CARTESIAN_POINT('Ctrl Pts',(5.179117605,3.266573167,-5.424642001));
#110379=CARTESIAN_POINT('Ctrl Pts',(4.884808226,3.330825242,-5.70563066));
#110380=CARTESIAN_POINT('Ctrl Pts',(4.561826248,3.395965514,-5.953128697));
#110381=CARTESIAN_POINT('Ctrl Pts',(4.831814,3.266573167,-5.405189494));
#110382=CARTESIAN_POINT('Ctrl Pts',(4.538560001,3.330825242,-5.667335489));
#110383=CARTESIAN_POINT('Ctrl Pts',(4.218665792,3.395965514,-5.89621564500001));
#110384=CARTESIAN_POINT('',(4.56182625396996,3.39596551397696,-5.95312869231247));
#110385=CARTESIAN_POINT('',(4.39024602614564,3.39596551522583,-5.92467216644601));
#110386=CARTESIAN_POINT('',(4.99485416922012,3.30628897734424,-5.59476825503998));
#110387=CARTESIAN_POINT('Origin',(-0.104112042527872,3.48210506471219,0.158580729364672));
#110388=CARTESIAN_POINT('Ctrl Pts',(4.82833188523068,3.26733592501069,-5.40830021398496));
#110389=CARTESIAN_POINT('Ctrl Pts',(4.85596152334697,3.2741505306834,-5.43940860997987));
#110390=CARTESIAN_POINT('Ctrl Pts',(4.88367175730801,3.28079893118907,-5.47051714869432));
#110391=CARTESIAN_POINT('Ctrl Pts',(4.93917220669472,3.2937726187639,-5.53266017110701));
#110392=CARTESIAN_POINT('Ctrl Pts',(4.96699542809321,3.30010561492509,-5.56373159971429));
#110393=CARTESIAN_POINT('Ctrl Pts',(4.99485416633788,3.30628897720176,-5.59476825754054));
#110394=CARTESIAN_POINT('Ctrl Pts',(5.41143189778815,3.3972605424113,-5.19292522215096));
#110395=CARTESIAN_POINT('Ctrl Pts',(5.40858329939408,3.39661302820565,-5.19588717907548));
#110396=CARTESIAN_POINT('Ctrl Pts',(5.405734701,3.395965514,-5.198849136));
#110397=CARTESIAN_POINT('Ctrl Pts',(5.320041815,3.376486685,-5.28795212699999));
#110398=CARTESIAN_POINT('Ctrl Pts',(5.2314589,3.357142857,-5.374182522));
#110399=CARTESIAN_POINT('Ctrl Pts',(5.02553655899999,3.31217565,-5.574636127));
#110400=CARTESIAN_POINT('Ctrl Pts',(4.804878973,3.266554913,-5.758744486));
#110401=CARTESIAN_POINT('Ctrl Pts',(5.39286432943003,3.3972605424113,-4.84557297336042));
#110402=CARTESIAN_POINT('Ctrl Pts',(5.39020606621502,3.39661302820565,-4.84852496518022));
#110403=CARTESIAN_POINT('Ctrl Pts',(5.387547803,3.395965514,-4.851476957));
#110404=CARTESIAN_POINT('Ctrl Pts',(5.30758067,3.376486685,-4.940280173));
#110405=CARTESIAN_POINT('Ctrl Pts',(5.224730277,3.357142857,-5.026399659));
#110406=CARTESIAN_POINT('Ctrl Pts',(5.032133918,3.31217565,-5.22659544400001));
#110407=CARTESIAN_POINT('Ctrl Pts',(4.82478297,3.266554913,-5.411466464));
#110408=CARTESIAN_POINT('',(5.40573470643638,3.39596551397716,-5.19884913029323));
#110409=CARTESIAN_POINT('Ctrl Pts',(4.99485417156935,3.3062889783089,-5.59476825287003));
#110410=CARTESIAN_POINT('Ctrl Pts',(5.07546648430106,3.32334891375403,-5.52279981230656));
#110411=CARTESIAN_POINT('Ctrl Pts',(5.15436406977217,3.34030767936791,-5.44922992368464));
#110412=CARTESIAN_POINT('Ctrl Pts',(5.23145889898019,3.35714285677832,-5.3741825227477));
#110413=CARTESIAN_POINT('Ctrl Pts',(5.29040470296592,3.37001483658936,-5.31680215796539));
#110414=CARTESIAN_POINT('Ctrl Pts',(5.34851555915562,3.38295904483425,-5.25834528453235));
#110415=CARTESIAN_POINT('Ctrl Pts',(5.40573470628808,3.39596551520492,-5.19884913024567));
#110416=CARTESIAN_POINT('',(5.39664125752635,3.3959655126796,-5.02516304056512));
#110417=CARTESIAN_POINT('Origin',(-1.06512021424976E-12,3.48737837499989,
1.34874750257197E-12));
#110418=CARTESIAN_POINT('',(5.00040409668657,3.48629831962102,-5.58980848202957));
#110419=CARTESIAN_POINT('Origin',(-0.139893566805701,3.62489370874121,0.123181968684504));
#110420=CARTESIAN_POINT('Origin',(-0.129030497729903,3.48214198866982,0.143249074360335));
#110421=CARTESIAN_POINT('Ctrl Pts',(6.22417039200001,3.266573167,-4.184459694));
#110422=CARTESIAN_POINT('Ctrl Pts',(5.997146059,3.330825242,-4.522146811));
#110423=CARTESIAN_POINT('Ctrl Pts',(5.734919982,3.395965514,-4.83329006));
#110424=CARTESIAN_POINT('Ctrl Pts',(5.880804839,3.266573167,-4.240121985));
#110425=CARTESIAN_POINT('Ctrl Pts',(5.650760595,3.330825242,-4.559180094));
#110426=CARTESIAN_POINT('Ctrl Pts',(5.38754780300001,3.395965514,-4.851476957));
#110427=CARTESIAN_POINT('',(5.73491998675332,3.39596551397696,-4.83329005408083));
#110428=CARTESIAN_POINT('',(5.56123389752299,3.39596551522583,-4.84238350273135));
#110429=CARTESIAN_POINT('',(6.08078704939524,3.30628897732461,-4.39021968257402));
#110430=CARTESIAN_POINT('Origin',(-0.135768054767925,3.48210502381861,0.13249211387284));
#110431=CARTESIAN_POINT('Ctrl Pts',(5.87807284719938,3.2673359249554,-4.24390852955201));
#110432=CARTESIAN_POINT('Ctrl Pts',(5.91174390509398,3.27415053062209,-4.26835007303321));
#110433=CARTESIAN_POINT('Ctrl Pts',(5.94549370534151,3.28079893112742,-4.29277443015119));
#110434=CARTESIAN_POINT('Ctrl Pts',(6.01305549792867,3.29377261871852,-4.34153362712332));
#110435=CARTESIAN_POINT('Ctrl Pts',(6.04690766664564,3.30010561489497,-4.36589745282733));
#110436=CARTESIAN_POINT('Ctrl Pts',(6.08078704722014,3.30628897719265,-4.39021968563735));
#110437=CARTESIAN_POINT('Ctrl Pts',(6.4012410481422,3.3972605424113,-3.90821961906406));
#110438=CARTESIAN_POINT('Ctrl Pts',(6.39909578157111,3.39661302820565,-3.91172469153203));
#110439=CARTESIAN_POINT('Ctrl Pts',(6.39695051500001,3.395965514,-3.915229764));
#110440=CARTESIAN_POINT('Ctrl Pts',(6.33241559,3.376486685,-4.020671014));
#110441=CARTESIAN_POINT('Ctrl Pts',(6.264440681,3.357142857,-4.123928098));
#110442=CARTESIAN_POINT('Ctrl Pts',(6.10642429,3.31217565,-4.363962426));
#110443=CARTESIAN_POINT('Ctrl Pts',(5.93050341,3.266554913,-4.591201292));
#110444=CARTESIAN_POINT('Ctrl Pts',(6.30843711407222,3.3972605424113,-3.5729797511861));
#110445=CARTESIAN_POINT('Ctrl Pts',(6.30647559053612,3.39661302820565,-3.57643417509305));
#110446=CARTESIAN_POINT('Ctrl Pts',(6.30451406700001,3.395965514,-3.579888599));
#110447=CARTESIAN_POINT('Ctrl Pts',(6.245506587,3.376486685,-3.683806215));
#110448=CARTESIAN_POINT('Ctrl Pts',(6.183106334,3.357142857,-3.785722661));
#110449=CARTESIAN_POINT('Ctrl Pts',(6.038048947,3.31217565,-4.022640503));
#110450=CARTESIAN_POINT('Ctrl Pts',(5.875287554,3.266554913,-4.247763666));
#110451=CARTESIAN_POINT('',(6.39695051908622,3.39596551397713,-3.91522975725942));
#110452=CARTESIAN_POINT('Ctrl Pts',(6.08078705139423,3.30628897830882,-4.39021968008645));
#110453=CARTESIAN_POINT('Ctrl Pts',(6.14404360579022,3.32334891375396,-4.30260455727574));
#110454=CARTESIAN_POINT('Ctrl Pts',(6.20528125817945,3.3403076793676,-4.21379404295133));
#110455=CARTESIAN_POINT('Ctrl Pts',(6.26444067997507,3.35714285672434,-4.12392809923762));
#110456=CARTESIAN_POINT('Ctrl Pts',(6.30967328093506,3.37001483649389,-4.05521765063235));
#110457=CARTESIAN_POINT('Ctrl Pts',(6.35385903796572,3.38295904483422,-3.9856353497436));
#110458=CARTESIAN_POINT('Ctrl Pts',(6.39695051892677,3.39596551520485,-3.91522975724217));
#110459=CARTESIAN_POINT('',(6.35073229512134,3.3959655126796,-3.74755917451584));
#110460=CARTESIAN_POINT('Origin',(6.00214322687975E-13,3.48737837499989,
-4.62737487216813E-13));
#110461=CARTESIAN_POINT('',(6.08514101776744,3.48629831964224,-4.38418279619622));
#110462=CARTESIAN_POINT('Origin',(-0.163103671461469,3.62489372136745,0.0902292550734224));
#110463=CARTESIAN_POINT('Origin',(-0.156808169483224,3.48214199047778,0.112162257750512));
#110464=CARTESIAN_POINT('Ctrl Pts',(6.97818789,3.266573167,-2.748616702));
#110465=CARTESIAN_POINT('Ctrl Pts',(6.829064008,3.330825242,-3.127212403));
#110466=CARTESIAN_POINT('Ctrl Pts',(6.639855232,3.395965514,-3.487452151));
#110467=CARTESIAN_POINT('Ctrl Pts',(6.654815779,3.266573167,-2.876791084));
#110468=CARTESIAN_POINT('Ctrl Pts',(6.498737904,3.330825242,-3.237842504));
#110469=CARTESIAN_POINT('Ctrl Pts',(6.304514067,3.395965514,-3.579888599));
#110470=CARTESIAN_POINT('',(6.63985523530303,3.39596551397696,-3.48745214416228));
#110471=CARTESIAN_POINT('',(6.47218465316547,3.39596551522583,-3.53367036828643));
#110472=CARTESIAN_POINT('',(6.88238908513195,3.30628897738563,-2.98038931745279));
#110473=CARTESIAN_POINT('Origin',(-0.161075771399515,3.48210503785382,0.100208411574002));
#110474=CARTESIAN_POINT('Ctrl Pts',(6.65296165528463,3.26733592498242,-2.8810763986581));
#110475=CARTESIAN_POINT('Ctrl Pts',(6.69109971203849,3.27415053066632,-2.89770823034314));
#110476=CARTESIAN_POINT('Ctrl Pts',(6.72931097559604,3.2807989311849,-2.91430635021598));
#110477=CARTESIAN_POINT('Ctrl Pts',(6.80577499705763,3.29377261878132,-2.94740179608021));
#110478=CARTESIAN_POINT('Ctrl Pts',(6.8440732232251,3.30010561496541,-2.96391879355285));
#110479=CARTESIAN_POINT('Ctrl Pts',(6.88238908369249,3.30628897725673,-2.98038932077374));
#110480=CARTESIAN_POINT('Ctrl Pts',(7.09173528189306,3.3972605424113,-2.44077001058573));
#110481=CARTESIAN_POINT('Ctrl Pts',(7.09039365744652,3.39661302820565,-2.44465430529287));
#110482=CARTESIAN_POINT('Ctrl Pts',(7.089052033,3.395965514,-2.4485386));
#110483=CARTESIAN_POINT('Ctrl Pts',(7.048692651,3.376486685,-2.565387793));
#110484=CARTESIAN_POINT('Ctrl Pts',(7.004504177,3.357142857,-2.68084338));
#110485=CARTESIAN_POINT('Ctrl Pts',(6.901782407,3.31217565,-2.949234692));
#110486=CARTESIAN_POINT('Ctrl Pts',(6.778824099,3.266554913,-3.208978629));
#110487=CARTESIAN_POINT('Ctrl Pts',(6.92903438933913,3.3972605424113,-2.13331796710826));
#110488=CARTESIAN_POINT('Ctrl Pts',(6.92786132416957,3.39661302820565,-2.13711329805413));
#110489=CARTESIAN_POINT('Ctrl Pts',(6.926688259,3.395965514,-2.140908629));
#110490=CARTESIAN_POINT('Ctrl Pts',(6.891399557,3.376486685,-2.255081572));
#110491=CARTESIAN_POINT('Ctrl Pts',(6.852367211,3.357142857,-2.368029478));
#110492=CARTESIAN_POINT('Ctrl Pts',(6.761631518,3.31217565,-2.630591364));
#110493=CARTESIAN_POINT('Ctrl Pts',(6.651070221,3.266554913,-2.88544016));
#110494=CARTESIAN_POINT('',(7.08905203541566,3.39596551397713,-2.44853859249506));
#110495=CARTESIAN_POINT('Ctrl Pts',(6.88238908634082,3.30628897830882,-2.98038931465817));
#110496=CARTESIAN_POINT('Ctrl Pts',(6.92533207594406,3.32334891375396,-2.88122429529154));
#110497=CARTESIAN_POINT('Ctrl Pts',(6.96604639052516,3.34030767936816,-2.78132583629271));
#110498=CARTESIAN_POINT('Ctrl Pts',(7.00450417663027,3.35714285683815,-2.68084338096604));
#110499=CARTESIAN_POINT('Ctrl Pts',(7.03390855033864,3.37001483669515,-2.60401567187915));
#110500=CARTESIAN_POINT('Ctrl Pts',(7.06210313077174,3.38295904483419,-2.52656153579043));
#110501=CARTESIAN_POINT('Ctrl Pts',(7.08905203538231,3.39596551520487,-2.44853859255604));
#110502=CARTESIAN_POINT('',(7.0078701485236,3.3959655126796,-2.29472360679316));
#110503=CARTESIAN_POINT('Origin',(7.78457159844592E-13,3.48737837499967,
-3.23525928269675E-13));
#110504=CARTESIAN_POINT('',(6.88534350783937,3.48629831963854,-2.97355759564998));
#110505=CARTESIAN_POINT('Origin',(-0.178686657029109,3.62489371308647,0.0530570999432844));
#110506=CARTESIAN_POINT('Origin',(-0.177253922351563,3.48214200983984,0.0758309610416999));
#110507=CARTESIAN_POINT('Ctrl Pts',(7.405913077,3.266573167,-1.184251449));
#110508=CARTESIAN_POINT('Ctrl Pts',(7.341662513,3.330825242,-1.586053019));
#110509=CARTESIAN_POINT('Ctrl Pts',(7.23431823,3.395965514,-1.978544855));
#110510=CARTESIAN_POINT('Ctrl Pts',(7.11765493,3.266573167,-1.37894463));
#110511=CARTESIAN_POINT('Ctrl Pts',(7.042841452,3.330825242,-1.765106997));
#110512=CARTESIAN_POINT('Ctrl Pts',(6.926688259,3.395965514,-2.140908629));
#110513=CARTESIAN_POINT('',(7.23431823199865,3.39596551397695,-1.97854484767375));
#110514=CARTESIAN_POINT('',(7.08050324663787,3.39596551522658,-2.05972673465086));
#110515=CARTESIAN_POINT('',(7.36217825648022,3.30628897732936,-1.43119925979488));
#110516=CARTESIAN_POINT('Origin',(-0.17885161942905,3.48210502933222,0.0632390378060677));
#110517=CARTESIAN_POINT('Ctrl Pts',(7.1167653709526,3.26733592502957,-1.3835283382044));
#110518=CARTESIAN_POINT('Ctrl Pts',(7.15758713331703,3.27415053070575,-1.39157277193384));
#110519=CARTESIAN_POINT('Ctrl Pts',(7.19847314391143,3.28079893121671,-1.39956854473737));
#110520=CARTESIAN_POINT('Ctrl Pts',(7.28026402154608,3.29377261878572,-1.41545273291013));
#110521=CARTESIAN_POINT('Ctrl Pts',(7.32121752243622,3.3001056149233,-1.42335058548555));
#110522=CARTESIAN_POINT('Ctrl Pts',(7.36217825580228,3.30628897719839,-1.43119926343611));
#110523=CARTESIAN_POINT('Ctrl Pts',(7.45062785596414,3.3972605424113,-0.859192708687909));
#110524=CARTESIAN_POINT('Ctrl Pts',(7.45015260648208,3.39661302820565,-0.863274600343954));
#110525=CARTESIAN_POINT('Ctrl Pts',(7.449677357,3.395965514,-0.867356492));
#110526=CARTESIAN_POINT('Ctrl Pts',(7.435380677,3.376486685,-0.99014989));
#110527=CARTESIAN_POINT('Ctrl Pts',(7.417044844,3.357142857,-1.112405405));
#110528=CARTESIAN_POINT('Ctrl Pts',(7.37442085,3.31217565,-1.396604021));
#110529=CARTESIAN_POINT('Ctrl Pts',(7.310174507,3.266554913,-1.676707691));
#110530=CARTESIAN_POINT('Ctrl Pts',(7.22563771925764,3.3972605424113,-0.593904605882858));
#110531=CARTESIAN_POINT('Ctrl Pts',(7.22530796362882,3.39661302820565,-0.597863378441429));
#110532=CARTESIAN_POINT('Ctrl Pts',(7.224978208,3.395965514,-0.601822151));
#110533=CARTESIAN_POINT('Ctrl Pts',(7.215058343,3.376486685,-0.720911822));
#110534=CARTESIAN_POINT('Ctrl Pts',(7.201219013,3.357142857,-0.839609869));
#110535=CARTESIAN_POINT('Ctrl Pts',(7.16904771400001,3.31217565,-1.115538695));
#110536=CARTESIAN_POINT('Ctrl Pts',(7.115856237,3.266554913,-1.38819668));
#110537=CARTESIAN_POINT('',(7.44967735812331,3.39596551354851,-0.867356486601909));
#110538=CARTESIAN_POINT('Ctrl Pts',(7.36217825729832,3.30628897830878,-1.43119925674442));
#110539=CARTESIAN_POINT('Ctrl Pts',(7.38279971594842,3.32334891375392,-1.3251211870437));
#110540=CARTESIAN_POINT('Ctrl Pts',(7.40108693691377,3.34030767936786,-1.21880592444598));
#110541=CARTESIAN_POINT('Ctrl Pts',(7.41704484379493,3.35714285678366,-1.11240540636732));
#110542=CARTESIAN_POINT('Ctrl Pts',(7.42924607266077,3.37001483659878,-1.03105281569138));
#110543=CARTESIAN_POINT('Ctrl Pts',(7.44013112972881,3.3829590448342,-0.949348512339761));
#110544=CARTESIAN_POINT('Ctrl Pts',(7.44967735772577,3.39596551520482,-0.867356484217573));
#110545=CARTESIAN_POINT('',(7.33732778330786,3.3959655126796,-0.734589313430841));
#110546=CARTESIAN_POINT('Origin',(-6.09321620936853E-13,3.487378375,2.26056152963228E-14));
#110547=CARTESIAN_POINT('',(7.36359498823962,3.48629831963846,-1.42389214627077));
#110548=CARTESIAN_POINT('Origin',(-0.185914974277281,3.62489366151202,0.0134043705532033));
#110549=CARTESIAN_POINT('Origin',(-0.189411175297511,3.48214197762132,0.0359537120336828));
#110550=CARTESIAN_POINT('Ctrl Pts',(7.487346,3.266573167,0.435488086));
#110551=CARTESIAN_POINT('Ctrl Pts',(7.510973039,3.330825242,0.029268441));
#110552=CARTESIAN_POINT('Ctrl Pts',(7.490512549,3.395965514,-0.377123002));
#110553=CARTESIAN_POINT('Ctrl Pts',(7.247680448,3.266573167,0.183379743));
#110554=CARTESIAN_POINT('Ctrl Pts',(7.257629561,3.330825242,-0.209837049));
#110555=CARTESIAN_POINT('Ctrl Pts',(7.224978208,3.395965514,-0.601822151));
#110556=CARTESIAN_POINT('',(7.49051254917363,3.39596551397693,-0.377122994396843));
#110557=CARTESIAN_POINT('',(7.35774537900854,3.39596551522778,-0.489472568855644));
#110558=CARTESIAN_POINT('',(7.4977201548532,3.3062889773198,0.184912084007772));
#110559=CARTESIAN_POINT('Origin',(-0.188264802751972,3.48210504267805,0.0233127280800562));
#110560=CARTESIAN_POINT('Ctrl Pts',(7.24779704645756,3.26733592488707,0.178711969599105));
#110561=CARTESIAN_POINT('Ctrl Pts',(7.28939373438671,3.27415053059898,0.179631082648405));
#110562=CARTESIAN_POINT('Ctrl Pts',(7.33104270767518,3.28079893112976,0.180611530324912));
#110563=CARTESIAN_POINT('Ctrl Pts',(7.41433599124088,3.29377261874755,0.182681326643943));
#110564=CARTESIAN_POINT('Ctrl Pts',(7.45602982699191,3.30010561490455,0.183771913555003));
#110565=CARTESIAN_POINT('Ctrl Pts',(7.49772015497779,3.30628897718653,0.18491208017517));
#110566=CARTESIAN_POINT('Ctrl Pts',(7.46113735175124,3.3972605424113,0.762559489829848));
#110567=CARTESIAN_POINT('Ctrl Pts',(7.46155069937562,3.39661302820565,0.758470865914925));
#110568=CARTESIAN_POINT('Ctrl Pts',(7.461964047,3.395965514,0.754382242));
#110569=CARTESIAN_POINT('Ctrl Pts',(7.474398566,3.376486685,0.631386321));
#110570=CARTESIAN_POINT('Ctrl Pts',(7.482772737,3.357142857,0.50804741));
#110571=CARTESIAN_POINT('Ctrl Pts',(7.50223956900001,3.31217565,0.221330301));
#110572=CARTESIAN_POINT('Ctrl Pts',(7.49970928,3.266554913,-0.066035765));
#110573=CARTESIAN_POINT('Ctrl Pts',(7.18437825902062,3.3972605424113,0.973279075776289));
#110574=CARTESIAN_POINT('Ctrl Pts',(7.18490723201031,3.39661302820565,0.969341969388144));
#110575=CARTESIAN_POINT('Ctrl Pts',(7.185436205,3.395965514,0.965404863));
#110576=CARTESIAN_POINT('Ctrl Pts',(7.201349021,3.376486685,0.846966964));
#110577=CARTESIAN_POINT('Ctrl Pts',(7.213349817,3.357142857,0.728068964));
#110578=CARTESIAN_POINT('Ctrl Pts',(7.241247207,3.31217565,0.451675322));
#110579=CARTESIAN_POINT('Ctrl Pts',(7.24791272300001,3.266554913,0.173957335));
#110580=CARTESIAN_POINT('',(7.46196404772562,3.39596551355055,0.754382245272086));
#110581=CARTESIAN_POINT('Ctrl Pts',(7.49772015484195,3.30628897830888,0.184912087247228));
#110582=CARTESIAN_POINT('Ctrl Pts',(7.49505584584998,3.32334891375402,0.292943114560101));
#110583=CARTESIAN_POINT('Ctrl Pts',(7.49006088308634,3.34030767936768,0.400703997279967));
#110584=CARTESIAN_POINT('Ctrl Pts',(7.48277273681091,3.35714285673465,0.50804740855631));
#110585=CARTESIAN_POINT('Ctrl Pts',(7.4772003050315,3.37001483626404,0.590120922717139));
#110586=CARTESIAN_POINT('Ctrl Pts',(7.47026686602102,3.38295904433524,0.672254989142124));
#110587=CARTESIAN_POINT('Ctrl Pts',(7.46196404651734,3.39596551445283,0.754382245007042));
#110588=CARTESIAN_POINT('',(7.32370012505435,3.3959655126796,0.859893560554126));
#110589=CARTESIAN_POINT('Origin',(6.28837260041593E-13,3.487378375,9.13711380862159E-14));
#110590=CARTESIAN_POINT('',(7.49753295098508,3.48629831961751,0.192352916921865));
#110591=CARTESIAN_POINT('Origin',(-0.18444968183899,3.62489371393,-0.0268752585810736));
#110592=CARTESIAN_POINT('Origin',(-0.192711909498522,3.48214199176069,-0.00560467464567588));
#110593=CARTESIAN_POINT('Ctrl Pts',(7.218678946,3.266573167,2.034864682));
#110594=CARTESIAN_POINT('Ctrl Pts',(7.329078814,3.330825242,1.643221342));
#110595=CARTESIAN_POINT('Ctrl Pts',(7.39645882600001,3.395965514,1.241932705));
#110596=CARTESIAN_POINT('Ctrl Pts',(7.038812482,3.266573167,1.737129483));
#110597=CARTESIAN_POINT('Ctrl Pts',(7.133058978,3.330825242,1.355244646));
#110598=CARTESIAN_POINT('Ctrl Pts',(7.185436205,3.395965514,0.965404863000001));
#110599=CARTESIAN_POINT('',(7.39645882446883,3.39596551397696,1.24193271243835));
#110600=CARTESIAN_POINT('',(7.29094751435517,3.39596551522583,1.10366879156288));
#110601=CARTESIAN_POINT('',(7.2826769922493,3.30628897734568,1.79237714414339));
#110602=CARTESIAN_POINT('Origin',(-0.188874803198071,3.48210505377031,-0.0177036707167831));
#110603=CARTESIAN_POINT('Ctrl Pts',(7.03992978882774,3.26733592500448,1.73259590554336));
#110604=CARTESIAN_POINT('Ctrl Pts',(7.08035638700341,3.27415053067568,1.74243558812496));
#110605=CARTESIAN_POINT('Ctrl Pts',(7.12082086307071,3.2807989311798,1.75234641132533));
#110606=CARTESIAN_POINT('Ctrl Pts',(7.20172185073038,3.2937726187524,1.77227341039973));
#110607=CARTESIAN_POINT('Ctrl Pts',(7.24220646393772,3.30010561492267,1.78230144215772));
#110608=CARTESIAN_POINT('Ctrl Pts',(7.28267699309591,3.30628897720145,1.79237714041993));
#110609=CARTESIAN_POINT('Ctrl Pts',(7.1227723568037,3.3972605424113,2.34865525323209));
#110610=CARTESIAN_POINT('Ctrl Pts',(7.12405497390185,3.39661302820565,2.34475107661605));
#110611=CARTESIAN_POINT('Ctrl Pts',(7.125337591,3.395965514,2.3408469));
#110612=CARTESIAN_POINT('Ctrl Pts',(7.163921886,3.376486685,2.22339961));
#110613=CARTESIAN_POINT('Ctrl Pts',(7.198614493,3.357142857,2.104744493));
#110614=CARTESIAN_POINT('Ctrl Pts',(7.279261905,3.31217565,1.828915464));
#110615=CARTESIAN_POINT('Ctrl Pts',(7.338565982,3.266554913,1.547723919));
#110616=CARTESIAN_POINT('Ctrl Pts',(6.80718525625549,3.3972605424113,2.49495330789937));
#110617=CARTESIAN_POINT('Ctrl Pts',(6.80854822362774,3.39661302820565,2.49122196244969));
#110618=CARTESIAN_POINT('Ctrl Pts',(6.809911191,3.395965514,2.487490617));
#110619=CARTESIAN_POINT('Ctrl Pts',(6.850912621,3.376486685,2.375242516));
#110620=CARTESIAN_POINT('Ctrl Pts',(6.888192401,3.357142857,2.261704102));
#110621=CARTESIAN_POINT('Ctrl Pts',(6.974854028,3.31217565,1.997769504));
#110622=CARTESIAN_POINT('Ctrl Pts',(7.041064867,3.266554913,1.727977298));
#110623=CARTESIAN_POINT('',(7.12533759102965,3.39596551355058,2.34084690331928));
#110624=CARTESIAN_POINT('Ctrl Pts',(7.2826769914196,3.3062889783088,1.79237714723104));
#110625=CARTESIAN_POINT('Ctrl Pts',(7.25685149499618,3.32334891375393,1.89730972162753));
#110626=CARTESIAN_POINT('Ctrl Pts',(7.22880790718498,3.34030767936789,2.00147744554113));
#110627=CARTESIAN_POINT('Ctrl Pts',(7.19861449338123,3.35714285678744,2.10474449169613));
#110628=CARTESIAN_POINT('Ctrl Pts',(7.17552896304024,3.37001483635539,2.18370126497809));
#110629=CARTESIAN_POINT('Ctrl Pts',(7.15110122700862,3.38295904433124,2.26242459777464));
#110630=CARTESIAN_POINT('Ctrl Pts',(7.12533758989274,3.39596551444677,2.34084690279715));
#110631=CARTESIAN_POINT('',(6.96762438834504,3.3959655126796,2.41416876616258));
#110632=CARTESIAN_POINT('Origin',(7.45931094670027E-14,3.48737837499989,
3.07913416985883E-14));
#110633=CARTESIAN_POINT('',(7.28089460575553,3.48629831964464,1.79960377154734));
#110634=CARTESIAN_POINT('Origin',(-0.174359959206638,3.62489367356382,-0.0658981559459898));
#110635=CARTESIAN_POINT('Origin',(-0.187001520370689,3.4821419913019,-0.0469009982022248));
#110636=CARTESIAN_POINT('Ctrl Pts',(6.612474487,3.266573167,3.539093268));
#110637=CARTESIAN_POINT('Ctrl Pts',(6.804485009,3.330825242,3.180339039));
#110638=CARTESIAN_POINT('Ctrl Pts',(6.956554908,3.395965514,2.802917018));
#110639=CARTESIAN_POINT('Ctrl Pts',(6.50081746800001,3.266573167,3.209652979));
#110640=CARTESIAN_POINT('Ctrl Pts',(6.674954485,3.330825242,2.856956608));
#110641=CARTESIAN_POINT('Ctrl Pts',(6.809911191,3.395965514,2.487490617));
#110642=CARTESIAN_POINT('',(6.95655490512513,3.39596551397696,2.80291702502385));
#110643=CARTESIAN_POINT('',(6.88323304675614,3.39596551522583,2.64520382463995));
#110644=CARTESIAN_POINT('',(6.72710394729357,3.30628897734393,3.3160326417093));
#110645=CARTESIAN_POINT('Origin',(-0.180653151738133,3.48210507734314,-0.0578922113520686));
#110646=CARTESIAN_POINT('Ctrl Pts',(6.50288323813701,3.26733592504243,3.20546558201951));
#110647=CARTESIAN_POINT('Ctrl Pts',(6.54024944394122,3.27415053070218,3.22376574196963));
#110648=CARTESIAN_POINT('Ctrl Pts',(6.57763734891704,3.28079893119047,3.24214352186137));
#110649=CARTESIAN_POINT('Ctrl Pts',(6.65236354640081,3.29377267879171,3.278996130233));
#110650=CARTESIAN_POINT('Ctrl Pts',(6.68974631313084,3.30010573699289,3.29749290274777));
#110651=CARTESIAN_POINT('Ctrl Pts',(6.72710394902543,3.3062889772105,3.31603263823113));
#110652=CARTESIAN_POINT('Ctrl Pts',(6.45135444343917,3.3972605424113,3.82493050776523));
#110653=CARTESIAN_POINT('Ctrl Pts',(6.45344635621958,3.39661302820565,3.82139333338262));
#110654=CARTESIAN_POINT('Ctrl Pts',(6.455538269,3.395965514,3.817856159));
#110655=CARTESIAN_POINT('Ctrl Pts',(6.51846818000001,3.376486685,3.711449204));
#110656=CARTESIAN_POINT('Ctrl Pts',(6.577857036,3.357142857,3.603026063));
#110657=CARTESIAN_POINT('Ctrl Pts',(6.71591404400001,3.31217565,3.350982573));
#110658=CARTESIAN_POINT('Ctrl Pts',(6.834279495,3.266554913,3.089113754));
#110659=CARTESIAN_POINT('Ctrl Pts',(6.11169583714959,3.3972605424113,3.89996629798646));
#110660=CARTESIAN_POINT('Ctrl Pts',(6.1138290680748,3.39661302820565,3.89661518699323));
#110661=CARTESIAN_POINT('Ctrl Pts',(6.115962299,3.395965514,3.893264076));
#110662=CARTESIAN_POINT('Ctrl Pts',(6.180135162,3.376486685,3.792454368));
#110663=CARTESIAN_POINT('Ctrl Pts',(6.240950764,3.357142857,3.68958447));
#110664=CARTESIAN_POINT('Ctrl Pts',(6.382324428,3.31217565,3.450450204));
#110665=CARTESIAN_POINT('Ctrl Pts',(6.504984643,3.266554913,3.201198963));
#110666=CARTESIAN_POINT('',(6.45553826832072,3.39596551355059,3.81785616224398));
#110667=CARTESIAN_POINT('Ctrl Pts',(6.72710394570673,3.30628897830882,3.31603264454493));
#110668=CARTESIAN_POINT('Ctrl Pts',(6.67932483331376,3.32334891375395,3.41296023525716));
#110669=CARTESIAN_POINT('Ctrl Pts',(6.62954390754829,3.34030767936776,3.50866403323463));
#110670=CARTESIAN_POINT('Ctrl Pts',(6.5778570366183,3.35714285675868,3.60302606167889));
#110671=CARTESIAN_POINT('Ctrl Pts',(6.53833786072227,3.37001483630424,3.67517416255527));
#110672=CARTESIAN_POINT('Ctrl Pts',(6.49755804217794,3.38295904433065,3.74680574662116));
#110673=CARTESIAN_POINT('Ctrl Pts',(6.45553826732074,3.39596551444587,3.81785616148869));
#110674=CARTESIAN_POINT('',(6.28575027975988,3.3959655126796,3.8555601244127));
#110675=CARTESIAN_POINT('Origin',(-1.33703811910912E-12,3.48737837499989,
-6.96057794735694E-13));
#110676=CARTESIAN_POINT('',(6.72380972100027,3.48629831961384,3.32270715385137));
#110677=CARTESIAN_POINT('Origin',(-0.156117583026004,3.62489372625139,-0.101839827650431));
#110678=CARTESIAN_POINT('Origin',(-0.172547195397816,3.48214198959482,-0.0860042770115643));
#110679=CARTESIAN_POINT('Ctrl Pts',(5.69707807,3.266573167,4.877837785));
#110680=CARTESIAN_POINT('Ctrl Pts',(5.961721047,3.330825242,4.568747618));
#110681=CARTESIAN_POINT('Ctrl Pts',(6.191370215,3.395965514,4.232840047));
#110682=CARTESIAN_POINT('Ctrl Pts',(5.658851455,3.266573167,4.532096669));
#110683=CARTESIAN_POINT('Ctrl Pts',(5.90473653900001,3.330825242,4.225080454));
#110684=CARTESIAN_POINT('Ctrl Pts',(6.115962299,3.395965514,3.893264076));
#110685=CARTESIAN_POINT('',(6.1913702105932,3.39596551397696,4.23284005318075));
#110686=CARTESIAN_POINT('',(6.15366625278541,3.39596551522583,4.06305206788318));
#110687=CARTESIAN_POINT('',(5.85697899846951,3.30628897736477,4.68463413833494));
#110688=CARTESIAN_POINT('Origin',(-0.163984420983014,3.48210502581023,-0.0953737962201601));
#110689=CARTESIAN_POINT('Ctrl Pts',(5.66176909444807,3.2673359249139,4.52845124930181));
#110690=CARTESIAN_POINT('Ctrl Pts',(5.69432770575813,3.2741505306263,4.55435619189982));
#110691=CARTESIAN_POINT('Ctrl Pts',(5.72689082285085,3.28079893114848,4.58034160419976));
#110692=CARTESIAN_POINT('Ctrl Pts',(5.79194744092253,3.29377261878756,4.63239630226048));
#110693=CARTESIAN_POINT('Ctrl Pts',(5.8244796192849,3.30010561494795,4.65849654522998));
#110694=CARTESIAN_POINT('Ctrl Pts',(5.85697900078839,3.30628897723755,4.68463413548175));
#110695=CARTESIAN_POINT('Ctrl Pts',(5.47827836712809,3.39726054241128,5.12235626254302));
#110696=CARTESIAN_POINT('Ctrl Pts',(5.48108176006405,3.39661302820564,5.11935148477151));
#110697=CARTESIAN_POINT('Ctrl Pts',(5.483885153,3.395965514,5.116346707));
#110698=CARTESIAN_POINT('Ctrl Pts',(5.568218147,3.376486685,5.025955559));
#110699=CARTESIAN_POINT('Ctrl Pts',(5.649526295,3.357142857,4.932834139));
#110700=CARTESIAN_POINT('Ctrl Pts',(5.838537507,3.31217565,4.71636146100001));
#110701=CARTESIAN_POINT('Ctrl Pts',(6.010429695,3.266554913,4.486060063));
#110702=CARTESIAN_POINT('Ctrl Pts',(5.13043031307462,3.39726054241128,5.12262119754953));
#110703=CARTESIAN_POINT('Ctrl Pts',(5.13323406003731,3.39661302820564,5.11980701527477));
#110704=CARTESIAN_POINT('Ctrl Pts',(5.136037807,3.395965514,5.11699283300001));
#110705=CARTESIAN_POINT('Ctrl Pts',(5.220381451,3.376486685,5.032335269));
#110706=CARTESIAN_POINT('Ctrl Pts',(5.301889206,3.357142857,4.944943968));
#110707=CARTESIAN_POINT('Ctrl Pts',(5.49136443,3.31217565,4.741791688));
#110708=CARTESIAN_POINT('Ctrl Pts',(5.664738566,3.266554913,4.524736122));
#110709=CARTESIAN_POINT('',(5.48388514991963,3.39596551354712,5.11634671104307));
#110710=CARTESIAN_POINT('Ctrl Pts',(5.85697899656006,3.30628897830817,4.6846341407772));
#110711=CARTESIAN_POINT('Ctrl Pts',(5.7894803663614,3.32334891375353,4.76902452145373));
#110712=CARTESIAN_POINT('Ctrl Pts',(5.72028980334209,3.34030767936758,4.85178939038818));
#110713=CARTESIAN_POINT('Ctrl Pts',(5.64952629587156,3.35714285676466,4.93283413787115));
#110714=CARTESIAN_POINT('Ctrl Pts',(5.59542134620887,3.3700148365652,4.99480000303176));
#110715=CARTESIAN_POINT('Ctrl Pts',(5.5401962631029,3.38295904483422,5.0559904258671));
#110716=CARTESIAN_POINT('Ctrl Pts',(5.48388514753892,3.39596551520486,5.1163467125916));
#110717=CARTESIAN_POINT('',(5.30996147437299,3.3959655126796,5.11666977583958));
#110718=CARTESIAN_POINT('Origin',(-2.61509564003504E-13,3.48737837500056,
-2.7451999007333E-13));
#110719=CARTESIAN_POINT('',(5.85232696648482,3.48629831960878,4.69044444290798));
#110720=CARTESIAN_POINT('Origin',(-0.130574933793124,3.62489369821667,-0.133019419928523));
#110721=CARTESIAN_POINT('Origin',(-0.150024756310734,3.48214198979312,-0.121086082947772));
#110722=CARTESIAN_POINT('Ctrl Pts',(4.515292615,3.266573167,5.988500029));
#110723=CARTESIAN_POINT('Ctrl Pts',(4.840193635,3.330825242,5.74352663499999));
#110724=CARTESIAN_POINT('Ctrl Pts',(5.136683932,3.395965514,5.464840179));
#110725=CARTESIAN_POINT('Ctrl Pts',(4.552283837,3.266573167,5.642624555));
#110726=CARTESIAN_POINT('Ctrl Pts',(4.858419675,3.330825242,5.395644234));
#110727=CARTESIAN_POINT('Ctrl Pts',(5.136037807,3.395965514,5.116992833));
#110728=CARTESIAN_POINT('',(5.13668392641925,3.39596551397696,5.46484018414394));
#110729=CARTESIAN_POINT('',(5.13636086401175,3.39596551522583,5.29091651132793));
#110730=CARTESIAN_POINT('',(4.71298822131528,3.30628897735935,5.83418734891346));
#110731=CARTESIAN_POINT('Origin',(-0.139648144273157,3.48210502084463,-0.12839596685466));
#110732=CARTESIAN_POINT('Ctrl Pts',(4.55591692076069,3.2673359248366,5.63969156977355));
#110733=CARTESIAN_POINT('Ctrl Pts',(4.58214553288379,3.27415053054439,5.67199000816677));
#110734=CARTESIAN_POINT('Ctrl Pts',(4.6083612468954,3.28079893108282,5.70436800366454));
#110735=CARTESIAN_POINT('Ctrl Pts',(4.66070665598637,3.29377261873428,5.76919094168075));
#110736=CARTESIAN_POINT('Ctrl Pts',(4.68686746942877,3.30010561492014,5.80167443228908));
#110737=CARTESIAN_POINT('Ctrl Pts',(4.71298822421363,3.3062889772303,5.83418734660105));
#110738=CARTESIAN_POINT('Ctrl Pts',(4.24904408282165,3.3972605424113,6.18026633229042));
#110739=CARTESIAN_POINT('Ctrl Pts',(4.25242787241083,3.39661302820565,6.17793445114522));
#110740=CARTESIAN_POINT('Ctrl Pts',(4.255811662,3.395965514,6.17560257000001));
#110741=CARTESIAN_POINT('Ctrl Pts',(4.357604423,3.376486685,6.105453817));
#110742=CARTESIAN_POINT('Ctrl Pts',(4.457029984,3.357142857,6.031988372));
#110743=CARTESIAN_POINT('Ctrl Pts',(4.68815744500001,3.31217565,5.86120852900001));
#110744=CARTESIAN_POINT('Ctrl Pts',(4.905538882,3.266554913,5.673243189));
#110745=CARTESIAN_POINT('Ctrl Pts',(3.90927156911326,3.3972605424113,6.1057480230819));
#110746=CARTESIAN_POINT('Ctrl Pts',(3.91261473205663,3.39661302820565,6.10360235754095));
#110747=CARTESIAN_POINT('Ctrl Pts',(3.915957895,3.395965514,6.101456692));
#110748=CARTESIAN_POINT('Ctrl Pts',(4.016528506,3.376486685,6.036909765));
#110749=CARTESIAN_POINT('Ctrl Pts',(4.114917201,3.357142857,5.969083383));
#110750=CARTESIAN_POINT('Ctrl Pts',(4.343634335,3.31217565,5.811412262));
#110751=CARTESIAN_POINT('Ctrl Pts',(4.55961561000001,3.266554913,5.636701649));
#110752=CARTESIAN_POINT('',(4.25581165538039,3.39596551397713,6.17560257428537));
#110753=CARTESIAN_POINT('Ctrl Pts',(4.71298821889922,3.30628897830884,5.83418735089416));
#110754=CARTESIAN_POINT('Ctrl Pts',(4.6289262320271,3.32334891375397,5.90209452101998));
#110755=CARTESIAN_POINT('Ctrl Pts',(4.54356130583569,3.34030767936806,5.968050467354));
#110756=CARTESIAN_POINT('Ctrl Pts',(4.45702998493824,3.35714285681746,6.03198837130674));
#110757=CARTESIAN_POINT('Ctrl Pts',(4.39086914972084,3.37001483665857,6.08087454457559));
#110758=CARTESIAN_POINT('Ctrl Pts',(4.32378106640564,3.38295904483421,6.12876260887068));
#110759=CARTESIAN_POINT('Ctrl Pts',(4.2558116554647,3.39596551520487,6.17560257428695));
#110760=CARTESIAN_POINT('',(4.08588477174921,3.3959655126796,6.13852963549342));
#110761=CARTESIAN_POINT('Origin',(-3.0964814046186E-13,3.48737837500011,
-4.24573570745324E-13));
#110762=CARTESIAN_POINT('',(4.70719590771123,3.486298319625,5.83886176247301));
#110763=CARTESIAN_POINT('Origin',(-0.0989268748628985,3.62489373771985,
-0.15797920210728));
#110764=CARTESIAN_POINT('Origin',(-0.120487295497355,3.48214202377494,-0.150505976053753));
#110765=CARTESIAN_POINT('Ctrl Pts',(3.122377096,3.266573167,6.819146668));
#110766=CARTESIAN_POINT('Ctrl Pts',(3.492344149,3.330825242,6.649744731));
#110767=CARTESIAN_POINT('Ctrl Pts',(3.841812017,3.395965514,6.441310459));
#110768=CARTESIAN_POINT('Ctrl Pts',(3.232856486,3.266573167,6.489309589));
#110769=CARTESIAN_POINT('Ctrl Pts',(3.584928506,3.330825242,6.31391368600001));
#110770=CARTESIAN_POINT('Ctrl Pts',(3.915957895,3.395965514,6.101456692));
#110771=CARTESIAN_POINT('',(3.84181201039949,3.39596551397696,6.44131046274925));
#110772=CARTESIAN_POINT('',(3.87888494949472,3.39596551522583,6.27138357952356));
#110773=CARTESIAN_POINT('',(3.34862335342703,3.30628897733836,6.71094044364197));
#110774=CARTESIAN_POINT('Origin',(-0.1087818672081,3.48210502909658,-0.155414273976533));
#110775=CARTESIAN_POINT('Ctrl Pts',(3.23703513543889,3.26733592487956,6.4872261814177));
#110776=CARTESIAN_POINT('Ctrl Pts',(3.25570709551634,3.27415044581596,6.52440741390821));
#110777=CARTESIAN_POINT('Ctrl Pts',(3.27434932675907,3.28079875863233,6.56166350460611));
#110778=CARTESIAN_POINT('Ctrl Pts',(3.31153658116327,3.29377267903747,6.63622497162145));
#110779=CARTESIAN_POINT('Ctrl Pts',(3.33010297381103,3.30010573760448,6.67357321278013));
#110780=CARTESIAN_POINT('Ctrl Pts',(3.34862335692902,3.30628897720421,6.71094044191187));
#110781=CARTESIAN_POINT('Ctrl Pts',(2.82112921903796,3.39726054241128,6.94919401667821));
#110782=CARTESIAN_POINT('Ctrl Pts',(2.82493518301898,3.39661302820564,6.9476440683391));
#110783=CARTESIAN_POINT('Ctrl Pts',(2.828741147,3.395965514,6.94609412));
#110784=CARTESIAN_POINT('Ctrl Pts',(2.943233958,3.376486685,6.89946784));
#110785=CARTESIAN_POINT('Ctrl Pts',(3.056127904,3.357142857,6.849093534));
#110786=CARTESIAN_POINT('Ctrl Pts',(3.318564352,3.31217565,6.73199200100001));
#110787=CARTESIAN_POINT('Ctrl Pts',(3.571270523,3.266554913,6.595151768));
#110788=CARTESIAN_POINT('Ctrl Pts',(2.50531963238601,3.39726054241128,6.80337685771355));
#110789=CARTESIAN_POINT('Ctrl Pts',(2.50904588869301,3.39661302820564,6.80200003785678));
#110790=CARTESIAN_POINT('Ctrl Pts',(2.512772145,3.395965514,6.800623218));
#110791=CARTESIAN_POINT('Ctrl Pts',(2.624867152,3.376486685,6.759205071));
#110792=CARTESIAN_POINT('Ctrl Pts',(2.735536241,3.357142857,6.714115092));
#110793=CARTESIAN_POINT('Ctrl Pts',(2.992800725,3.31217565,6.609297658));
#110794=CARTESIAN_POINT('Ctrl Pts',(3.241290096,3.266554913,6.485101272));
#110795=CARTESIAN_POINT('',(2.82874113965045,3.39596551397711,6.9460941228516));
#110796=CARTESIAN_POINT('Ctrl Pts',(3.34862335043211,3.30628897830838,6.71094044494617));
#110797=CARTESIAN_POINT('Ctrl Pts',(3.25192865189507,3.32334891375364,6.75918914112259));
#110798=CARTESIAN_POINT('Ctrl Pts',(3.15438093133575,3.34030767936753,6.80525213843028));
#110799=CARTESIAN_POINT('Ctrl Pts',(3.05612790517976,3.35714285674499,6.849093533206));
#110800=CARTESIAN_POINT('Ctrl Pts',(2.9810047912196,3.37001483653036,6.88261415006091));
#110801=CARTESIAN_POINT('Ctrl Pts',(2.90519067147907,3.38295904483422,6.91496066358033));
#110802=CARTESIAN_POINT('Ctrl Pts',(2.82874113969565,3.39596551520471,6.94609412278089));
#110803=CARTESIAN_POINT('',(2.67075663844161,3.39596551267969,6.87335867193694));
#110804=CARTESIAN_POINT('Origin',(-1.02999206386123E-13,3.487378375,-1.96023752785379E-13));
#110805=CARTESIAN_POINT('',(3.34196159990722,3.48629831963972,6.71426039577534));
#110806=CARTESIAN_POINT('Origin',(-0.0626532617245851,3.62489367964053,
-0.175552255267503));
#110807=CARTESIAN_POINT('Origin',(-0.085315925288148,3.48214200458338,-0.172888223368134));
#110808=CARTESIAN_POINT('Ctrl Pts',(1.583462693,3.266573167,7.330937587));
#110809=CARTESIAN_POINT('Ctrl Pts',(1.981196531,3.330825242,7.24502815300001));
#110810=CARTESIAN_POINT('Ctrl Pts',(2.367301242,3.395965514,7.11659222000001));
#110811=CARTESIAN_POINT('Ctrl Pts',(1.762264358,3.266573167,7.032561719));
#110812=CARTESIAN_POINT('Ctrl Pts',(2.143810065,3.330825242,6.93695155199999));
#110813=CARTESIAN_POINT('Ctrl Pts',(2.512772145,3.395965514,6.800623218));
#110814=CARTESIAN_POINT('',(2.36730123479723,3.39596551397696,7.11659222239137));
#110815=CARTESIAN_POINT('',(2.44003668628186,3.39596551522583,6.95860772153104));
#110816=CARTESIAN_POINT('',(1.82768057874502,3.30628897738304,7.27389742193992));
#110817=CARTESIAN_POINT('Origin',(-0.0728291577683449,3.48210502662294,
-0.175165736868625));
#110818=CARTESIAN_POINT('Ctrl Pts',(1.76679318450052,3.26733592499019,7.03142530652031));
#110819=CARTESIAN_POINT('Ctrl Pts',(1.77703586598406,3.27415053065561,7.07175168348233));
#110820=CARTESIAN_POINT('Ctrl Pts',(1.78723343627441,3.28079893115732,7.11214484880847));
#110821=CARTESIAN_POINT('Ctrl Pts',(1.80752239786033,3.2937726187693,7.1929558207359));
#110822=CARTESIAN_POINT('Ctrl Pts',(1.81762584548155,3.30010561494277,7.23342167884843));
#110823=CARTESIAN_POINT('Ctrl Pts',(1.82768058216335,3.30628897725914,7.27389742110968));
#110824=CARTESIAN_POINT('Ctrl Pts',(1.26130148850622,3.3972605424113,7.39318511227826));
#110825=CARTESIAN_POINT('Ctrl Pts',(1.26535166425311,3.39661302820565,7.39248957063913));
#110826=CARTESIAN_POINT('Ctrl Pts',(1.26940184,3.395965514,7.39179402900001));
#110827=CARTESIAN_POINT('Ctrl Pts',(1.391241145,3.376486685,7.370870416));
#110828=CARTESIAN_POINT('Ctrl Pts',(1.51232468,3.357142857,7.345942694));
#110829=CARTESIAN_POINT('Ctrl Pts',(1.793798878,3.31217565,7.28799500900001));
#110830=CARTESIAN_POINT('Ctrl Pts',(2.070013524,3.266554913,7.208678382));
#110831=CARTESIAN_POINT('Ctrl Pts',(0.98422173280296,3.3972605424113,7.18288735118082));
#110832=CARTESIAN_POINT('Ctrl Pts',(0.98815684690148,3.39661302820565,7.18234375559041));
#110833=CARTESIAN_POINT('Ctrl Pts',(0.992091961000001,3.395965514,7.18180016));
#110834=CARTESIAN_POINT('Ctrl Pts',(1.110469927,3.376486685,7.16544746));
#110835=CARTESIAN_POINT('Ctrl Pts',(1.228244647,3.357142857,7.145202243));
#110836=CARTESIAN_POINT('Ctrl Pts',(1.502027081,3.31217565,7.09813964100001));
#110837=CARTESIAN_POINT('Ctrl Pts',(1.77140546,3.266554913,7.030264767));
#110838=CARTESIAN_POINT('',(1.26940183221709,3.39596551397713,7.39179403025101));
#110839=CARTESIAN_POINT('Ctrl Pts',(1.82768057589193,3.30628897830882,7.27389742284408));
#110840=CARTESIAN_POINT('Ctrl Pts',(1.72287450224015,3.32334891375395,7.30023158920542));
#110841=CARTESIAN_POINT('Ctrl Pts',(1.61770521034536,3.34030767936791,7.32424778261358));
#110842=CARTESIAN_POINT('Ctrl Pts',(1.51232468132775,3.35714285678788,7.34594269372665));
#110843=CARTESIAN_POINT('Ctrl Pts',(1.4317519622742,3.37001483660626,7.36253036886505));
#110844=CARTESIAN_POINT('Ctrl Pts',(1.35075679015301,3.38295904483418,7.37782284375787));
#110845=CARTESIAN_POINT('Ctrl Pts',(1.26940183226868,3.39596551520485,7.39179403014655));
#110846=CARTESIAN_POINT('',(1.13074689248646,3.3959655126796,7.28679709574352));
#110847=CARTESIAN_POINT('Origin',(-3.19622800448727E-13,3.48737837500067,
-1.20606649667288E-12));
#110848=CARTESIAN_POINT('',(1.82046088170413,3.48629831962542,7.27570767520948));
#110849=CARTESIAN_POINT('Origin',(-0.0234499208463798,3.6248937128969,-0.184916550395832));
#110850=CARTESIAN_POINT('Origin',(-0.0461554583641602,3.48214200263419,
-0.187186741471569));
#110851=CARTESIAN_POINT('Ctrl Pts',(-0.029492665,3.266573167,7.499942012));
#110852=CARTESIAN_POINT('Ctrl Pts',(0.377410366,3.330825242,7.501542112));
#110853=CARTESIAN_POINT('Ctrl Pts',(0.782098092,3.395965514,7.45911003900001));
#110854=CARTESIAN_POINT('Ctrl Pts',(0.209270708,3.266573167,7.246979079));
#110855=CARTESIAN_POINT('Ctrl Pts',(0.602449449000001,3.330825242,7.235625273));
#110856=CARTESIAN_POINT('Ctrl Pts',(0.992091961,3.395965514,7.18180016));
#110857=CARTESIAN_POINT('',(0.782098084443958,3.39596551397696,7.45911003971456));
#110858=CARTESIAN_POINT('',(0.887095018906516,3.39596551522583,7.32045510042018));
#110859=CARTESIAN_POINT('',(0.221277491332775,3.3062889773396,7.49673504102568));
#110860=CARTESIAN_POINT('Origin',(-0.0334709849852924,3.48210504334308,
-0.186726363592657));
#110861=CARTESIAN_POINT('Ctrl Pts',(0.213937948288746,3.26733592498261,
7.24684279884774));
#110862=CARTESIAN_POINT('Ctrl Pts',(0.215272182578208,3.27415053065561,
7.28842824134559));
#110863=CARTESIAN_POINT('Ctrl Pts',(0.21654800280224,3.28079893116271,7.33006921317212));
#110864=CARTESIAN_POINT('Ctrl Pts',(0.21899064948497,3.29377261875098,7.41335239647561));
#110865=CARTESIAN_POINT('Ctrl Pts',(0.220158920749398,3.30010561492063,
7.45504412795859));
#110866=CARTESIAN_POINT('Ctrl Pts',(0.221277495101919,3.3062889772091,7.49673504094391));
#110867=CARTESIAN_POINT('Ctrl Pts',(-0.357503297558374,3.39726054241128,
7.49147908942938));
#110868=CARTESIAN_POINT('Ctrl Pts',(-0.353398291779187,3.39661302820564,
7.49167047721469));
#110869=CARTESIAN_POINT('Ctrl Pts',(-0.349293286,3.395965514,7.491861865));
#110870=CARTESIAN_POINT('Ctrl Pts',(-0.225804558,3.376486685,7.497619283));
#110871=CARTESIAN_POINT('Ctrl Pts',(-0.102193166,3.357142857,7.499303738));
#110872=CARTESIAN_POINT('Ctrl Pts',(0.185157361,3.31217565,7.50321947));
#110873=CARTESIAN_POINT('Ctrl Pts',(0.471964993000001,3.266554913,7.48513520600001));
#110874=CARTESIAN_POINT('Ctrl Pts',(-0.582897279531815,3.39726054241128,
7.2265340158684));
#110875=CARTESIAN_POINT('Ctrl Pts',(-0.578937309265908,3.39661302820564,
7.2268490624342));
#110876=CARTESIAN_POINT('Ctrl Pts',(-0.574977339,3.395965514,7.227164109));
#110877=CARTESIAN_POINT('Ctrl Pts',(-0.455851638000001,3.376486685,7.236641489));
#110878=CARTESIAN_POINT('Ctrl Pts',(-0.336478302,3.357142857,7.242187677));
#110879=CARTESIAN_POINT('Ctrl Pts',(-0.058979681,3.31217565,7.25508050300001));
#110880=CARTESIAN_POINT('Ctrl Pts',(0.218691873,3.266554913,7.246700895));
#110881=CARTESIAN_POINT('',(-0.349293289221942,3.39596551355055,7.49186186590368));
#110882=CARTESIAN_POINT('Ctrl Pts',(0.221277488156341,3.3062889783084,7.49673504116422));
#110883=CARTESIAN_POINT('Ctrl Pts',(0.113260654782681,3.32334891375368,
7.49992332148587));
#110884=CARTESIAN_POINT('Ctrl Pts',(0.00538739075076868,3.34030767936764,
7.50076974060923));
#110885=CARTESIAN_POINT('Ctrl Pts',(-0.102193164471641,3.35714285676083,
7.49930373802083));
#110886=CARTESIAN_POINT('Ctrl Pts',(-0.184447995828977,3.37001483630999,
7.49818284974637));
#110887=CARTESIAN_POINT('Ctrl Pts',(-0.266836974385724,3.38295904433457,
7.49570622753082));
#110888=CARTESIAN_POINT('Ctrl Pts',(-0.349293289022749,3.39596551445177,
7.49186186468031));
#110889=CARTESIAN_POINT('',(-0.462135320593511,3.3959655126796,7.35951298649177));
#110890=CARTESIAN_POINT('Origin',(4.30970363562988E-15,3.48737837499922,
3.37403716077489E-13));
#110891=CARTESIAN_POINT('',(0.213837435912931,3.48629831963484,7.49695095004132));
#110892=CARTESIAN_POINT('Origin',(0.0168499294855356,3.62489369157933,-0.185634169748569));
#110893=CARTESIAN_POINT('Origin',(-0.00483675567923905,3.48214198196337,
-0.192732463258353));
#110894=CARTESIAN_POINT('Ctrl Pts',(0.431186334568378,2.49597508212359,
7.48817336585162));
#110895=CARTESIAN_POINT('Ctrl Pts',(0.445305298725013,2.4937079305618,7.48730692006504));
#110896=CARTESIAN_POINT('Ctrl Pts',(0.459424262881653,2.491440779,7.48644047427845));
#110897=CARTESIAN_POINT('Ctrl Pts',(0.868893215852792,2.425690334,7.46131238094947));
#110898=CARTESIAN_POINT('Ctrl Pts',(1.27317905959915,2.360702725,7.39167617769089));
#110899=CARTESIAN_POINT('Ctrl Pts',(0.178710628942825,2.4959750821236,7.24784866891599));
#110900=CARTESIAN_POINT('Ctrl Pts',(0.192378157971412,2.4937079305618,7.24746007945792));
#110901=CARTESIAN_POINT('Ctrl Pts',(0.206045687,2.491440779,7.24707149000001));
#110902=CARTESIAN_POINT('Ctrl Pts',(0.602422414,2.425690334,7.235801873));
#110903=CARTESIAN_POINT('Ctrl Pts',(0.99520558,2.360702725,7.181369358));
#110904=CARTESIAN_POINT('',(0.990540537957771,2.36147458141303,7.18201430105441));
#110905=CARTESIAN_POINT('Origin',(0.00477268321056754,2.55353552148333,
-0.196313054014068));
#110906=CARTESIAN_POINT('Ctrl Pts',(1.02346990277171,2.40074633455827,7.42983912041194));
#110907=CARTESIAN_POINT('Ctrl Pts',(1.01793509438388,2.3945034694007,7.38850162286635));
#110908=CARTESIAN_POINT('Ctrl Pts',(1.01241952112976,2.38811405787387,7.34716093692049));
#110909=CARTESIAN_POINT('Ctrl Pts',(1.00144325721363,2.37503353899324,7.26456531650046));
#110910=CARTESIAN_POINT('Ctrl Pts',(0.995976668043135,2.36833540947472,
7.2232660213906));
#110911=CARTESIAN_POINT('Ctrl Pts',(0.990540535864242,2.36147458185979,
7.18201430276513));
#110912=CARTESIAN_POINT('Ctrl Pts',(0.775652296,2.36069511,7.459783074));
#110913=CARTESIAN_POINT('Ctrl Pts',(1.181411227,2.42611337,7.41759312800001));
#110914=CARTESIAN_POINT('Ctrl Pts',(1.580200173,2.491440779,7.331641522));
#110915=CARTESIAN_POINT('Ctrl Pts',(0.985885713,2.36069511,7.182654757));
#110916=CARTESIAN_POINT('Ctrl Pts',(1.376570843,2.42611337,7.129029614));
#110917=CARTESIAN_POINT('Ctrl Pts',(1.759134602,2.491440779,7.033345253));
#110918=CARTESIAN_POINT('Origin',(-0.0353484116106306,2.41071388899553,
-0.196509256623171));
#110919=CARTESIAN_POINT('Ctrl Pts',(2.03084136166895,2.4959750823296,7.22041171789993));
#110920=CARTESIAN_POINT('Ctrl Pts',(2.04444397266669,2.4937079306648,7.21653036902814));
#110921=CARTESIAN_POINT('Ctrl Pts',(2.0580465836644,2.491440779,7.21264902015633));
#110922=CARTESIAN_POINT('Ctrl Pts',(2.45254058252075,2.425690334,7.10008468690785));
#110923=CARTESIAN_POINT('Ctrl Pts',(2.83240472203601,2.360702725,6.9451670333772));
#110924=CARTESIAN_POINT('Ctrl Pts',(1.73260569168895,2.4959750823296,7.03998049159346));
#110925=CARTESIAN_POINT('Ctrl Pts',(1.74587014684451,2.4937079306648,7.03666287229668));
#110926=CARTESIAN_POINT('Ctrl Pts',(1.759134602,2.491440779,7.033345253));
#110927=CARTESIAN_POINT('Ctrl Pts',(2.143821627,2.425690334,6.93712983500001));
#110928=CARTESIAN_POINT('Ctrl Pts',(2.515720358,2.360702725,6.79953315100001));
#110929=CARTESIAN_POINT('',(2.51130302647691,2.36147458139038,6.80116586227588));
#110930=CARTESIAN_POINT('Origin',(-0.037539604168903,2.55353595096111,-0.192746987546534));
#110931=CARTESIAN_POINT('Ctrl Pts',(2.59673753170465,2.40074633454041,7.03611783518101));
#110932=CARTESIAN_POINT('Ctrl Pts',(2.58244578398888,2.3945034693668,6.99693660543367));
#110933=CARTESIAN_POINT('Ctrl Pts',(2.56817213626816,2.38811405780995,6.95774812676184));
#110934=CARTESIAN_POINT('Ctrl Pts',(2.53969690108746,2.37503355114849,6.87944319142751));
#110935=CARTESIAN_POINT('Ctrl Pts',(2.52547997584348,2.36833541537222,6.84028456675752));
#110936=CARTESIAN_POINT('Ctrl Pts',(2.51130302489948,2.36147458172356,6.80116586364809));
#110937=CARTESIAN_POINT('Ctrl Pts',(2.361150828,2.36069511,7.118635176));
#110938=CARTESIAN_POINT('Ctrl Pts',(2.748353749,2.42611337,6.990205431));
#110939=CARTESIAN_POINT('Ctrl Pts',(3.119342177,2.491440779,6.820535491));
#110940=CARTESIAN_POINT('Ctrl Pts',(2.506894708,2.36069511,6.802791995));
#110941=CARTESIAN_POINT('Ctrl Pts',(2.876918016,2.42611337,6.666434823));
#110942=CARTESIAN_POINT('Ctrl Pts',(3.229968338,2.491440779,6.49074761));
#110943=CARTESIAN_POINT('Origin',(-0.0767657578313008,2.4107138892903,-0.184316315788779));
#110944=CARTESIAN_POINT('Ctrl Pts',(3.53553650424483,2.49597508246236,6.61503164336028));
#110945=CARTESIAN_POINT('Ctrl Pts',(3.54798671884754,2.49370793073122,6.60831687878963));
#110946=CARTESIAN_POINT('Ctrl Pts',(3.56043693345028,2.491440779,6.60160211421911));
#110947=CARTESIAN_POINT('Ctrl Pts',(3.92150987762511,2.425690334,6.40686492371389));
#110948=CARTESIAN_POINT('Ctrl Pts',(4.25919028771019,2.360702725,6.17390959719505));
#110949=CARTESIAN_POINT('Ctrl Pts',(3.20548603833938,2.49597508246235,6.50293065227997));
#110950=CARTESIAN_POINT('Ctrl Pts',(3.21772718816967,2.49370793073122,6.49683913113996));
#110951=CARTESIAN_POINT('Ctrl Pts',(3.229968338,2.491440779,6.49074761));
#110952=CARTESIAN_POINT('Ctrl Pts',(3.584978123,2.425690334,6.31408531600001));
#110953=CARTESIAN_POINT('Ctrl Pts',(3.918602849,2.360702725,6.099758332));
#110954=CARTESIAN_POINT('',(3.91463977674166,2.36147458139229,6.10230246674701));
#110955=CARTESIAN_POINT('Origin',(-0.0780968644945962,2.55353597351477,
-0.18017079869992));
#110956=CARTESIAN_POINT('Ctrl Pts',(4.04858459986332,2.40074633454433,6.31339549972611));
#110957=CARTESIAN_POINT('Ctrl Pts',(4.02620398823041,2.39450341615075,6.27820230870856));
#110958=CARTESIAN_POINT('Ctrl Pts',(4.00383978725195,2.38811403160265,6.24299860634402));
#110959=CARTESIAN_POINT('Ctrl Pts',(3.95919710097473,2.3750335425731,6.17264582572751));
#110960=CARTESIAN_POINT('Ctrl Pts',(3.93689462839103,2.36833541116663,6.13745895128617));
#110961=CARTESIAN_POINT('Ctrl Pts',(3.9146397755647,2.3614745817329,6.10230246879974));
#110962=CARTESIAN_POINT('Ctrl Pts',(3.836244571,2.36069511,6.444627809));
#110963=CARTESIAN_POINT('Ctrl Pts',(4.186786305,2.42611337,6.235963497));
#110964=CARTESIAN_POINT('Ctrl Pts',(4.512627207,2.491440779,5.99050879999999));
#110965=CARTESIAN_POINT('Ctrl Pts',(3.910684093,2.36069511,6.104838239));
#110966=CARTESIAN_POINT('Ctrl Pts',(4.2427437,2.42611337,5.89212495));
#110967=CARTESIAN_POINT('Ctrl Pts',(4.549772344,2.491440779,5.644649822));
#110968=CARTESIAN_POINT('Origin',(-0.114593353872106,2.41071384020386,-0.163504429967748));
#110969=CARTESIAN_POINT('Ctrl Pts',(4.87491388932696,2.49597508251598,5.70034004077986));
#110970=CARTESIAN_POINT('Ctrl Pts',(4.88562954905136,2.49370793075803,5.6911058354888));
#110971=CARTESIAN_POINT('Ctrl Pts',(4.89634520877575,2.491440779,5.68187163019773));
#110972=CARTESIAN_POINT('Ctrl Pts',(5.20711372828778,2.425690334,5.41406727834382));
#110973=CARTESIAN_POINT('Ctrl Pts',(5.48682085031788,2.360702725,5.11396701104611));
#110974=CARTESIAN_POINT('Ctrl Pts',(4.52848142063812,2.49597508251598,5.66181100249455));
#110975=CARTESIAN_POINT('Ctrl Pts',(4.53912688231906,2.49370793075803,5.65323041224728));
#110976=CARTESIAN_POINT('Ctrl Pts',(4.549772344,2.491440779,5.644649822));
#110977=CARTESIAN_POINT('Ctrl Pts',(4.858505026,2.425690334,5.395801184));
#110978=CARTESIAN_POINT('Ctrl Pts',(5.138255826,2.360702725,5.114765592));
#110979=CARTESIAN_POINT('',(5.13493232112417,2.36147458135829,5.11810219084302));
#110980=CARTESIAN_POINT('Origin',(-0.115002567746854,2.55353598996265,-0.159170189430652));
#110981=CARTESIAN_POINT('Ctrl Pts',(5.31112435157405,2.40074633451179,5.2954658080937));
#110982=CARTESIAN_POINT('Ctrl Pts',(5.2817017413302,2.39450346936203,5.26590683617229));
#110983=CARTESIAN_POINT('Ctrl Pts',(5.25229251438714,2.38811405780908,5.23633368521848));
#110984=CARTESIAN_POINT('Ctrl Pts',(5.19356970548814,2.37503355193669,5.17722249497532));
#110985=CARTESIAN_POINT('Ctrl Pts',(5.16422449208846,2.36833541577011,5.14765261981391));
#110986=CARTESIAN_POINT('Ctrl Pts',(5.13493232125685,2.36147458173208,5.11810219192745));
#110987=CARTESIAN_POINT('Ctrl Pts',(5.131959782,2.36069511,5.469276808));
#110988=CARTESIAN_POINT('Ctrl Pts',(5.429449386,2.42611337,5.190134841));
#110989=CARTESIAN_POINT('Ctrl Pts',(5.694906805,2.491440779,4.880372576));
#110990=CARTESIAN_POINT('Ctrl Pts',(5.131614236,2.36069511,5.121429033));
#110991=CARTESIAN_POINT('Ctrl Pts',(5.410183404,2.42611337,4.842305862));
#110992=CARTESIAN_POINT('Ctrl Pts',(5.65683405200001,2.491440779,4.534614483));
#110993=CARTESIAN_POINT('Origin',(-0.1470630375133,2.410713851561,-0.135047780565773));
#110994=CARTESIAN_POINT('Ctrl Pts',(5.98634572009426,2.49597508243042,4.51910687327443));
#110995=CARTESIAN_POINT('Ctrl Pts',(5.9948257723109,2.49370793071522,4.50778500869404));
#110996=CARTESIAN_POINT('Ctrl Pts',(6.00330582452749,2.491440779,4.4964631441136));
#110997=CARTESIAN_POINT('Ctrl Pts',(6.24923872929147,2.425690334,4.16811386365014));
#110998=CARTESIAN_POINT('Ctrl Pts',(6.45789376747328,2.360702725,3.81490101081275));
#110999=CARTESIAN_POINT('Ctrl Pts',(5.63973004538815,2.49597508243039,4.55595136341759));
#111000=CARTESIAN_POINT('Ctrl Pts',(5.64828204869408,2.49370793071524,4.54528292320879));
#111001=CARTESIAN_POINT('Ctrl Pts',(5.656834052,2.491440779,4.534614483));
#111002=CARTESIAN_POINT('Ctrl Pts',(5.904853635,2.425690334,4.225215387));
#111003=CARTESIAN_POINT('Ctrl Pts',(6.117649671,2.360702725,3.890612098));
#111004=CARTESIAN_POINT('',(6.11512113791658,2.36147458135708,3.89458514479899));
#111005=CARTESIAN_POINT('Origin',(-0.146530587764919,2.55353595661026,-0.130726585502198));
#111006=CARTESIAN_POINT('Ctrl Pts',(6.3253218314692,2.40074633450931,4.02992602048566));
#111007=CARTESIAN_POINT('Ctrl Pts',(6.29023280025013,2.39450346934649,4.00738311236295));
#111008=CARTESIAN_POINT('Ctrl Pts',(6.25515379150861,2.38811405781194,3.98482347979215));
#111009=CARTESIAN_POINT('Ctrl Pts',(6.18509674548874,2.37503355473301,3.93971795405276));
#111010=CARTESIAN_POINT('Ctrl Pts',(6.15008094986346,2.36833541717758,3.91714775456561));
#111011=CARTESIAN_POINT('Ctrl Pts',(6.11512113812636,2.36147458179299,3.89458514566824));
#111012=CARTESIAN_POINT('Ctrl Pts',(6.18771025700001,2.36069511,4.238188502));
#111013=CARTESIAN_POINT('Ctrl Pts',(6.418237448,2.42611337,3.901621248));
#111014=CARTESIAN_POINT('Ctrl Pts',(6.61089889,2.491440779,3.542035555));
#111015=CARTESIAN_POINT('Ctrl Pts',(6.1125958,2.36069511,3.898547497));
#111016=CARTESIAN_POINT('Ctrl Pts',(6.324648946,2.42611337,3.566065933));
#111017=CARTESIAN_POINT('Ctrl Pts',(6.499388487,2.491440779,3.21254561));
#111018=CARTESIAN_POINT('Origin',(-0.172655948842431,2.41071392620491,-0.100276158910808));
#111019=CARTESIAN_POINT('Ctrl Pts',(6.81786267752745,2.49597508234954,3.12656529063839));
#111020=CARTESIAN_POINT('Ctrl Pts',(6.82371060452681,2.49370793067477,3.11368516462101));
#111021=CARTESIAN_POINT('Ctrl Pts',(6.82955853152627,2.491440779,3.10080503860365));
#111022=CARTESIAN_POINT('Ctrl Pts',(6.99915627252464,2.425690334,2.72726407673456));
#111023=CARTESIAN_POINT('Ctrl Pts',(7.12700274970052,2.360702725,2.33745447875269));
#111024=CARTESIAN_POINT('Ctrl Pts',(6.4872711613576,2.49597508234954,3.23706050140318));
#111025=CARTESIAN_POINT('Ctrl Pts',(6.49332982417881,2.49370793067477,3.22480305570161));
#111026=CARTESIAN_POINT('Ctrl Pts',(6.499388487,2.491440779,3.21254561));
#111027=CARTESIAN_POINT('Ctrl Pts',(6.67509785,2.425690334,2.857063214));
#111028=CARTESIAN_POINT('Ctrl Pts',(6.810989017,2.360702725,2.484537907));
#111029=CARTESIAN_POINT('',(6.80937368675615,2.36147458134305,2.48896162520109));
#111030=CARTESIAN_POINT('Origin',(-0.171207237284685,2.55353595066915,-0.0961705711236122));
#111031=CARTESIAN_POINT('Ctrl Pts',(7.04375429273431,2.40074633454334,2.57595137079213));
#111032=CARTESIAN_POINT('Ctrl Pts',(7.00463956477323,2.39450346938452,2.56147860793005));
#111033=CARTESIAN_POINT('Ctrl Pts',(6.96553102956395,2.3881140578281,2.54698735705099));
#111034=CARTESIAN_POINT('Ctrl Pts',(6.88741540060877,2.37503353410922,2.51799652197757));
#111035=CARTESIAN_POINT('Ctrl Pts',(6.84836639463092,2.36833540700786,2.50348138654198));
#111036=CARTESIAN_POINT('Ctrl Pts',(6.80937368765278,2.36147458174416,2.48896162659278));
#111037=CARTESIAN_POINT('Ctrl Pts',(6.954130278,2.36069511,2.808927212));
#111038=CARTESIAN_POINT('Ctrl Pts',(7.10691586000001,2.42611337,2.430672182));
#111039=CARTESIAN_POINT('Ctrl Pts',(7.21777269,2.491440779,2.038076888));
#111040=CARTESIAN_POINT('Ctrl Pts',(6.807759179,2.36069511,2.493374213));
#111041=CARTESIAN_POINT('Ctrl Pts',(6.943380931,2.42611337,2.123080726));
#111042=CARTESIAN_POINT('Ctrl Pts',(7.03803874,2.491440779,1.740261674));
#111043=CARTESIAN_POINT('Origin',(-0.190175948612856,2.41071383979128,-0.0608158988614296));
#111044=CARTESIAN_POINT('Ctrl Pts',(7.33058395393016,2.49597508242676,1.58782899156932));
#111045=CARTESIAN_POINT('Ctrl Pts',(7.33352631333063,2.49370793071342,1.57399286405882));
#111046=CARTESIAN_POINT('Ctrl Pts',(7.33646867273096,2.491440779,1.56015673654826));
#111047=CARTESIAN_POINT('Ctrl Pts',(7.42180104761325,2.425690334,1.1588904536096));
#111048=CARTESIAN_POINT('Ctrl Pts',(7.46286100361699,2.360702725,0.750711174245291));
#111049=CARTESIAN_POINT('Ctrl Pts',(7.03147468762232,2.4959750824268,1.76680828812868));
#111050=CARTESIAN_POINT('Ctrl Pts',(7.03475671381116,2.4937079307134,1.75353498106434));
#111051=CARTESIAN_POINT('Ctrl Pts',(7.03803874,2.491440779,1.740261674));
#111052=CARTESIAN_POINT('Ctrl Pts',(7.133221908,2.425690334,1.35531794));
#111053=CARTESIAN_POINT('Ctrl Pts',(7.185854086,2.360702725,0.962289484));
#111054=CARTESIAN_POINT('',(7.18522749011262,2.36147458135454,0.966957026736748));
#111055=CARTESIAN_POINT('Origin',(-0.187878458689477,2.55353595748085,-0.0571176862103746));
#111056=CARTESIAN_POINT('Ctrl Pts',(7.43282863154981,2.40074633450367,1.00152809855962));
#111057=CARTESIAN_POINT('Ctrl Pts',(7.39151716795935,2.3945034693615,0.995802211064734));
#111058=CARTESIAN_POINT('Ctrl Pts',(7.35020777802992,2.38811405783215,0.9900569365596));
#111059=CARTESIAN_POINT('Ctrl Pts',(7.26768633535209,2.37503354348097,0.978536450388198));
#111060=CARTESIAN_POINT('Ctrl Pts',(7.22642991707173,2.36833541165497,0.972755048399386));
#111061=CARTESIAN_POINT('Ctrl Pts',(7.18522749108296,2.36147458180083,0.966957027865269));
#111062=CARTESIAN_POINT('Ctrl Pts',(7.395382895,2.36069511,1.248323608));
#111063=CARTESIAN_POINT('Ctrl Pts',(7.463282786,2.42611337,0.846067586));
#111064=CARTESIAN_POINT('Ctrl Pts',(7.487151461,2.491440779,0.43882001));
#111065=CARTESIAN_POINT('Ctrl Pts',(7.184599304,2.36069511,0.971613522));
#111066=CARTESIAN_POINT('Ctrl Pts',(7.237448142,2.42611337,0.580822623));
#111067=CARTESIAN_POINT('Ctrl Pts',(7.247598124,2.491440779,0.186605037));
#111068=CARTESIAN_POINT('Origin',(-0.198803195775803,2.41071385645573,-0.0185118389587539));
#111069=CARTESIAN_POINT('Ctrl Pts',(7.50053527191827,2.4959750822797,-0.0251524287664814));
#111070=CARTESIAN_POINT('Ctrl Pts',(7.50043448216075,2.49370793063989,-0.0392975951575152));
#111071=CARTESIAN_POINT('Ctrl Pts',(7.50033369240322,2.491440779,-0.0534427615485497));
#111072=CARTESIAN_POINT('Ctrl Pts',(7.49741065395632,2.425690334,-0.463671600436942));
#111073=CARTESIAN_POINT('Ctrl Pts',(7.4497641723792,2.360702725,-0.87113455191811));
#111074=CARTESIAN_POINT('Ctrl Pts',(7.24689427289999,2.4959750822797,0.213942082389185));
#111075=CARTESIAN_POINT('Ctrl Pts',(7.24724619844996,2.49370793063989,0.200273559694589));
#111076=CARTESIAN_POINT('Ctrl Pts',(7.247598124,2.491440779,0.186605037));
#111077=CARTESIAN_POINT('Ctrl Pts',(7.257804438,2.425690334,-0.209800494));
#111078=CARTESIAN_POINT('Ctrl Pts',(7.22471660500001,2.360702725,-0.604954526));
#111079=CARTESIAN_POINT('',(7.2251080422661,2.36147458140569,-0.600261409189046));
#111080=CARTESIAN_POINT('Origin',(-0.195764717093502,2.55353597250716,-0.0153939945248779));
#111081=CARTESIAN_POINT('Ctrl Pts',(7.47435216496847,2.4007463345685,-0.619725515399625));
#111082=CARTESIAN_POINT('Ctrl Pts',(7.43277529405746,2.39450341687222,-0.616436763641023));
#111083=CARTESIAN_POINT('Ctrl Pts',(7.39119681606624,2.38811403197589,-0.613167433927704));
#111084=CARTESIAN_POINT('Ctrl Pts',(7.30812833342854,2.37503355199203,-0.606678923770133));
#111085=CARTESIAN_POINT('Ctrl Pts',(7.26659360799277,2.36833541581745,-0.60345624713839));
#111086=CARTESIAN_POINT('Ctrl Pts',(7.22510804348048,2.36147458176016,-0.60026140759842));
#111087=CARTESIAN_POINT('Ctrl Pts',(7.490835629,2.36069511,-0.370650221));
#111088=CARTESIAN_POINT('Ctrl Pts',(7.470674903,2.42611337,-0.77809819));
#111089=CARTESIAN_POINT('Ctrl Pts',(7.406439351,2.491440779,-1.180955603));
#111090=CARTESIAN_POINT('Ctrl Pts',(7.225495552,2.36069511,-0.595578738));
#111091=CARTESIAN_POINT('Ctrl Pts',(7.19310032100001,2.42611337,-0.988594101));
#111092=CARTESIAN_POINT('Ctrl Pts',(7.118267874,2.491440779,-1.375777044));
#111093=CARTESIAN_POINT('Origin',(-0.198134895535887,2.41071388758876,0.0246577965306941));
#111094=CARTESIAN_POINT('Ctrl Pts',(7.31976989665382,2.49597508238335,-1.63695774767015));
#111095=CARTESIAN_POINT('Ctrl Pts',(7.31663067059766,2.49370793069171,-1.65075054141746));
#111096=CARTESIAN_POINT('Ctrl Pts',(7.31349144454157,2.491440779,-1.66454333516476));
#111097=CARTESIAN_POINT('Ctrl Pts',(7.22244967133344,2.425690334,-2.06455288459223));
#111098=CARTESIAN_POINT('Ctrl Pts',(7.08832464740652,2.360702725,-2.45224699364326));
#111099=CARTESIAN_POINT('Ctrl Pts',(7.12345713531641,2.49597508238334,-1.34892781573121));
#111100=CARTESIAN_POINT('Ctrl Pts',(7.12086250465821,2.49370793069171,-1.36235242986561));
#111101=CARTESIAN_POINT('Ctrl Pts',(7.118267874,2.491440779,-1.375777044));
#111102=CARTESIAN_POINT('Ctrl Pts',(7.043020099,2.425690334,-1.76510889));
#111103=CARTESIAN_POINT('Ctrl Pts',(6.925759405,2.360702725,-2.143911534));
#111104=CARTESIAN_POINT('',(6.92715057170216,2.36147458141132,-2.13941228764283));
#111105=CARTESIAN_POINT('Origin',(-0.19449701381967,2.55353595734725,0.0270495149301808));
#111106=CARTESIAN_POINT('Ctrl Pts',(7.1663832978545,2.4007463345425,-2.21200145241878));
#111107=CARTESIAN_POINT('Ctrl Pts',(7.12648545170843,2.39450341625723,-2.19985179039366));
#111108=CARTESIAN_POINT('Ctrl Pts',(7.08658186676122,2.38811403167542,-2.18772075264125));
#111109=CARTESIAN_POINT('Ctrl Pts',(7.0068502209734,2.37503353593916,-2.16352664264567));
#111110=CARTESIAN_POINT('Ctrl Pts',(6.96697938663502,2.36833540792811,-2.15145058793241));
#111111=CARTESIAN_POINT('Ctrl Pts',(6.92715057360104,2.36147458177965,-2.13941228563727));
#111112=CARTESIAN_POINT('Ctrl Pts',(7.236025213,2.36069511,-1.972292858));
#111113=CARTESIAN_POINT('Ctrl Pts',(7.128746565,2.42611337,-2.365880959));
#111114=CARTESIAN_POINT('Ctrl Pts',(6.979410369,2.491440779,-2.745511045));
#111115=CARTESIAN_POINT('Ctrl Pts',(6.928535658,2.36069511,-2.134922397));
#111116=CARTESIAN_POINT('Ctrl Pts',(6.812411124,2.42611337,-2.511785262));
#111117=CARTESIAN_POINT('Ctrl Pts',(6.65609533,2.491440779,-2.873829319));
#111118=CARTESIAN_POINT('Origin',(-0.188201868405449,2.41071387521461,0.0666744331180874));
#111119=CARTESIAN_POINT('Ctrl Pts',(6.79674021710689,2.49597508252471,-3.17222074089898));
#111120=CARTESIAN_POINT('Ctrl Pts',(6.79070934129096,2.49370793076239,-3.18501622638997));
#111121=CARTESIAN_POINT('Ctrl Pts',(6.78467846547508,2.491440779,-3.19781171188092));
#111122=CARTESIAN_POINT('Ctrl Pts',(6.60977496972601,2.425690334,-3.56889797041118));
#111123=CARTESIAN_POINT('Ctrl Pts',(6.3954429407611,2.360702725,-3.91869509163868));
#111124=CARTESIAN_POINT('Ctrl Pts',(6.66693506001777,2.49597508252471,-2.84872334773867));
#111125=CARTESIAN_POINT('Ctrl Pts',(6.6615151950089,2.49370793076239,-2.86127633336936));
#111126=CARTESIAN_POINT('Ctrl Pts',(6.65609533,2.491440779,-2.873829319));
#111127=CARTESIAN_POINT('Ctrl Pts',(6.498911968,2.425690334,-3.237882756));
#111128=CARTESIAN_POINT('Ctrl Pts',(6.302961392,2.360702725,-3.582621622));
#111129=CARTESIAN_POINT('',(6.30528724043917,2.36147458137357,-3.57852662396335));
#111130=CARTESIAN_POINT('Origin',(-0.184134812498761,2.55353595767753,0.0682281691905767));
#111131=CARTESIAN_POINT('Ctrl Pts',(6.52332231319455,2.40074633455067,-3.70084665970845));
#111132=CARTESIAN_POINT('Ctrl Pts',(6.48696938400318,2.3945034693982,-3.68040436650925));
#111133=CARTESIAN_POINT('Ctrl Pts',(6.45060637304175,2.38811405784751,-3.65997876206446));
#111134=CARTESIAN_POINT('Ctrl Pts',(6.37793976229787,2.37503355046822,-3.61921031372038));
#111135=CARTESIAN_POINT('Ctrl Pts',(6.34159703770279,2.36833541508829,-3.59884551561224));
#111136=CARTESIAN_POINT('Ctrl Pts',(6.30528724136624,2.3614745818094,-3.57852662358162));
#111137=CARTESIAN_POINT('Ctrl Pts',(6.64286630100001,2.36069511,-3.481713272));
#111138=CARTESIAN_POINT('Ctrl Pts',(6.45348596100001,2.42611337,-3.843037764));
#111139=CARTESIAN_POINT('Ctrl Pts',(6.226031915,2.491440779,-4.181689442));
#111140=CARTESIAN_POINT('Ctrl Pts',(6.307605137,2.36069511,-3.574439458));
#111141=CARTESIAN_POINT('Ctrl Pts',(6.11318115400001,2.42611337,-3.917528137));
#111142=CARTESIAN_POINT('Ctrl Pts',(5.882691166,2.491440779,-4.23750453));
#111143=CARTESIAN_POINT('Origin',(-0.169468734258499,2.41071389137068,0.105573437157334));
#111144=CARTESIAN_POINT('Ctrl Pts',(5.95590251870123,2.49597508252968,-4.55915421965815));
#111145=CARTESIAN_POINT('Ctrl Pts',(5.94726199025258,2.49370793076488,-4.57035409378245));
#111146=CARTESIAN_POINT('Ctrl Pts',(5.93862146180392,2.491440779,-4.58155396790664));
#111147=CARTESIAN_POINT('Ctrl Pts',(5.6880345362443,2.425690334,-4.90636535416808));
#111148=CARTESIAN_POINT('Ctrl Pts',(5.40351742966767,2.360702725,-5.20190936238205));
#111149=CARTESIAN_POINT('Ctrl Pts',(5.89867451079924,2.49597508252968,-4.21531574393402));
#111150=CARTESIAN_POINT('Ctrl Pts',(5.8906828383996,2.49370793076488,-4.22641013696702));
#111151=CARTESIAN_POINT('Ctrl Pts',(5.882691166,2.491440779,-4.23750453));
#111152=CARTESIAN_POINT('Ctrl Pts',(5.650921937,2.425690334,-4.559256823));
#111153=CARTESIAN_POINT('Ctrl Pts',(5.385443911,2.360702725,-4.853812304));
#111154=CARTESIAN_POINT('',(5.38859568422889,2.36147458137419,-4.8503130343453));
#111155=CARTESIAN_POINT('Origin',(-0.165164502110791,2.55353553498122,0.10621801655163));
#111156=CARTESIAN_POINT('Ctrl Pts',(5.57523802689835,2.4007463345603,-5.0166443907419));
#111157=CARTESIAN_POINT('Ctrl Pts',(5.54412949788782,2.39450346940797,-4.98886522176393));
#111158=CARTESIAN_POINT('Ctrl Pts',(5.5130075352218,2.38811405785102,-4.96110018408175));
#111159=CARTESIAN_POINT('Ctrl Pts',(5.45080379357579,2.37503354047566,-4.90566366378113));
#111160=CARTESIAN_POINT('Ctrl Pts',(5.41968859661357,2.3683354101439,-4.87796239430515));
#111161=CARTESIAN_POINT('Ctrl Pts',(5.3885956866165,2.3614745817378,-4.85031303352163));
#111162=CARTESIAN_POINT('Ctrl Pts',(5.739094344,2.36069511,-4.828332643));
#111163=CARTESIAN_POINT('Ctrl Pts',(5.476467525,2.42611337,-5.140498395));
#111164=CARTESIAN_POINT('Ctrl Pts',(5.181531129,2.491440779,-5.42233668900001));
#111165=CARTESIAN_POINT('Ctrl Pts',(5.39173801,2.36069511,-4.846819703));
#111166=CARTESIAN_POINT('Ctrl Pts',(5.128105628,2.42611337,-5.14009175));
#111167=CARTESIAN_POINT('Ctrl Pts',(4.834218902,2.491440779,-5.403038739));
#111168=CARTESIAN_POINT('Origin',(-0.142811494539211,2.41071387228298,0.139535953330484));
#111169=CARTESIAN_POINT('Ctrl Pts',(4.83657343703978,2.4959750822612,-5.73290671538372));
#111170=CARTESIAN_POINT('Ctrl Pts',(4.82572727809061,2.49370793063064,-5.74198728391551));
#111171=CARTESIAN_POINT('Ctrl Pts',(4.81488111914144,2.491440779,-5.75106785244731));
#111172=CARTESIAN_POINT('Ctrl Pts',(4.50032792921937,2.425690334,-6.01441654679815));
#111173=CARTESIAN_POINT('Ctrl Pts',(4.15892944980332,2.360702725,-6.24188813278773));
#111174=CARTESIAN_POINT('Ctrl Pts',(4.85459849703071,2.4959750822612,-5.38480466216928));
#111175=CARTESIAN_POINT('Ctrl Pts',(4.84440869951533,2.49370793063064,-5.39392170058464));
#111176=CARTESIAN_POINT('Ctrl Pts',(4.83421890200001,2.491440779,-5.403038739));
#111177=CARTESIAN_POINT('Ctrl Pts',(4.538701076,2.425690334,-5.667445109));
#111178=CARTESIAN_POINT('Ctrl Pts',(4.216109057,2.360702725,-5.898044118));
#111179=CARTESIAN_POINT('',(4.21993938413277,2.36147458134235,-5.89530419657684));
#111180=CARTESIAN_POINT('Origin',(-0.138467891967822,2.55353595480635,0.13923832245939));
#111181=CARTESIAN_POINT('Ctrl Pts',(4.36646180685913,2.40074633452991,-6.09786940580669));
#111182=CARTESIAN_POINT('Ctrl Pts',(4.34205207570985,2.39450341760044,-6.06405200370533));
#111183=CARTESIAN_POINT('Ctrl Pts',(4.3176264968511,2.38811403232265,-6.03024594398858));
#111184=CARTESIAN_POINT('Ctrl Pts',(4.26879433193897,2.3750335349705,-5.96273363615639));
#111185=CARTESIAN_POINT('Ctrl Pts',(4.24436155596373,2.3683354074509,-5.9289911744189));
#111186=CARTESIAN_POINT('Ctrl Pts',(4.21993938576903,2.36147458177666,-5.89530419695903));
#111187=CARTESIAN_POINT('Ctrl Pts',(4.566968713,2.36069511,-5.94918454700001));
#111188=CARTESIAN_POINT('Ctrl Pts',(4.243375555,2.42611337,-6.19759503400001));
#111189=CARTESIAN_POINT('Ctrl Pts',(3.894747705,2.491440779,-6.409441498));
#111190=CARTESIAN_POINT('Ctrl Pts',(4.223759206,2.36069511,-5.892568045));
#111191=CARTESIAN_POINT('Ctrl Pts',(3.903245582,2.42611337,-6.122310386));
#111192=CARTESIAN_POINT('Ctrl Pts',(3.559703934,2.491440779,-6.315932861));
#111193=CARTESIAN_POINT('Origin',(-0.109476389224066,2.41071387441741,0.166973696340317));
#111194=CARTESIAN_POINT('Ctrl Pts',(3.49109155737623,2.49597508229257,-6.63859486236934));
#111195=CARTESIAN_POINT('Ctrl Pts',(3.47854692169554,2.49370793064629,-6.64513152876386));
#111196=CARTESIAN_POINT('Ctrl Pts',(3.46600228601477,2.491440779,-6.65166819515836));
#111197=CARTESIAN_POINT('Ctrl Pts',(3.10219099014338,2.425690334,-6.84124030647186));
#111198=CARTESIAN_POINT('Ctrl Pts',(2.71987455125237,2.360702725,-6.99000315145689));
#111199=CARTESIAN_POINT('Ctrl Pts',(3.58352685309772,2.49597508229257,-6.30250609716514));
#111200=CARTESIAN_POINT('Ctrl Pts',(3.57161539354887,2.49370793064629,-6.30921947908256));
#111201=CARTESIAN_POINT('Ctrl Pts',(3.559703934,2.491440779,-6.315932861));
#111202=CARTESIAN_POINT('Ctrl Pts',(3.214255597,2.425690334,-6.51062996));
#111203=CARTESIAN_POINT('Ctrl Pts',(2.84963363,2.360702725,-6.666489944));
#111204=CARTESIAN_POINT('',(2.85396340807876,2.36147458133375,-6.66463748776735));
#111205=CARTESIAN_POINT('Origin',(-0.105298459875244,2.55353594867096,0.165749496562412));
#111206=CARTESIAN_POINT('Ctrl Pts',(2.95351468598881,2.4007463345525,-6.893964824483));
#111207=CARTESIAN_POINT('Ctrl Pts',(2.93694538232913,2.39450341751036,-6.8556906831616));
#111208=CARTESIAN_POINT('Ctrl Pts',(2.92035816359941,2.38811403227426,-6.8174242132272));
#111209=CARTESIAN_POINT('Ctrl Pts',(2.88718082282725,2.375033536788,-6.74099284469345));
#111210=CARTESIAN_POINT('Ctrl Pts',(2.87057290089408,2.36833540831626,-6.70278693262186));
#111211=CARTESIAN_POINT('Ctrl Pts',(2.85396340960552,2.36147458173546,-6.66463748835739));
#111212=CARTESIAN_POINT('Ctrl Pts',(3.181296702,2.36069511,-6.79185919300001));
#111213=CARTESIAN_POINT('Ctrl Pts',(2.81186806,2.42611337,-6.964899017));
#111214=CARTESIAN_POINT('Ctrl Pts',(2.425850208,2.491440779,-7.096847946));
#111215=CARTESIAN_POINT('Ctrl Pts',(2.858282117,2.36069511,-6.662786455));
#111216=CARTESIAN_POINT('Ctrl Pts',(2.49587411,2.42611337,-6.81825659200001));
#111217=CARTESIAN_POINT('Ctrl Pts',(2.118741167,2.491440779,-6.933500982));
#111218=CARTESIAN_POINT('Origin',(-0.071022573616687,2.41071391683862,0.186604418640867));
#111219=CARTESIAN_POINT('Ctrl Pts',(1.98237012011077,2.49597508279149,-7.23386969147354));
#111220=CARTESIAN_POINT('Ctrl Pts',(1.96871357948591,2.49370793089575,-7.23755680881284));
#111221=CARTESIAN_POINT('Ctrl Pts',(1.95505703886105,2.491440779,-7.24124392615215));
#111222=CARTESIAN_POINT('Ctrl Pts',(1.55899904868913,2.425690334,-7.34817527304667));
#111223=CARTESIAN_POINT('Ctrl Pts',(1.15364134058453,2.360702725,-7.41127339159409));
#111224=CARTESIAN_POINT('Ctrl Pts',(2.14489347970249,2.49597508279145,-6.9255093509647));
#111225=CARTESIAN_POINT('Ctrl Pts',(2.13181732335125,2.49370793089577,-6.92950516648233));
#111226=CARTESIAN_POINT('Ctrl Pts',(2.118741167,2.491440779,-6.933500982));
#111227=CARTESIAN_POINT('Ctrl Pts',(1.739515099,2.425690334,-7.04938499));
#111228=CARTESIAN_POINT('Ctrl Pts',(1.349912501,2.360702725,-7.12321811));
#111229=CARTESIAN_POINT('',(1.35453927523772,2.36147458134696,-7.12233973723395));
#111230=CARTESIAN_POINT('Origin',(-0.0672054225599605,2.55353596763685,
0.184510496211542));
#111231=CARTESIAN_POINT('Ctrl Pts',(1.40246450071486,2.40074633455926,-7.36770611019184));
#111232=CARTESIAN_POINT('Ctrl Pts',(1.39451038722834,2.39450341760035,-7.32676488706728));
#111233=CARTESIAN_POINT('Ctrl Pts',(1.38653712826532,2.38811403233655,-7.28582730402155));
#111234=CARTESIAN_POINT('Ctrl Pts',(1.37056594056082,2.37503353713036,-7.20405071257824));
#111235=CARTESIAN_POINT('Ctrl Pts',(1.36255944421315,2.36833540852492,-7.16316782030079));
#111236=CARTESIAN_POINT('Ctrl Pts',(1.35453927636171,2.36147458179984,-7.12233973828936));
#111237=CARTESIAN_POINT('Ctrl Pts',(1.646870792,2.36069511,-7.316954052));
#111238=CARTESIAN_POINT('Ctrl Pts',(1.24888074,2.42611337,-7.40653206300001));
#111239=CARTESIAN_POINT('Ctrl Pts',(0.843522651,2.491440779,-7.45241367199999));
#111240=CARTESIAN_POINT('Ctrl Pts',(1.359154932,2.36069511,-7.121460375));
#111241=CARTESIAN_POINT('Ctrl Pts',(0.971798339000001,2.42611337,-7.195388698));
#111242=CARTESIAN_POINT('Ctrl Pts',(0.578708417,2.491440779,-7.226866303));
#111243=CARTESIAN_POINT('Origin',(-0.0292476493498572,2.4107139102224,0.197509355480732));
#111244=CARTESIAN_POINT('Ctrl Pts',(0.363937711287557,2.49319894677753,
-7.49137623344886));
#111245=CARTESIAN_POINT('Ctrl Pts',(0.358459121765824,2.49231986288877,
-7.49163435721352));
#111246=CARTESIAN_POINT('Ctrl Pts',(0.352980532244091,2.491440779,-7.49189248097817));
#111247=CARTESIAN_POINT('Ctrl Pts',(-0.0567866169785492,2.425690334,-7.51119866166007));
#111248=CARTESIAN_POINT('Ctrl Pts',(-0.466215022234156,2.360702725,-7.48569914995376));
#111249=CARTESIAN_POINT('Ctrl Pts',(0.589277985104296,2.49319894677753,
-7.22601991980783));
#111250=CARTESIAN_POINT('Ctrl Pts',(0.583993201052148,2.49231986288877,
-7.22644311140391));
#111251=CARTESIAN_POINT('Ctrl Pts',(0.578708417,2.491440779,-7.226866303));
#111252=CARTESIAN_POINT('Ctrl Pts',(0.183436808,2.425690334,-7.258518613));
#111253=CARTESIAN_POINT('Ctrl Pts',(-0.212929036,2.360702725,-7.246872513));
#111254=CARTESIAN_POINT('',(-0.208221609147027,2.36147458135266,-7.24700929638663));
#111255=CARTESIAN_POINT('Origin',(-0.0259698947458284,2.55353597210639,
0.194643709376892));
#111256=CARTESIAN_POINT('Ctrl Pts',(-0.214163364830837,2.40074633010132,
-7.49694161690444));
#111257=CARTESIAN_POINT('Ctrl Pts',(-0.213130371432346,2.39450346485659,
-7.4552480234001));
#111258=CARTESIAN_POINT('Ctrl Pts',(-0.212116845861083,2.38811405782144,
-7.41355336951517));
#111259=CARTESIAN_POINT('Ctrl Pts',(-0.210135085308225,2.37503355527668,
-7.33025528930787));
#111260=CARTESIAN_POINT('Ctrl Pts',(-0.209165779495856,2.36833541741468,
-7.28860699457912));
#111261=CARTESIAN_POINT('Ctrl Pts',(-0.208221608534118,2.3614745817406,
-7.2470092971132));
#111262=CARTESIAN_POINT('Ctrl Pts',(0.035439035,2.36069511,-7.499916271));
#111263=CARTESIAN_POINT('Ctrl Pts',(-0.372502856,2.42611337,-7.50184390200001));
#111264=CARTESIAN_POINT('Ctrl Pts',(-0.778247087,2.491440779,-7.459512817));
#111265=CARTESIAN_POINT('Ctrl Pts',(-0.203524827,2.36069511,-7.24714272300001));
#111266=CARTESIAN_POINT('Ctrl Pts',(-0.597717642,2.42611337,-7.236072426));
#111267=CARTESIAN_POINT('Ctrl Pts',(-0.988384095,2.491440779,-7.182311389));
#111268=CARTESIAN_POINT('Origin',(0.0138950876763513,2.41071430159107,0.199181670296006));
#111269=CARTESIAN_POINT('Ctrl Pts',(-1.2382726553927,2.49597508222491,-7.39765792981161));
#111270=CARTESIAN_POINT('Ctrl Pts',(-1.25221517461467,2.49370793061246,
-7.39527003456471));
#111271=CARTESIAN_POINT('Ctrl Pts',(-1.26615769383664,2.491440779,-7.39288213931789));
#111272=CARTESIAN_POINT('Ctrl Pts',(-1.67050949731884,2.425690334,-7.32362996657868));
#111273=CARTESIAN_POINT('Ctrl Pts',(-2.06489640117708,2.360702725,-7.21069098516172));
#111274=CARTESIAN_POINT('Ctrl Pts',(-0.961293303489874,2.49597508222487,
-7.18603945174254));
#111275=CARTESIAN_POINT('Ctrl Pts',(-0.974838699244942,2.49370793061248,
-7.18417542037124));
#111276=CARTESIAN_POINT('Ctrl Pts',(-0.988384094999999,2.491440779,-7.182311389));
#111277=CARTESIAN_POINT('Ctrl Pts',(-1.381218784,2.425690334,-7.128251973));
#111278=CARTESIAN_POINT('Ctrl Pts',(-1.765814248,2.360702725,-7.031671213));
#111279=CARTESIAN_POINT('',(-1.76124628360346,2.36147458140683,-7.03281675504062));
#111280=CARTESIAN_POINT('Origin',(0.0164799599871354,2.55353599730958,0.195676067966756));
#111281=CARTESIAN_POINT('Ctrl Pts',(-1.82077719099447,2.40074633449545,
-7.27562852393234));
#111282=CARTESIAN_POINT('Ctrl Pts',(-1.81080545823754,2.39450346933559,
-7.23513176665407));
#111283=CARTESIAN_POINT('Ctrl Pts',(-1.8008525031392,2.38811405780701,-7.1946297599833));
#111284=CARTESIAN_POINT('Ctrl Pts',(-1.78101041491868,2.37503353213395,
-7.11370501954481));
#111285=CARTESIAN_POINT('Ctrl Pts',(-1.77111063743132,2.36833540606227,
-7.07323888724965));
#111286=CARTESIAN_POINT('Ctrl Pts',(-1.76124628168249,2.36147458179985,
-7.03281675696655));
#111287=CARTESIAN_POINT('Ctrl Pts',(-1.577649813,2.36069511,-7.332190741));
#111288=CARTESIAN_POINT('Ctrl Pts',(-1.976468632,2.42611337,-7.24637785700001));
#111289=CARTESIAN_POINT('Ctrl Pts',(-2.363626857,2.491440779,-7.11781343400001));
#111290=CARTESIAN_POINT('Ctrl Pts',(-1.756687991,2.36069511,-7.033956732));
#111291=CARTESIAN_POINT('Ctrl Pts',(-2.13928501,2.42611337,-6.93840544900001));
#111292=CARTESIAN_POINT('Ctrl Pts',(-2.509260865,2.491440779,-6.801919576));
#111293=CARTESIAN_POINT('Origin',(0.0563876163794358,2.41071387880783,0.191535565088941));
#111294=CARTESIAN_POINT('Ctrl Pts',(-2.7996003098369,2.49597508240935,-6.95851278037652));
#111295=CARTESIAN_POINT('Ctrl Pts',(-2.81270353432863,2.49370793070468,
-6.95318348310568));
#111296=CARTESIAN_POINT('Ctrl Pts',(-2.82580675882035,2.491440779,-6.94785418583485));
#111297=CARTESIAN_POINT('Ctrl Pts',(-3.20581787121601,2.425690334,-6.79329740590194));
#111298=CARTESIAN_POINT('Ctrl Pts',(-3.56670568702239,2.360702725,-6.5982173485554));
#111299=CARTESIAN_POINT('Ctrl Pts',(-2.48360486337345,2.49597508240936,
-6.81138419847442));
#111300=CARTESIAN_POINT('Ctrl Pts',(-2.49643286418676,2.49370793070468,
-6.8066518872372));
#111301=CARTESIAN_POINT('Ctrl Pts',(-2.509260865,2.491440779,-6.801919576));
#111302=CARTESIAN_POINT('Ctrl Pts',(-2.881290121,2.425690334,-6.664676193));
#111303=CARTESIAN_POINT('Ctrl Pts',(-3.236131948,2.360702725,-6.487676781));
#111304=CARTESIAN_POINT('',(-3.23191703699043,2.36147458135554,-6.48977751941193));
#111305=CARTESIAN_POINT('Origin',(0.058159215223072,2.55353598666095,0.187558505738186));
#111306=CARTESIAN_POINT('Ctrl Pts',(-3.34225349900583,2.40074633454303,
-6.7141150980915));
#111307=CARTESIAN_POINT('Ctrl Pts',(-3.32380929400625,2.39450346938553,
-6.67670876023693));
#111308=CARTESIAN_POINT('Ctrl Pts',(-3.30538229912372,2.38811405783145,
-6.63929325890826));
#111309=CARTESIAN_POINT('Ctrl Pts',(-3.26860772365964,2.37503354743692,
-6.56452604360058));
#111310=CARTESIAN_POINT('Ctrl Pts',(-3.2502403522527,2.36833541359946,-6.52713410004322));
#111311=CARTESIAN_POINT('Ctrl Pts',(-3.23191703633811,2.36147458180118,
-6.48977752054085));
#111312=CARTESIAN_POINT('Ctrl Pts',(-3.116969508,2.36069511,-6.821620122));
#111313=CARTESIAN_POINT('Ctrl Pts',(-3.488016932,2.42611337,-6.652079238));
#111314=CARTESIAN_POINT('Ctrl Pts',(-3.838486062,2.491440779,-6.443293005));
#111315=CARTESIAN_POINT('Ctrl Pts',(-3.227710377,2.36069511,-6.491870741));
#111316=CARTESIAN_POINT('Ctrl Pts',(-3.580821789,2.42611337,-6.316306345));
#111317=CARTESIAN_POINT('Ctrl Pts',(-3.912807385,2.491440779,-6.103477563));
#111318=CARTESIAN_POINT('Origin',(0.0962436524464921,2.41071388612422,0.174935665357462));
#111319=CARTESIAN_POINT('Ctrl Pts',(-4.23002176612037,2.49597508244881,
-6.19399530803162));
#111320=CARTESIAN_POINT('Ctrl Pts',(-4.2416730032187,2.49370793072441,-6.18597380075739));
#111321=CARTESIAN_POINT('Ctrl Pts',(-4.25332424031696,2.491440779,-6.17795229348326));
#111322=CARTESIAN_POINT('Ctrl Pts',(-4.59122576484367,2.425690334,-5.94531780891545));
#111323=CARTESIAN_POINT('Ctrl Pts',(-4.90173977726586,2.360702725,-5.67721840209496));
#111324=CARTESIAN_POINT('Ctrl Pts',(-3.88978582024371,2.49597508244882,
-6.11823618995914));
#111325=CARTESIAN_POINT('Ctrl Pts',(-3.90129660262183,2.49370793072441,
-6.11085687647957));
#111326=CARTESIAN_POINT('Ctrl Pts',(-3.912807385,2.491440779,-6.103477563));
#111327=CARTESIAN_POINT('Ctrl Pts',(-4.246635534,2.425690334,-5.889467561));
#111328=CARTESIAN_POINT('Ctrl Pts',(-4.55513171500001,2.360702725,-5.640325794));
#111329=CARTESIAN_POINT('',(-4.55146694340284,2.3614745814012,-5.64328349840463));
#111330=CARTESIAN_POINT('Origin',(0.0971190746755296,2.55353596056757,0.170671054071678));
#111331=CARTESIAN_POINT('Ctrl Pts',(-4.70744974767337,2.40074633452359,
-5.8386571123626));
#111332=CARTESIAN_POINT('Ctrl Pts',(-4.68139528364874,2.39450341726951,
-5.80609000094193));
#111333=CARTESIAN_POINT('Ctrl Pts',(-4.65535599040997,2.38811403216799,
-5.77351065652692));
#111334=CARTESIAN_POINT('Ctrl Pts',(-4.60336851064569,2.37503353882064,
-5.70839698870585));
#111335=CARTESIAN_POINT('Ctrl Pts',(-4.57739241382645,2.36833540936728,
-5.67582771278331));
#111336=CARTESIAN_POINT('Ctrl Pts',(-4.55146694245506,2.36147458181044,
-5.64328350085495));
#111337=CARTESIAN_POINT('Ctrl Pts',(-4.510543174,2.36069511,-5.992078127));
#111338=CARTESIAN_POINT('Ctrl Pts',(-4.83646943600001,2.42611337,-5.746736787));
#111339=CARTESIAN_POINT('Ctrl Pts',(-5.133861925,2.491440779,-5.46749135700001));
#111340=CARTESIAN_POINT('Ctrl Pts',(-4.547808613,2.36069511,-5.64623209));
#111341=CARTESIAN_POINT('Ctrl Pts',(-4.854923321,2.42611337,-5.398863776));
#111342=CARTESIAN_POINT('Ctrl Pts',(-5.133395382,2.491440779,-5.119643723));
#111343=CARTESIAN_POINT('Origin',(0.131599621200214,2.41071388183387,0.150156326072586));
#111344=CARTESIAN_POINT('Ctrl Pts',(-5.46265210513852,2.49597508244516,
-5.13985349893491));
#111345=CARTESIAN_POINT('Ctrl Pts',(-5.47230655587297,2.49370793072262,
-5.12951485847333));
#111346=CARTESIAN_POINT('Ctrl Pts',(-5.48196100660741,2.491440779,-5.11917621801159));
#111347=CARTESIAN_POINT('Ctrl Pts',(-5.76195304493989,2.425690334,-4.81934175864285));
#111348=CARTESIAN_POINT('Ctrl Pts',(-6.00757396462814,2.360702725,-4.49075903227299));
#111349=CARTESIAN_POINT('Ctrl Pts',(-5.1140847172565,2.49597508244516,-5.13900625734142));
#111350=CARTESIAN_POINT('Ctrl Pts',(-5.12374004962819,2.49370793072262,
-5.12932499017063));
#111351=CARTESIAN_POINT('Ctrl Pts',(-5.133395382,2.491440779,-5.119643723));
#111352=CARTESIAN_POINT('Ctrl Pts',(-5.413412989,2.425690334,-4.838873972));
#111353=CARTESIAN_POINT('Ctrl Pts',(-5.661138586,2.360702725,-4.529239441));
#111354=CARTESIAN_POINT('',(-5.65819531292125,2.36147458136162,-4.53291581459397));
#111355=CARTESIAN_POINT('Origin',(0.131537820879867,2.55353600730791,0.145803241101173));
#111356=CARTESIAN_POINT('Ctrl Pts',(-5.85253087835358,2.40074633455458,
-4.69019000897543));
#111357=CARTESIAN_POINT('Ctrl Pts',(-5.82008458820373,2.39450341754668,
-4.66398523911349));
#111358=CARTESIAN_POINT('Ctrl Pts',(-5.78765048252088,2.38811403232733,
-4.6377652594527));
#111359=CARTESIAN_POINT('Ctrl Pts',(-5.72288093750899,2.37503354102958,
-4.58534969261362));
#111360=CARTESIAN_POINT('Ctrl Pts',(-5.69051071011439,2.36833541046703,
-4.5591259566022));
#111361=CARTESIAN_POINT('Ctrl Pts',(-5.65819531327409,2.36147458182936,
-4.5329158161715));
#111362=CARTESIAN_POINT('Ctrl Pts',(-5.693208854,2.36069511,-4.882353219));
#111363=CARTESIAN_POINT('Ctrl Pts',(-5.95877400500001,2.42611337,-4.57268331000001));
#111364=CARTESIAN_POINT('Ctrl Pts',(-6.18918411,2.491440779,-4.23603589));
#111365=CARTESIAN_POINT('Ctrl Pts',(-5.655256373,2.36069511,-4.536581902));
#111366=CARTESIAN_POINT('Ctrl Pts',(-5.902014034,2.42611337,-4.228976338));
#111367=CARTESIAN_POINT('Ctrl Pts',(-6.113951515,2.491440779,-3.896421033));
#111368=CARTESIAN_POINT('Origin',(0.160802047155614,2.41071386843307,0.11835571462205));
#111369=CARTESIAN_POINT('Ctrl Pts',(-6.43985490420489,2.49597508252274,
-3.84537785260529));
#111370=CARTESIAN_POINT('Ctrl Pts',(-6.44706113725208,2.49370793076141,
-3.83320550208452));
#111371=CARTESIAN_POINT('Ctrl Pts',(-6.45426737029939,2.491440779,-3.82103315156376));
#111372=CARTESIAN_POINT('Ctrl Pts',(-6.66325780389173,2.425690334,-3.46801864364053));
#111373=CARTESIAN_POINT('Ctrl Pts',(-6.83250066956373,2.360702725,-3.09431676174519));
#111374=CARTESIAN_POINT('Ctrl Pts',(-6.09925469507655,2.49597508252274,
-3.91948210457872));
#111375=CARTESIAN_POINT('Ctrl Pts',(-6.10660310503828,2.49370793076141,
-3.90795156878934));
#111376=CARTESIAN_POINT('Ctrl Pts',(-6.113951515,2.491440779,-3.896421033));
#111377=CARTESIAN_POINT('Ctrl Pts',(-6.32706527000001,2.425690334,-3.562020014));
#111378=CARTESIAN_POINT('Ctrl Pts',(-6.50243690800001,2.360702725,-3.206370886));
#111379=CARTESIAN_POINT('',(-6.5003527587057,2.36147458134442,-3.21059402478539));
#111380=CARTESIAN_POINT('Origin',(0.159805770113787,2.55353595460724,0.114117596466036));
#111381=CARTESIAN_POINT('Ctrl Pts',(-6.72395416956975,2.40074633454225,
-3.32241483335559));
#111382=CARTESIAN_POINT('Ctrl Pts',(-6.68663319934288,2.39450341663434,
-3.30379770709918));
#111383=CARTESIAN_POINT('Ctrl Pts',(-6.64932086725947,2.38811403186844,
-3.28516311144202));
#111384=CARTESIAN_POINT('Ctrl Pts',(-6.57479782539573,2.37503354490892,
-3.24789654151664));
#111385=CARTESIAN_POINT('Ctrl Pts',(-6.53754705603456,2.36833541236912,
-3.22924453809376));
#111386=CARTESIAN_POINT('Ctrl Pts',(-6.50035275940381,2.36147458181569,
-3.21059402611262));
#111387=CARTESIAN_POINT('Ctrl Pts',(-6.609666415,2.36069511,-3.5443349));
#111388=CARTESIAN_POINT('Ctrl Pts',(-6.802452925,2.42611337,-3.184816244));
#111389=CARTESIAN_POINT('Ctrl Pts',(-6.955106924,2.491440779,-2.806508092));
#111390=CARTESIAN_POINT('Ctrl Pts',(-6.49827063,2.36069511,-3.214806186));
#111391=CARTESIAN_POINT('Ctrl Pts',(-6.673133131,2.42611337,-2.861346666));
#111392=CARTESIAN_POINT('Ctrl Pts',(-6.808626071,2.491440779,-2.491006026));
#111393=CARTESIAN_POINT('Origin',(0.182487905438553,2.41071429564125,0.0810218689469716));
#111394=CARTESIAN_POINT('Ctrl Pts',(-7.11593724508701,2.49597508225771,
-2.37109661029227));
#111395=CARTESIAN_POINT('Ctrl Pts',(-7.12035830459428,2.49370793062889,
-2.35765971624731));
#111396=CARTESIAN_POINT('Ctrl Pts',(-7.12477936410143,2.491440779,-2.34422282220235));
#111397=CARTESIAN_POINT('Ctrl Pts',(-7.25299603309939,2.425690334,-1.95453483150014));
#111398=CARTESIAN_POINT('Ctrl Pts',(-7.33794723805909,2.360702725,-1.55318767885172));
#111399=CARTESIAN_POINT('Ctrl Pts',(-6.79923030378816,2.49597508225771,
-2.51668732283746));
#111400=CARTESIAN_POINT('Ctrl Pts',(-6.80392818739409,2.49370793062889,
-2.50384667441869));
#111401=CARTESIAN_POINT('Ctrl Pts',(-6.80862607100001,2.491440779,-2.491006026));
#111402=CARTESIAN_POINT('Ctrl Pts',(-6.944871011,2.425690334,-2.11860996));
#111403=CARTESIAN_POINT('Ctrl Pts',(-7.039688507,2.360702725,-1.733575992));
#111404=CARTESIAN_POINT('',(-7.03856093436333,2.36147458134285,-1.73814842650295));
#111405=CARTESIAN_POINT('Origin',(0.180601220225389,2.55353597284607,0.0770959809789962));
#111406=CARTESIAN_POINT('Ctrl Pts',(-7.28097283682833,2.40074633457552,
-1.79928723337112));
#111407=CARTESIAN_POINT('Ctrl Pts',(-7.24052262012437,2.39450346940029,
-1.78912835643461));
#111408=CARTESIAN_POINT('Ctrl Pts',(-7.20007656101851,2.38811405783542,
-1.77895043030641));
#111409=CARTESIAN_POINT('Ctrl Pts',(-7.11928449131764,2.37503355074156,
-1.75857535170139));
#111410=CARTESIAN_POINT('Ctrl Pts',(-7.07889497548673,2.36833541519939,
-1.74836723103845));
#111411=CARTESIAN_POINT('Ctrl Pts',(-7.03856093503845,2.36147458176162,
-1.73814842746186));
#111412=CARTESIAN_POINT('Ctrl Pts',(-7.217063321,2.36069511,-2.040587421));
#111413=CARTESIAN_POINT('Ctrl Pts',(-7.328056705,2.42611337,-1.648030711));
#111414=CARTESIAN_POINT('Ctrl Pts',(-7.39581666999999,2.491440779,-1.245751095));
#111415=CARTESIAN_POINT('Ctrl Pts',(-7.03743297500001,2.36069511,-1.742709706));
#111416=CARTESIAN_POINT('Ctrl Pts',(-7.132223939,2.42611337,-1.359923604));
#111417=CARTESIAN_POINT('Ctrl Pts',(-7.184936839,2.491440779,-0.969114346));
#111418=CARTESIAN_POINT('Origin',(0.195638787465489,2.41071431194102,0.0398981238600597));
#111419=CARTESIAN_POINT('Ctrl Pts',(-7.45928626917492,2.49597508222446,
-0.785945526233097));
#111420=CARTESIAN_POINT('Ctrl Pts',(-7.46071543173044,2.49370793061227,
-0.771872382326965));
#111421=CARTESIAN_POINT('Ctrl Pts',(-7.462144594286,2.491440779,-0.757799238420837));
#111422=CARTESIAN_POINT('Ctrl Pts',(-7.50359222994364,2.425690334,-0.349659143433354));
#111423=CARTESIAN_POINT('Ctrl Pts',(-7.50027954846603,2.360702725,0.0605667337499607));
#111424=CARTESIAN_POINT('Ctrl Pts',(-7.18128145937083,2.49597508222447,
-0.996215040427868));
#111425=CARTESIAN_POINT('Ctrl Pts',(-7.18310914918541,2.49370793061227,
-0.982664693213935));
#111426=CARTESIAN_POINT('Ctrl Pts',(-7.184936839,2.491440779,-0.969114346));
#111427=CARTESIAN_POINT('Ctrl Pts',(-7.237942301,2.425690334,-0.576136058));
#111428=CARTESIAN_POINT('Ctrl Pts',(-7.24777209600001,2.360702725,-0.179721011));
#111429=CARTESIAN_POINT('',(-7.24765382360903,2.36147458135816,-0.184428939767084));
#111430=CARTESIAN_POINT('Origin',(0.192952530454964,2.55353598637138,0.0364696205559954));
#111431=CARTESIAN_POINT('Ctrl Pts',(-7.49754130656375,2.40074633455833,
-0.192026962126391));
#111432=CARTESIAN_POINT('Ctrl Pts',(-7.45585293515902,2.39450346937786,
-0.190801194864945));
#111433=CARTESIAN_POINT('Ctrl Pts',(-7.41416452940256,2.38811405784962,
-0.189555930013006));
#111434=CARTESIAN_POINT('Ctrl Pts',(-7.33088131199388,2.37503355361642,
-0.187025116539651));
#111435=CARTESIAN_POINT('Ctrl Pts',(-7.28924162669139,2.36833541661307,
-0.185738207668953));
#111436=CARTESIAN_POINT('Ctrl Pts',(-7.24765382450455,2.36147458176434,
-0.184428940115875));
#111437=CARTESIAN_POINT('Ctrl Pts',(-7.486998367,2.36069511,-0.441424342));
#111438=CARTESIAN_POINT('Ctrl Pts',(-7.511008699,2.42611337,-0.034185093));
#111439=CARTESIAN_POINT('Ctrl Pts',(-7.490706247,2.491440779,0.373255838));
#111440=CARTESIAN_POINT('Ctrl Pts',(-7.247532776,2.36069511,-0.189126057));
#111441=CARTESIAN_POINT('Ctrl Pts',(-7.257819883,2.42611337,0.205087974));
#111442=CARTESIAN_POINT('Ctrl Pts',(-7.225287946,2.491440779,0.598092044));
#111443=CARTESIAN_POINT('Origin',(0.199639167737231,2.41071391476071,-0.00309109376033817));
#111444=CARTESIAN_POINT('Ctrl Pts',(-7.45384735693224,2.49597508251434,
0.835955493822569));
#111445=CARTESIAN_POINT('Ctrl Pts',(-7.45221779643163,2.49370793075721,
0.850006844084534));
#111446=CARTESIAN_POINT('Ctrl Pts',(-7.45058823593115,2.491440779,0.864058194346502));
#111447=CARTESIAN_POINT('Ctrl Pts',(-7.40332879345145,2.425690334,1.27156621829887));
#111448=CARTESIAN_POINT('Ctrl Pts',(-7.31190712236696,2.360702725,1.67148911281306));
#111449=CARTESIAN_POINT('Ctrl Pts',(-7.22754387548367,2.49597508251434,
0.570839148403493));
#111450=CARTESIAN_POINT('Ctrl Pts',(-7.22641591074183,2.49370793075721,
0.584465596201748));
#111451=CARTESIAN_POINT('Ctrl Pts',(-7.225287946,2.491440779,0.598092044));
#111452=CARTESIAN_POINT('Ctrl Pts',(-7.192575454,2.425690334,0.993277326));
#111453=CARTESIAN_POINT('Ctrl Pts',(-7.116957917,2.360702725,1.382537524));
#111454=CARTESIAN_POINT('',(-7.11785447482644,2.36147458139012,1.37791424072264));
#111455=CARTESIAN_POINT('Origin',(0.196281286854487,2.5535358133817,-0.00586212603583963));
#111456=CARTESIAN_POINT('Ctrl Pts',(-7.36353307773095,2.40074633454747,
1.42421227703032));
#111457=CARTESIAN_POINT('Ctrl Pts',(-7.32255551225088,2.39450341737561,
1.41644755423288));
#111458=CARTESIAN_POINT('Ctrl Pts',(-7.28157424400633,2.38811403222071,
1.40870196489122));
#111459=CARTESIAN_POINT('Ctrl Pts',(-7.19969419612551,2.3750335446404,1.39327019884403));
#111460=CARTESIAN_POINT('Ctrl Pts',(-7.1587514060899,2.36833541220006,1.38557572453513));
#111461=CARTESIAN_POINT('Ctrl Pts',(-7.11785447620099,2.36147458176668,
1.37791423874306));
#111462=CARTESIAN_POINT('Ctrl Pts',(-7.406849691,2.36069511,1.178379249));
#111463=CARTESIAN_POINT('Ctrl Pts',(-7.342754274,2.42611337,1.581258982));
#111464=CARTESIAN_POINT('Ctrl Pts',(-7.235338726,2.491440779,1.974809744));
#111465=CARTESIAN_POINT('Ctrl Pts',(-7.118745999,2.36069511,1.373300916));
#111466=CARTESIAN_POINT('Ctrl Pts',(-7.044048235,2.42611337,1.760509866));
#111467=CARTESIAN_POINT('Ctrl Pts',(-6.92779261899999,2.491440779,2.137332315));
#111468=CARTESIAN_POINT('Origin',(0.194307367130044,2.41071390558892,-0.0459353841191443));
#111469=CARTESIAN_POINT('Ctrl Pts',(-7.09987482744547,2.49597508226345,
2.41876816842104));
#111470=CARTESIAN_POINT('Ctrl Pts',(-7.09526274045952,2.49370793063177,
2.43214069782287));
#111471=CARTESIAN_POINT('Ctrl Pts',(-7.09065065347373,2.491440779,2.4455132272247));
#111472=CARTESIAN_POINT('Ctrl Pts',(-6.95689393096362,2.425690334,2.83333455625786));
#111473=CARTESIAN_POINT('Ctrl Pts',(-6.78163804747186,2.360702725,3.2042545191125));
#111474=CARTESIAN_POINT('Ctrl Pts',(-6.93585437261289,2.49597508226346,
2.11120153655164));
#111475=CARTESIAN_POINT('Ctrl Pts',(-6.9318234958064,2.49370793063177,2.12426692577582));
#111476=CARTESIAN_POINT('Ctrl Pts',(-6.92779261900001,2.491440779,2.137332315));
#111477=CARTESIAN_POINT('Ctrl Pts',(-6.810891773,2.425690334,2.516246166));
#111478=CARTESIAN_POINT('Ctrl Pts',(-6.653362696,2.360702725,2.880150141));
#111479=CARTESIAN_POINT('',(-6.65523216194324,2.36147458138726,2.87582768139692));
#111480=CARTESIAN_POINT('Origin',(0.190432156601331,2.55353592875688,-0.0479197318352048));
#111481=CARTESIAN_POINT('Ctrl Pts',(-6.88521422635454,2.40074633447517,
2.97385693256405));
#111482=CARTESIAN_POINT('Ctrl Pts',(-6.84686419893038,2.39450346931693,
2.95746491590463));
#111483=CARTESIAN_POINT('Ctrl Pts',(-6.80850595347635,2.38811405780224,
2.94109058031555));
#111484=CARTESIAN_POINT('Ctrl Pts',(-6.73185741844179,2.37503354110023,
2.90841773763505));
#111485=CARTESIAN_POINT('Ctrl Pts',(-6.69352594351825,2.36833541044172,
2.89210167091586));
#111486=CARTESIAN_POINT('Ctrl Pts',(-6.65523216371794,2.36147458173047,
2.87582767950765));
#111487=CARTESIAN_POINT('Ctrl Pts',(-6.980364955,2.36069511,2.743083136));
#111488=CARTESIAN_POINT('Ctrl Pts',(-6.83116082000001,2.42611337,3.122765145));
#111489=CARTESIAN_POINT('Ctrl Pts',(-6.641654807,2.491440779,3.48402374));
#111490=CARTESIAN_POINT('Ctrl Pts',(-6.65709457100001,2.36069511,2.871513865));
#111491=CARTESIAN_POINT('Ctrl Pts',(-6.500904721,2.42611337,3.233612273));
#111492=CARTESIAN_POINT('Ctrl Pts',(-6.306361409,2.491440779,3.576633302));
#111493=CARTESIAN_POINT('Origin',(0.17988987011895,2.41071387449181,-0.0866317942443601));
#111494=CARTESIAN_POINT('Ctrl Pts',(-6.41392004192706,2.49597508250466,
3.88848192866056));
#111495=CARTESIAN_POINT('Ctrl Pts',(-6.4065410840626,2.49370793075237,3.9005503540226));
#111496=CARTESIAN_POINT('Ctrl Pts',(-6.39916212619799,2.491440779,3.91261877938463));
#111497=CARTESIAN_POINT('Ctrl Pts',(-6.18516244014714,2.425690334,4.26261931956866));
#111498=CARTESIAN_POINT('Ctrl Pts',(-5.93426711362043,2.360702725,4.58719254601069));
#111499=CARTESIAN_POINT('Ctrl Pts',(-6.31985202892025,2.49597508250466,
3.55284648411619));
#111500=CARTESIAN_POINT('Ctrl Pts',(-6.31310671896012,2.49370793075237,
3.56473989305809));
#111501=CARTESIAN_POINT('Ctrl Pts',(-6.306361409,2.491440779,3.576633302));
#111502=CARTESIAN_POINT('Ctrl Pts',(-6.110738363,2.425690334,3.921558131));
#111503=CARTESIAN_POINT('Ctrl Pts',(-5.87866363,2.360702725,4.243090139));
#111504=CARTESIAN_POINT('',(-5.88141858947572,2.36147458139205,4.23927061567419));
#111505=CARTESIAN_POINT('Origin',(0.17567859128798,2.55353596923167,-0.0877366492651954));
#111506=CARTESIAN_POINT('Ctrl Pts',(-6.0849504101184,2.400746334527,4.38444734373401));
#111507=CARTESIAN_POINT('Ctrl Pts',(-6.05102049224245,2.39450341566143,
4.36019423236533));
#111508=CARTESIAN_POINT('Ctrl Pts',(-6.01707919396739,2.3881140313641,4.33595694134223));
#111509=CARTESIAN_POINT('Ctrl Pts',(-5.94924644971532,2.37503353301049,
4.28757086998339));
#111510=CARTESIAN_POINT('Ctrl Pts',(-5.91531863784454,2.36833540648173,
4.26339614570779));
#111511=CARTESIAN_POINT('Ctrl Pts',(-5.88141859215414,2.36147458175874,
4.23927061437437));
#111512=CARTESIAN_POINT('Ctrl Pts',(-6.227486113,2.36069511,4.179523504));
#111513=CARTESIAN_POINT('Ctrl Pts',(-6.000149879,2.42611337,4.51825428));
#111514=CARTESIAN_POINT('Ctrl Pts',(-5.737414491,2.491440779,4.83032865900001));
#111515=CARTESIAN_POINT('Ctrl Pts',(-5.884164799,2.36069511,4.235458017));
#111516=CARTESIAN_POINT('Ctrl Pts',(-5.653786127,2.42611337,4.555514565));
#111517=CARTESIAN_POINT('Ctrl Pts',(-5.390051748,2.491440779,4.848694892));
#111518=CARTESIAN_POINT('Origin',(0.157060863459541,2.41071387183971,-0.123277390313924));
#111519=CARTESIAN_POINT('Ctrl Pts',(-5.42805748376532,2.49597508245143,
5.17637459698762));
#111520=CARTESIAN_POINT('Ctrl Pts',(-5.41825668723348,2.49370793072575,
5.18657461133535));
#111521=CARTESIAN_POINT('Ctrl Pts',(-5.40845589070163,2.491440779,5.19677462568309));
#111522=CARTESIAN_POINT('Ctrl Pts',(-5.12421962807833,2.425690334,5.49258874114573));
#111523=CARTESIAN_POINT('Ctrl Pts',(-4.80941644524494,2.360702725,5.75563854725621));
#111524=CARTESIAN_POINT('Ctrl Pts',(-5.40834042720503,2.49597508245143,
4.82836428150074));
#111525=CARTESIAN_POINT('Ctrl Pts',(-5.39919608760243,2.49370793072576,
4.83852958675043));
#111526=CARTESIAN_POINT('Ctrl Pts',(-5.390051748,2.491440779,4.848694892));
#111527=CARTESIAN_POINT('Ctrl Pts',(-5.124853618,2.425690334,5.143502397));
#111528=CARTESIAN_POINT('Ctrl Pts',(-4.829084786,2.360702725,5.407627958));
#111529=CARTESIAN_POINT('',(-4.83259642189076,2.36147458135634,5.40448996696835));
#111530=CARTESIAN_POINT('Origin',(0.152710607699905,2.55353599870726,-0.123451173809973));
#111531=CARTESIAN_POINT('Ctrl Pts',(-5.00016107556259,2.40074633453265,
5.59002586934225));
#111532=CARTESIAN_POINT('Ctrl Pts',(-4.97223836249954,2.39450346937479,
5.55904611943058));
#111533=CARTESIAN_POINT('Ctrl Pts',(-4.94430076676404,2.38811405783615,
5.52807896560669));
#111534=CARTESIAN_POINT('Ctrl Pts',(-4.8884553877854,2.37503353569015,5.46624198633146));
#111535=CARTESIAN_POINT('Ctrl Pts',(-4.86051763445355,2.36833540783023,
5.4353389703849));
#111536=CARTESIAN_POINT('Ctrl Pts',(-4.83259642383872,2.36147458182015,
5.40448996692274));
#111537=CARTESIAN_POINT('Ctrl Pts',(-5.183416941,2.36069511,5.42053399799999));
#111538=CARTESIAN_POINT('Ctrl Pts',(-4.888578597,2.42611337,5.702474866));
#111539=CARTESIAN_POINT('Ctrl Pts',(-4.564899051,2.491440779,5.950772778));
#111540=CARTESIAN_POINT('Ctrl Pts',(-4.836098022,2.36069511,5.401356859));
#111541=CARTESIAN_POINT('Ctrl Pts',(-4.542302778,2.42611337,5.664406059));
#111542=CARTESIAN_POINT('Ctrl Pts',(-4.221709258,2.491440779,5.894036897));
#111543=CARTESIAN_POINT('Origin',(0.12688778706036,2.41071389289739,-0.154158578376882));
#111544=CARTESIAN_POINT('Ctrl Pts',(-4.1883849903721,2.49597508243633,6.22222574211514));
#111545=CARTESIAN_POINT('Ctrl Pts',(-4.17662062947665,2.4937079307182,6.23008040424037));
#111546=CARTESIAN_POINT('Ctrl Pts',(-4.16485626858112,2.491440779,6.23793506636559));
#111547=CARTESIAN_POINT('Ctrl Pts',(-3.82367400106207,2.425690334,6.4657308181516));
#111548=CARTESIAN_POINT('Ctrl Pts',(-3.45968280923341,2.360702725,6.65495728654121));
#111549=CARTESIAN_POINT('Ctrl Pts',(-4.24394083831678,2.49597508243633,
5.87811313032217));
#111550=CARTESIAN_POINT('Ctrl Pts',(-4.23282504815834,2.4937079307182,5.88607501366108));
#111551=CARTESIAN_POINT('Ctrl Pts',(-4.221709258,2.491440779,5.894036897));
#111552=CARTESIAN_POINT('Ctrl Pts',(-3.899336413,2.425690334,6.124942208));
#111553=CARTESIAN_POINT('Ctrl Pts',(-3.553703304,2.360702725,6.319311104));
#111554=CARTESIAN_POINT('',(-3.55780741590456,2.36147458136437,6.31700137503095));
#111555=CARTESIAN_POINT('Origin',(0.122601975477235,2.55353596932925,-0.153393243284287));
#111556=CARTESIAN_POINT('Ctrl Pts',(-3.68156976613605,2.40074633450448,
6.53422099858764));
#111557=CARTESIAN_POINT('Ctrl Pts',(-3.6609596010483,2.39450346936461,6.49796298013453));
#111558=CARTESIAN_POINT('Ctrl Pts',(-3.6403321933983,2.38811405783015,6.46171406386962));
#111559=CARTESIAN_POINT('Ctrl Pts',(-3.59908559050729,2.37503354191843,
6.38931772749768));
#111560=CARTESIAN_POINT('Ctrl Pts',(-3.57844423085058,2.36833541091996,
6.3531313975145));
#111561=CARTESIAN_POINT('Ctrl Pts',(-3.55780741727867,2.36147458187027,
6.31700137561664));
#111562=CARTESIAN_POINT('Ctrl Pts',(-3.896976953,2.36069511,6.408086347));
#111563=CARTESIAN_POINT('Ctrl Pts',(-3.548422814,2.42611337,6.62005406600001));
#111564=CARTESIAN_POINT('Ctrl Pts',(-3.178934004,2.491440779,6.792965376));
#111565=CARTESIAN_POINT('Ctrl Pts',(-3.561900676,2.36069511,6.314694258));
#111566=CARTESIAN_POINT('Ctrl Pts',(-3.218426399,2.42611337,6.508436221));
#111567=CARTESIAN_POINT('Ctrl Pts',(-2.855964336,2.491440779,6.663780287));
#111568=CARTESIAN_POINT('Origin',(0.0907828019592194,2.41071434575424,-0.177833967379083));
#111569=CARTESIAN_POINT('Ctrl Pts',(-2.75286827051218,2.49597508252244,
6.97713252655705));
#111570=CARTESIAN_POINT('Ctrl Pts',(-2.73969043341109,2.49370793076126,
6.982274561309));
#111571=CARTESIAN_POINT('Ctrl Pts',(-2.72651259631005,2.491440779,6.98741659606107));
#111572=CARTESIAN_POINT('Ctrl Pts',(-2.34433762754852,2.425690334,7.13654250767061));
#111573=CARTESIAN_POINT('Ctrl Pts',(-1.94817824990591,2.360702725,7.24309761964013));
#111574=CARTESIAN_POINT('Ctrl Pts',(-2.88109929397571,2.49597508252244,
6.65300794152305));
#111575=CARTESIAN_POINT('Ctrl Pts',(-2.86853181498786,2.49370793076126,
6.65839411426155));
#111576=CARTESIAN_POINT('Ctrl Pts',(-2.855964336,2.491440779,6.663780287));
#111577=CARTESIAN_POINT('Ctrl Pts',(-2.491490572,2.425690334,6.819986528));
#111578=CARTESIAN_POINT('Ctrl Pts',(-2.112154606,2.360702725,6.935510285));
#111579=CARTESIAN_POINT('',(-2.11665928906527,2.36147458134173,6.93413681942433));
#111580=CARTESIAN_POINT('Origin',(0.0867605426048537,2.55353593756859,-0.17616271679774));
#111581=CARTESIAN_POINT('Ctrl Pts',(-2.19083234638043,2.40074633453881,
7.17288321586643));
#111582=CARTESIAN_POINT('Ctrl Pts',(-2.17849833213471,2.39450341596068,
7.1330419724508));
#111583=CARTESIAN_POINT('Ctrl Pts',(-2.16614568309511,2.38811403152101,
7.09320643362084));
#111584=CARTESIAN_POINT('Ctrl Pts',(-2.14142653374841,2.37503354663782,
7.01363607193964));
#111585=CARTESIAN_POINT('Ctrl Pts',(-2.12904674398792,2.36833541317278,
6.9738584605462));
#111586=CARTESIAN_POINT('Ctrl Pts',(-2.11665928997783,2.3614745817451,6.9341368200675));
#111587=CARTESIAN_POINT('Ctrl Pts',(-2.428318655,2.36069511,7.0960037));
#111588=CARTESIAN_POINT('Ctrl Pts',(-2.042346724,2.42611337,7.22808689500001));
#111589=CARTESIAN_POINT('Ctrl Pts',(-1.644325536,2.491440779,7.317526463));
#111590=CARTESIAN_POINT('Ctrl Pts',(-2.121152813,2.36069511,6.932763572));
#111591=CARTESIAN_POINT('Ctrl Pts',(-1.744059979,2.42611337,7.048139138));
#111592=CARTESIAN_POINT('Ctrl Pts',(-1.356677695,2.491440779,7.121932718));
#111593=CARTESIAN_POINT('Origin',(0.0504308075600973,2.41071389512704,-0.193189663991771));
#111594=CARTESIAN_POINT('Ctrl Pts',(-1.18863048790655,2.49597508226724,
7.40579634977361));
#111595=CARTESIAN_POINT('Ctrl Pts',(-1.17465535663115,2.49370793063366,
7.40798532104452));
#111596=CARTESIAN_POINT('Ctrl Pts',(-1.16068022535578,2.491440779,7.4101742923153));
#111597=CARTESIAN_POINT('Ctrl Pts',(-0.755382632264268,2.425690334,7.47365740169885));
#111598=CARTESIAN_POINT('Ctrl Pts',(-0.345579041176663,2.360702725,7.49255875907289));
#111599=CARTESIAN_POINT('Ctrl Pts',(-1.38354074594054,2.49597508226724,
7.11681549620122));
#111600=CARTESIAN_POINT('Ctrl Pts',(-1.37010922047026,2.49370793063366,
7.11937410660064));
#111601=CARTESIAN_POINT('Ctrl Pts',(-1.356677695,2.491440779,7.12193271700001));
#111602=CARTESIAN_POINT('Ctrl Pts',(-0.967145401,2.425690334,7.196135858));
#111603=CARTESIAN_POINT('Ctrl Pts',(-0.571843906,2.360702725,7.227412715));
#111604=CARTESIAN_POINT('',(-0.57653852648969,2.36147458135925,7.22703973357806));
#111605=CARTESIAN_POINT('Origin',(0.0468623792659997,2.55353595236423,-0.190695107929225));
#111606=CARTESIAN_POINT('Ctrl Pts',(-0.597654041416066,2.400746334532,7.4761493862767));
#111607=CARTESIAN_POINT('Ctrl Pts',(-0.594173108960324,2.39450346937549,
7.43458851622998));
#111608=CARTESIAN_POINT('Ctrl Pts',(-0.590672705689646,2.38811405787017,
7.39302866746393));
#111609=CARTESIAN_POINT('Ctrl Pts',(-0.583636731008162,2.37503353385956,
7.31000448191802));
#111610=CARTESIAN_POINT('Ctrl Pts',(-0.580097388195057,2.36833540694216,
7.26849560360237));
#111611=CARTESIAN_POINT('Ctrl Pts',(-0.576538527924448,2.36147458183712,
7.22703973472027));
#111612=CARTESIAN_POINT('Ctrl Pts',(-0.846114875,2.36069511,7.452119807));
#111613=CARTESIAN_POINT('Ctrl Pts',(-0.440772771,2.42611337,7.49814241400001));
#111614=CARTESIAN_POINT('Ctrl Pts',(-0.032830234,2.491440779,7.499928145));
#111615=CARTESIAN_POINT('Ctrl Pts',(-0.581222202,2.36069511,7.226664566));
#111616=CARTESIAN_POINT('Ctrl Pts',(-0.188143253,2.42611337,7.25827890400001));
#111617=CARTESIAN_POINT('Ctrl Pts',(0.206045687,2.491440779,7.24707148999999));
#111618=CARTESIAN_POINT('Origin',(0.00772170226827618,2.41071388357142,
-0.199513755488948));
#111619=CARTESIAN_POINT('Ctrl Pts',(-1.361241758,3.526465848,7.12106178));
#111620=CARTESIAN_POINT('Ctrl Pts',(-0.971016684,3.460723853,7.195656087));
#111621=CARTESIAN_POINT('Ctrl Pts',(-0.574977339,3.395965514,7.227164109));
#111622=CARTESIAN_POINT('Ctrl Pts',(-1.649014893,3.526465848,7.316471136));
#111623=CARTESIAN_POINT('Ctrl Pts',(-1.248081637,3.460723853,7.406835042));
#111624=CARTESIAN_POINT('Ctrl Pts',(-0.839675095,3.395965514,7.452848163));
#111625=CARTESIAN_POINT('',(-1.35657627656236,3.52567991525468,7.12195203434018));
#111626=CARTESIAN_POINT('Origin',(0.0523978542384437,3.62492142657274,-0.186938114701938));
#111627=CARTESIAN_POINT('Ctrl Pts',(-1.40278481009805,3.4862983188696,7.36764513055359));
#111628=CARTESIAN_POINT('Ctrl Pts',(-1.39511199963782,3.49254601522961,
7.32664918607182));
#111629=CARTESIAN_POINT('Ctrl Pts',(-1.38742201379164,3.49894654287788,
7.2856556149904));
#111630=CARTESIAN_POINT('Ctrl Pts',(-1.37202285368929,3.51206280605285,
7.20377130722841));
#111631=CARTESIAN_POINT('Ctrl Pts',(-1.36430479237325,3.51878610650216,
7.16283330034619));
#111632=CARTESIAN_POINT('Ctrl Pts',(-1.35657627478824,3.52567991511443,
7.12195203641864));
#111633=CARTESIAN_POINT('Ctrl Pts',(-2.14101470880455,3.39148928113836,
6.92670820838241));
#111634=CARTESIAN_POINT('Ctrl Pts',(-2.12808802390228,3.39372739756918,
6.93065105269119));
#111635=CARTESIAN_POINT('Ctrl Pts',(-2.115161339,3.395965514,6.934593897));
#111636=CARTESIAN_POINT('Ctrl Pts',(-1.738674564,3.461150149,7.049428346));
#111637=CARTESIAN_POINT('Ctrl Pts',(-1.35196834,3.526458173,7.122828203));
#111638=CARTESIAN_POINT('Ctrl Pts',(-1.97832240686564,3.39148928113836,
7.23497047159279));
#111639=CARTESIAN_POINT('Ctrl Pts',(-1.96482223297234,3.39372739756918,
7.23860790526758));
#111640=CARTESIAN_POINT('Ctrl Pts',(-1.95132205907898,3.395965514,7.24224533894237));
#111641=CARTESIAN_POINT('Ctrl Pts',(-1.55813254688242,3.461150149,7.34818477228137));
#111642=CARTESIAN_POINT('Ctrl Pts',(-1.15578476260318,3.526458173,7.41093360613679));
#111643=CARTESIAN_POINT('Origin',(0.0444211629504335,3.48214329357323,-0.194615624345732));
#111644=CARTESIAN_POINT('Ctrl Pts',(-2.860234467,3.526465848,6.661948573));
#111645=CARTESIAN_POINT('Ctrl Pts',(-2.495168211,3.460723853,6.818685762));
#111646=CARTESIAN_POINT('Ctrl Pts',(-2.115161339,3.395965514,6.934593897));
#111647=CARTESIAN_POINT('Ctrl Pts',(-3.183286862,3.526465848,6.79092664900001));
#111648=CARTESIAN_POINT('Ctrl Pts',(-2.811152772,3.460723853,6.965366696));
#111649=CARTESIAN_POINT('Ctrl Pts',(-2.422186008,3.395965514,7.098099389));
#111650=CARTESIAN_POINT('',(-2.85586944022338,3.52567991541331,6.66382095494341));
#111651=CARTESIAN_POINT('Origin',(0.0913593601432727,3.62492148818353,-0.171304427496621));
#111652=CARTESIAN_POINT('Ctrl Pts',(-2.95381439782472,3.48629831883926,
6.89383641350067));
#111653=CARTESIAN_POINT('Ctrl Pts',(-2.93750805711256,3.49254601521039,
6.85544835880128));
#111654=CARTESIAN_POINT('Ctrl Pts',(-2.92118545276567,3.4989465428767,6.81706631419639));
#111655=CARTESIAN_POINT('Ctrl Pts',(-2.88854361064173,3.51206280608755,
6.74040678022559));
#111656=CARTESIAN_POINT('Ctrl Pts',(-2.87220553190004,3.51878610654731,
6.70208503630344));
#111657=CARTESIAN_POINT('Ctrl Pts',(-2.85586943938469,3.52567991517898,
6.66382095653845));
#111658=CARTESIAN_POINT('Ctrl Pts',(-3.57999648816175,3.39148928099491,
6.30451074469791));
#111659=CARTESIAN_POINT('Ctrl Pts',(-3.56821961658091,3.39372739749746,
6.31114026284889));
#111660=CARTESIAN_POINT('Ctrl Pts',(-3.556442745,3.395965514,6.317769781));
#111661=CARTESIAN_POINT('Ctrl Pts',(-3.213444034,3.461150149,6.510852992));
#111662=CARTESIAN_POINT('Ctrl Pts',(-2.851557586,3.526458173,6.665667208));
#111663=CARTESIAN_POINT('Ctrl Pts',(-3.48737511649809,3.3914892809949,6.64054004360659));
#111664=CARTESIAN_POINT('Ctrl Pts',(-3.47497250948965,3.39372739749745,
6.64699457464484));
#111665=CARTESIAN_POINT('Ctrl Pts',(-3.4625699024813,3.395965514,6.65344910568322));
#111666=CARTESIAN_POINT('Ctrl Pts',(-3.10134678922173,3.461150149,6.84143585675353));
#111667=CARTESIAN_POINT('Ctrl Pts',(-2.72189481628153,3.526458173,6.98921053722955));
#111668=CARTESIAN_POINT('Origin',(0.0852192425559628,3.48214323855182,-0.180516398354257));
#111669=CARTESIAN_POINT('Ctrl Pts',(-4.225485793,3.526465848,5.891330055));
#111670=CARTESIAN_POINT('Ctrl Pts',(-3.902648444,3.460723853,6.122881269));
#111671=CARTESIAN_POINT('Ctrl Pts',(-3.556442745,3.395965514,6.317769781));
#111672=CARTESIAN_POINT('Ctrl Pts',(-4.56871187600001,3.526465848,5.94784598));
#111673=CARTESIAN_POINT('Ctrl Pts',(-4.242777527,3.460723853,6.198205544));
#111674=CARTESIAN_POINT('Ctrl Pts',(-3.891438196,3.395965514,6.411451378));
#111675=CARTESIAN_POINT('',(-4.22162532483267,3.52567991538939,5.89409701316192));
#111676=CARTESIAN_POINT('Origin',(0.126048906263722,3.62492145840609,-0.147660019288895));
#111677=CARTESIAN_POINT('Ctrl Pts',(-4.36672690769358,3.48629831887157,
6.09767956762302));
#111678=CARTESIAN_POINT('Ctrl Pts',(-4.34254950320055,3.49254601523147,
6.06369438560012));
#111679=CARTESIAN_POINT('Ctrl Pts',(-4.3183575074241,3.49894654285412,6.0297185695337));
#111680=CARTESIAN_POINT('Ctrl Pts',(-4.26999927978729,3.5120628060483,5.96186832409333));
#111681=CARTESIAN_POINT('Ctrl Pts',(-4.24580513409496,3.51878610651955,
5.92795472514906));
#111682=CARTESIAN_POINT('Ctrl Pts',(-4.22162532432222,3.52567991516351,
5.89409701520979));
#111683=CARTESIAN_POINT('Ctrl Pts',(-4.85158160960764,3.39148928105395,
5.38752136628062));
#111684=CARTESIAN_POINT('Ctrl Pts',(-4.84150522530381,3.39372739752697,
5.39652756914034));
#111685=CARTESIAN_POINT('Ctrl Pts',(-4.831428841,3.395965514,5.405533772));
#111686=CARTESIAN_POINT('Ctrl Pts',(-4.537956432,3.461150149,5.667837389));
#111687=CARTESIAN_POINT('Ctrl Pts',(-4.217811169,3.526458173,5.896827024));
#111688=CARTESIAN_POINT('Ctrl Pts',(-4.83336204012894,3.39148928105394,
5.73560534434831));
#111689=CARTESIAN_POINT('Ctrl Pts',(-4.82263693272546,3.39372739752697,
5.74457516578482));
#111690=CARTESIAN_POINT('Ctrl Pts',(-4.811911825322,3.395965514,5.75354498722122));
#111691=CARTESIAN_POINT('Ctrl Pts',(-4.49954550307979,3.461150149,6.01478900351506));
#111692=CARTESIAN_POINT('Ctrl Pts',(-4.16073209479072,3.526458173,6.24067975220765));
#111693=CARTESIAN_POINT('Origin',(0.122032535617754,3.48214323624807,-0.157976378280283));
#111694=CARTESIAN_POINT('Ctrl Pts',(-5.393158098,3.526465848,4.845239491));
#111695=CARTESIAN_POINT('Ctrl Pts',(-5.127645174,3.460723853,5.140777654));
#111696=CARTESIAN_POINT('Ctrl Pts',(-4.83142884100001,3.395965514,5.40553377200001));
#111697=CARTESIAN_POINT('Ctrl Pts',(-5.740508999,3.526465848,4.826650643));
#111698=CARTESIAN_POINT('Ctrl Pts',(-5.476014721,3.460723853,5.14122319));
#111699=CARTESIAN_POINT('Ctrl Pts',(-5.178731058,3.395965514,5.425011025));
#111700=CARTESIAN_POINT('',(-5.38998270028869,3.52567991539829,4.84877164614679));
#111701=CARTESIAN_POINT('Origin',(0.154844449716129,3.62492148424465,-0.11711098248098));
#111702=CARTESIAN_POINT('Ctrl Pts',(-5.57545611982745,3.48629831884877,
5.01640200221238));
#111703=CARTESIAN_POINT('Ctrl Pts',(-5.54453816000373,3.49254601522222,
4.98840880214834));
#111704=CARTESIAN_POINT('Ctrl Pts',(-5.51360796327686,3.49894654288713,
4.96042788561611));
#111705=CARTESIAN_POINT('Ctrl Pts',(-5.45179452686104,3.5120628060797,4.90455953070738));
#111706=CARTESIAN_POINT('Ctrl Pts',(-5.42087560556212,3.51878610652425,
4.87663983909214));
#111707=CARTESIAN_POINT('Ctrl Pts',(-5.3899826994675,3.52567991513125,4.84877164802182));
#111708=CARTESIAN_POINT('Ctrl Pts',(-5.89631216715022,3.39148928109063,
4.21861747589908));
#111709=CARTESIAN_POINT('Ctrl Pts',(-5.88840743057512,3.39372739754531,
4.22957924344953));
#111710=CARTESIAN_POINT('Ctrl Pts',(-5.880502694,3.395965514,4.240541011));
#111711=CARTESIAN_POINT('Ctrl Pts',(-5.650279031,3.461150149,4.559800009));
#111712=CARTESIAN_POINT('Ctrl Pts',(-5.386844588,3.526458173,4.852257761));
#111713=CARTESIAN_POINT('Ctrl Pts',(-5.95334632703453,3.39148928109063,
4.56248011289003));
#111714=CARTESIAN_POINT('Ctrl Pts',(-5.94480021320308,3.39372739754531,
4.57354580586494));
#111715=CARTESIAN_POINT('Ctrl Pts',(-5.93625409937163,3.395965514,4.58461149883985));
#111716=CARTESIAN_POINT('Ctrl Pts',(-5.68735046899794,3.461150149,4.9068973012961));
#111717=CARTESIAN_POINT('Ctrl Pts',(-5.40501816371073,3.526458173,5.20034171740979));
#111718=CARTESIAN_POINT('Origin',(0.153139825867278,3.48214326136743,-0.128049668617121));
#111719=CARTESIAN_POINT('Ctrl Pts',(-6.30865232500001,3.526465848,3.572590914));
#111720=CARTESIAN_POINT('Ctrl Pts',(-6.112878915,3.460723853,3.918296989));
#111721=CARTESIAN_POINT('Ctrl Pts',(-5.880502694,3.395965514,4.240541011));
#111722=CARTESIAN_POINT('Ctrl Pts',(-6.643886303,3.526465848,3.479766486));
#111723=CARTESIAN_POINT('Ctrl Pts',(-6.453199552,3.460723853,3.843842954));
#111724=CARTESIAN_POINT('Ctrl Pts',(-6.223872212,3.395965514,4.184903187));
#111725=CARTESIAN_POINT('',(-6.3063104754868,3.52567991541429,3.57672310566886));
#111726=CARTESIAN_POINT('Origin',(0.176399700344673,3.62492144098057,-0.0810860420705356));
#111727=CARTESIAN_POINT('Ctrl Pts',(-6.52348320097803,3.48629831885008,
3.70056305449003));
#111728=CARTESIAN_POINT('Ctrl Pts',(-6.48727037534097,3.4925460152164,3.6798707673355));
#111729=CARTESIAN_POINT('Ctrl Pts',(-6.45104823951126,3.49894654286907,
3.65919310715012));
#111730=CARTESIAN_POINT('Ctrl Pts',(-6.3786699219615,3.51206280606079,3.6179189850791));
#111731=CARTESIAN_POINT('Ctrl Pts',(-6.34247195938134,3.51878610651248,
3.59729869452434));
#111732=CARTESIAN_POINT('Ctrl Pts',(-6.30631047486904,3.52567991512919,
3.57672310798306));
#111733=CARTESIAN_POINT('Ctrl Pts',(-6.66533772140166,3.39148928113425,
2.85245572182119));
#111734=CARTESIAN_POINT('Ctrl Pts',(-6.65997424920077,3.39372739756712,
2.86486049391057));
#111735=CARTESIAN_POINT('Ctrl Pts',(-6.654610777,3.395965514,2.877265266));
#111736=CARTESIAN_POINT('Ctrl Pts',(-6.49840086199999,3.461150149,3.238551448));
#111737=CARTESIAN_POINT('Ctrl Pts',(-6.303995142,3.526458173,3.580802319));
#111738=CARTESIAN_POINT('Ctrl Pts',(-6.7949587564644,3.39148928113426,3.17601838304456));
#111739=CARTESIAN_POINT('Ctrl Pts',(-6.78899124297181,3.39372739756712,
3.18866252798933));
#111740=CARTESIAN_POINT('Ctrl Pts',(-6.78302372947929,3.395965514,3.20130667293414));
#111741=CARTESIAN_POINT('Ctrl Pts',(-6.60922124844986,3.461150149,3.56956453521738));
#111742=CARTESIAN_POINT('Ctrl Pts',(-6.39657159139355,3.526458173,3.91684148375792));
#111743=CARTESIAN_POINT('Origin',(0.177086448535619,3.48214322481508,-0.0921354177508632));
#111744=CARTESIAN_POINT('Ctrl Pts',(-6.92916098100001,3.526465848,2.132891956));
#111745=CARTESIAN_POINT('Ctrl Pts',(-6.812281231,3.460723853,2.512601111));
#111746=CARTESIAN_POINT('Ctrl Pts',(-6.654610777,3.395965514,2.877265266));
#111747=CARTESIAN_POINT('Ctrl Pts',(-7.236602866,3.526465848,1.970172316));
#111748=CARTESIAN_POINT('Ctrl Pts',(-7.128639944,3.460723853,2.366728893));
#111749=CARTESIAN_POINT('Ctrl Pts',(-6.977992019,3.395965514,2.749113927));
#111750=CARTESIAN_POINT('',(-6.92776218145326,3.52567991543165,2.13743096775294));
#111751=CARTESIAN_POINT('Origin',(0.18970668803777,3.6249214517105,-0.0412695740069899));
#111752=CARTESIAN_POINT('Ctrl Pts',(-7.16647945765255,3.48629831881963,
2.21168989111538));
#111753=CARTESIAN_POINT('Ctrl Pts',(-7.12666503765092,3.49254601519576,
2.19926606514368));
#111754=CARTESIAN_POINT('Ctrl Pts',(-7.08684466969436,3.49894654283194,
2.18685852563207));
#111755=CARTESIAN_POINT('Ctrl Pts',(-7.00728580086712,3.51206280605708,
2.16210856821299));
#111756=CARTESIAN_POINT('Ctrl Pts',(-6.96750137362573,3.51878610653685,
2.14975186042951));
#111757=CARTESIAN_POINT('Ctrl Pts',(-6.92776218168722,3.52567991519186,
2.13743096977317));
#111758=CARTESIAN_POINT('Ctrl Pts',(-7.12269949194841,3.39148928101336,
1.35291630750235));
#111759=CARTESIAN_POINT('Ctrl Pts',(-7.12012807397428,3.39372739750668,
1.36618405125118));
#111760=CARTESIAN_POINT('Ctrl Pts',(-7.11755665599999,3.395965514,1.379451795));
#111761=CARTESIAN_POINT('Ctrl Pts',(-7.042664691,3.461150149,1.765871821));
#111762=CARTESIAN_POINT('Ctrl Pts',(-6.92637789,3.526458173,2.141912539));
#111763=CARTESIAN_POINT('Ctrl Pts',(-7.31884646688559,3.39148928101336,
1.64104956198232));
#111764=CARTESIAN_POINT('Ctrl Pts',(-7.31573658786461,3.39372739750668,
1.65468093325028));
#111765=CARTESIAN_POINT('Ctrl Pts',(-7.31262670884364,3.395965514,1.66831230451831));
#111766=CARTESIAN_POINT('Ctrl Pts',(-7.22205218804404,3.461150149,2.06532289950126));
#111767=CARTESIAN_POINT('Ctrl Pts',(-7.08902844015172,3.526458173,2.45019409568168));
#111768=CARTESIAN_POINT('Origin',(0.192752513181269,3.48214325539603,-0.0519129632307747));
#111769=CARTESIAN_POINT('Ctrl Pts',(-7.22566977100001,3.526465848,0.593461341));
#111770=CARTESIAN_POINT('Ctrl Pts',(-7.193148849,3.460723853,0.989418798));
#111771=CARTESIAN_POINT('Ctrl Pts',(-7.117556656,3.395965514,1.379451795));
#111772=CARTESIAN_POINT('Ctrl Pts',(-7.49094392300001,3.526465848,0.368455079));
#111773=CARTESIAN_POINT('Ctrl Pts',(-7.470753056,3.460723853,0.77894922));
#111774=CARTESIAN_POINT('Ctrl Pts',(-7.405828674,3.395965514,1.184779155));
#111775=CARTESIAN_POINT('',(-7.22527942719966,3.52567991541072,0.598194933891261));
#111776=CARTESIAN_POINT('Origin',(0.194143031089954,3.62492147818242,0.000476651601998418));
#111777=CARTESIAN_POINT('Ctrl Pts',(-7.474379099935,3.48629831882758,0.619400567375752));
#111778=CARTESIAN_POINT('Ctrl Pts',(-7.43282476363648,3.49254601520315,
0.615826126927508));
#111779=CARTESIAN_POINT('Ctrl Pts',(-7.39126811926568,3.49894654288035,
0.612268870771432));
#111780=CARTESIAN_POINT('Ctrl Pts',(-7.3082487833973,3.51206280609374,0.605200358586718));
#111781=CARTESIAN_POINT('Ctrl Pts',(-7.26673816733997,3.5187861065218,0.601685019581434));
#111782=CARTESIAN_POINT('Ctrl Pts',(-7.22527942859502,3.52567991512498,
0.598194936057684));
#111783=CARTESIAN_POINT('Ctrl Pts',(-7.24701174985952,3.3914892810937,-0.209883968754185));
#111784=CARTESIAN_POINT('Ctrl Pts',(-7.2473526229297,3.39372739754685,-0.196373638877095));
#111785=CARTESIAN_POINT('Ctrl Pts',(-7.24769349600001,3.395965514,-0.182863309));
#111786=CARTESIAN_POINT('Ctrl Pts',(-7.257621347,3.461150149,0.21062199));
#111787=CARTESIAN_POINT('Ctrl Pts',(-7.224890905,3.526458173,0.60286931));
#111788=CARTESIAN_POINT('Ctrl Pts',(-7.50051305040811,3.3914892810937,0.0293470895752078));
#111789=CARTESIAN_POINT('Ctrl Pts',(-7.50040622050875,3.39372739754685,
0.0433282987454922));
#111790=CARTESIAN_POINT('Ctrl Pts',(-7.5002993906094,3.395965514,0.0573095079157767));
#111791=CARTESIAN_POINT('Ctrl Pts',(-7.49718799397627,3.461150149,0.464509059725247));
#111792=CARTESIAN_POINT('Ctrl Pts',(-7.45001019763175,3.526458173,0.868978355344271));
#111793=CARTESIAN_POINT('Origin',(0.199405651581279,3.48214325129353,-0.00926317386774702));
#111794=CARTESIAN_POINT('Ctrl Pts',(-7.184314273,3.526465848,-0.973718867));
#111795=CARTESIAN_POINT('Ctrl Pts',(-7.237672821,3.460723853,-0.580027638));
#111796=CARTESIAN_POINT('Ctrl Pts',(-7.247693496,3.395965514,-0.182863309));
#111797=CARTESIAN_POINT('Ctrl Pts',(-7.395016767,3.526465848,-1.250490709));
#111798=CARTESIAN_POINT('Ctrl Pts',(-7.463542058,3.460723853,-0.845253253));
#111799=CARTESIAN_POINT('Ctrl Pts',(-7.487377012,3.395965514,-0.434954574));
#111800=CARTESIAN_POINT('',(-7.18495063795781,3.52567991538893,-0.969012030082798));
#111801=CARTESIAN_POINT('Origin',(0.189501763583084,3.62492144712771,0.0422005216843591));
#111802=CARTESIAN_POINT('Ctrl Pts',(-7.43278508283957,3.48629831884151,
-1.00185123952923));
#111803=CARTESIAN_POINT('Ctrl Pts',(-7.39143386477356,3.49254601521193,
-0.996409157496579));
#111804=CARTESIAN_POINT('Ctrl Pts',(-7.35008408696199,3.49894654284543,
-0.990949796784443));
#111805=CARTESIAN_POINT('Ctrl Pts',(-7.2674861758617,3.5120628060405,-0.980006347682485));
#111806=CARTESIAN_POINT('Ctrl Pts',(-7.22619036093362,3.51878610646488,
-0.974515944472787));
#111807=CARTESIAN_POINT('Ctrl Pts',(-7.18495063964874,3.52567991506207,
-0.969012028304349));
#111808=CARTESIAN_POINT('Ctrl Pts',(-7.03246179338903,3.39148928094506,
-1.76287030428815));
#111809=CARTESIAN_POINT('Ctrl Pts',(-7.03569901869452,3.39372739747253,
-1.74974911564411));
#111810=CARTESIAN_POINT('Ctrl Pts',(-7.03893624400001,3.395965514,-1.736627927));
#111811=CARTESIAN_POINT('Ctrl Pts',(-7.13321969499999,3.461150149,-1.354476291));
#111812=CARTESIAN_POINT('Ctrl Pts',(-7.185576052,3.526458173,-0.964363417));
#111813=CARTESIAN_POINT('Ctrl Pts',(-7.33146397982515,3.39148928094506,
-1.5837276227993));
#111814=CARTESIAN_POINT('Ctrl Pts',(-7.33436519435894,3.39372739747253,
-1.57005032079391));
#111815=CARTESIAN_POINT('Ctrl Pts',(-7.33726640889262,3.395965514,-1.5563730187886));
#111816=CARTESIAN_POINT('Ctrl Pts',(-7.42176362256031,3.461150149,-1.15802470758192));
#111817=CARTESIAN_POINT('Ctrl Pts',(-7.46263775903074,3.526458173,-0.752869847804082));
#111818=CARTESIAN_POINT('Origin',(0.196735211445208,3.482143250559,0.0338197687897776));
#111819=CARTESIAN_POINT('Ctrl Pts',(-6.807028224,3.526465848,-2.495369062));
#111820=CARTESIAN_POINT('Ctrl Pts',(-6.943771255,3.460723853,-2.122352626));
#111821=CARTESIAN_POINT('Ctrl Pts',(-7.038936244,3.395965514,-1.736627927));
#111822=CARTESIAN_POINT('Ctrl Pts',(-6.953306846,3.526465848,-2.810964941));
#111823=CARTESIAN_POINT('Ctrl Pts',(-7.107344128,3.460723853,-2.429932623));
#111824=CARTESIAN_POINT('Ctrl Pts',(-7.218823922,3.395965514,-2.03435031));
#111825=CARTESIAN_POINT('',(-6.8086615418157,3.52567991540629,-2.49090906873649));
#111826=CARTESIAN_POINT('Origin',(0.175999427407891,3.62492148308023,0.0819511757576769));
#111827=CARTESIAN_POINT('Ctrl Pts',(-7.04364229597215,3.48629831884724,
-2.57625759581233));
#111828=CARTESIAN_POINT('Ctrl Pts',(-7.00442773317179,3.49254601521909,
-2.56205345706564));
#111829=CARTESIAN_POINT('Ctrl Pts',(-6.96521829159601,3.49894654281944,
-2.54783275332507));
#111830=CARTESIAN_POINT('Ctrl Pts',(-6.88690399178184,3.51206280604993,
-2.51938904670169));
#111831=CARTESIAN_POINT('Ctrl Pts',(-6.84775392418869,3.51878610654272,
-2.50514962649814));
#111832=CARTESIAN_POINT('Ctrl Pts',(-6.80866154374564,3.52567991521619,
-2.49090906776779));
#111833=CARTESIAN_POINT('Ctrl Pts',(-6.48908173905949,3.39148928095608,
-3.23342678352247));
#111834=CARTESIAN_POINT('Ctrl Pts',(-6.49506394752967,3.39372739747804,
-3.22130826876123));
#111835=CARTESIAN_POINT('Ctrl Pts',(-6.50104615600001,3.395965514,-3.209189754));
#111836=CARTESIAN_POINT('Ctrl Pts',(-6.675276618,3.461150149,-2.856240766));
#111837=CARTESIAN_POINT('Ctrl Pts',(-6.810271649,3.526458173,-2.486503584));
#111838=CARTESIAN_POINT('Ctrl Pts',(-6.81960380219367,3.39148928095609,
-3.12274899055064));
#111839=CARTESIAN_POINT('Ctrl Pts',(-6.8253774035498,3.39372739747804,-3.11001513166759));
#111840=CARTESIAN_POINT('Ctrl Pts',(-6.83115100490594,3.395965514,-3.0972812727845));
#111841=CARTESIAN_POINT('Ctrl Pts',(-6.99930583212015,3.461150149,-2.72641052709717));
#111842=CARTESIAN_POINT('Ctrl Pts',(-7.12632067321713,3.526458173,-2.33951469307182));
#111843=CARTESIAN_POINT('Origin',(0.184865071285664,3.48214320604127,0.0753211970402862));
#111844=CARTESIAN_POINT('Ctrl Pts',(-6.11145310100001,3.526465848,-3.900338574));
#111845=CARTESIAN_POINT('Ctrl Pts',(-6.325186664,3.460723853,-3.565438765));
#111846=CARTESIAN_POINT('Ctrl Pts',(-6.50104615600001,3.395965514,-3.209189754));
#111847=CARTESIAN_POINT('Ctrl Pts',(-6.186468026,3.526465848,-4.240001576));
#111848=CARTESIAN_POINT('Ctrl Pts',(-6.418814686,3.460723853,-3.900991045));
#111849=CARTESIAN_POINT('Ctrl Pts',(-6.612726649,3.395965514,-3.538622086));
#111850=CARTESIAN_POINT('',(-6.11400699950171,3.52567991541422,-3.89633396843858));
#111851=CARTESIAN_POINT('Origin',(0.15426755881971,3.62492150645954,0.117869865155411));
#111852=CARTESIAN_POINT('Ctrl Pts',(-6.32514662409161,3.48629831884354,
-4.03020100952011));
#111853=CARTESIAN_POINT('Ctrl Pts',(-6.28990234594227,3.49254601521795,
-4.00789898382161));
#111854=CARTESIAN_POINT('Ctrl Pts',(-6.25466663006605,3.49894654285478,
-3.9855818812002));
#111855=CARTESIAN_POINT('Ctrl Pts',(-6.18429783112566,3.51206280607743,
-3.94096791317394));
#111856=CARTESIAN_POINT('Ctrl Pts',(-6.14912412478399,3.51878610654907,
-3.9186452955183));
#111857=CARTESIAN_POINT('Ctrl Pts',(-6.11400700156399,3.52567991519606,
-3.89633396700649));
#111858=CARTESIAN_POINT('Ctrl Pts',(-5.64227943465134,3.39148928097793,
-4.55279182018316));
#111859=CARTESIAN_POINT('Ctrl Pts',(-5.65072690482569,3.39372739748896,
-4.54224262759158));
#111860=CARTESIAN_POINT('Ctrl Pts',(-5.659174375,3.395965514,-4.531693435));
#111861=CARTESIAN_POINT('Ctrl Pts',(-5.905205025,3.461150149,-4.224450597));
#111862=CARTESIAN_POINT('Ctrl Pts',(-6.116526512,3.526458173,-3.892377606));
#111863=CARTESIAN_POINT('Ctrl Pts',(-5.98886652980762,3.39148928097793,
-4.51575408564639));
#111864=CARTESIAN_POINT('Ctrl Pts',(-5.99724255079055,3.39372739748897,
-4.50455909097359));
#111865=CARTESIAN_POINT('Ctrl Pts',(-6.00561857177365,3.395965514,-4.49336409630081));
#111866=CARTESIAN_POINT('Ctrl Pts',(-6.24956828030756,3.461150149,-4.16731241937839));
#111867=CARTESIAN_POINT('Ctrl Pts',(-6.45678475223131,3.526458173,-3.81676643166149));
#111868=CARTESIAN_POINT('Origin',(0.164351554709367,3.48214325047369,0.113301003398428));
#111869=CARTESIAN_POINT('Ctrl Pts',(-5.130113223,3.526465848,-5.122932589));
#111870=CARTESIAN_POINT('Ctrl Pts',(-5.410843374,3.460723853,-4.841808949));
#111871=CARTESIAN_POINT('Ctrl Pts',(-5.659174375,3.395965514,-4.531693435));
#111872=CARTESIAN_POINT('Ctrl Pts',(-5.13035683600001,3.526465848,-5.470780451));
#111873=CARTESIAN_POINT('Ctrl Pts',(-5.430148604,3.460723853,-5.189643461));
#111874=CARTESIAN_POINT('Ctrl Pts',(-5.697425627,3.395965514,-4.877431827));
#111875=CARTESIAN_POINT('',(-5.13346828522413,3.52567991540396,-5.119570621364));
#111876=CARTESIAN_POINT('Origin',(0.125322351743835,3.62492145200994,0.148277099372972));
#111877=CARTESIAN_POINT('Ctrl Pts',(-5.31089412599478,3.48629831883356,
-5.29569670360672));
#111878=CARTESIAN_POINT('Ctrl Pts',(-5.2812681157569,3.49254601519222,-5.26633960900819));
#111879=CARTESIAN_POINT('Ctrl Pts',(-5.2516537084966,3.4989465428554,-5.23696963039118));
#111880=CARTESIAN_POINT('Ctrl Pts',(-5.19252077726191,3.51206280604437,
-5.17827150053571));
#111881=CARTESIAN_POINT('Ctrl Pts',(-5.16296811547869,3.51878610651194,
-5.14890946606444));
#111882=CARTESIAN_POINT('Ctrl Pts',(-5.1334682871504,3.52567991514279,-5.11957062045771));
#111883=CARTESIAN_POINT('Ctrl Pts',(-4.53165041690712,3.39148928120598,
-5.65927337102999));
#111884=CARTESIAN_POINT('Ctrl Pts',(-4.54216815395354,3.39372739760299,
-5.65078676951494));
#111885=CARTESIAN_POINT('Ctrl Pts',(-4.552685891,3.395965514,-5.64230016800001));
#111886=CARTESIAN_POINT('Ctrl Pts',(-4.859012609,3.461150149,-5.395129814));
#111887=CARTESIAN_POINT('Ctrl Pts',(-5.136779394,3.526458173,-5.116248377));
#111888=CARTESIAN_POINT('Ctrl Pts',(-4.87809651566209,3.39148928120598,
-5.69760753822724));
#111889=CARTESIAN_POINT('Ctrl Pts',(-4.88868330231097,3.39372739760299,
-5.68847487366667));
#111890=CARTESIAN_POINT('Ctrl Pts',(-4.89927008895973,3.395965514,-5.67934220910622));
#111891=CARTESIAN_POINT('Ctrl Pts',(-5.20760786104525,3.461150149,-5.41335541469938));
#111892=CARTESIAN_POINT('Ctrl Pts',(-5.4853367528461,3.526458173,-5.11555041405223));
#111893=CARTESIAN_POINT('Origin',(0.136152707977599,3.48214322157363,0.145982787016208));
#111894=CARTESIAN_POINT('Ctrl Pts',(-3.908894953,3.526465848,-6.10598397));
#111895=CARTESIAN_POINT('Ctrl Pts',(-4.243495061,3.460723853,-5.89178152900001));
#111896=CARTESIAN_POINT('Ctrl Pts',(-4.552685891,3.395965514,-5.642300168));
#111897=CARTESIAN_POINT('Ctrl Pts',(-3.834355862,3.526465848,-6.445751711));
#111898=CARTESIAN_POINT('Ctrl Pts',(-4.187574808,3.460723853,-6.235633917));
#111899=CARTESIAN_POINT('Ctrl Pts',(-4.51571931500001,3.395965514,-5.988178277));
#111900=CARTESIAN_POINT('',(-3.9128942992225,3.52567991540626,-6.10342184278223));
#111901=CARTESIAN_POINT('Origin',(0.0905172887038647,3.62492145983665,0.171751205630448));
#111902=CARTESIAN_POINT('Ctrl Pts',(-4.04831012087657,3.48629831884072,
-6.31357150580349));
#111903=CARTESIAN_POINT('Ctrl Pts',(-4.02568765781779,3.49254601519901,
-6.27853204729132));
#111904=CARTESIAN_POINT('Ctrl Pts',(-4.00307929618703,3.49894654285463,
-6.24348250033077));
#111905=CARTESIAN_POINT('Ctrl Pts',(-3.95794722285298,3.51206280605495,
-6.17344486789823));
#111906=CARTESIAN_POINT('Ctrl Pts',(-3.93539745539643,3.51878610652987,
-6.13841635280557));
#111907=CARTESIAN_POINT('Ctrl Pts',(-3.91289430129605,3.52567991517878,
-6.10342184208375));
#111908=CARTESIAN_POINT('Ctrl Pts',(-3.20912646051089,3.391489281171,-6.50113358893938));
#111909=CARTESIAN_POINT('Ctrl Pts',(-3.22122266725546,3.3937273975855,-6.49510640196969));
#111910=CARTESIAN_POINT('Ctrl Pts',(-3.233318874,3.395965514,-6.489079215));
#111911=CARTESIAN_POINT('Ctrl Pts',(-3.585618163,3.461150149,-6.313538756));
#111912=CARTESIAN_POINT('Ctrl Pts',(-3.91684218,3.526458173,-6.100889061));
#111913=CARTESIAN_POINT('Ctrl Pts',(-3.53923212929024,3.39148928117102,
-6.61304719478717));
#111914=CARTESIAN_POINT('Ctrl Pts',(-3.5515346557487,3.3937273975855,-6.60640389301607));
#111915=CARTESIAN_POINT('Ctrl Pts',(-3.56383718220717,3.395965514,-6.59976059124494));
#111916=CARTESIAN_POINT('Ctrl Pts',(-3.92214548626916,3.461150149,-6.40627592782903));
#111917=CARTESIAN_POINT('Ctrl Pts',(-4.25740050355601,3.526458173,-6.175136944924));
#111918=CARTESIAN_POINT('Origin',(0.101587567894683,3.48214325638124,0.171838632591572));
#111919=CARTESIAN_POINT('Ctrl Pts',(-2.504901099,3.526465848,-6.803526327));
#111920=CARTESIAN_POINT('Ctrl Pts',(-2.877725636,3.460723853,-6.666260952));
#111921=CARTESIAN_POINT('Ctrl Pts',(-3.233318874,3.395965514,-6.489079215));
#111922=CARTESIAN_POINT('Ctrl Pts',(-2.35906467,3.526465848,-7.119326786));
#111923=CARTESIAN_POINT('Ctrl Pts',(-2.749194668,3.460723853,-6.99005306100001));
#111924=CARTESIAN_POINT('Ctrl Pts',(-3.122862986,3.395965514,-6.81892416500001));
#111925=CARTESIAN_POINT('',(-2.50935772461912,3.5256799154024,-6.80188384143029));
#111926=CARTESIAN_POINT('Origin',(0.0514794809429503,3.62492147913838,0.187194024079387));
#111927=CARTESIAN_POINT('Ctrl Pts',(-2.59643163413031,3.48629831882752,
-7.03623072135717));
#111928=CARTESIAN_POINT('Ctrl Pts',(-2.58187051952427,3.49254601518489,
-6.99714730511123));
#111929=CARTESIAN_POINT('Ctrl Pts',(-2.56732534538742,3.49894654282687,
-6.95805706773302));
#111930=CARTESIAN_POINT('Ctrl Pts',(-2.53830445549345,3.51206280601471,
-6.87995481461204));
#111931=CARTESIAN_POINT('Ctrl Pts',(-2.5238119843407,3.51878610648465,-6.84089771329479));
#111932=CARTESIAN_POINT('Ctrl Pts',(-2.50935772681528,3.52567991512012,
-6.80188384184327));
#111933=CARTESIAN_POINT('Ctrl Pts',(-1.73654731746914,3.39148928114318,
-7.03900802661295));
#111934=CARTESIAN_POINT('Ctrl Pts',(-1.74965638873457,3.39372739757159,
-7.03572207880648));
#111935=CARTESIAN_POINT('Ctrl Pts',(-1.76276546,3.395965514,-7.032436131));
#111936=CARTESIAN_POINT('Ctrl Pts',(-2.144564197,3.461150149,-6.936733644));
#111937=CARTESIAN_POINT('Ctrl Pts',(-2.51375778,3.526458173,-6.800258953));
#111938=CARTESIAN_POINT('Ctrl Pts',(-2.03487718227089,3.39148928114319,
-7.2192681159125));
#111939=CARTESIAN_POINT('Ctrl Pts',(-2.04832019609804,3.39372739757159,
-7.21542481033627));
#111940=CARTESIAN_POINT('Ctrl Pts',(-2.06176320992517,3.395965514,-7.21158150475991));
#111941=CARTESIAN_POINT('Ctrl Pts',(-2.45328794853941,3.461150149,-7.09964609871575));
#111942=CARTESIAN_POINT('Ctrl Pts',(-2.83039293831108,3.526458173,-6.94598093486384));
#111943=CARTESIAN_POINT('Origin',(0.0622722465864306,3.48214326322917,0.189659333558916));
#111944=CARTESIAN_POINT('Ctrl Pts',(-0.983780854,3.526465848,-7.182943354));
#111945=CARTESIAN_POINT('Ctrl Pts',(-1.377396959,3.460723853,-7.129033422));
#111946=CARTESIAN_POINT('Ctrl Pts',(-1.76276546,3.395965514,-7.032436131));
#111947=CARTESIAN_POINT('Ctrl Pts',(-0.773466236,3.526465848,-7.460010052));
#111948=CARTESIAN_POINT('Ctrl Pts',(-1.182265241,3.460723853,-7.417625092));
#111949=CARTESIAN_POINT('Ctrl Pts',(-1.583985056,3.395965514,-7.330824738));
#111950=CARTESIAN_POINT('',(-0.988486371605558,3.5256799154039,-7.18229731209713));
#111951=CARTESIAN_POINT('Origin',(0.0100347628190417,3.62492146056771,0.19388418036362));
#111952=CARTESIAN_POINT('Ctrl Pts',(-1.02314688972635,3.48629831883303,
-7.42988360828838));
#111953=CARTESIAN_POINT('Ctrl Pts',(-1.0173279850979,3.49254601520365,-7.388583731331));
#111954=CARTESIAN_POINT('Ctrl Pts',(-1.01152611461239,3.49894654284631,
-7.34728061954439));
#111955=CARTESIAN_POINT('Ctrl Pts',(-0.999973392745211,3.51206280605282,
-7.26476572022423));
#111956=CARTESIAN_POINT('Ctrl Pts',(-0.994215869778384,3.51878610652593,
-7.22350629936899));
#111957=CARTESIAN_POINT('Ctrl Pts',(-0.988486373856841,3.52567991516553,
-7.18229731247012));
#111958=CARTESIAN_POINT('Ctrl Pts',(-0.182769151460141,3.39148928109655,
-7.24774627167997));
#111959=CARTESIAN_POINT('Ctrl Pts',(-0.196278121730071,3.39372739754827,
-7.24735521034));
#111960=CARTESIAN_POINT('Ctrl Pts',(-0.209787092,3.395965514,-7.24696414899999));
#111961=CARTESIAN_POINT('Ctrl Pts',(-0.603232793,3.461150149,-7.235574576));
#111962=CARTESIAN_POINT('Ctrl Pts',(-0.993132859,3.526458173,-7.181656294));
#111963=CARTESIAN_POINT('Ctrl Pts',(-0.435373639031206,3.39148928109655,
-7.4879240829896));
#111964=CARTESIAN_POINT('Ctrl Pts',(-0.449328559914331,3.39372739754827,
-7.48706048234389));
#111965=CARTESIAN_POINT('Ctrl Pts',(-0.463283480797445,3.395965514,-7.4861968816982));
#111966=CARTESIAN_POINT('Ctrl Pts',(-0.869717392453809,3.461150149,-7.46104470839123));
#111967=CARTESIAN_POINT('Ctrl Pts',(-1.27103934506535,3.526458173,-7.39203857617559));
#111968=CARTESIAN_POINT('Origin',(0.0200451930806927,3.48214323715933,0.198611868377269));
#111969=CARTESIAN_POINT('Ctrl Pts',(0.58333989,3.526465848,-7.226493934));
#111970=CARTESIAN_POINT('Ctrl Pts',(0.18733727,3.460723853,-7.258460213));
#111971=CARTESIAN_POINT('Ctrl Pts',(-0.209787092,3.395965514,-7.246964149));
#111972=CARTESIAN_POINT('Ctrl Pts',(0.84829862,3.526465848,-7.45187154));
#111973=CARTESIAN_POINT('Ctrl Pts',(0.439945595,3.460723853,-7.498357219));
#111974=CARTESIAN_POINT('Ctrl Pts',(0.028958256,3.395965514,-7.499944094));
#111975=CARTESIAN_POINT('',(0.578605504968755,3.52567991539871,-7.2268745428914));
#111976=CARTESIAN_POINT('Origin',(-0.0318792103603806,3.62492147346623,
0.191508480028005));
#111977=CARTESIAN_POINT('Ctrl Pts',(0.5979790664113,3.48629831884111,-7.47612339587756));
#111978=CARTESIAN_POINT('Ctrl Pts',(0.594783675462233,3.49254601521968,
-7.4345381945661));
#111979=CARTESIAN_POINT('Ctrl Pts',(0.591570953208007,3.49894654283551,
-7.39295349612528));
#111980=CARTESIAN_POINT('Ctrl Pts',(0.585115314289095,3.51206280605377,
-7.30988425562773));
#111981=CARTESIAN_POINT('Ctrl Pts',(0.581868673498221,3.51878610651907,
-7.26835175999189));
#111982=CARTESIAN_POINT('Ctrl Pts',(0.578605502673376,3.52567991515746,
-7.2268745441991));
#111983=CARTESIAN_POINT('Ctrl Pts',(1.37955509719461,3.39148928095979,-7.11758795639031));
#111984=CARTESIAN_POINT('Ctrl Pts',(1.36627789209731,3.3937273974799,-7.1201100671952));
#111985=CARTESIAN_POINT('Ctrl Pts',(1.353000687,3.395965514,-7.122632178));
#111986=CARTESIAN_POINT('Ctrl Pts',(0.966305106,3.461150149,-7.196088082));
#111987=CARTESIAN_POINT('Ctrl Pts',(0.57392985,3.526458173,-7.227247369));
#111988=CARTESIAN_POINT('Ctrl Pts',(1.18448749190377,3.39148928095979,-7.40645304119305));
#111989=CARTESIAN_POINT('Ctrl Pts',(1.17067318028301,3.3937273974799,-7.40860952663753));
#111990=CARTESIAN_POINT('Ctrl Pts',(1.15685886866229,3.395965514,-7.41076601208203));
#111991=CARTESIAN_POINT('Ctrl Pts',(0.754520182233867,3.461150149,-7.47357316055637));
#111992=CARTESIAN_POINT('Ctrl Pts',(0.347746635845621,3.526458173,-7.49245271025973));
#111993=CARTESIAN_POINT('Origin',(-0.0231191456030383,3.48214324217312,
0.19827763683482));
#111994=CARTESIAN_POINT('Ctrl Pts',(2.12318431,3.526465848,-6.932141688));
#111995=CARTESIAN_POINT('Ctrl Pts',(1.743311816,3.460723853,-7.048489472));
#111996=CARTESIAN_POINT('Ctrl Pts',(1.353000687,3.395965514,-7.122632178));
#111997=CARTESIAN_POINT('Ctrl Pts',(2.430397975,3.526465848,-7.095291797));
#111998=CARTESIAN_POINT('Ctrl Pts',(2.041585064,3.460723853,-7.228474496));
#111999=CARTESIAN_POINT('Ctrl Pts',(1.640547511,3.395965514,-7.3183744));
#112000=CARTESIAN_POINT('',(2.11864243188285,3.52567991541344,-6.9335311516546));
#112001=CARTESIAN_POINT('Origin',(-0.0723025751553144,3.6249214524772,0.18017811992764));
#112002=CARTESIAN_POINT('Ctrl Pts',(2.19114418540924,3.48629831884211,-7.17278796232453));
#112003=CARTESIAN_POINT('Ctrl Pts',(2.17908391196435,3.49254601521138,-7.13286191455645));
#112004=CARTESIAN_POINT('Ctrl Pts',(2.16700682047426,3.4989465428543,-7.09294008337225));
#112005=CARTESIAN_POINT('Ctrl Pts',(2.14284467989402,3.51206280606465,-7.01320072698359));
#112006=CARTESIAN_POINT('Ctrl Pts',(2.13074568506188,3.5187861065394,-6.97333716963481));
#112007=CARTESIAN_POINT('Ctrl Pts',(2.11864243027881,3.52567991518217,-6.93353115313885));
#112008=CARTESIAN_POINT('Ctrl Pts',(2.87737288140405,3.3914892811314,-6.65461913858258));
#112009=CARTESIAN_POINT('Ctrl Pts',(2.86494826970199,3.3937273975657,-6.65993649029124));
#112010=CARTESIAN_POINT('Ctrl Pts',(2.852523658,3.395965514,-6.665253842));
#112011=CARTESIAN_POINT('Ctrl Pts',(2.490659652,3.461150149,-6.820120508));
#112012=CARTESIAN_POINT('Ctrl Pts',(2.114156238,3.526458173,-6.934900389));
#112013=CARTESIAN_POINT('Ctrl Pts',(2.74896330195076,3.39148928113139,-6.97866448862964));
#112014=CARTESIAN_POINT('Ctrl Pts',(2.73593554238889,3.3937273975657,-6.98374022506011));
#112015=CARTESIAN_POINT('Ctrl Pts',(2.72290778282702,3.395965514,-6.98881596149056));
#112016=CARTESIAN_POINT('Ctrl Pts',(2.34347723180972,3.461150149,-7.13664563715228));
#112017=CARTESIAN_POINT('Ctrl Pts',(1.95027237024044,3.526458173,-7.24252808155912));
#112018=CARTESIAN_POINT('Origin',(-0.065202394651328,3.48214328243972,0.188671929290466));
#112019=CARTESIAN_POINT('Ctrl Pts',(3.563750991,3.526465848,-6.313650202));
#112020=CARTESIAN_POINT('Ctrl Pts',(3.217771039,3.460723853,-6.50893919600001));
#112021=CARTESIAN_POINT('Ctrl Pts',(2.852523658,3.395965514,-6.66525384200001));
#112022=CARTESIAN_POINT('Ctrl Pts',(3.898854622,3.526465848,-6.406944095));
#112023=CARTESIAN_POINT('Ctrl Pts',(3.547762284,3.460723853,-6.620596339));
#112024=CARTESIAN_POINT('Ctrl Pts',(3.175426589,3.395965514,-6.794605653));
#112025=CARTESIAN_POINT('',(3.55961399279691,3.52567991539475,-6.31598355033359));
#112026=CARTESIAN_POINT('Origin',(-0.109345231367666,3.624921467088,0.160422896054845));
#112027=CARTESIAN_POINT('Ctrl Pts',(3.6818538378336,3.4862983188185,-6.53406093560932));
#112028=CARTESIAN_POINT('Ctrl Pts',(3.66149260672344,3.49254601520393,-6.49766093882917));
#112029=CARTESIAN_POINT('Ctrl Pts',(3.64111585723239,3.49894654284766,-6.46126867554383));
#112030=CARTESIAN_POINT('Ctrl Pts',(3.60037700929721,3.51206280607397,-6.38858772696084));
#112031=CARTESIAN_POINT('Ctrl Pts',(3.5799913957474,3.51878610651668,-6.35225708390216));
#112032=CARTESIAN_POINT('Ctrl Pts',(3.55961399137252,3.52567991513177,-6.31598355218538));
#112033=CARTESIAN_POINT('Ctrl Pts',(4.24064790842477,3.39148928092428,-5.8804877258907));
#112034=CARTESIAN_POINT('Ctrl Pts',(4.22965685021238,3.39372739746214,-5.88835168544536));
#112035=CARTESIAN_POINT('Ctrl Pts',(4.218665792,3.395965514,-5.896215645));
#112036=CARTESIAN_POINT('Ctrl Pts',(3.898553722,3.461150149,-6.125251678));
#112037=CARTESIAN_POINT('Ctrl Pts',(3.555527029,3.526458173,-6.318285174));
#112038=CARTESIAN_POINT('Ctrl Pts',(4.18490064530936,3.39148928092428,-6.22456133883201));
#112039=CARTESIAN_POINT('Ctrl Pts',(4.17326860031493,3.39372739746214,-6.23231899095407));
#112040=CARTESIAN_POINT('Ctrl Pts',(4.1616365553205,3.395965514,-6.24007664307597));
#112041=CARTESIAN_POINT('Ctrl Pts',(3.82285589111576,3.461150149,-6.46601649628232));
#112042=CARTESIAN_POINT('Ctrl Pts',(3.4616055353622,3.526458173,-6.6539508899692));
#112043=CARTESIAN_POINT('Origin',(-0.10423690204041,3.4821432418066,0.170244306811728));
#112044=CARTESIAN_POINT('Ctrl Pts',(4.837680637,3.526465848,-5.39993945));
#112045=CARTESIAN_POINT('Ctrl Pts',(4.541770865,3.460723853,-5.66503815800001));
#112046=CARTESIAN_POINT('Ctrl Pts',(4.218665792,3.395965514,-5.896215645));
#112047=CARTESIAN_POINT('Ctrl Pts',(5.18500516,3.526465848,-5.419014808));
#112048=CARTESIAN_POINT('Ctrl Pts',(4.88805008300001,3.460723853,-5.703146456));
#112049=CARTESIAN_POINT('Ctrl Pts',(4.561826248,3.395965514,-5.953128697));
#112050=CARTESIAN_POINT('',(4.83414195952737,3.52567991540482,-5.40310757827952));
#112051=CARTESIAN_POINT('Origin',(-0.1412747507766,3.62492147087993,0.133166016273699));
#112052=CARTESIAN_POINT('Ctrl Pts',(5.00040409687358,3.4862983188267,-5.58980848170412));
#112053=CARTESIAN_POINT('Ctrl Pts',(4.97269397672632,3.49254601519868,-5.55863655952063));
#112054=CARTESIAN_POINT('Ctrl Pts',(4.94497036347985,3.49894654282933,-5.527475526028));
#112055=CARTESIAN_POINT('Ctrl Pts',(4.88955971170044,3.51206280603054,-5.46525146593907));
#112056=CARTESIAN_POINT('Ctrl Pts',(4.86184068816916,3.51878610645722,-5.43415251760096));
#112057=CARTESIAN_POINT('Ctrl Pts',(4.83414195911805,3.5256799150601,-5.40310758066948));
#112058=CARTESIAN_POINT('Ctrl Pts',(5.40563495190804,3.39148928096534,-4.83139124279981));
#112059=CARTESIAN_POINT('Ctrl Pts',(5.39659137745394,3.39372739748267,-4.84143409989997));
#112060=CARTESIAN_POINT('Ctrl Pts',(5.38754780300001,3.395965514,-4.851476957));
#112061=CARTESIAN_POINT('Ctrl Pts',(5.124155752,3.461150149,-5.143972888));
#112062=CARTESIAN_POINT('Ctrl Pts',(4.830645328,3.526458173,-5.406233968));
#112063=CARTESIAN_POINT('Ctrl Pts',(5.42515668503526,3.39148928096534,-5.17940461951063));
#112064=CARTESIAN_POINT('Ctrl Pts',(5.41546425676381,3.39372739748267,-5.18948144778356));
#112065=CARTESIAN_POINT('Ctrl Pts',(5.40577182849223,3.395965514,-5.19955827605655));
#112066=CARTESIAN_POINT('Ctrl Pts',(5.12348205749383,3.461150149,-5.49304360974957));
#112067=CARTESIAN_POINT('Ctrl Pts',(4.8110778735632,3.526458173,-5.7542423504641));
#112068=CARTESIAN_POINT('Origin',(-0.138397360011063,3.48214325877107,0.14385621190067));
#112069=CARTESIAN_POINT('Ctrl Pts',(5.885405712,3.526465848,-4.23373353));
#112070=CARTESIAN_POINT('Ctrl Pts',(5.653402532,3.460723853,-4.556246232));
#112071=CARTESIAN_POINT('Ctrl Pts',(5.387547803,3.395965514,-4.85147695700001));
#112072=CARTESIAN_POINT('Ctrl Pts',(6.22871062,3.526465848,-4.177698412));
#112073=CARTESIAN_POINT('Ctrl Pts',(5.999778092,3.460723853,-4.519023783));
#112074=CARTESIAN_POINT('Ctrl Pts',(5.734919982,3.395965514,-4.83329006));
#112075=CARTESIAN_POINT('',(5.8826308220411,3.52567991540452,-4.23758830006617));
#112076=CARTESIAN_POINT('Origin',(-0.166598778539352,3.62492148010577,0.0996829396709153));
#112077=CARTESIAN_POINT('Ctrl Pts',(6.08514101783682,3.48629831886233,-4.38418279590156));
#112078=CARTESIAN_POINT('Ctrl Pts',(6.0513777031033,3.49254601523024,-4.35969651263282));
#112079=CARTESIAN_POINT('Ctrl Pts',(6.01760355145017,3.49894654286214,-4.33522376406252));
#112080=CARTESIAN_POINT('Ctrl Pts',(5.95011203634992,3.51206280606942,-4.28636611987752));
#112081=CARTESIAN_POINT('Ctrl Pts',(5.91635571338162,3.51878610654161,-4.26195301803481));
#112082=CARTESIAN_POINT('Ctrl Pts',(5.88263082133316,3.52567991518665,-4.2375883020626));
#112083=CARTESIAN_POINT('Ctrl Pts',(6.31786051366746,3.39148928095982,-3.55638427523239));
#112084=CARTESIAN_POINT('Ctrl Pts',(6.31118729033379,3.39372739747991,-3.56813643711619));
#112085=CARTESIAN_POINT('Ctrl Pts',(6.304514067,3.395965514,-3.579888599));
#112086=CARTESIAN_POINT('Ctrl Pts',(6.11015795399999,3.461150149,-3.922167643));
#112087=CARTESIAN_POINT('Ctrl Pts',(5.879888021,3.526458173,-4.241393269));
#112088=CARTESIAN_POINT('Ctrl Pts',(6.41173842758416,3.39148928095982,-3.89206469702066));
#112089=CARTESIAN_POINT('Ctrl Pts',(6.40443882310263,3.39372739747991,-3.90398952023208));
#112090=CARTESIAN_POINT('Ctrl Pts',(6.39713921862109,3.395965514,-3.91591434344356));
#112091=CARTESIAN_POINT('Ctrl Pts',(6.18453989704745,3.461150149,-4.26322210937187));
#112092=CARTESIAN_POINT('Ctrl Pts',(5.93558955777851,3.526458173,-4.58547183331436));
#112093=CARTESIAN_POINT('Origin',(-0.166086502363476,3.48214323145688,0.110741551565392));
#112094=CARTESIAN_POINT('Ctrl Pts',(6.657935758,3.526465848,-2.869562936));
#112095=CARTESIAN_POINT('Ctrl Pts',(6.500687381,3.460723853,-3.234409296));
#112096=CARTESIAN_POINT('Ctrl Pts',(6.30451406700001,3.395965514,-3.579888599));
#112097=CARTESIAN_POINT('Ctrl Pts',(6.981168493,3.526465848,-2.741037481));
#112098=CARTESIAN_POINT('Ctrl Pts',(6.830963147,3.460723853,-3.123596581));
#112099=CARTESIAN_POINT('Ctrl Pts',(6.639855232,3.395965514,-3.487452151));
#112100=CARTESIAN_POINT('',(6.65605440469573,3.52567991541251,-2.87392410309611));
#112101=CARTESIAN_POINT('Origin',(-0.184132620657596,3.62492144599365,0.0615385729235612));
#112102=CARTESIAN_POINT('Ctrl Pts',(6.88534350778262,3.48629831885202,-2.97355759548524));
#112103=CARTESIAN_POINT('Ctrl Pts',(6.84710573362347,3.49254601520656,-2.95690190251033));
#112104=CARTESIAN_POINT('Ctrl Pts',(6.80886028528215,3.49894654285973,-2.94026175731254));
#112105=CARTESIAN_POINT('Ctrl Pts',(6.7324437352632,3.5120628060585,-2.90705505827975));
#112106=CARTESIAN_POINT('Ctrl Pts',(6.69422852120966,3.51878610653489,-2.89046933272017));
#112107=CARTESIAN_POINT('Ctrl Pts',(6.65605440477926,3.52567991518518,-2.8739241051104));
#112108=CARTESIAN_POINT('Ctrl Pts',(6.93466993795907,3.39148928115785,-2.11508473291005));
#112109=CARTESIAN_POINT('Ctrl Pts',(6.93067909847946,3.39372739757893,-2.12799668095506));
#112110=CARTESIAN_POINT('Ctrl Pts',(6.926688259,3.395965514,-2.140908629));
#112111=CARTESIAN_POINT('Ctrl Pts',(6.810455961,3.461150149,-2.516966198));
#112112=CARTESIAN_POINT('Ctrl Pts',(6.654193685,3.526458173,-2.878229735));
#112113=CARTESIAN_POINT('Ctrl Pts',(7.09851440741408,3.39148928115785,-2.42273615647617));
#112114=CARTESIAN_POINT('Ctrl Pts',(7.09394894829047,3.39372739757893,-2.43595138255228));
#112115=CARTESIAN_POINT('Ctrl Pts',(7.08938348916687,3.395965514,-2.44916660862833));
#112116=CARTESIAN_POINT('Ctrl Pts',(6.95641552388255,3.461150149,-2.8340570817505));
#112117=CARTESIAN_POINT('Ctrl Pts',(6.78255967079351,3.526458173,-3.20228974984023));
#112118=CARTESIAN_POINT('Origin',(-0.186009880412594,3.48214322465404,0.0724488708943488));
#112119=CARTESIAN_POINT('Ctrl Pts',(7.119148127,3.526465848,-1.371214768));
#112120=CARTESIAN_POINT('Ctrl Pts',(7.044007313,3.460723853,-1.761334976));
#112121=CARTESIAN_POINT('Ctrl Pts',(6.926688259,3.395965514,-2.140908629));
#112122=CARTESIAN_POINT('Ctrl Pts',(7.407194687,3.526465848,-1.176208683));
#112123=CARTESIAN_POINT('Ctrl Pts',(7.342739956,3.460723853,-1.582113474));
#112124=CARTESIAN_POINT('Ctrl Pts',(7.23431823,3.395965514,-1.978544855));
#112125=CARTESIAN_POINT('',(7.11824828114541,3.52567991539768,-1.37587840931426));
#112126=CARTESIAN_POINT('Origin',(-0.193056728397172,3.62492146203427,0.0205167761913733));
#112127=CARTESIAN_POINT('Ctrl Pts',(7.36359498822141,3.48629831884877,-1.42389214575025));
#112128=CARTESIAN_POINT('Ctrl Pts',(7.32267071009219,3.49254601522387,-1.41584584484627));
#112129=CARTESIAN_POINT('Ctrl Pts',(7.28174227990182,3.49894654283125,-1.40781637803124));
#112130=CARTESIAN_POINT('Ctrl Pts',(7.19997384731184,3.51206280602885,-1.3918133327918));
#112131=CARTESIAN_POINT('Ctrl Pts',(7.15908664291011,3.51878610648578,-1.38383051380354));
#112132=CARTESIAN_POINT('Ctrl Pts',(7.11824828113933,3.52567991511134,-1.37587841117221));
#112133=CARTESIAN_POINT('Ctrl Pts',(7.22722190550165,3.39148928110903,-0.574886177936338));
#112134=CARTESIAN_POINT('Ctrl Pts',(7.22610005675088,3.39372739755452,-0.588354164468173));
#112135=CARTESIAN_POINT('Ctrl Pts',(7.224978208,3.395965514,-0.601822151));
#112136=CARTESIAN_POINT('Ctrl Pts',(7.192304617,3.461150149,-0.994074210999999));
#112137=CARTESIAN_POINT('Ctrl Pts',(7.117356647,3.526458173,-1.380483378));
#112138=CARTESIAN_POINT('Ctrl Pts',(7.45337174375708,3.39148928110902,-0.840123164237828));
#112139=CARTESIAN_POINT('Ctrl Pts',(7.45175390547908,3.39372739755452,-0.854010864550351));
#112140=CARTESIAN_POINT('Ctrl Pts',(7.45013606720119,3.395965514,-0.867898564862873));
#112141=CARTESIAN_POINT('Ctrl Pts',(7.40301689346605,3.461150149,-1.27237469374638));
#112142=CARTESIAN_POINT('Ctrl Pts',(7.31238483253964,3.526458173,-1.66937215709889));
#112143=CARTESIAN_POINT('Origin',(-0.197235680099412,3.48214320229941,0.0307684671072975));
#112144=CARTESIAN_POINT('Ctrl Pts',(7.247477043,3.526465848,0.191249878));
#112145=CARTESIAN_POINT('Ctrl Pts',(7.257957291,3.460723853,-0.20590259));
#112146=CARTESIAN_POINT('Ctrl Pts',(7.224978208,3.395965514,-0.601822151));
#112147=CARTESIAN_POINT('Ctrl Pts',(7.48686869,3.526465848,0.443618325));
#112148=CARTESIAN_POINT('Ctrl Pts',(7.511178407,3.460723853,0.033347501));
#112149=CARTESIAN_POINT('Ctrl Pts',(7.49051254899999,3.395965514,-0.377123002));
#112150=CARTESIAN_POINT('',(7.24760077907798,3.52567991540728,0.186501829924383));
#112151=CARTESIAN_POINT('Origin',(-0.192953488755793,3.62492145760987,-0.0214644009633342));
#112152=CARTESIAN_POINT('Ctrl Pts',(7.49753295086236,3.48629831882052,0.192352917068684));
#112153=CARTESIAN_POINT('Ctrl Pts',(7.45583574284632,3.49254601518459,0.191413589910313));
#112154=CARTESIAN_POINT('Ctrl Pts',(7.41413809829101,3.49894654284407,0.190456929640105));
#112155=CARTESIAN_POINT('Ctrl Pts',(7.33084118470806,3.51206280604116,0.188508036656145));
#112156=CARTESIAN_POINT('Ctrl Pts',(7.28919383066968,3.51878610646118,0.187514681429563));
#112157=CARTESIAN_POINT('Ctrl Pts',(7.24760078045297,3.52567991505855,0.186501827635311));
#112158=CARTESIAN_POINT('Ctrl Pts',(7.18183700810298,3.39148928114563,0.992193416467413));
#112159=CARTESIAN_POINT('Ctrl Pts',(7.18363660655154,3.39372739757282,0.978799139733706));
#112160=CARTESIAN_POINT('Ctrl Pts',(7.185436205,3.395965514,0.965404863000001));
#112161=CARTESIAN_POINT('Ctrl Pts',(7.237849103,3.461150149,0.575299581));
#112162=CARTESIAN_POINT('Ctrl Pts',(7.247719923,3.526458173,0.181812848));
#112163=CARTESIAN_POINT('Ctrl Pts',(7.45971770060393,3.39148928114563,0.781773053476565));
#112164=CARTESIAN_POINT('Ctrl Pts',(7.46112313152643,3.39372739757282,0.76786225255639));
#112165=CARTESIAN_POINT('Ctrl Pts',(7.46252856244906,3.395965514,0.753951451636205));
#112166=CARTESIAN_POINT('Ctrl Pts',(7.5034614203627,3.461150149,0.348802519468901));
#112167=CARTESIAN_POINT('Ctrl Pts',(7.5002910056817,3.526458173,-0.0583965774921274));
#112168=CARTESIAN_POINT('Origin',(-0.19923832847399,3.48214324621981,-0.0123506811089137));
#112169=CARTESIAN_POINT('Ctrl Pts',(7.03692198700001,3.526465848,1.744771892));
#112170=CARTESIAN_POINT('Ctrl Pts',(7.132533254,3.460723853,1.359157572));
#112171=CARTESIAN_POINT('Ctrl Pts',(7.185436205,3.395965514,0.965404863));
#112172=CARTESIAN_POINT('Ctrl Pts',(7.216465034,3.526465848,2.042702233));
#112173=CARTESIAN_POINT('Ctrl Pts',(7.328402503,3.460723853,1.647249183));
#112174=CARTESIAN_POINT('Ctrl Pts',(7.39645882600001,3.395965514,1.241932705));
#112175=CARTESIAN_POINT('',(7.03806351988731,3.52567991539917,1.74016145083006));
#112176=CARTESIAN_POINT('Origin',(-0.18382809921942,3.62492146996118,-0.0624418681181543));
#112177=CARTESIAN_POINT('Ctrl Pts',(7.2808946056302,3.48629831885698,1.79960377156328));
#112178=CARTESIAN_POINT('Ctrl Pts',(7.24037418281053,3.49254601522146,1.78972273822684));
#112179=CARTESIAN_POINT('Ctrl Pts',(7.19985705962658,3.49894654290227,1.77982468312599));
#112180=CARTESIAN_POINT('Ctrl Pts',(7.11892653610697,3.51206280609361,1.76001497998509));
#112181=CARTESIAN_POINT('Ctrl Pts',(7.0784664161188,3.5187861065103,1.75009189878341));
#112182=CARTESIAN_POINT('Ctrl Pts',(7.03806352196428,3.52567991509905,1.74016144855234));
#112183=CARTESIAN_POINT('Ctrl Pts',(6.80063739414523,3.3914892811293,2.51287914801983));
#112184=CARTESIAN_POINT('Ctrl Pts',(6.80527429257269,3.39372739756465,2.50018488250989));
#112185=CARTESIAN_POINT('Ctrl Pts',(6.809911191,3.395965514,2.487490617));
#112186=CARTESIAN_POINT('Ctrl Pts',(6.944959809,3.461150149,2.117773005));
#112187=CARTESIAN_POINT('Ctrl Pts',(7.039187871,3.526458173,1.735607707));
#112188=CARTESIAN_POINT('Ctrl Pts',(7.11725554807386,3.39148928112931,2.36711443152031));
#112189=CARTESIAN_POINT('Ctrl Pts',(7.12161853183056,3.39372739756465,2.35383098346513));
#112190=CARTESIAN_POINT('Ctrl Pts',(7.12598151558714,3.395965514,2.34054753540996));
#112191=CARTESIAN_POINT('Ctrl Pts',(7.2530524307516,3.461150149,1.95367011503013));
#112192=CARTESIAN_POINT('Ctrl Pts',(7.33749190763702,3.526458173,1.55530956171755));
#112193=CARTESIAN_POINT('Origin',(-0.191925213453235,3.48214323319159,-0.0548922832923227));
#112194=CARTESIAN_POINT('Ctrl Pts',(6.497328279,3.526465848,3.216710312));
#112195=CARTESIAN_POINT('Ctrl Pts',(6.673599888,3.460723853,2.860665037));
#112196=CARTESIAN_POINT('Ctrl Pts',(6.809911191,3.395965514,2.487490617));
#112197=CARTESIAN_POINT('Ctrl Pts',(6.608627494,3.526465848,3.546271655));
#112198=CARTESIAN_POINT('Ctrl Pts',(6.802958642,3.460723853,3.184127325));
#112199=CARTESIAN_POINT('Ctrl Pts',(6.956554908,3.395965514,2.802917018));
#112200=CARTESIAN_POINT('',(6.49943423274102,3.52567991543021,3.2124530563957));
#112201=CARTESIAN_POINT('Origin',(-0.166107150037931,3.62492145770722,-0.100499613472969));
#112202=CARTESIAN_POINT('Ctrl Pts',(6.72380972081418,3.4862983188088,3.32270715395699));
#112203=CARTESIAN_POINT('Ctrl Pts',(6.68636077307945,3.49254601517424,3.3043464405831));
#112204=CARTESIAN_POINT('Ctrl Pts',(6.64891870713739,3.49894654282947,3.28596981283343));
#112205=CARTESIAN_POINT('Ctrl Pts',(6.57413879475269,3.51206280603208,3.24922557947771));
#112206=CARTESIAN_POINT('Ctrl Pts',(6.536757778616,3.51878610650794,3.23083676461094));
#112207=CARTESIAN_POINT('Ctrl Pts',(6.49943423450968,3.5256799151533,3.21245305497855));
#112208=CARTESIAN_POINT('Ctrl Pts',(6.10144753459324,3.39148928110132,3.91606544530404));
#112209=CARTESIAN_POINT('Ctrl Pts',(6.10870491679661,3.39372739755066,3.90466476065205));
#112210=CARTESIAN_POINT('Ctrl Pts',(6.115962299,3.395965514,3.893264076));
#112211=CARTESIAN_POINT('Ctrl Pts',(6.327331913,3.461150149,3.561221716));
#112212=CARTESIAN_POINT('Ctrl Pts',(6.501511218,3.526458173,3.208247479));
#112213=CARTESIAN_POINT('Ctrl Pts',(6.44199843683067,3.39148928110133,3.84177217006765));
#112214=CARTESIAN_POINT('Ctrl Pts',(6.44911496517995,3.39372739755066,3.82973719410252));
#112215=CARTESIAN_POINT('Ctrl Pts',(6.45623149352924,3.395965514,3.81770221813733));
#112216=CARTESIAN_POINT('Ctrl Pts',(6.66349877090998,3.461150149,3.4671862672109));
#112217=CARTESIAN_POINT('Ctrl Pts',(6.83159984383319,3.526458173,3.09629115331918));
#112218=CARTESIAN_POINT('Origin',(-0.175638016403085,3.48214322456174,-0.0948672503717629));
#112219=CARTESIAN_POINT('Ctrl Pts',(5.653926723,3.526465848,4.538238933));
#112220=CARTESIAN_POINT('Ctrl Pts',(5.902616409,3.460723853,4.228410983));
#112221=CARTESIAN_POINT('Ctrl Pts',(6.115962299,3.395965514,3.893264076));
#112222=CARTESIAN_POINT('Ctrl Pts',(5.691777876,3.526465848,4.884021356));
#112223=CARTESIAN_POINT('Ctrl Pts',(5.959415997,3.460723853,4.572119212));
#112224=CARTESIAN_POINT('Ctrl Pts',(6.191370215,3.395965514,4.232840047));
#112225=CARTESIAN_POINT('',(5.65689862469282,3.5256799154174,4.53453392705498));
#112226=CARTESIAN_POINT('Origin',(-0.140619338899652,3.62492146217939,-0.133858214481626));
#112227=CARTESIAN_POINT('Ctrl Pts',(5.85232696622104,3.48629831880185,4.69044444304518));
#112228=CARTESIAN_POINT('Ctrl Pts',(5.81970056460953,3.4925460151888,4.66446257602376));
#112229=CARTESIAN_POINT('Ctrl Pts',(5.78708430511003,3.49894654285328,4.63846664610451));
#112230=CARTESIAN_POINT('Ctrl Pts',(5.72195162960035,3.51206280607769,4.58650600149994));
#112231=CARTESIAN_POINT('Ctrl Pts',(5.68939761283673,3.5187861065053,4.56051129344055));
#112232=CARTESIAN_POINT('Ctrl Pts',(5.65689862700699,3.52567991510503,4.53453392596363));
#112233=CARTESIAN_POINT('Ctrl Pts',(5.11696076934136,3.39148928110283,5.13614087364819));
#112234=CARTESIAN_POINT('Ctrl Pts',(5.12649928817063,3.39372739755142,5.12656685332415));
#112235=CARTESIAN_POINT('Ctrl Pts',(5.136037807,3.395965514,5.116992833));
#112236=CARTESIAN_POINT('Ctrl Pts',(5.413845009,3.461150149,4.838151658));
#112237=CARTESIAN_POINT('Ctrl Pts',(5.659831125,3.526458173,4.530873164));
#112238=CARTESIAN_POINT('Ctrl Pts',(5.46552063919645,3.39148928110284,5.136792911313));
#112239=CARTESIAN_POINT('Ctrl Pts',(5.47505795112847,3.39372739755142,5.12656914964218));
#112240=CARTESIAN_POINT('Ctrl Pts',(5.48459526306049,3.395965514,5.11634538797148));
#112241=CARTESIAN_POINT('Ctrl Pts',(5.76236731444876,3.461150149,4.81858064331118));
#112242=CARTESIAN_POINT('Ctrl Pts',(6.00626976343008,3.526458173,4.49249361300634));
#112243=CARTESIAN_POINT('Origin',(-0.151138060335976,3.48214328140649,-0.13040629004142));
#112244=CARTESIAN_POINT('Ctrl Pts',(4.546153837,3.526465848,5.647564545));
#112245=CARTESIAN_POINT('Ctrl Pts',(4.85563314700001,3.460723853,5.398441132));
#112246=CARTESIAN_POINT('Ctrl Pts',(5.136037807,3.395965514,5.11699283300001));
#112247=CARTESIAN_POINT('Ctrl Pts',(4.508787052,3.526465848,5.993399646));
#112248=CARTESIAN_POINT('Ctrl Pts',(4.837217683,3.460723853,5.746323886));
#112249=CARTESIAN_POINT('Ctrl Pts',(5.136683932,3.395965514,5.464840179));
#112250=CARTESIAN_POINT('',(4.54985272407115,3.52567991539807,5.64458503122447));
#112251=CARTESIAN_POINT('Origin',(-0.108556179647278,3.62492147900981,-0.160957689453805));
#112252=CARTESIAN_POINT('Ctrl Pts',(4.70719590746653,3.4862983188276,5.83886176251773));
#112253=CARTESIAN_POINT('Ctrl Pts',(4.68091762642385,3.49254601520108,5.8064736252346));
#112254=CARTESIAN_POINT('Ctrl Pts',(4.65465227342764,3.49894654286217,5.77407393406611));
#112255=CARTESIAN_POINT('Ctrl Pts',(4.60221236624675,3.51206280607866,5.70932650065181));
#112256=CARTESIAN_POINT('Ctrl Pts',(4.57600753795857,3.51878610653334,5.67694138305702));
#112257=CARTESIAN_POINT('Ctrl Pts',(4.54985272626207,3.52567991516297,5.64458503070716));
#112258=CARTESIAN_POINT('Ctrl Pts',(3.89321060505149,3.39148928108099,6.11605606300189));
#112259=CARTESIAN_POINT('Ctrl Pts',(3.90458425002574,3.3937273975405,6.10875637750094));
#112260=CARTESIAN_POINT('Ctrl Pts',(3.915957895,3.395965514,6.101456692));
#112261=CARTESIAN_POINT('Ctrl Pts',(4.247212729,3.461150149,5.88885500499999));
#112262=CARTESIAN_POINT('Ctrl Pts',(4.55350362,3.526458173,5.64164025600001));
#112263=CARTESIAN_POINT('Ctrl Pts',(4.23348117065251,3.39148928108099,6.19162292591446));
#112264=CARTESIAN_POINT('Ctrl Pts',(4.24499331214562,3.3937273975405,6.18368843019944));
#112265=CARTESIAN_POINT('Ctrl Pts',(4.25650545363876,3.395965514,6.17575393448438));
#112266=CARTESIAN_POINT('Ctrl Pts',(4.59179396738459,3.461150149,5.94466354376875));
#112267=CARTESIAN_POINT('Ctrl Pts',(4.90009318391137,3.526458173,5.67863206376881));
#112268=CARTESIAN_POINT('Origin',(-0.119570898867882,3.48214322970563,-0.159847509292387));
#112269=CARTESIAN_POINT('Ctrl Pts',(3.22580785,3.526465848,6.49281631600001));
#112270=CARTESIAN_POINT('Ctrl Pts',(3.581605876,3.460723853,6.316046174));
#112271=CARTESIAN_POINT('Ctrl Pts',(3.915957895,3.395965514,6.101456692));
#112272=CARTESIAN_POINT('Ctrl Pts',(3.114970356,3.526465848,6.822533231));
#112273=CARTESIAN_POINT('Ctrl Pts',(3.488836447,3.460723853,6.651836841));
#112274=CARTESIAN_POINT('Ctrl Pts',(3.841812017,3.395965514,6.441310459));
#112275=CARTESIAN_POINT('',(3.23006076639938,3.52567991540093,6.49070161271788));
#112276=CARTESIAN_POINT('Origin',(-0.0714169527961889,3.62492144218,-0.180530784337261));
#112277=CARTESIAN_POINT('Ctrl Pts',(3.34196159965904,3.48629831886319,6.71426039576971));
#112278=CARTESIAN_POINT('Ctrl Pts',(3.32326018235622,3.49254601522207,6.6769804215401));
#112279=CARTESIAN_POINT('Ctrl Pts',(3.30457387463035,3.49894654285152,6.63969194278602));
#112280=CARTESIAN_POINT('Ctrl Pts',(3.26727876750601,3.51206280604764,6.56518523846719));
#112281=CARTESIAN_POINT('Ctrl Pts',(3.24864843637578,3.51878610652078,6.52792400329999));
#112282=CARTESIAN_POINT('Ctrl Pts',(3.23006076876783,3.52567991516642,6.49070161298076));
#112283=CARTESIAN_POINT('Ctrl Pts',(2.48741823989616,3.39148928091091,6.80999126922818));
#112284=CARTESIAN_POINT('Ctrl Pts',(2.5000951924481,3.39372739745545,6.80530724361409));
#112285=CARTESIAN_POINT('Ctrl Pts',(2.512772145,3.395965514,6.800623218));
#112286=CARTESIAN_POINT('Ctrl Pts',(2.881985503,3.461150149,6.664202038));
#112287=CARTESIAN_POINT('Ctrl Pts',(3.234259347,3.526458173,6.48861052000001));
#112288=CARTESIAN_POINT('Ctrl Pts',(2.80348882619201,3.39148928091091,6.95693953369113));
#112289=CARTESIAN_POINT('Ctrl Pts',(2.81643750275045,3.39372739745545,6.9516653120311));
#112290=CARTESIAN_POINT('Ctrl Pts',(2.82938617930894,3.395965514,6.94639109037117));
#112291=CARTESIAN_POINT('Ctrl Pts',(3.20651343716055,3.461150149,6.79278058485489));
#112292=CARTESIAN_POINT('Ctrl Pts',(3.56479369392163,3.526458173,6.59924399066081));
#112293=CARTESIAN_POINT('Origin',(-0.0824129386034567,3.48214323024491,
-0.181814627493688));
#112294=CARTESIAN_POINT('Ctrl Pts',(1.754626674,3.526465848,7.034471212));
#112295=CARTESIAN_POINT('Ctrl Pts',(2.140106694,3.460723853,6.938319916));
#112296=CARTESIAN_POINT('Ctrl Pts',(2.512772145,3.395965514,6.800623218));
#112297=CARTESIAN_POINT('Ctrl Pts',(1.575501108,3.526465848,7.332652744));
#112298=CARTESIAN_POINT('Ctrl Pts',(1.977321095,3.460723853,7.246317299));
#112299=CARTESIAN_POINT('Ctrl Pts',(2.367301242,3.395965514,7.11659222));
#112300=CARTESIAN_POINT('',(1.7592347577013,3.52567991540696,7.03332020118498));
#112301=CARTESIAN_POINT('Origin',(-0.0309385539742335,3.62492149359909,
-0.191662856884642));
#112302=CARTESIAN_POINT('Ctrl Pts',(1.82046088137077,3.48629831883827,7.27570767517235));
#112303=CARTESIAN_POINT('Ctrl Pts',(1.81021078533887,3.49254601521445,7.23527903401874));
#112304=CARTESIAN_POINT('Ctrl Pts',(1.79997727388744,3.49894654284948,7.19484533535449));
#112305=CARTESIAN_POINT('Ctrl Pts',(1.77957084490071,3.51206280606853,7.11406321064714));
#112306=CARTESIAN_POINT('Ctrl Pts',(1.76938614485983,3.51878610653735,7.07366815198741));
#112307=CARTESIAN_POINT('Ctrl Pts',(1.75923476045434,3.52567991517846,7.03332020138535));
#112308=CARTESIAN_POINT('Ctrl Pts',(0.965316962573027,3.39148928101642,
7.18549885113208));
#112309=CARTESIAN_POINT('Ctrl Pts',(0.978704461786508,3.39372739750821,
7.18364950556611));
#112310=CARTESIAN_POINT('Ctrl Pts',(0.992091961,3.395965514,7.18180016));
#112311=CARTESIAN_POINT('Ctrl Pts',(1.381999838,3.461150149,7.12793839));
#112312=CARTESIAN_POINT('Ctrl Pts',(1.763784701,3.526458173,7.032180567));
#112313=CARTESIAN_POINT('Ctrl Pts',(1.24240846170559,3.3914892810164,7.39695738031954));
#112314=CARTESIAN_POINT('Ctrl Pts',(1.25618820682695,3.39372739750821,7.39459004977929));
#112315=CARTESIAN_POINT('Ctrl Pts',(1.26996795194829,3.395965514,7.39222271923901));
#112316=CARTESIAN_POINT('Ctrl Pts',(1.67129990201468,3.461150149,7.32327475439529));
#112317=CARTESIAN_POINT('Ctrl Pts',(2.06280841283414,3.526458173,7.21128260347993));
#112318=CARTESIAN_POINT('Origin',(-0.0414014279420537,3.48214326373977,
-0.195280406556784));
#112319=CARTESIAN_POINT('Ctrl Pts',(0.201401104,3.526465848,7.247202053));
#112320=CARTESIAN_POINT('Ctrl Pts',(0.598538503,3.460723853,7.23616553));
#112321=CARTESIAN_POINT('Ctrl Pts',(0.992091961000001,3.395965514,7.18180016));
#112322=CARTESIAN_POINT('Ctrl Pts',(-0.037636821,3.526465848,7.499905564));
#112323=CARTESIAN_POINT('Ctrl Pts',(0.373348407,3.460723853,7.501968014));
#112324=CARTESIAN_POINT('Ctrl Pts',(0.782098092,3.395965514,7.459110039));
#112325=CARTESIAN_POINT('',(0.206148887086937,3.52567991542637,7.24706855394498));
#112326=CARTESIAN_POINT('Origin',(0.0109866099485638,3.62492146493991,-0.193832750940208));
#112327=CARTESIAN_POINT('Ctrl Pts',(0.213837435628791,3.48629831884979,
7.49695094993265));
#112328=CARTESIAN_POINT('Ctrl Pts',(0.212517943928668,3.49254601521909,
7.45526404033161));
#112329=CARTESIAN_POINT('Ctrl Pts',(0.211215736273181,3.49894654286066,
7.41357575659991));
#112330=CARTESIAN_POINT('Ctrl Pts',(0.208652167091656,3.51206280608243,
7.33029549416932));
#112331=CARTESIAN_POINT('Ctrl Pts',(0.207389323161436,3.51878610655237,
7.2886554401733));
#112332=CARTESIAN_POINT('Ctrl Pts',(0.206148889088203,3.52567991520143,
7.24706855474586));
#112333=CARTESIAN_POINT('Ctrl Pts',(-0.601921461963398,3.39148928102925,
7.22502049361108));
#112334=CARTESIAN_POINT('Ctrl Pts',(-0.588449400481704,3.39372739751463,
7.22609230130554));
#112335=CARTESIAN_POINT('Ctrl Pts',(-0.574977339,3.395965514,7.227164109));
#112336=CARTESIAN_POINT('Ctrl Pts',(-0.182606604,3.461150149,7.258380265));
#112337=CARTESIAN_POINT('Ctrl Pts',(0.210837442,3.526458173,7.246933667));
#112338=CARTESIAN_POINT('Ctrl Pts',(-0.376765541909082,3.39148928102926,
7.49110172164201));
#112339=CARTESIAN_POINT('Ctrl Pts',(-0.362799053537817,3.39372739751463,
7.49175197583758));
#112340=CARTESIAN_POINT('Ctrl Pts',(-0.348832565166553,3.395965514,7.49240223003305));
#112341=CARTESIAN_POINT('Ctrl Pts',(0.0579382408488792,3.461150149,7.51134073598912));
#112342=CARTESIAN_POINT('Ctrl Pts',(0.46436850244113,3.526458173,7.48612965584789));
#112343=CARTESIAN_POINT('Origin',(0.00154602868513654,3.48214325210162,
-0.199614718843649));
#112344=CARTESIAN_POINT('Ctrl Pts',(0.201310764,2.492226207,7.247204563));
#112345=CARTESIAN_POINT('Ctrl Pts',(0.597708493,2.42647128,7.236193541));
#112346=CARTESIAN_POINT('Ctrl Pts',(0.990540534000001,2.361474582,7.182014303));
#112347=CARTESIAN_POINT('Ctrl Pts',(0.994451674780801,2.36082745750497,
7.1814748800276));
#112348=CARTESIAN_POINT('Ctrl Pts',(0.998362815561602,2.36018033300993,
7.18093545705518));
#112349=CARTESIAN_POINT('Ctrl Pts',(-0.03773031,2.492226207,7.499905094));
#112350=CARTESIAN_POINT('Ctrl Pts',(0.372489288,2.42647128,7.501968815));
#112351=CARTESIAN_POINT('Ctrl Pts',(0.780486766,2.361474582,7.45927881300001));
#112352=CARTESIAN_POINT('Ctrl Pts',(0.78454889792439,2.36082745750497,7.4588537799316));
#112353=CARTESIAN_POINT('Ctrl Pts',(0.788611029848782,2.36018033300993,
7.45842874686319));
#112354=CARTESIAN_POINT('',(0.213277379534241,2.452029426852,7.49696690919716));
#112355=CARTESIAN_POINT('',(0.780486763977484,2.36147458149274,7.45927881126999));
#112356=CARTESIAN_POINT('Origin',(0.0109054895757806,2.55351791639885,-0.188512452785666));
#112357=CARTESIAN_POINT('',(0.885513641295677,2.36147458056994,7.32064655905289));
#112358=CARTESIAN_POINT('Ctrl Pts',(0.21327737739871,2.45202942666989,7.49696690365892));
#112359=CARTESIAN_POINT('Ctrl Pts',(0.212033149998612,2.45828501820065,
7.45527809421543));
#112360=CARTESIAN_POINT('Ctrl Pts',(0.210806624554835,2.46469207979751,
7.41358805137032));
#112361=CARTESIAN_POINT('Ctrl Pts',(0.208395237952903,2.47781843917276,
7.33030329110628));
#112362=CARTESIAN_POINT('Ctrl Pts',(0.207208999418987,2.48454521298205,
7.28866109792748));
#112363=CARTESIAN_POINT('Ctrl Pts',(0.206045687659983,2.49144077620845,
7.2470715019965));
#112364=CARTESIAN_POINT('Ctrl Pts',(0.98273624710617,2.36016764195642,7.18309066712261));
#112365=CARTESIAN_POINT('Ctrl Pts',(0.986638390553085,2.36082111197821,
7.18255248506131));
#112366=CARTESIAN_POINT('Ctrl Pts',(0.990540534,2.361474582,7.18201430300001));
#112367=CARTESIAN_POINT('Ctrl Pts',(1.381189167,2.426894312,7.12813620000001));
#112368=CARTESIAN_POINT('Ctrl Pts',(1.763689251,2.492218586,7.032204507));
#112369=CARTESIAN_POINT('Ctrl Pts',(1.25977250362045,2.36016764195642,7.39344572270517));
#112370=CARTESIAN_POINT('Ctrl Pts',(1.26378877381022,2.36082111197821,7.39275689685258));
#112371=CARTESIAN_POINT('Ctrl Pts',(1.267805044,2.361474582,7.392068071));
#112372=CARTESIAN_POINT('Ctrl Pts',(1.669879053,2.426894312,7.323108823));
#112373=CARTESIAN_POINT('Ctrl Pts',(2.062101341,2.492218586,7.210945712));
#112374=CARTESIAN_POINT('',(1.26780503971333,2.36147458096339,7.39206804979796));
#112375=CARTESIAN_POINT('',(1.81991734971456,2.45202942680341,7.27584365708309));
#112376=CARTESIAN_POINT('Origin',(-0.0403900291321555,2.41071409422485,
-0.188786091166397));
#112377=CARTESIAN_POINT('Ctrl Pts',(1.75913460499445,2.49144077640748,7.03334526460813));
#112378=CARTESIAN_POINT('Ctrl Pts',(1.76921125281641,2.48454521318186,7.07371244111567));
#112379=CARTESIAN_POINT('Ctrl Pts',(1.77932159849006,2.47781843922911,7.11412605749383));
#112380=CARTESIAN_POINT('Ctrl Pts',(1.79958036973389,2.46469207981283,7.19494528958312));
#112381=CARTESIAN_POINT('Ctrl Pts',(1.80974034658981,2.4582850181691,7.2353969759097));
#112382=CARTESIAN_POINT('Ctrl Pts',(1.81991734640429,2.45202942659619,7.27584365226265));
#112383=CARTESIAN_POINT('',(1.12917279935051,2.36147458031212,7.28704118539612));
#112384=CARTESIAN_POINT('Origin',(2.63894808782972E-13,2.45311202899967,
7.8236028766554E-13));
#112385=CARTESIAN_POINT('',(1.82645773667202,2.27159573076564,7.27420457036109));
#112386=CARTESIAN_POINT('Ctrl Pts',(1.8264577281804,2.27159573309127,7.27420457225405));
#112387=CARTESIAN_POINT('Ctrl Pts',(1.7973070705304,2.27631121118619,7.28152392215389));
#112388=CARTESIAN_POINT('Ctrl Pts',(1.76813109415185,2.28101755501093,7.28866334775712));
#112389=CARTESIAN_POINT('Ctrl Pts',(1.73893308895609,2.28571428598668,7.29562277789647));
#112390=CARTESIAN_POINT('Ctrl Pts',(1.59152439382906,2.30942614431015,7.33075807194632));
#112391=CARTESIAN_POINT('Ctrl Pts',(1.4425453427614,2.33338333523652,7.36154196553795));
#112392=CARTESIAN_POINT('Ctrl Pts',(1.29238815216021,2.35752265772375,7.38780974699737));
#112393=CARTESIAN_POINT('Ctrl Pts',(1.28419726093286,2.3588394282627,7.38924262237188));
#112394=CARTESIAN_POINT('Ctrl Pts',(1.27600287000738,2.36015673981136,7.39066207115902));
#112395=CARTESIAN_POINT('Ctrl Pts',(1.26780504503328,2.36147458179854,7.39206807061842));
#112396=CARTESIAN_POINT('',(2.36576386665489,2.36147458149275,7.11710343474374));
#112397=CARTESIAN_POINT('Origin',(-0.0678177627952725,2.41070047484541,
-0.178936091179097));
#112398=CARTESIAN_POINT('Origin',(-0.029874064411306,2.55351790539617,-0.186449428114565));
#112399=CARTESIAN_POINT('Ctrl Pts',(1.754538986,2.492226207,7.034493084));
#112400=CARTESIAN_POINT('Ctrl Pts',(2.139302112,2.42647128,6.938525699));
#112401=CARTESIAN_POINT('Ctrl Pts',(2.511303023,2.361474582,6.801165865));
#112402=CARTESIAN_POINT('Ctrl Pts',(2.5150067634836,2.36082745750497,6.7997982737846));
#112403=CARTESIAN_POINT('Ctrl Pts',(2.5187105039672,2.36018033300993,6.79843068256919));
#112404=CARTESIAN_POINT('Ctrl Pts',(1.575409703,2.492226207,7.332672382));
#112405=CARTESIAN_POINT('Ctrl Pts',(1.976482234,2.42647128,7.246502767));
#112406=CARTESIAN_POINT('Ctrl Pts',(2.365763869,2.361474582,7.117103436));
#112407=CARTESIAN_POINT('Ctrl Pts',(2.36963966098986,2.36082745750497,7.11581510167983));
#112408=CARTESIAN_POINT('Ctrl Pts',(2.37351545297971,2.36018033300993,7.11452676735966));
#112409=CARTESIAN_POINT('',(2.43853343772574,2.36147458056998,6.95913465339936));
#112410=CARTESIAN_POINT('Ctrl Pts',(2.50391258247664,2.36016764195642,6.80389475530675));
#112411=CARTESIAN_POINT('Ctrl Pts',(2.50760780273832,2.36082111197821,6.80253031015338));
#112412=CARTESIAN_POINT('Ctrl Pts',(2.511303023,2.361474582,6.801165865));
#112413=CARTESIAN_POINT('Ctrl Pts',(2.881236308,2.426894312,6.664569494));
#112414=CARTESIAN_POINT('Ctrl Pts',(3.234171275,2.492218586,6.48865441900001));
#112415=CARTESIAN_POINT('Ctrl Pts',(2.81969200434841,2.36016764195642,6.94977722071898));
#112416=CARTESIAN_POINT('Ctrl Pts',(2.82346629917421,2.36082111197821,6.94824111985949));
#112417=CARTESIAN_POINT('Ctrl Pts',(2.827240594,2.361474582,6.946705019));
#112418=CARTESIAN_POINT('Ctrl Pts',(3.205090136,2.426894312,6.79292397300001));
#112419=CARTESIAN_POINT('Ctrl Pts',(3.564030731,2.492218586,6.599066975));
#112420=CARTESIAN_POINT('',(2.82724058529781,2.36147458096342,6.9467049992098));
#112421=CARTESIAN_POINT('',(3.34146000745496,2.45202942687121,6.71451004157885));
#112422=CARTESIAN_POINT('Origin',(-0.0800291984243725,2.4107140862089,-0.175689795986495));
#112423=CARTESIAN_POINT('Ctrl Pts',(3.22996834292614,2.49144077637346,6.49074762063525));
#112424=CARTESIAN_POINT('Ctrl Pts',(3.24848715411197,2.48454521317637,6.52800485345517));
#112425=CARTESIAN_POINT('Ctrl Pts',(3.26704885856273,2.47781843923068,6.56530019645369));
#112426=CARTESIAN_POINT('Ctrl Pts',(3.30420772731042,2.46469208329873,6.63987486303306));
#112427=CARTESIAN_POINT('Ctrl Pts',(3.32282607478242,2.45828502541683,6.67719669328445));
#112428=CARTESIAN_POINT('Ctrl Pts',(3.34146000317469,2.45202942670672,6.7145100372272));
#112429=CARTESIAN_POINT('',(2.66927181826374,2.36147458031212,6.87393543820857));
#112430=CARTESIAN_POINT('Origin',(4.52112305926455E-13,2.45311202899922,
9.03357250114922E-13));
#112431=CARTESIAN_POINT('',(3.34749512840975,2.27159573075016,6.71150328609892));
#112432=CARTESIAN_POINT('Ctrl Pts',(3.34749512062753,2.27159573306644,6.71150328981358));
#112433=CARTESIAN_POINT('Ctrl Pts',(3.32059943308098,2.27631121117738,6.724918047135));
#112434=CARTESIAN_POINT('Ctrl Pts',(3.29364034028498,2.28101755501029,6.73816252941245));
#112435=CARTESIAN_POINT('Ctrl Pts',(3.26662103989866,2.28571428600481,6.75123595998502));
#112436=CARTESIAN_POINT('Ctrl Pts',(3.13021152700453,2.309426179206,6.81723841983366));
#112437=CARTESIAN_POINT('Ctrl Pts',(2.99133294332461,2.33338340554088,6.87932878025919));
#112438=CARTESIAN_POINT('Ctrl Pts',(2.85033292833529,2.35752276396414,6.93726186564666));
#112439=CARTESIAN_POINT('Ctrl Pts',(2.84264176798055,2.35883949911844,6.94042195502391));
#112440=CARTESIAN_POINT('Ctrl Pts',(2.83494430377073,2.36015677525334,6.9435696847162));
#112441=CARTESIAN_POINT('Ctrl Pts',(2.8272405949271,2.36147458179854,6.94670501840523));
#112442=CARTESIAN_POINT('',(3.84042048042676,2.36147458149274,6.44214021129295));
#112443=CARTESIAN_POINT('Origin',(-0.104698240445678,2.41070046968801,-0.160173936573987));
#112444=CARTESIAN_POINT('Origin',(-0.0692568098882768,2.55351788595202,
-0.175668412511882));
#112445=CARTESIAN_POINT('Ctrl Pts',(3.225726914,2.492226207,6.492856527));
#112446=CARTESIAN_POINT('Ctrl Pts',(3.580864341,2.42647128,6.316420107));
#112447=CARTESIAN_POINT('Ctrl Pts',(3.914639774,2.361474582,6.10230247));
#112448=CARTESIAN_POINT('Ctrl Pts',(3.91796293140924,2.36082745750497,6.10017065758514));
#112449=CARTESIAN_POINT('Ctrl Pts',(3.92128608881848,2.36018033300993,6.09803884517028));
#112450=CARTESIAN_POINT('Ctrl Pts',(3.11488531,2.492226207,6.82257206));
#112451=CARTESIAN_POINT('Ctrl Pts',(3.488057068,2.42647128,6.652198303));
#112452=CARTESIAN_POINT('Ctrl Pts',(3.840420483,2.361474582,6.442140212));
#112453=CARTESIAN_POINT('Ctrl Pts',(3.84392870732549,2.36082745750497,6.44004881750999));
#112454=CARTESIAN_POINT('Ctrl Pts',(3.84743693165098,2.36018033300993,6.43795742301998));
#112455=CARTESIAN_POINT('',(3.87753012104247,2.36147458056998,6.2722213456103));
#112456=CARTESIAN_POINT('Ctrl Pts',(3.908008748627,2.36016764195642,6.10655628662292));
#112457=CARTESIAN_POINT('Ctrl Pts',(3.9113242613135,2.36082111197821,6.10442937831146));
#112458=CARTESIAN_POINT('Ctrl Pts',(3.914639774,2.361474582,6.10230247));
#112459=CARTESIAN_POINT('Ctrl Pts',(4.246560042,2.426894312,5.889374925));
#112460=CARTESIAN_POINT('Ctrl Pts',(4.553427044,2.492218586,5.641702062));
#112461=CARTESIAN_POINT('Ctrl Pts',(4.24776584072616,2.36016764195642,6.18114485999082));
#112462=CARTESIAN_POINT('Ctrl Pts',(4.25112167836308,2.36082111197821,6.17883331049541));
#112463=CARTESIAN_POINT('Ctrl Pts',(4.254477516,2.361474582,6.176521761));
#112464=CARTESIAN_POINT('Ctrl Pts',(4.590434767,2.426894312,5.945109548));
#112465=CARTESIAN_POINT('Ctrl Pts',(4.899310006,2.492218586,5.678623201));
#112466=CARTESIAN_POINT('',(4.2544775032456,2.36147458096339,6.17652174354511));
#112467=CARTESIAN_POINT('',(4.70675970893107,2.45202942683396,5.83921339942039));
#112468=CARTESIAN_POINT('Origin',(-0.115926191916461,2.41071410523568,-0.154378239308755));
#112469=CARTESIAN_POINT('Ctrl Pts',(4.54977235062771,2.49144077650933,5.64464983131305));
#112470=CARTESIAN_POINT('Ctrl Pts',(4.5758674060766,2.48454521330205,5.67705501364799));
#112471=CARTESIAN_POINT('Ctrl Pts',(4.60201254479543,2.47781843927961,5.70948819475178));
#112472=CARTESIAN_POINT('Ctrl Pts',(4.65433402260713,2.46469207987452,5.77433130573284));
#112473=CARTESIAN_POINT('Ctrl Pts',(4.68054019026222,2.45828501822244,5.80677819834295));
#112474=CARTESIAN_POINT('Ctrl Pts',(4.70675970388043,2.45202942664259,5.83921339628418));
#112475=CARTESIAN_POINT('',(4.08455865372057,2.3614745803121,6.13941210969819));
#112476=CARTESIAN_POINT('Origin',(1.24856722183431E-12,2.45311202899956,
1.52005144582468E-12));
#112477=CARTESIAN_POINT('',(4.71200736856892,2.27159573077527,5.83497956779286));
#112478=CARTESIAN_POINT('Ctrl Pts',(4.71200736155291,2.27159573310906,5.83497957305765));
#112479=CARTESIAN_POINT('Ctrl Pts',(4.68862425625641,2.27631121119035,5.85386247845562));
#112480=CARTESIAN_POINT('Ctrl Pts',(4.66514262405863,2.28101755500929,5.87259272007343));
#112481=CARTESIAN_POINT('Ctrl Pts',(4.64156542103399,2.28571428599323,5.89116885197322));
#112482=CARTESIAN_POINT('Ctrl Pts',(4.52253390152555,2.30942613223479,5.98495203822414));
#112483=CARTESIAN_POINT('Ctrl Pts',(4.40025006189854,2.33338331075958,6.07544537852409));
#112484=CARTESIAN_POINT('Ctrl Pts',(4.27500070883594,2.35752262072372,6.16233469842595));
#112485=CARTESIAN_POINT('Ctrl Pts',(4.2681684422202,2.35883940358577,6.16707445144753));
#112486=CARTESIAN_POINT('Ctrl Pts',(4.26132736152242,2.36015672746786,6.17180348811389));
#112487=CARTESIAN_POINT('Ctrl Pts',(4.25447751677773,2.36147458179851,6.17652176021973));
#112488=CARTESIAN_POINT('',(5.13550330134351,2.36147458149276,5.46594967184533));
#112489=CARTESIAN_POINT('Origin',(-0.136683026004824,2.41070043159255,-0.133922036617143));
#112490=CARTESIAN_POINT('Origin',(-0.105401060621905,2.55351787062719,-0.156673127077545));
#112491=CARTESIAN_POINT('Ctrl Pts',(4.546083437,2.492226207,5.647621215));
#112492=CARTESIAN_POINT('Ctrl Pts',(4.854989334,2.42647128,5.398965732));
#112493=CARTESIAN_POINT('Ctrl Pts',(5.13493232,2.361474582,5.118102194));
#112494=CARTESIAN_POINT('Ctrl Pts',(5.13771950718071,2.36082745750497,5.11530584155758));
#112495=CARTESIAN_POINT('Ctrl Pts',(5.1405066943614,2.36018033300993,5.11250948911515));
#112496=CARTESIAN_POINT('Ctrl Pts',(4.508712341,2.492226207,5.99345585));
#112497=CARTESIAN_POINT('Ctrl Pts',(4.83653423,2.42647128,5.74684444));
#112498=CARTESIAN_POINT('Ctrl Pts',(5.135503304,2.361474582,5.465949672));
#112499=CARTESIAN_POINT('Ctrl Pts',(5.13847991999737,2.36082745750497,5.46315300862335));
#112500=CARTESIAN_POINT('Ctrl Pts',(5.14145653599474,2.36018033300993,5.46035634524671));
#112501=CARTESIAN_POINT('',(5.13521780570789,2.36147458056998,5.29202593910566));
#112502=CARTESIAN_POINT('Ctrl Pts',(5.1293707691374,2.36016764195642,5.12368203318865));
#112503=CARTESIAN_POINT('Ctrl Pts',(5.13215154456869,2.36082111197821,5.12089211359432));
#112504=CARTESIAN_POINT('Ctrl Pts',(5.13493232,2.361474582,5.118102194));
#112505=CARTESIAN_POINT('Ctrl Pts',(5.413319349,2.426894312,4.838799731));
#112506=CARTESIAN_POINT('Ctrl Pts',(5.659769626,2.492218586,4.530949987));
#112507=CARTESIAN_POINT('Ctrl Pts',(5.47721886760684,2.36016764195642,5.12348903528974));
#112508=CARTESIAN_POINT('Ctrl Pts',(5.47999933280342,2.36082111197821,5.12051012264487));
#112509=CARTESIAN_POINT('Ctrl Pts',(5.48277979800001,2.361474582,5.11753121));
#112510=CARTESIAN_POINT('Ctrl Pts',(5.761135769,2.426894312,4.819308408));
#112511=CARTESIAN_POINT('Ctrl Pts',(6.00550299000001,2.492218586,4.492653318));
#112512=CARTESIAN_POINT('',(5.48277978178718,2.36147458096342,5.11753119569418));
#112513=CARTESIAN_POINT('',(5.85197655738761,2.45202942686292,4.69088162852638));
#112514=CARTESIAN_POINT('Origin',(-0.146402830297621,2.41071406611784,-0.12584841218946));
#112515=CARTESIAN_POINT('Ctrl Pts',(5.65683406098997,2.49144077636711,4.53461449072042));
#112516=CARTESIAN_POINT('Ctrl Pts',(5.68928518494927,2.48454521316727,4.56065239240826));
#112517=CARTESIAN_POINT('Ctrl Pts',(5.72179123964571,2.47781843924977,4.58670687141016));
#112518=CARTESIAN_POINT('Ctrl Pts',(5.78682882247503,2.46469207986781,4.63878641528251));
#112519=CARTESIAN_POINT('Ctrl Pts',(5.81939742714816,2.45828501824452,4.66484116602438));
#112520=CARTESIAN_POINT('Ctrl Pts',(5.85197655176899,2.45202942668633,4.69088162653268));
#112521=CARTESIAN_POINT('',(5.30885606626941,2.36147458031211,5.11781669445923));
#112522=CARTESIAN_POINT('Origin',(5.25187532351978E-13,2.45311202899933,
3.48245737802344E-13));
#112523=CARTESIAN_POINT('',(5.85619138107285,2.27159573078832,4.68561868955803));
#112524=CARTESIAN_POINT('Ctrl Pts',(5.85619137521515,2.27159573313753,4.68561869622839));
#112525=CARTESIAN_POINT('Ctrl Pts',(5.8374142203088,2.27631121119808,4.70908680616086));
#112526=CARTESIAN_POINT('Ctrl Pts',(5.81850802386978,2.28101755500772,4.73242700194082));
#112527=CARTESIAN_POINT('Ctrl Pts',(5.79947536200712,2.28571428599824,4.75563723599132));
#112528=CARTESIAN_POINT('Ctrl Pts',(5.70338729269073,2.30942614547804,4.87281614740652));
#112529=CARTESIAN_POINT('Ctrl Pts',(5.60341571685522,2.33338333746231,4.98748127694228));
#112530=CARTESIAN_POINT('Ctrl Pts',(5.49977319763934,2.35752266107725,5.0992641401815));
#112531=CARTESIAN_POINT('Ctrl Pts',(5.4941196299469,2.3588394304991,5.10536175329394));
#112532=CARTESIAN_POINT('Ctrl Pts',(5.48845515076391,2.3601567409299,5.11145079553456));
#112533=CARTESIAN_POINT('Ctrl Pts',(5.48277979859175,2.36147458179852,5.11753120907084));
#112534=CARTESIAN_POINT('',(6.19045569537311,2.36147458149269,4.23417740041582));
#112535=CARTESIAN_POINT('Origin',(-0.162276638322637,2.4107004468959,-0.101408132842024));
#112536=CARTESIAN_POINT('Origin',(-0.136617111854956,2.55351791166208,-0.130352226288843));
#112537=CARTESIAN_POINT('Ctrl Pts',(5.653870151,2.492226207,4.538309411));
#112538=CARTESIAN_POINT('Ctrl Pts',(5.902100421,2.42647128,4.229061719));
#112539=CARTESIAN_POINT('Ctrl Pts',(6.115121138,2.361474582,3.894585148));
#112540=CARTESIAN_POINT('Ctrl Pts',(6.11724202918621,2.36082745750497,3.89125500987346));
#112541=CARTESIAN_POINT('Ctrl Pts',(6.1193629203724,2.36018033300994,3.88792487174692));
#112542=CARTESIAN_POINT('Ctrl Pts',(5.69171699500001,2.492226207,4.884092306));
#112543=CARTESIAN_POINT('Ctrl Pts',(5.958860426,2.42647128,4.572774518));
#112544=CARTESIAN_POINT('Ctrl Pts',(6.190455698,2.361474582,4.2341774));
#112545=CARTESIAN_POINT('Ctrl Pts',(6.19276152241965,2.36082745750497,4.23080623660635));
#112546=CARTESIAN_POINT('Ctrl Pts',(6.1950673468393,2.36018033300994,4.2274350732127));
#112547=CARTESIAN_POINT('',(6.15278841316685,2.36147458056978,4.06438128131659));
#112548=CARTESIAN_POINT('Ctrl Pts',(6.11088911360345,2.36016764195642,3.90123010271037));
#112549=CARTESIAN_POINT('Ctrl Pts',(6.11300512580173,2.36082111197821,3.89790762535519));
#112550=CARTESIAN_POINT('Ctrl Pts',(6.11512113800001,2.361474582,3.894585148));
#112551=CARTESIAN_POINT('Ctrl Pts',(6.326957859,2.426894312,3.561967638));
#112552=CARTESIAN_POINT('Ctrl Pts',(6.50146767100001,2.492218586,3.208335726));
#112553=CARTESIAN_POINT('Ctrl Pts',(6.45056322737555,2.36016764195642,3.82626455831515));
#112554=CARTESIAN_POINT('Ctrl Pts',(6.45263830868778,2.36082111197821,3.82275757315758));
#112555=CARTESIAN_POINT('Ctrl Pts',(6.45471339,2.361474582,3.819250588));
#112556=CARTESIAN_POINT('Ctrl Pts',(6.662452467,2.426894312,3.468161763));
#112557=CARTESIAN_POINT('Ctrl Pts',(6.830885329,2.492218586,3.096611959));
#112558=CARTESIAN_POINT('',(6.45471337105975,2.36147458096336,3.81925057755459));
#112559=CARTESIAN_POINT('',(6.72356148620511,2.45202942682532,3.32320944645836));
#112560=CARTESIAN_POINT('Origin',(-0.170033501176531,2.41071412305941,-0.0914337445244639));
#112561=CARTESIAN_POINT('Ctrl Pts',(6.49938849766516,2.49144077636212,3.2125456154371));
#112562=CARTESIAN_POINT('Ctrl Pts',(6.53667831149826,2.48454521316004,3.23099873309163));
#112563=CARTESIAN_POINT('Ctrl Pts',(6.57402533555748,2.47781843922486,3.24945623208448));
#112564=CARTESIAN_POINT('Ctrl Pts',(6.64873793827138,2.46469207983345,3.28633702754683));
#112565=CARTESIAN_POINT('Ctrl Pts',(6.68614610834328,2.4582850181975,3.3047813455483));
#112566=CARTESIAN_POINT('Ctrl Pts',(6.72356148043066,2.45202942662919,3.32320944593048));
#112567=CARTESIAN_POINT('',(6.28491726947834,2.36147458031213,3.85691785907295));
#112568=CARTESIAN_POINT('Origin',(7.02563007770607E-14,2.45311202899911,
-5.33427468862868E-14));
#112569=CARTESIAN_POINT('',(6.72654639328456,2.27159573075196,3.31716348945614));
#112570=CARTESIAN_POINT('Ctrl Pts',(6.72654638901667,2.27159573310009,3.31716349722683));
#112571=CARTESIAN_POINT('Ctrl Pts',(6.71325318346979,2.27631121117457,3.34411946911683));
#112572=CARTESIAN_POINT('Ctrl Pts',(6.69980645556126,2.28101755499664,3.3709782575355));
#112573=CARTESIAN_POINT('Ctrl Pts',(6.6862082810288,2.28571428598099,3.3977373088993));
#112574=CARTESIAN_POINT('Ctrl Pts',(6.61755681684858,2.30942610477132,3.53283250499352));
#112575=CARTESIAN_POINT('Ctrl Pts',(6.5445722664743,2.33338325540565,3.66630753594886));
#112576=CARTESIAN_POINT('Ctrl Pts',(6.46738300984023,2.35752253707386,3.79775683820576));
#112577=CARTESIAN_POINT('Ctrl Pts',(6.46317229461663,2.35883934779648,3.80492746793172));
#112578=CARTESIAN_POINT('Ctrl Pts',(6.45894907973879,2.3601566995621,3.81209207243943));
#112579=CARTESIAN_POINT('Ctrl Pts',(6.4547133903781,2.36147458179854,3.81925058696547));
#112580=CARTESIAN_POINT('',(6.95594926052349,2.36147458149275,2.80441969999315));
#112581=CARTESIAN_POINT('Origin',(-0.180282775616545,2.4107004840551,-0.0641527183467833));
#112582=CARTESIAN_POINT('Origin',(-0.161444725146068,2.55351788295849,-0.0979359078788294));
#112583=CARTESIAN_POINT('Ctrl Pts',(6.497288181,2.492226207,3.216791304));
#112584=CARTESIAN_POINT('Ctrl Pts',(6.67323585300001,2.42647128,2.86141148));
#112585=CARTESIAN_POINT('Ctrl Pts',(6.809373687,2.361474582,2.488961628));
#112586=CARTESIAN_POINT('Ctrl Pts',(6.81072911165684,2.36082745750497,2.48525341773983));
#112587=CARTESIAN_POINT('Ctrl Pts',(6.81208453631367,2.36018033300993,2.48154520747966));
#112588=CARTESIAN_POINT('Ctrl Pts',(6.60858328699999,2.492226207,3.546354034));
#112589=CARTESIAN_POINT('Ctrl Pts',(6.802556932,2.42647128,3.184886742));
#112590=CARTESIAN_POINT('Ctrl Pts',(6.955949263,2.361474582,2.804419699));
#112591=CARTESIAN_POINT('Ctrl Pts',(6.95747647804007,2.36082745750497,2.80063166744372));
#112592=CARTESIAN_POINT('Ctrl Pts',(6.95900369308013,2.36018033300993,2.79684363588743));
#112593=CARTESIAN_POINT('',(6.88266147185314,2.36147458056998,2.64669067168334));
#112594=CARTESIAN_POINT('Ctrl Pts',(6.80666907381407,2.36016764195642,2.496360987497));
#112595=CARTESIAN_POINT('Ctrl Pts',(6.80802138040703,2.36082111197821,2.4926613077485));
#112596=CARTESIAN_POINT('Ctrl Pts',(6.809373687,2.361474582,2.488961628));
#112597=CARTESIAN_POINT('Ctrl Pts',(6.944754851,2.426894312,2.118581898));
#112598=CARTESIAN_POINT('Ctrl Pts',(7.039164313,2.492218586,1.735703252));
#112599=CARTESIAN_POINT('Ctrl Pts',(7.12228642016887,2.36016764195642,2.35012820286911));
#112600=CARTESIAN_POINT('Ctrl Pts',(7.12355908908444,2.36082111197821,2.34625712793456));
#112601=CARTESIAN_POINT('Ctrl Pts',(7.124831758,2.361474582,2.342386053));
#112602=CARTESIAN_POINT('Ctrl Pts',(7.252240291,2.426894312,1.954847729));
#112603=CARTESIAN_POINT('Ctrl Pts',(7.336863062,2.492218586,1.555776466));
#112604=CARTESIAN_POINT('',(7.12483173727822,2.3614745809634,2.34238604683087));
#112605=CARTESIAN_POINT('',(7.28076015244391,2.45202942683899,1.80014768399621));
#112606=CARTESIAN_POINT('Origin',(-0.185713957054917,2.41071409415622,-0.0527439563721279));
#112607=CARTESIAN_POINT('Ctrl Pts',(7.03803875139302,2.4914407764281,1.74026167702851));
#112608=CARTESIAN_POINT('Ctrl Pts',(7.07842362486222,2.4845452132121,1.75026716357087));
#112609=CARTESIAN_POINT('Ctrl Pts',(7.11886531295691,2.47781843925694,1.76026463046666));
#112610=CARTESIAN_POINT('Ctrl Pts',(7.19975945731228,2.46469207985518,1.78022217257698));
#112611=CARTESIAN_POINT('Ctrl Pts',(7.24025802831338,2.45828501821586,1.79019362197555));
#112612=CARTESIAN_POINT('Ctrl Pts',(7.28076014663648,2.45202942664997,1.80014768467118));
#112613=CARTESIAN_POINT('',(6.96710272593122,2.36147458031212,2.41567383060393));
#112614=CARTESIAN_POINT('Origin',(-6.62230686954146E-13,2.45311202900033,
-3.47595216498853E-13));
#112615=CARTESIAN_POINT('',(7.28237557187738,2.2715957307624,1.79360141123147));
#112616=CARTESIAN_POINT('Ctrl Pts',(7.28237556955524,2.27159573308897,1.79360141962778));
#112617=CARTESIAN_POINT('Ctrl Pts',(7.27518788909083,2.27631121118345,1.82278482206762));
#112618=CARTESIAN_POINT('Ctrl Pts',(7.26782938382074,2.281017555009,1.85190631585837));
#112619=CARTESIAN_POINT('Ctrl Pts',(7.26030153198921,2.28571428600673,1.88096296104166));
#112620=CARTESIAN_POINT('Ctrl Pts',(7.2222964727339,2.30942616856895,2.02765813658417));
#112621=CARTESIAN_POINT('Ctrl Pts',(7.17971132022375,2.33338338402406,2.17370250603423));
#112622=CARTESIAN_POINT('Ctrl Pts',(7.13258426888173,2.35752273144221,2.31867238862267));
#112623=CARTESIAN_POINT('Ctrl Pts',(7.13001359641854,2.35883947742822,2.32658016291681));
#112624=CARTESIAN_POINT('Ctrl Pts',(7.12742942262058,2.36015676440385,2.33448474022867));
#112625=CARTESIAN_POINT('Ctrl Pts',(7.12483175814687,2.36147458179854,2.34238605190836));
#112626=CARTESIAN_POINT('',(7.39619036979387,2.36147458149275,1.243530451497));
#112627=CARTESIAN_POINT('Origin',(-0.189858677544673,2.41070042531505,-0.023897387776198));
#112628=CARTESIAN_POINT('Origin',(-0.178723583569177,2.55351789973106,-0.0609403871456785));
#112629=CARTESIAN_POINT('Ctrl Pts',(7.036900237,2.492226207,1.74485961));
#112630=CARTESIAN_POINT('Ctrl Pts',(7.132338192,2.42647128,1.359964821));
#112631=CARTESIAN_POINT('Ctrl Pts',(7.18522749100001,2.361474582,0.96695703));
#112632=CARTESIAN_POINT('Ctrl Pts',(7.185754070995,2.36082745750497,0.963044139405232));
#112633=CARTESIAN_POINT('Ctrl Pts',(7.18628065099001,2.36018033300993,0.959131248810464));
#112634=CARTESIAN_POINT('Ctrl Pts',(7.21643957,2.492226207,2.042792189));
#112635=CARTESIAN_POINT('Ctrl Pts',(7.328173436,2.42647128,1.648077202));
#112636=CARTESIAN_POINT('Ctrl Pts',(7.396190372,2.361474582,1.24353045));
#112637=CARTESIAN_POINT('Ctrl Pts',(7.39686756679169,2.36082745750497,1.23950267442584));
#112638=CARTESIAN_POINT('Ctrl Pts',(7.39754476158338,2.36018033300993,1.23547489885168));
#112639=CARTESIAN_POINT('',(7.29070893018589,2.36147458056998,1.1052437486685));
#112640=CARTESIAN_POINT('Ctrl Pts',(7.18417675373603,2.36016764195642,0.974764808487868));
#112641=CARTESIAN_POINT('Ctrl Pts',(7.18470212236801,2.36082111197821,0.970860919243934));
#112642=CARTESIAN_POINT('Ctrl Pts',(7.185227491,2.361474582,0.96695703));
#112643=CARTESIAN_POINT('Ctrl Pts',(7.237822825,2.426894312,0.576133623));
#112644=CARTESIAN_POINT('Ctrl Pts',(7.247717455,2.492218586,0.181911224));
#112645=CARTESIAN_POINT('Ctrl Pts',(7.46097941612226,2.36016764195642,0.764102464106214));
#112646=CARTESIAN_POINT('Ctrl Pts',(7.46139016406113,2.36082111197821,0.760048306553106));
#112647=CARTESIAN_POINT('Ctrl Pts',(7.461800912,2.361474582,0.755994149));
#112648=CARTESIAN_POINT('Ctrl Pts',(7.50292142,2.426894312,0.350127187));
#112649=CARTESIAN_POINT('Ctrl Pts',(7.499777232,2.492218586,-0.057805406));
#112650=CARTESIAN_POINT('Ctrl Pts',(7.24759813527961,2.49144077636324,0.186605038200559));
#112651=CARTESIAN_POINT('Ctrl Pts',(7.28918971677884,2.48454521314802,0.187695047633678));
#112652=CARTESIAN_POINT('Ctrl Pts',(7.3308350603499,2.47781843923321,0.188765011539292));
#112653=CARTESIAN_POINT('Ctrl Pts',(7.41412822619493,2.46469207984091,0.190866107168316));
#112654=CARTESIAN_POINT('Ctrl Pts',(7.45582352990115,2.45828501821583,0.191898433840291));
#112655=CARTESIAN_POINT('Ctrl Pts',(7.49751856038283,2.4520294266588,0.192913017772023));
#112656=CARTESIAN_POINT('',(7.32351420272364,2.36147458031212,0.86147557909768));
#112657=CARTESIAN_POINT('Ctrl Pts',(7.247474658,2.492226207,0.191340221));
#112658=CARTESIAN_POINT('Ctrl Pts',(7.257940325,2.42647128,-0.205072282));
#112659=CARTESIAN_POINT('Ctrl Pts',(7.22510804400001,2.361474582,-0.600261405));
#112660=CARTESIAN_POINT('Ctrl Pts',(7.22478115703626,2.36082745750497,-0.604196013519101));
#112661=CARTESIAN_POINT('Ctrl Pts',(7.2244542700725,2.36018033300993,-0.608130622038201));
#112662=CARTESIAN_POINT('Ctrl Pts',(7.48686316,2.492226207,0.443711652));
#112663=CARTESIAN_POINT('Ctrl Pts',(7.511132695,2.42647128,0.034205403));
#112664=CARTESIAN_POINT('Ctrl Pts',(7.49059384,2.361474582,-0.375504901));
#112665=CARTESIAN_POINT('Ctrl Pts',(7.4903893496708,2.36082745750497,-0.379584086277783));
#112666=CARTESIAN_POINT('Ctrl Pts',(7.49018485934162,2.36018033300993,-0.383663271555566));
#112667=CARTESIAN_POINT('',(7.35785094258008,2.36147458056998,-0.487883144251673));
#112668=CARTESIAN_POINT('Ctrl Pts',(7.2257603139574,2.36016764195642,-0.592410290582772));
#112669=CARTESIAN_POINT('Ctrl Pts',(7.2254341789787,2.36082111197821,-0.596335847791386));
#112670=CARTESIAN_POINT('Ctrl Pts',(7.225108044,2.361474582,-0.600261405));
#112671=CARTESIAN_POINT('Ctrl Pts',(7.192458249,2.426894312,-0.99325402));
#112672=CARTESIAN_POINT('Ctrl Pts',(7.117375384,2.492218586,-1.380386771));
#112673=CARTESIAN_POINT('Ctrl Pts',(7.45080530628486,2.36016764195642,-0.8576518564782));
#112674=CARTESIAN_POINT('Ctrl Pts',(7.45033492714243,2.36082111197821,-0.8616995287391));
#112675=CARTESIAN_POINT('Ctrl Pts',(7.449864548,2.361474582,-0.865747201));
#112676=CARTESIAN_POINT('Ctrl Pts',(7.402774283,2.426894312,-1.270964912));
#112677=CARTESIAN_POINT('Ctrl Pts',(7.312010155,2.492218586,-1.668684361));
#112678=CARTESIAN_POINT('',(7.44986452659274,2.3614745809634,-0.86574719785456));
#112679=CARTESIAN_POINT('',(7.36370134498239,2.45202942682888,-1.42334204951334));
#112680=CARTESIAN_POINT('Origin',(-0.190695837988908,2.41071407000259,0.0301101055091291));
#112681=CARTESIAN_POINT('Ctrl Pts',(7.11826788532725,2.49144077642908,-1.37577704600419));
#112682=CARTESIAN_POINT('Ctrl Pts',(7.15912139879897,2.48454521318342,-1.38365348071112));
#112683=CARTESIAN_POINT('Ctrl Pts',(7.20002310802721,2.47781843927426,-1.39156104960372));
#112684=CARTESIAN_POINT('Ctrl Pts',(7.28182059975392,2.46469207984667,-1.40741464471913));
#112685=CARTESIAN_POINT('Ctrl Pts',(7.32276301032829,2.45828501820481,-1.4153697110069));
#112686=CARTESIAN_POINT('Ctrl Pts',(7.36370133986324,2.45202942663467,-1.42334204651203));
#112687=CARTESIAN_POINT('',(7.33748629495884,2.36147458031212,-0.733004313422165));
#112688=CARTESIAN_POINT('Origin',(1.99926880606327E-12,2.45311202899956,
-3.96167473826203E-13));
#112689=CARTESIAN_POINT('',(7.36241875102517,2.27159573074673,-1.42996158277913));
#112690=CARTESIAN_POINT('Ctrl Pts',(7.36241875243634,2.27159573307529,-1.42996157417025));
#112691=CARTESIAN_POINT('Ctrl Pts',(7.36814918304015,2.27631121117315,-1.40045740682588));
#112692=CARTESIAN_POINT('Ctrl Pts',(7.37369858250963,2.28101755500325,-1.37093769877651));
#112693=CARTESIAN_POINT('Ctrl Pts',(7.37906705789564,2.2857142859868,-1.34140573896273));
#112694=CARTESIAN_POINT('Ctrl Pts',(7.4061702772824,2.30942614453486,-1.19231104347212));
#112695=CARTESIAN_POINT('Ctrl Pts',(7.42884346071946,2.33338333568924,-1.04188387518592));
#112696=CARTESIAN_POINT('Ctrl Pts',(7.44694337228644,2.35752265840788,-0.890524792629102));
#112697=CARTESIAN_POINT('Ctrl Pts',(7.44793070016065,2.35883942871897,-0.882268341172374));
#112698=CARTESIAN_POINT('Ctrl Pts',(7.44890443167442,2.36015674003959,-0.87400912205204));
#112699=CARTESIAN_POINT('Ctrl Pts',(7.44986454767493,2.36147458179854,-0.865747202052421));
#112700=CARTESIAN_POINT('',(7.23474546263687,2.36147458149274,-1.97698205770052));
#112701=CARTESIAN_POINT('Origin',(-0.182345328122927,2.41070047910294,0.0580309238822652));
#112702=CARTESIAN_POINT('Origin',(-0.187793153545018,2.55351788034799,0.019736059035676));
#112703=CARTESIAN_POINT('Ctrl Pts',(7.11916522,2.492226207,-1.371126025));
#112704=CARTESIAN_POINT('Ctrl Pts',(7.044169235,2.42647128,-1.760520432));
#112705=CARTESIAN_POINT('Ctrl Pts',(6.927150574,2.361474582,-2.139412284));
#112706=CARTESIAN_POINT('Ctrl Pts',(6.92598550493897,2.36082745750497,-2.14318463253374));
#112707=CARTESIAN_POINT('Ctrl Pts',(6.92482043587793,2.36018033300993,-2.14695698106747));
#112708=CARTESIAN_POINT('Ctrl Pts',(7.407209349,2.492226207,-1.176116349));
#112709=CARTESIAN_POINT('Ctrl Pts',(7.34287973799999,2.42647128,-1.581265802));
#112710=CARTESIAN_POINT('Ctrl Pts',(7.234745464,2.361474582,-1.97698206));
#112711=CARTESIAN_POINT('Ctrl Pts',(7.23366885027021,2.36082745750497,-1.98092191681603));
#112712=CARTESIAN_POINT('Ctrl Pts',(7.23259223654041,2.36018033300993,-1.98486177363207));
#112713=CARTESIAN_POINT('',(7.08094802144715,2.36147458056998,-2.05819716358091));
#112714=CARTESIAN_POINT('Ctrl Pts',(6.92947535176304,2.36016764195642,-2.1318849430597));
#112715=CARTESIAN_POINT('Ctrl Pts',(6.92831296288152,2.36082111197821,-2.13564861352985));
#112716=CARTESIAN_POINT('Ctrl Pts',(6.92715057400001,2.361474582,-2.139412284));
#112717=CARTESIAN_POINT('Ctrl Pts',(6.810782318,2.426894312,-2.516198208));
#112718=CARTESIAN_POINT('Ctrl Pts',(6.654232751,2.492218586,-2.878139415));
#112719=CARTESIAN_POINT('Ctrl Pts',(7.0922398216647,2.36016764195642,-2.43930332935916));
#112720=CARTESIAN_POINT('Ctrl Pts',(7.09091030983235,2.36082111197821,-2.44315525167958));
#112721=CARTESIAN_POINT('Ctrl Pts',(7.089580798,2.361474582,-2.447007174));
#112722=CARTESIAN_POINT('Ctrl Pts',(6.956481647,2.426894312,-2.832628105));
#112723=CARTESIAN_POINT('Ctrl Pts',(6.782341609,2.492218586,-3.201537489));
#112724=CARTESIAN_POINT('',(7.08958077776817,2.36147458096341,-2.44700716636999));
#112725=CARTESIAN_POINT('',(6.88556563225692,2.45202942686305,-2.97304322297742));
#112726=CARTESIAN_POINT('Origin',(-0.179764760123894,2.41071407563139,0.0704001507666559));
#112727=CARTESIAN_POINT('Ctrl Pts',(6.65609534086865,2.49144077640618,-2.87382932423452));
#112728=CARTESIAN_POINT('Ctrl Pts',(6.69430052125234,2.48454521316161,-2.89030390998572));
#112729=CARTESIAN_POINT('Ctrl Pts',(6.73254607754049,2.47781843927154,-2.90681926266846));
#112730=CARTESIAN_POINT('Ctrl Pts',(6.80902313486423,2.46469207986071,-2.9398862522766));
#112731=CARTESIAN_POINT('Ctrl Pts',(6.84729823036649,2.45828501823745,-2.95645674151964));
#112732=CARTESIAN_POINT('Ctrl Pts',(6.88556562787249,2.45202942668653,-2.97304321894631));
#112733=CARTESIAN_POINT('',(7.00836568274272,2.36147458031212,-2.29320973895468));
#112734=CARTESIAN_POINT('Origin',(-9.76215636105948E-13,2.45311202899922,
4.39969241594618E-13));
#112735=CARTESIAN_POINT('',(6.88289002122442,2.27159573079936,-2.97923227567974));
#112736=CARTESIAN_POINT('Ctrl Pts',(6.88289002437727,2.27159573313914,-2.97923226743001));
#112737=CARTESIAN_POINT('Ctrl Pts',(6.8948290042822,2.27631121120396,-2.95164976425878));
#112738=CARTESIAN_POINT('Ctrl Pts',(6.90659452628485,2.28101755501304,-2.92401316740996));
#112739=CARTESIAN_POINT('Ctrl Pts',(6.91818598809468,2.28571428603837,-2.89632571177384));
#112740=CARTESIAN_POINT('Ctrl Pts',(6.97670677214404,2.30942625373646,-2.75654251561478));
#112741=CARTESIAN_POINT('Ctrl Pts',(7.03118749456151,2.3333835557567,-2.61450565346097));
#112742=CARTESIAN_POINT('Ctrl Pts',(7.08140215982957,2.35752299096738,-2.47057552999628));
#112743=CARTESIAN_POINT('Ctrl Pts',(7.08414106477529,2.35883965051559,-2.46272501610972));
#112744=CARTESIAN_POINT('Ctrl Pts',(7.08686728833517,2.36015685098211,-2.45486887740036));
#112745=CARTESIAN_POINT('Ctrl Pts',(7.08958079745629,2.36147458179854,-2.44700717495794));
#112746=CARTESIAN_POINT('',(6.64060843113895,2.36147458149276,-3.48601773348323));
#112747=CARTESIAN_POINT('Origin',(-0.165607402435284,2.41070043976848,0.0958731050958894));
#112748=CARTESIAN_POINT('Origin',(-0.179160224013873,2.55351789408286,0.0596447154192725));
#112749=CARTESIAN_POINT('Ctrl Pts',(6.657971528,2.492226207,-2.869479942));
#112750=CARTESIAN_POINT('Ctrl Pts',(6.50102062,2.42647128,-3.233648604));
#112751=CARTESIAN_POINT('Ctrl Pts',(6.30528724300001,2.361474582,-3.578526622));
#112752=CARTESIAN_POINT('Ctrl Pts',(6.30333846919071,2.36082745750497,-3.58196031971256));
#112753=CARTESIAN_POINT('Ctrl Pts',(6.30138969538143,2.36018033300993,-3.58539401742512));
#112754=CARTESIAN_POINT('Ctrl Pts',(6.981202661,2.492226207,-2.740950457));
#112755=CARTESIAN_POINT('Ctrl Pts',(6.831281884,2.42647128,-3.122798776));
#112756=CARTESIAN_POINT('Ctrl Pts',(6.640608432,2.361474582,-3.486017736));
#112757=CARTESIAN_POINT('Ctrl Pts',(6.63871003615623,2.36082745750497,-3.48963404103255));
#112758=CARTESIAN_POINT('Ctrl Pts',(6.63681164031246,2.36018033300993,-3.4932503460651));
#112759=CARTESIAN_POINT('',(6.4729478416998,2.36147458056998,-3.5322721713038));
#112760=CARTESIAN_POINT('Ctrl Pts',(6.30917582457058,2.36016764195642,-3.57167502459223));
#112761=CARTESIAN_POINT('Ctrl Pts',(6.30723153378529,2.36082111197821,-3.57510082329612));
#112762=CARTESIAN_POINT('Ctrl Pts',(6.305287243,2.361474582,-3.578526622));
#112763=CARTESIAN_POINT('Ctrl Pts',(6.110641775,2.426894312,-3.921487766));
#112764=CARTESIAN_POINT('Ctrl Pts',(5.87994559000001,2.492218586,-4.241313459));
#112765=CARTESIAN_POINT('Ctrl Pts',(6.40204908504071,2.36016764195642,-3.90689568945038));
#112766=CARTESIAN_POINT('Ctrl Pts',(6.39992260702036,2.36082111197821,-3.91037175022519));
#112767=CARTESIAN_POINT('Ctrl Pts',(6.397796129,2.361474582,-3.913847811));
#112768=CARTESIAN_POINT('Ctrl Pts',(6.184911661,2.426894312,-4.261840756));
#112769=CARTESIAN_POINT('Ctrl Pts',(5.93553830800001,2.492218586,-4.584690283));
#112770=CARTESIAN_POINT('',(6.39779611089142,2.36147458096338,-3.913847799171));
#112771=CARTESIAN_POINT('',(6.08546852367397,2.45202942687596,-4.38372819973879));
#112772=CARTESIAN_POINT('Origin',(-0.160428043470981,2.41071407866953,0.107398362108932));
#112773=CARTESIAN_POINT('Ctrl Pts',(5.88269117573753,2.49144077634923,-4.23750453653325));
#112774=CARTESIAN_POINT('Ctrl Pts',(5.91646159105472,2.48454521315402,-4.26180694017867));
#112775=CARTESIAN_POINT('Ctrl Pts',(5.95026267507658,2.47781843922848,-4.28615783750334));
#112776=CARTESIAN_POINT('Ctrl Pts',(6.01784331582932,2.46469207986924,-4.33489204607862));
#112777=CARTESIAN_POINT('Ctrl Pts',(6.05166139552129,2.45828501825422,-4.35930314069997));
#112778=CARTESIAN_POINT('Ctrl Pts',(6.08546852022469,2.4520294267061,-4.38372819485558));
#112779=CARTESIAN_POINT('',(6.35154168067892,2.36147458031212,-3.74618722552173));
#112780=CARTESIAN_POINT('Origin',(1.95156391047391E-14,2.45311202900011,
-1.23599047663348E-13));
#112781=CARTESIAN_POINT('',(6.08152500337026,2.27159573077931,-4.38919737833573));
#112782=CARTESIAN_POINT('Ctrl Pts',(6.08152500825334,2.27159573310914,-4.38919737108322));
#112783=CARTESIAN_POINT('Ctrl Pts',(6.09911428445537,2.27631121119346,-4.36482625939919));
#112784=CARTESIAN_POINT('Ctrl Pts',(6.11654578662252,2.28101755501234,-4.3403650303756));
#112785=CARTESIAN_POINT('Ctrl Pts',(6.13381823102573,2.28571428600965,-4.31581671390275));
#112786=CARTESIAN_POINT('Ctrl Pts',(6.22101983715752,2.30942618592822,-4.19188216373346));
#112787=CARTESIAN_POINT('Ctrl Pts',(6.30476032883193,2.33338341906849,-4.06487815968526));
#112788=CARTESIAN_POINT('Ctrl Pts',(6.38474151856246,2.35752278440514,-3.93510809695038));
#112789=CARTESIAN_POINT('Ctrl Pts',(6.38910424716817,2.3588395127513,-3.92802953801965));
#112790=CARTESIAN_POINT('Ctrl Pts',(6.39345579887504,2.36015678207248,-3.92094275878753));
#112791=CARTESIAN_POINT('Ctrl Pts',(6.39779612826307,2.36147458179854,-3.91384781181866));
#112792=CARTESIAN_POINT('',(5.73596392970765,2.36147458149275,-4.83205109335265));
#112793=CARTESIAN_POINT('Origin',(-0.141125708619402,2.4107004559566,0.129232339767804));
#112794=CARTESIAN_POINT('Origin',(-0.162149707107304,2.5535178731589,0.0967644146262725));
#112795=CARTESIAN_POINT('Ctrl Pts',(5.885458487,2.492226207,-4.233660165));
#112796=CARTESIAN_POINT('Ctrl Pts',(5.653891507,2.42647128,-4.555574961));
#112797=CARTESIAN_POINT('Ctrl Pts',(5.388595688,2.361474582,-4.850313032));
#112798=CARTESIAN_POINT('Ctrl Pts',(5.38595433192827,2.36082745750497,-4.8532475230008));
#112799=CARTESIAN_POINT('Ctrl Pts',(5.38331297585654,2.36018033300993,-4.85618201400161));
#112800=CARTESIAN_POINT('Ctrl Pts',(6.228762696,2.492226207,-4.177620768));
#112801=CARTESIAN_POINT('Ctrl Pts',(6.000260882,2.42647128,-4.51831315));
#112802=CARTESIAN_POINT('Ctrl Pts',(5.73596393,2.361474582,-4.832051096));
#112803=CARTESIAN_POINT('Ctrl Pts',(5.73333251891506,2.36082745750497,-4.83517475483384));
#112804=CARTESIAN_POINT('Ctrl Pts',(5.73070110783012,2.36018033300993,-4.83829841366768));
#112805=CARTESIAN_POINT('',(5.56227981475606,2.36147458056998,-4.84118205738657));
#112806=CARTESIAN_POINT('Ctrl Pts',(5.39386624760077,2.36016764195642,-4.84445755122613));
#112807=CARTESIAN_POINT('Ctrl Pts',(5.39123096780039,2.36082111197821,-4.84738529161306));
#112808=CARTESIAN_POINT('Ctrl Pts',(5.38859568799999,2.361474582,-4.850313032));
#112809=CARTESIAN_POINT('Ctrl Pts',(5.124774415,2.426894312,-5.143412913));
#112810=CARTESIAN_POINT('Ctrl Pts',(4.830718708,2.492218586,-5.40616839900001));
#112811=CARTESIAN_POINT('Ctrl Pts',(5.41250564892147,2.36016764195642,-5.19180595003168));
#112812=CARTESIAN_POINT('Ctrl Pts',(5.40968163646073,2.36082111197821,-5.19474361251584));
#112813=CARTESIAN_POINT('Ctrl Pts',(5.406857624,2.361474582,-5.197681275));
#112814=CARTESIAN_POINT('Ctrl Pts',(5.12414208000001,2.426894312,-5.49177447));
#112815=CARTESIAN_POINT('Ctrl Pts',(4.811195832,2.492218586,-5.75346805500001));
#112816=CARTESIAN_POINT('',(5.40685760886689,2.36147458096338,-5.19768125953299));
#112817=CARTESIAN_POINT('',(5.00082167051335,2.4520294268514,-5.58943491793815));
#112818=CARTESIAN_POINT('Origin',(-0.133589863414661,2.41071407407032,0.139374754044277));
#112819=CARTESIAN_POINT('Ctrl Pts',(4.83421890979896,2.49144077619964,-5.40303874779536));
#112820=CARTESIAN_POINT('Ctrl Pts',(4.86197549339698,2.48454521296006,-5.43403261592637));
#112821=CARTESIAN_POINT('Ctrl Pts',(4.88975160320432,2.47781843917396,-5.46508043601207));
#112822=CARTESIAN_POINT('Ctrl Pts',(4.94527583200974,2.46469207979229,-5.52720310597014));
#112823=CARTESIAN_POINT('Ctrl Pts',(4.97305559996261,2.45828501819729,-5.5583133701044));
#112824=CARTESIAN_POINT('Ctrl Pts',(5.00082166815137,2.45202942666902,-5.58943491241765));
#112825=CARTESIAN_POINT('',(5.39772664886391,2.36147458031212,-5.02399716116693));
#112826=CARTESIAN_POINT('Origin',(3.0140820395097E-13,2.45311202899956,
-4.33680868994202E-13));
#112827=CARTESIAN_POINT('',(4.99579463605586,2.2715957307672,-5.59392849012071));
#112828=CARTESIAN_POINT('Ctrl Pts',(4.99579464238751,2.27159573309948,-5.5939284840713));
#112829=CARTESIAN_POINT('Ctrl Pts',(5.01821175973075,2.27631121118552,-5.57390832984172));
#112830=CARTESIAN_POINT('Ctrl Pts',(5.04049416430141,2.28101755500763,-5.55376624842468));
#112831=CARTESIAN_POINT('Ctrl Pts',(5.06263995095078,2.28571428598914,-5.53350492287605));
#112832=CARTESIAN_POINT('Ctrl Pts',(5.17444495087571,2.30942615500799,-5.43121379376971));
#112833=CARTESIAN_POINT('Ctrl Pts',(5.28352960527545,2.33338335682526,-5.32518094602194));
#112834=CARTESIAN_POINT('Ctrl Pts',(5.38953747703969,2.35752269035039,-5.21563857865579));
#112835=CARTESIAN_POINT('Ctrl Pts',(5.39532002651813,2.35883945002269,-5.20966322844134));
#112836=CARTESIAN_POINT('Ctrl Pts',(5.40109342709373,2.36015675069572,-5.20367744691155));
#112837=CARTESIAN_POINT('Ctrl Pts',(5.40685762310432,2.36147458179854,-5.1976812756411));
#112838=CARTESIAN_POINT('',(4.56311212928963,2.36147458149275,-5.95214311534979));
#112839=CARTESIAN_POINT('Origin',(-0.110044981492499,2.41070042225928,0.156548632073102));
#112840=CARTESIAN_POINT('Origin',(-0.137556999251891,2.55351788794162,0.129359209222423));
#112841=CARTESIAN_POINT('Ctrl Pts',(4.837747949,2.492226207,-5.399879145));
#112842=CARTESIAN_POINT('Ctrl Pts',(4.542392711,2.42647128,-5.664487697));
#112843=CARTESIAN_POINT('Ctrl Pts',(4.219939387,2.361474582,-5.895304196));
#112844=CARTESIAN_POINT('Ctrl Pts',(4.21672895553369,2.36082745750497,-5.89760226674754));
#112845=CARTESIAN_POINT('Ctrl Pts',(4.21351852406738,2.36018033300993,-5.89990033749508));
#112846=CARTESIAN_POINT('Ctrl Pts',(5.18507271,2.492226207,-5.418950174));
#112847=CARTESIAN_POINT('Ctrl Pts',(4.888674351,2.42647128,-5.702556223));
#112848=CARTESIAN_POINT('Ctrl Pts',(4.563112129,2.361474582,-5.952143118));
#112849=CARTESIAN_POINT('Ctrl Pts',(4.55987074451438,2.36082745750497,-5.95462807182634));
#112850=CARTESIAN_POINT('Ctrl Pts',(4.55662936002876,2.36018033300993,-5.95711302565267));
#112851=CARTESIAN_POINT('',(4.39152576504318,2.36147458056998,-5.92372365177857));
#112852=CARTESIAN_POINT('Ctrl Pts',(4.22634547911204,2.36016764195642,-5.89071862761956));
#112853=CARTESIAN_POINT('Ctrl Pts',(4.22314243305602,2.36082111197821,-5.89301141180978));
#112854=CARTESIAN_POINT('Ctrl Pts',(4.219939387,2.361474582,-5.895304196));
#112855=CARTESIAN_POINT('Ctrl Pts',(3.899278299,2.426894312,-6.12483779));
#112856=CARTESIAN_POINT('Ctrl Pts',(3.555612789,2.492218586,-6.318236914));
#112857=CARTESIAN_POINT('Ctrl Pts',(4.16987946444665,2.36016764195642,-6.23395313325984));
#112858=CARTESIAN_POINT('Ctrl Pts',(4.16648996522332,2.36082111197821,-6.23621503562992));
#112859=CARTESIAN_POINT('Ctrl Pts',(4.163100466,2.361474582,-6.238476938));
#112860=CARTESIAN_POINT('Ctrl Pts',(3.82377331,2.426894312,-6.46491891300001));
#112861=CARTESIAN_POINT('Ctrl Pts',(3.461887187,2.492218586,-6.653220055));
#112862=CARTESIAN_POINT('',(4.16310045450136,2.36147458096341,-6.23847691969746));
#112863=CARTESIAN_POINT('',(3.68234195387786,2.45202942688314,-6.53378587147896));
#112864=CARTESIAN_POINT('Origin',(-0.100505229271112,2.41071409629437,0.164834243166782));
#112865=CARTESIAN_POINT('Ctrl Pts',(3.55970394000875,2.49144077637471,-6.31593287126581));
#112866=CARTESIAN_POINT('Ctrl Pts',(3.58014882443327,2.48454521317143,-6.35216896470848));
#112867=CARTESIAN_POINT('Ctrl Pts',(3.60060118099897,2.47781843924586,-6.38846194721864));
#112868=CARTESIAN_POINT('Ctrl Pts',(3.64147274625851,2.46469207987447,-6.46106829132436));
#112869=CARTESIAN_POINT('Ctrl Pts',(3.66191525146325,2.45828501826216,-6.49742304371203));
#112870=CARTESIAN_POINT('Ctrl Pts',(3.68234195274149,2.4520294267171,-6.5337858655678));
#112871=CARTESIAN_POINT('',(4.19151991788259,2.36147458031212,-6.06689057295364));
#112872=CARTESIAN_POINT('Origin',(-3.29163779566599E-13,2.453112029,5.62917767954474E-13));
#112873=CARTESIAN_POINT('',(3.6764664637425,2.27159573079627,-6.53709372270527));
#112874=CARTESIAN_POINT('Ctrl Pts',(3.67646647129025,2.27159573315182,-6.53709371793003));
#112875=CARTESIAN_POINT('Ctrl Pts',(3.70266323014006,2.27631121120201,-6.52236064107112));
#112876=CARTESIAN_POINT('Ctrl Pts',(3.72875463649749,2.28101755500699,-6.50747952845856));
#112877=CARTESIAN_POINT('Ctrl Pts',(3.75473825304687,2.28571428600847,-6.4924525909729));
#112878=CARTESIAN_POINT('Ctrl Pts',(3.88591898369805,2.30942617320938,-6.41658768496772));
#112879=CARTESIAN_POINT('Ctrl Pts',(4.01524732444754,2.33338339338091,-6.33648373760001));
#112880=CARTESIAN_POINT('Ctrl Pts',(4.14232525569792,2.35752274558242,-6.25229089772399));
#112881=CARTESIAN_POINT('Ctrl Pts',(4.14925703895402,2.35883948685887,-6.24769838892255));
#112882=CARTESIAN_POINT('Ctrl Pts',(4.15618212981563,2.36015676912106,-6.24309372628041));
#112883=CARTESIAN_POINT('Ctrl Pts',(4.16310046498744,2.36147458179854,-6.23847693843357));
#112884=CARTESIAN_POINT('',(3.1768942778333,2.36147458149276,-6.79391954047577));
#112885=CARTESIAN_POINT('Origin',(-0.0738188840871684,2.41070043582995,
0.176545072828828));
#112886=CARTESIAN_POINT('Origin',(-0.106532826126692,2.5535179002561,0.155905997732412));
#112887=CARTESIAN_POINT('Ctrl Pts',(3.563829693,2.492226207,-6.313605778));
#112888=CARTESIAN_POINT('Ctrl Pts',(3.21849668,2.42647128,-6.508535283));
#112889=CARTESIAN_POINT('Ctrl Pts',(2.853963411,2.361474582,-6.664637488));
#112890=CARTESIAN_POINT('Ctrl Pts',(2.85033402035581,2.36082745750497,-6.66619168326981));
#112891=CARTESIAN_POINT('Ctrl Pts',(2.84670462971162,2.36018033300993,-6.6677458785396));
#112892=CARTESIAN_POINT('Ctrl Pts',(3.898934487,2.492226207,-6.406895494));
#112893=CARTESIAN_POINT('Ctrl Pts',(3.548498839,2.42647128,-6.620154104));
#112894=CARTESIAN_POINT('Ctrl Pts',(3.176894277,2.361474582,-6.79391954300001));
#112895=CARTESIAN_POINT('Ctrl Pts',(3.17319448267296,2.36082745750497,-6.79564959814783));
#112896=CARTESIAN_POINT('Ctrl Pts',(3.16949468834593,2.36018033300993,-6.79737965329567));
#112897=CARTESIAN_POINT('',(3.01542885200097,2.36147458056998,-6.72927851191472));
#112898=CARTESIAN_POINT('Ctrl Pts',(2.86120549389769,2.36016764195642,-6.66153624811899));
#112899=CARTESIAN_POINT('Ctrl Pts',(2.85758445244885,2.36082111197821,-6.66308686805949));
#112900=CARTESIAN_POINT('Ctrl Pts',(2.853963411,2.361474582,-6.664637488));
#112901=CARTESIAN_POINT('Ctrl Pts',(2.491456263,2.426894312,-6.819872058));
#112902=CARTESIAN_POINT('Ctrl Pts',(2.114250367,2.492218586,-6.934871692));
#112903=CARTESIAN_POINT('Ctrl Pts',(2.7322743505124,2.36016764195642,-6.98460759756821));
#112904=CARTESIAN_POINT('Ctrl Pts',(2.7284778537562,2.36082111197821,-6.9860879757841));
#112905=CARTESIAN_POINT('Ctrl Pts',(2.724681357,2.361474582,-6.98756835400001));
#112906=CARTESIAN_POINT('Ctrl Pts',(2.344609151,2.426894312,-7.13577093400001));
#112907=CARTESIAN_POINT('Ctrl Pts',(1.950704544,2.492218586,-7.24187488));
#112908=CARTESIAN_POINT('',(2.72468134975038,2.36147458096339,-6.98756833361612));
#112909=CARTESIAN_POINT('',(2.19168002063031,2.45202942684316,-7.1726242596834));
#112910=CARTESIAN_POINT('Origin',(-0.0627208430799763,2.4107140698826,0.182585748484438));
#112911=CARTESIAN_POINT('Ctrl Pts',(2.11874117040428,2.49144077629052,-6.93350099351369));
#112912=CARTESIAN_POINT('Ctrl Pts',(2.13091837590245,2.48454521305579,-6.97328495320926));
#112913=CARTESIAN_POINT('Ctrl Pts',(2.14309064927467,2.47781843918746,-7.01312607778268));
#112914=CARTESIAN_POINT('Ctrl Pts',(2.16739844250754,2.46469207980608,-7.09282110454116));
#112915=CARTESIAN_POINT('Ctrl Pts',(2.17954781629908,2.45828501819535,-7.13272043748061));
#112916=CARTESIAN_POINT('Ctrl Pts',(2.19168002095519,2.45202942665626,-7.17262425381494));
#112917=CARTESIAN_POINT('',(2.78932237430421,2.36147458031212,-6.82610292496196));
#112918=CARTESIAN_POINT('Origin',(-3.60605642568679E-13,2.45311202900022,
9.36750677027476E-13));
#112919=CARTESIAN_POINT('',(2.18523080563448,2.27159573074892,-7.1745917181958));
#112920=CARTESIAN_POINT('Ctrl Pts',(2.1852308139442,2.27159573308574,-7.17459171531735));
#112921=CARTESIAN_POINT('Ctrl Pts',(2.2139822832731,2.27631121117266,-7.16583461865168));
#112922=CARTESIAN_POINT('Ctrl Pts',(2.24266268651128,2.28101755499938,-7.15691029945946));
#112923=CARTESIAN_POINT('Ctrl Pts',(2.2712691678847,2.28571428597161,-7.14782039293411));
#112924=CARTESIAN_POINT('Ctrl Pts',(2.41569123321526,2.30942610013226,-7.10192928621603));
#112925=CARTESIAN_POINT('Ctrl Pts',(2.55921549262729,2.33338324614021,-7.05150006404015));
#112926=CARTESIAN_POINT('Ctrl Pts',(2.70142095576105,2.35752252307876,-6.99659380100814));
#112927=CARTESIAN_POINT('Ctrl Pts',(2.7091783687944,2.35883933846272,-6.99359862381121));
#112928=CARTESIAN_POINT('Ctrl Pts',(2.71693185817446,2.36015669489342,-6.99059013675634));
#112929=CARTESIAN_POINT('Ctrl Pts',(2.72468135591791,2.36147458179854,-6.98756835420575));
#112930=CARTESIAN_POINT('',(1.64212838139087,2.36147458149274,-7.31801983771833));
#112931=CARTESIAN_POINT('Origin',(-0.0341410904291883,2.41070048836924,
0.188286562001653));
#112932=CARTESIAN_POINT('Origin',(-0.0705268457592495,2.55351783676061,
0.175162031699275));
#112933=CARTESIAN_POINT('Ctrl Pts',(2.123270722,2.492226207,-6.932115221));
#112934=CARTESIAN_POINT('Ctrl Pts',(1.744107321,2.42647128,-7.048250993));
#112935=CARTESIAN_POINT('Ctrl Pts',(1.354539278,2.361474582,-7.12233973800001));
#112936=CARTESIAN_POINT('Ctrl Pts',(1.35066063445556,2.36082745750497,-7.12307738534472));
#112937=CARTESIAN_POINT('Ctrl Pts',(1.34678199091112,2.36018033300993,-7.12381503268945));
#112938=CARTESIAN_POINT('Ctrl Pts',(2.430486421,2.492226207,-7.0952615));
#112939=CARTESIAN_POINT('Ctrl Pts',(2.042399466,2.42647128,-7.228200938));
#112940=CARTESIAN_POINT('Ctrl Pts',(1.64212838,2.361474582,-7.31801984));
#112941=CARTESIAN_POINT('Ctrl Pts',(1.63814317409917,2.36082745750497,-7.31891410099156));
#112942=CARTESIAN_POINT('Ctrl Pts',(1.63415796819833,2.36018033300993,-7.31980836198311));
#112943=CARTESIAN_POINT('',(1.49833383758464,2.36147458056998,-7.22017978721851));
#112944=CARTESIAN_POINT('Ctrl Pts',(1.36227871992292,2.36016764195642,-7.12086783712926));
#112945=CARTESIAN_POINT('Ctrl Pts',(1.35840899896146,2.36082111197821,-7.12160378756463));
#112946=CARTESIAN_POINT('Ctrl Pts',(1.354539278,2.361474582,-7.122339738));
#112947=CARTESIAN_POINT('Ctrl Pts',(0.967136502,2.426894312,-7.19601668900001));
#112948=CARTESIAN_POINT('Ctrl Pts',(0.574027948,2.492218586,-7.227239578));
#112949=CARTESIAN_POINT('Ctrl Pts',(1.16691112465914,2.36016764195642,-7.40866957357816));
#112950=CARTESIAN_POINT('Ctrl Pts',(1.16288515032957,2.36082111197821,-7.40929920678909));
#112951=CARTESIAN_POINT('Ctrl Pts',(1.158859176,2.361474582,-7.40992884));
#112952=CARTESIAN_POINT('Ctrl Pts',(0.755813673,2.426894312,-7.472962236));
#112953=CARTESIAN_POINT('Ctrl Pts',(0.348309125,2.492218586,-7.491907685));
#112954=CARTESIAN_POINT('',(1.15885917331566,2.36147458096338,-7.40992881852834));
#112955=CARTESIAN_POINT('',(0.598537565187556,2.45202942683418,-7.47607870941393));
#112956=CARTESIAN_POINT('Origin',(-0.0220039527230042,2.41071407041494,
0.191800369024843));
#112957=CARTESIAN_POINT('Ctrl Pts',(0.578708418762666,2.49144077643974,
-7.226866314466));
#112958=CARTESIAN_POINT('Ctrl Pts',(0.582048552589304,2.48454521326316,
-7.26833788628168));
#112959=CARTESIAN_POINT('Ctrl Pts',(0.58537158092354,2.47781843925376,-7.30986422738255));
#112960=CARTESIAN_POINT('Ctrl Pts',(0.591978996387378,2.4646920798733,-7.39292148573499));
#112961=CARTESIAN_POINT('Ctrl Pts',(0.595267147371582,2.45828501822336,
-7.43449975091216));
#112962=CARTESIAN_POINT('Ctrl Pts',(0.598537566821972,2.45202942664249,
-7.47607870383028));
#112963=CARTESIAN_POINT('',(1.25669921667918,2.36147458031212,-7.26613429078502));
#112964=CARTESIAN_POINT('Origin',(-1.70999011391698E-14,2.45311202899944,
3.44342609981396E-13));
#112965=CARTESIAN_POINT('',(0.591816183403944,2.27159573078526,-7.47661377876439));
#112966=CARTESIAN_POINT('Ctrl Pts',(0.591816192120807,2.27159573311852,
-7.47661377775117));
#112967=CARTESIAN_POINT('Ctrl Pts',(0.621777984919688,2.2763112111963,-7.47424213319847));
#112968=CARTESIAN_POINT('Ctrl Pts',(0.65170632102208,2.28101755501207,-7.47169189856643));
#112969=CARTESIAN_POINT('Ctrl Pts',(0.681598059968947,2.28571428597833,
-7.46896405687537));
#112970=CARTESIAN_POINT('Ctrl Pts',(0.832509017219529,2.30942612645993,
-7.45519231806404));
#112971=CARTESIAN_POINT('Ctrl Pts',(0.983518718670204,2.33338329926306,
-7.43679555110876));
#112972=CARTESIAN_POINT('Ctrl Pts',(1.13420288686114,2.35752260336165,-7.4137429016284));
#112973=CARTESIAN_POINT('Ctrl Pts',(1.1424226433557,2.35883939200654,-7.41248538952506));
#112974=CARTESIAN_POINT('Ctrl Pts',(1.15064142919396,2.36015672167605,-7.41121403583437));
#112975=CARTESIAN_POINT('Ctrl Pts',(1.15885917489897,2.36147458179854,-7.40992883996832));
#112976=CARTESIAN_POINT('',(0.0305783858254816,2.36147458149275,-7.49993766206233));
#112977=CARTESIAN_POINT('Origin',(0.00713314255944587,2.41070046639263,
0.191223796676153));
#112978=CARTESIAN_POINT('Origin',(-0.0312233225700945,2.55351786385627,
0.186228177215475));
#112979=CARTESIAN_POINT('Ctrl Pts',(0.583429972,2.492226207,-7.226486661));
#112980=CARTESIAN_POINT('Ctrl Pts',(0.188165442,2.42647128,-7.25839832));
#112981=CARTESIAN_POINT('Ctrl Pts',(-0.208221606,2.361474582,-7.247009298));
#112982=CARTESIAN_POINT('Ctrl Pts',(-0.212168141380535,2.36082745750497,
-7.24689590585336));
#112983=CARTESIAN_POINT('Ctrl Pts',(-0.216114676761069,2.36018033300993,
-7.24678251370672));
#112984=CARTESIAN_POINT('Ctrl Pts',(0.848391511,2.492226207,-7.451860965));
#112985=CARTESIAN_POINT('Ctrl Pts',(0.440799764,2.42647128,-7.498265129));
#112986=CARTESIAN_POINT('Ctrl Pts',(0.030578384,2.361474582,-7.499937664));
#112987=CARTESIAN_POINT('Ctrl Pts',(0.0264941103129808,2.36082745750497,
-7.49995431620543));
#112988=CARTESIAN_POINT('Ctrl Pts',(0.0224098366259617,2.36018033300993,
-7.49997096841086));
#112989=CARTESIAN_POINT('',(-0.0888216022330978,2.36147458056998,-7.37347348110561));
#112990=CARTESIAN_POINT('Ctrl Pts',(-0.200346692749638,2.36016764195642,
-7.24723556060147));
#112991=CARTESIAN_POINT('Ctrl Pts',(-0.204284149374819,2.36082111197821,
-7.24712242930074));
#112992=CARTESIAN_POINT('Ctrl Pts',(-0.208221606,2.361474582,-7.247009298));
#112993=CARTESIAN_POINT('Ctrl Pts',(-0.602405487,2.426894312,-7.235683577));
#112994=CARTESIAN_POINT('Ctrl Pts',(-0.99303538,2.492218586,-7.181669773));
#112995=CARTESIAN_POINT('Ctrl Pts',(-0.453015568348983,2.36016764195642,
-7.48631039345565));
#112996=CARTESIAN_POINT('Ctrl Pts',(-0.457082770174491,2.36082111197821,
-7.48605984072782));
#112997=CARTESIAN_POINT('Ctrl Pts',(-0.461149972,2.361474582,-7.485809288));
#112998=CARTESIAN_POINT('Ctrl Pts',(-0.868322813,2.426894312,-7.46072613));
#112999=CARTESIAN_POINT('Ctrl Pts',(-1.270372842,2.492218586,-7.391627212));
#113000=CARTESIAN_POINT('',(-0.461149970041696,2.36147458096337,-7.48580926646544));
#113001=CARTESIAN_POINT('',(-1.02259184184624,2.45202942681409,-7.42996002746998));
#113002=CARTESIAN_POINT('Origin',(0.0197418695140492,2.41071412747366,0.192046098608932));
#113003=CARTESIAN_POINT('Ctrl Pts',(-0.988384096490083,2.49144077631088,
-7.18231140053096));
#113004=CARTESIAN_POINT('Ctrl Pts',(-0.994037214993464,2.484545213046,-7.22353142046831));
#113005=CARTESIAN_POINT('Ctrl Pts',(-0.999718812712841,2.47781843921912,
-7.26480125044355));
#113006=CARTESIAN_POINT('Ctrl Pts',(-1.01112073014719,2.4646920797927,-7.34733707540548));
#113007=CARTESIAN_POINT('Ctrl Pts',(-1.01684755219409,2.45828501816591,
-7.38865011890989));
#113008=CARTESIAN_POINT('Ctrl Pts',(-1.02259183909231,2.45202942661235,
-7.42996002228574));
#113009=CARTESIAN_POINT('',(-0.334685799463248,2.36147458031212,-7.36640929252461));
#113010=CARTESIAN_POINT('Origin',(-2.13289672382211E-13,2.45311202900011,
-9.91394466520745E-13));
#113011=CARTESIAN_POINT('',(-1.02927110528062,2.2715957307877,-7.42903768924827));
#113012=CARTESIAN_POINT('Ctrl Pts',(-1.0292710965881,2.27159573311762,-7.42903769016891));
#113013=CARTESIAN_POINT('Ctrl Pts',(-0.99949996036425,2.27631121119929,
-7.43316239308187));
#113014=CARTESIAN_POINT('Ctrl Pts',(-0.969723107050798,2.28101755501532,
-7.43710548900528));
#113015=CARTESIAN_POINT('Ctrl Pts',(-0.939943815032056,2.28571428599494,
-7.44086726299595));
#113016=CARTESIAN_POINT('Ctrl Pts',(-0.78960049165936,2.3094261366726,-7.4598589037277));
#113017=CARTESIAN_POINT('Ctrl Pts',(-0.638166486807453,2.33338331970726,
-7.47435486833261));
#113018=CARTESIAN_POINT('Ctrl Pts',(-0.486049526748782,2.35752263424557,
-7.48423381842671));
#113019=CARTESIAN_POINT('Ctrl Pts',(-0.477751680484724,2.35883941260402,
-7.484772706458));
#113020=CARTESIAN_POINT('Ctrl Pts',(-0.469451806683069,2.3601567319788,
-7.48529786806292));
#113021=CARTESIAN_POINT('Ctrl Pts',(-0.461149973068477,2.36147458179854,
-7.48580928773238));
#113022=CARTESIAN_POINT('',(-1.58240141979816,2.36147458149275,-7.33116673650159));
#113023=CARTESIAN_POINT('Origin',(0.0480737921281871,2.4107004486788,0.185219410287693));
#113024=CARTESIAN_POINT('Origin',(0.00954017434101576,2.55351784356558,
0.188586111362571));
#113025=CARTESIAN_POINT('Ctrl Pts',(-0.983691316,2.492226207,-7.18295561700001));
#113026=CARTESIAN_POINT('Ctrl Pts',(-1.376574843,2.42647128,-7.12915100900001));
#113027=CARTESIAN_POINT('Ctrl Pts',(-1.76124628,2.361474582,-7.032816757));
#113028=CARTESIAN_POINT('Ctrl Pts',(-1.76507617162653,2.36082745750497,
-7.03185762744268));
#113029=CARTESIAN_POINT('Ctrl Pts',(-1.76890606325307,2.36018033300993,
-7.03089849788536));
#113030=CARTESIAN_POINT('Ctrl Pts',(-0.773373243,2.492226207,-7.460019693));
#113031=CARTESIAN_POINT('Ctrl Pts',(-1.181411245,2.42647128,-7.417718777));
#113032=CARTESIAN_POINT('Ctrl Pts',(-1.582401422,2.361474582,-7.33116673800001));
#113033=CARTESIAN_POINT('Ctrl Pts',(-1.586393787363,2.36082745750497,-7.33030500276952));
#113034=CARTESIAN_POINT('Ctrl Pts',(-1.590386152726,2.36018033300993,-7.32944326753903));
#113035=CARTESIAN_POINT('',(-1.67182384246072,2.36147458056997,-7.18199174948777));
#113036=CARTESIAN_POINT('Ctrl Pts',(-1.75360411761002,2.36016764195642,
-7.03473060324848));
#113037=CARTESIAN_POINT('Ctrl Pts',(-1.75742519880501,2.36082111197821,
-7.03377368012423));
#113038=CARTESIAN_POINT('Ctrl Pts',(-1.76124628,2.361474582,-7.032816757));
#113039=CARTESIAN_POINT('Ctrl Pts',(-2.143779666,2.426894312,-6.937017944));
#113040=CARTESIAN_POINT('Ctrl Pts',(-2.513665477,2.492218586,-6.800293072));
#113041=CARTESIAN_POINT('Ctrl Pts',(-2.05175975706096,2.36016764195642,
-7.2138996612507));
#113042=CARTESIAN_POINT('Ctrl Pts',(-2.05567800853048,2.36082111197821,
-7.21278063812536));
#113043=CARTESIAN_POINT('Ctrl Pts',(-2.05959626,2.361474582,-7.211661615));
#113044=CARTESIAN_POINT('Ctrl Pts',(-2.451857488,2.426894312,-7.099634761));
#113045=CARTESIAN_POINT('Ctrl Pts',(-2.829653587,2.492218586,-6.945722466));
#113046=CARTESIAN_POINT('',(-2.05959625342164,2.36147458096337,-7.21166159438652));
#113047=CARTESIAN_POINT('',(-2.59590599068159,2.45202942681774,-7.0364246722059));
#113048=CARTESIAN_POINT('Origin',(0.0605646944270258,2.41071409752193,0.183312664479299));
#113049=CARTESIAN_POINT('Ctrl Pts',(-2.50926086840674,2.49144077630432,
-6.80191958692098));
#113050=CARTESIAN_POINT('Ctrl Pts',(-2.52364290615911,2.48454521307526,
-6.84096065213392));
#113051=CARTESIAN_POINT('Ctrl Pts',(-2.53806346503165,2.47781843922134,
-6.88004424096436));
#113052=CARTESIAN_POINT('Ctrl Pts',(-2.56694157478326,2.46469207980874,
-6.95819934878544));
#113053=CARTESIAN_POINT('Ctrl Pts',(-2.5814155901075,2.45828501817934,-6.9973154187694));
#113054=CARTESIAN_POINT('Ctrl Pts',(-2.59590598689054,2.45202942661805,
-7.03642466765963));
#113055=CARTESIAN_POINT('',(-1.91042128011643,2.36147458031212,-7.12223918328643));
#113056=CARTESIAN_POINT('Origin',(-4.23706209007335E-13,2.45311202900022,
-9.58001039608192E-13));
#113057=CARTESIAN_POINT('',(-2.60223082121476,2.27159573077689,-7.0340880540497));
#113058=CARTESIAN_POINT('Ctrl Pts',(-2.6022308128611,2.27159573311295,-7.03408805678627));
#113059=CARTESIAN_POINT('Ctrl Pts',(-2.57404239845067,2.27631121119102,
-7.04451624071727));
#113060=CARTESIAN_POINT('Ctrl Pts',(-2.54580936050126,2.28101755500866,
-7.05476829257287));
#113061=CARTESIAN_POINT('Ctrl Pts',(-2.51753496199034,2.28571428597445,
-7.06484378586096));
#113062=CARTESIAN_POINT('Ctrl Pts',(-2.37478933436481,2.30942611803928,
-7.11571074207617));
#113063=CARTESIAN_POINT('Ctrl Pts',(-2.23001209113176,2.33338328229228,
-7.16242160133055));
#113064=CARTESIAN_POINT('Ctrl Pts',(-2.0835753404843,2.35752257771581,-7.20477021148193));
#113065=CARTESIAN_POINT('Ctrl Pts',(-2.07558722410083,2.35883937490235,
-7.20708032574677));
#113066=CARTESIAN_POINT('Ctrl Pts',(-2.06759417666474,2.36015671312055,
-7.20937746999141));
#113067=CARTESIAN_POINT('Ctrl Pts',(-2.05959626098597,2.36147458179854,
-7.21166161450894));
#113068=CARTESIAN_POINT('',(-3.1213898945122,2.36147458149274,-6.81959860202504));
#113069=CARTESIAN_POINT('Origin',(0.0867666093167069,2.41070047480533,0.170554746132112));
#113070=CARTESIAN_POINT('Origin',(0.0498576749899327,2.55351787035918,0.182126480656974));
#113071=CARTESIAN_POINT('Ctrl Pts',(-2.50481629,2.492226207,-6.803557551));
#113072=CARTESIAN_POINT('Ctrl Pts',(-2.876948019,2.42647128,-6.66655252));
#113073=CARTESIAN_POINT('Ctrl Pts',(-3.231917035,2.361474582,-6.489777522));
#113074=CARTESIAN_POINT('Ctrl Pts',(-3.23545120138537,2.36082745750497,
-6.48801750287848));
#113075=CARTESIAN_POINT('Ctrl Pts',(-3.23898536777074,2.36018033300993,
-6.48625748375697));
#113076=CARTESIAN_POINT('Ctrl Pts',(-2.358975924,2.492226207,-7.11935619199999));
#113077=CARTESIAN_POINT('Ctrl Pts',(-2.748380777,2.42647128,-6.990328138));
#113078=CARTESIAN_POINT('Ctrl Pts',(-3.121389897,2.361474582,-6.819598603));
#113079=CARTESIAN_POINT('Ctrl Pts',(-3.12510367548184,2.36082745750497,
-6.8178987741237));
#113080=CARTESIAN_POINT('Ctrl Pts',(-3.12881745396368,2.36018033300993,
-6.81619894524741));
#113081=CARTESIAN_POINT('',(-3.17665345808772,2.36147458056998,-6.65468806627697));
#113082=CARTESIAN_POINT('Ctrl Pts',(-3.22486496249061,2.36016764195642,
-6.49328946261241));
#113083=CARTESIAN_POINT('Ctrl Pts',(-3.22839099874531,2.36082111197821,
-6.49153349230621));
#113084=CARTESIAN_POINT('Ctrl Pts',(-3.231917035,2.361474582,-6.489777522));
#113085=CARTESIAN_POINT('Ctrl Pts',(-3.58491309,2.426894312,-6.313985061));
#113086=CARTESIAN_POINT('Ctrl Pts',(-3.916759371,2.492218586,-6.100942225));
#113087=CARTESIAN_POINT('Ctrl Pts',(-3.55456593991965,2.36016764195642,
-6.60417499745423));
#113088=CARTESIAN_POINT('Ctrl Pts',(-3.55815202795983,2.36082111197821,
-6.60223982822711));
#113089=CARTESIAN_POINT('Ctrl Pts',(-3.561738116,2.361474582,-6.600304659));
#113090=CARTESIAN_POINT('Ctrl Pts',(-3.920746033,2.426894312,-6.406572362));
#113091=CARTESIAN_POINT('Ctrl Pts',(-4.256622874,2.492218586,-6.175043458));
#113092=CARTESIAN_POINT('',(-3.56173810521021,2.36147458096338,-6.60030464027285));
#113093=CARTESIAN_POINT('',(-4.04783846069933,2.45202942686021,-6.3138739202179));
#113094=CARTESIAN_POINT('Origin',(0.0985555131148149,2.41071414370196,0.166007272848912));
#113095=CARTESIAN_POINT('Ctrl Pts',(-3.91280739158238,2.4914407763751,-6.10347757308063));
#113096=CARTESIAN_POINT('Ctrl Pts',(-3.93524586013339,2.48454521318475,
-6.13851416683736));
#113097=CARTESIAN_POINT('Ctrl Pts',(-3.95773109099203,2.47781843923352,
-6.17358400978743));
#113098=CARTESIAN_POINT('Ctrl Pts',(-4.00273507261549,2.46469208331324,
-6.2437039360965));
#113099=CARTESIAN_POINT('Ctrl Pts',(-4.02527947815753,2.45828502544634,
-6.27879398664533));
#113100=CARTESIAN_POINT('Ctrl Pts',(-4.04783845597553,2.4520294266905,-6.31387391636804));
#113101=CARTESIAN_POINT('',(-3.39682758479658,2.36147458031212,-6.54504108567515));
#113102=CARTESIAN_POINT('Origin',(-4.72278466334686E-13,2.45311202899944,
-7.53303669442928E-13));
#113103=CARTESIAN_POINT('',(-4.0535131159682,2.27159573076159,-6.3102322787032));
#113104=CARTESIAN_POINT('Ctrl Pts',(-4.05351310848486,2.27159573309017,
-6.31023228319568));
#113105=CARTESIAN_POINT('Ctrl Pts',(-4.02822547480738,2.27631121118252,
-6.32647633788707));
#113106=CARTESIAN_POINT('Ctrl Pts',(-4.00285639763014,2.28101755500765,
-6.34255797109834));
#113107=CARTESIAN_POINT('Ctrl Pts',(-3.97740897208463,2.28571428597299,
-6.35847606489208));
#113108=CARTESIAN_POINT('Ctrl Pts',(-3.84893570007535,2.30942609046359,
-6.43883977728116));
#113109=CARTESIAN_POINT('Ctrl Pts',(-3.71758487779749,2.33338322658657,
-6.51558130515849));
#113110=CARTESIAN_POINT('Ctrl Pts',(-3.58367559790876,2.35752249352444,
-6.58841932518766));
#113111=CARTESIAN_POINT('Ctrl Pts',(-3.57637069016739,2.35883931875173,
-6.59239272431891));
#113112=CARTESIAN_POINT('Ctrl Pts',(-3.56905817816386,2.36015668503395,
-6.59635451619828));
#113113=CARTESIAN_POINT('Ctrl Pts',(-3.56173811685735,2.36147458179854,
-6.60030465830847));
#113114=CARTESIAN_POINT('',(-4.51442564736556,2.36147458149274,-5.98915361657529));
#113115=CARTESIAN_POINT('Origin',(0.121402364642468,2.41070043805478,0.147915157977384));
#113116=CARTESIAN_POINT('Origin',(0.0878437654423592,2.55351790115179,0.167150433932087));
#113117=CARTESIAN_POINT('Ctrl Pts',(-3.908818839,2.492226207,-6.106032696));
#113118=CARTESIAN_POINT('Ctrl Pts',(-4.242798303,2.42647128,-5.892233444));
#113119=CARTESIAN_POINT('Ctrl Pts',(-4.551466941,2.361474582,-5.643283502));
#113120=CARTESIAN_POINT('Ctrl Pts',(-4.55454012844867,2.36082745750497,
-5.64080488984796));
#113121=CARTESIAN_POINT('Ctrl Pts',(-4.55761331589734,2.36018033300993,
-5.63832627769592));
#113122=CARTESIAN_POINT('Ctrl Pts',(-3.834275513,2.492226207,-6.445799508));
#113123=CARTESIAN_POINT('Ctrl Pts',(-4.186839079,2.42647128,-6.236077526));
#113124=CARTESIAN_POINT('Ctrl Pts',(-4.51442565,2.361474582,-5.989153617));
#113125=CARTESIAN_POINT('Ctrl Pts',(-4.51768718944525,2.36082745750497,
-5.98669517657394));
#113126=CARTESIAN_POINT('Ctrl Pts',(-4.52094872889051,2.36018033300993,
-5.98423673614789));
#113127=CARTESIAN_POINT('',(-4.53294628858464,2.36147458056998,-5.81621856488957));
#113128=CARTESIAN_POINT('Ctrl Pts',(-4.54533470543984,2.36016764195642,
-5.64822932251851));
#113129=CARTESIAN_POINT('Ctrl Pts',(-4.54840082321992,2.36082111197821,
-5.64575641225926));
#113130=CARTESIAN_POINT('Ctrl Pts',(-4.551466941,2.361474582,-5.643283502));
#113131=CARTESIAN_POINT('Ctrl Pts',(-4.85841996200001,2.426894312,-5.395717254));
#113132=CARTESIAN_POINT('Ctrl Pts',(-5.136709949,2.492218586,-5.11631810000001));
#113133=CARTESIAN_POINT('Ctrl Pts',(-4.89116456977673,2.36016764195642,
-5.68564645093098));
#113134=CARTESIAN_POINT('Ctrl Pts',(-4.89425081288837,2.36082111197821,
-5.68298562196549));
#113135=CARTESIAN_POINT('Ctrl Pts',(-4.897337056,2.361474582,-5.68032479300001));
#113136=CARTESIAN_POINT('Ctrl Pts',(-5.20630485,2.426894312,-5.41394576));
#113137=CARTESIAN_POINT('Ctrl Pts',(-5.484557207,2.492218586,-5.11562628));
#113138=CARTESIAN_POINT('',(-4.89733704140428,2.36147458096338,-5.68032477704211));
#113139=CARTESIAN_POINT('',(-5.31049850288104,2.45202942688488,-5.2960934406446));
#113140=CARTESIAN_POINT('Origin',(0.131937943596592,2.41071410073285,0.140939548902802));
#113141=CARTESIAN_POINT('Ctrl Pts',(-5.13339538944625,2.49144077639895,
-5.11964373170493));
#113142=CARTESIAN_POINT('Ctrl Pts',(-5.16284109109888,2.48454521322505,
-5.14903758175326));
#113143=CARTESIAN_POINT('Ctrl Pts',(-5.19233960943423,2.47781843926765,
-5.17845385126795));
#113144=CARTESIAN_POINT('Ctrl Pts',(-5.25136513497413,2.46469208324408,
-5.23725988734003));
#113145=CARTESIAN_POINT('Ctrl Pts',(-5.28092578911374,2.45828502525069,
-5.26668317184299));
#113146=CARTESIAN_POINT('Ctrl Pts',(-5.31049849743009,2.45202942672717,
-5.296093437831));
#113147=CARTESIAN_POINT('',(-4.72440200654202,2.36147458031212,-5.66180414078946));
#113148=CARTESIAN_POINT('Origin',(-9.68843061333047E-13,2.45311202899956,
-9.64072571774111E-13));
#113149=CARTESIAN_POINT('',(-5.31525764273741,2.27159573079945,-5.29131705571896));
#113150=CARTESIAN_POINT('Ctrl Pts',(-5.3152576362519,2.2715957331383,-5.29131706170207));
#113151=CARTESIAN_POINT('Ctrl Pts',(-5.29405320487535,2.27631121120431,
-5.31261743299678));
#113152=CARTESIAN_POINT('Ctrl Pts',(-5.27273431832996,2.28101755501361,
-5.3337766881094));
#113153=CARTESIAN_POINT('Ctrl Pts',(-5.25130375898295,2.28571428600374,
-5.35479307001672));
#113154=CARTESIAN_POINT('Ctrl Pts',(-5.1431096261441,2.30942616017083,-5.46089619160282));
#113155=CARTESIAN_POINT('Ctrl Pts',(-5.03132653530554,2.3333833670886,-5.56408038258613));
#113156=CARTESIAN_POINT('Ctrl Pts',(-4.91620564381651,2.35752270584896,
-5.66400230049066));
#113157=CARTESIAN_POINT('Ctrl Pts',(-4.90992602055992,2.35883946035909,
-5.6694528489654));
#113158=CARTESIAN_POINT('Ctrl Pts',(-4.903636476675,2.36015675586587,-5.6748936972916));
#113159=CARTESIAN_POINT('Ctrl Pts',(-4.89733705668865,2.36147458179854,
-5.68032479214033));
#113160=CARTESIAN_POINT('',(-5.69637187435096,2.36147458149277,-4.87866246511143));
#113161=CARTESIAN_POINT('Origin',(0.150361561842405,2.41070048208448,0.118359186090153));
#113162=CARTESIAN_POINT('Origin',(0.1217224472246,2.55351790750067,0.144358771677074));
#113163=CARTESIAN_POINT('Ctrl Pts',(-5.130049363,2.492226207,-5.122996538));
#113164=CARTESIAN_POINT('Ctrl Pts',(-5.410260054,2.42647128,-4.842400082));
#113165=CARTESIAN_POINT('Ctrl Pts',(-5.658195312,2.361474582,-4.532915818));
#113166=CARTESIAN_POINT('Ctrl Pts',(-5.66066382168697,2.36082745750497,
-4.5298345099609));
#113167=CARTESIAN_POINT('Ctrl Pts',(-5.66313233137395,2.36018033300993,
-4.52675320192181));
#113168=CARTESIAN_POINT('Ctrl Pts',(-5.13028864,2.492226207,-5.47084440199999));
#113169=CARTESIAN_POINT('Ctrl Pts',(-5.429525439,2.42647128,-5.190234859));
#113170=CARTESIAN_POINT('Ctrl Pts',(-5.696371877,2.361474582,-4.878662465));
#113171=CARTESIAN_POINT('Ctrl Pts',(-5.69902867144889,2.36082745750497,
-4.8755603669806));
#113172=CARTESIAN_POINT('Ctrl Pts',(-5.70168546589777,2.36018033300993,
-4.87245826896118));
#113173=CARTESIAN_POINT('',(-5.67728358890492,2.36147458056998,-4.70578914825017));
#113174=CARTESIAN_POINT('Ctrl Pts',(-5.65326964992618,2.36016764195642,
-4.53906425736617));
#113175=CARTESIAN_POINT('Ctrl Pts',(-5.6557324809631,2.36082111197821,-4.53599003768308));
#113176=CARTESIAN_POINT('Ctrl Pts',(-5.658195312,2.361474582,-4.532915818));
#113177=CARTESIAN_POINT('Ctrl Pts',(-5.904752516,2.426894312,-4.225151705));
#113178=CARTESIAN_POINT('Ctrl Pts',(-6.116473679,2.492218586,-3.892460627));
#113179=CARTESIAN_POINT('Ctrl Pts',(-5.9990577812363,2.36016764195642,-4.50126339560797));
#113180=CARTESIAN_POINT('Ctrl Pts',(-6.00149987011815,2.36082111197821,
-4.49800132430398));
#113181=CARTESIAN_POINT('Ctrl Pts',(-6.003941959,2.361474582,-4.494739253));
#113182=CARTESIAN_POINT('Ctrl Pts',(-6.248422639,2.426894312,-4.168169071));
#113183=CARTESIAN_POINT('Ctrl Pts',(-6.456039741,2.492218586,-3.817008103));
#113184=CARTESIAN_POINT('',(-6.00394194129903,2.36147458096338,-4.49473924056304));
#113185=CARTESIAN_POINT('',(-6.32484553738381,2.45202942687081,-4.0306735180325));
#113186=CARTESIAN_POINT('Origin',(0.159151262774024,2.41071408942526,0.109281780000698));
#113187=CARTESIAN_POINT('Ctrl Pts',(-6.11395152485902,2.49144077640977,
-3.89642103948569));
#113188=CARTESIAN_POINT('Ctrl Pts',(-6.14902761125584,2.48454521320101,
-3.91879772233175));
#113189=CARTESIAN_POINT('Ctrl Pts',(-6.18416009891479,2.47781843925053,
-3.94118494631363));
#113190=CARTESIAN_POINT('Ctrl Pts',(-6.25444719952214,2.46469208329045,
-3.98592738649413));
#113191=CARTESIAN_POINT('Ctrl Pts',(-6.28964187791987,2.45828502538417,
-4.00830810378044));
#113192=CARTESIAN_POINT('Ctrl Pts',(-6.3248455314697,2.45202942670608,-4.03067351650012));
#113193=CARTESIAN_POINT('',(-5.83106864191144,2.36147458031212,-4.51382752721755));
#113194=CARTESIAN_POINT('Origin',(1.18308141061618E-12,2.45311202899989,
7.16874476447416E-13));
#113195=CARTESIAN_POINT('',(-6.32846662960937,2.27159573078434,-4.02498572816645));
#113196=CARTESIAN_POINT('Ctrl Pts',(-6.32846662458287,2.27159573312165,
-4.02498573540134));
#113197=CARTESIAN_POINT('Ctrl Pts',(-6.31233689126107,2.27631121119474,
-4.05034644181493));
#113198=CARTESIAN_POINT('Ctrl Pts',(-6.29606504286073,2.28101755500958,
-4.0755939357117));
#113199=CARTESIAN_POINT('Ctrl Pts',(-6.27965341894199,2.2857142860166,-4.10072590308884));
#113200=CARTESIAN_POINT('Ctrl Pts',(-6.19679771580215,2.30942619544187,
-4.22760712186647));
#113201=CARTESIAN_POINT('Ctrl Pts',(-6.10980946753997,2.33338343821218,
-4.35240916577372));
#113202=CARTESIAN_POINT('Ctrl Pts',(-6.01886015123036,2.35752281333228,
-4.47474272741705));
#113203=CARTESIAN_POINT('Ctrl Pts',(-6.01389918326844,2.35883953204388,
-4.48141559648969));
#113204=CARTESIAN_POINT('Ctrl Pts',(-6.00892644201457,2.36015679172259,
-4.48808112523777));
#113205=CARTESIAN_POINT('Ctrl Pts',(-6.00394195948775,2.36147458179854,
-4.49473925201239));
#113206=CARTESIAN_POINT('',(-6.6119620824281,2.36147458149273,-3.54005047773608));
#113207=CARTESIAN_POINT('Origin',(0.172289535167827,2.41070046788128,0.0832684843953935));
#113208=CARTESIAN_POINT('Origin',(0.149909449784781,2.55351788003384,0.11481695861501));
#113209=CARTESIAN_POINT('Ctrl Pts',(-6.111404481,2.492226207,-3.900414756));
#113210=CARTESIAN_POINT('Ctrl Pts',(-6.324744057,2.42647128,-3.566141474));
#113211=CARTESIAN_POINT('Ctrl Pts',(-6.50035275900001,2.361474582,-3.210594028));
#113212=CARTESIAN_POINT('Ctrl Pts',(-6.50210116616686,2.36082745750497,
-3.20705410261097));
#113213=CARTESIAN_POINT('Ctrl Pts',(-6.50384957333372,2.36018033300993,
-3.20351417722194));
#113214=CARTESIAN_POINT('Ctrl Pts',(-6.18641517199999,2.492226207,-4.240078693));
#113215=CARTESIAN_POINT('Ctrl Pts',(-6.418333224,2.42647128,-3.901702578));
#113216=CARTESIAN_POINT('Ctrl Pts',(-6.611962085,2.361474582,-3.540050477));
#113217=CARTESIAN_POINT('Ctrl Pts',(-6.61388990568557,2.36082745750497,
-3.53644977203438));
#113218=CARTESIAN_POINT('Ctrl Pts',(-6.61581772637116,2.36018033300993,
-3.53284906706876));
#113219=CARTESIAN_POINT('',(-6.55615741798682,2.36147458056998,-3.37532226029513));
#113220=CARTESIAN_POINT('Ctrl Pts',(-6.49686398890001,2.36016764195642,
-3.21765759201994));
#113221=CARTESIAN_POINT('Ctrl Pts',(-6.49860837395001,2.36082111197821,
-3.21412581000997));
#113222=CARTESIAN_POINT('Ctrl Pts',(-6.50035275900001,2.361474582,-3.210594028));
#113223=CARTESIAN_POINT('Ctrl Pts',(-6.674985405,2.426894312,-2.857022758));
#113224=CARTESIAN_POINT('Ctrl Pts',(-6.81023789800001,2.492218586,-2.486596021));
#113225=CARTESIAN_POINT('Ctrl Pts',(-6.82644171740222,2.36016764195642,
-3.10640626662274));
#113226=CARTESIAN_POINT('Ctrl Pts',(-6.82812546270111,2.36082111197821,
-3.10269548381137));
#113227=CARTESIAN_POINT('Ctrl Pts',(-6.829809208,2.361474582,-3.098984701));
#113228=CARTESIAN_POINT('Ctrl Pts',(-6.99837113000001,2.426894312,-2.727493429));
#113229=CARTESIAN_POINT('Ctrl Pts',(-7.125645032,2.492218586,-2.33991087));
#113230=CARTESIAN_POINT('',(-6.82980918807998,2.36147458096342,-3.09898469261055));
#113231=CARTESIAN_POINT('',(-7.04344982391374,2.45202942682679,-2.5767837820567));
#113232=CARTESIAN_POINT('Origin',(0.178922741658617,2.41071411444908,0.0725140132615187));
#113233=CARTESIAN_POINT('Ctrl Pts',(-6.80862608234284,2.49144077638204,
-2.4910060298125));
#113234=CARTESIAN_POINT('Ctrl Pts',(-6.84769243472193,2.48454521316273,
-2.50531923665124));
#113235=CARTESIAN_POINT('Ctrl Pts',(-6.88681613542936,2.47781843924689,
-2.51963061350475));
#113236=CARTESIAN_POINT('Ctrl Pts',(-6.96507828507022,2.46469207983398,
-2.54821735912881));
#113237=CARTESIAN_POINT('Ctrl Pts',(-7.00426134831749,2.45828501820032,
-2.56250902116586));
#113238=CARTESIAN_POINT('Ctrl Pts',(-7.0434498179514,2.45202942663179,-2.57678378194847));
#113239=CARTESIAN_POINT('',(-6.66508098798106,2.36147458031212,-3.15478935503292));
#113240=CARTESIAN_POINT('Origin',(1.07292646989166E-12,2.45311202900022,
3.62990887348147E-13));
#113241=CARTESIAN_POINT('',(-7.04576355034384,2.27159573077844,-2.57045054130644));
#113242=CARTESIAN_POINT('Ctrl Pts',(-7.04576354714259,2.27159573310333,
-2.57045054939503));
#113243=CARTESIAN_POINT('Ctrl Pts',(-7.03546272052735,2.27631121119429,
-2.59868575241402));
#113244=CARTESIAN_POINT('Ctrl Pts',(-7.02499876399313,2.28101755501505,
-2.62684094026218));
#113245=CARTESIAN_POINT('Ctrl Pts',(-7.01437346494182,2.2857142860237,-2.65491335014355));
#113246=CARTESIAN_POINT('Ctrl Pts',(-6.96073054894625,2.30942621516319,
-2.7966398013827));
#113247=CARTESIAN_POINT('Ctrl Pts',(-6.90260473575005,2.33338347798104,
-2.93722406043176));
#113248=CARTESIAN_POINT('Ctrl Pts',(-6.84007980371666,2.35752287343183,
-3.07624905883119));
#113249=CARTESIAN_POINT('Ctrl Pts',(-6.83666934148838,2.35883957212659,
-3.08383226588809));
#113250=CARTESIAN_POINT('Ctrl Pts',(-6.83324580366523,2.36015681177196,
-3.09141083528376));
#113251=CARTESIAN_POINT('Ctrl Pts',(-6.82980920826404,2.36147458179854,
-3.09898469993063));
#113252=CARTESIAN_POINT('',(-7.2183842936436,2.36147458149276,-2.0359096652279));
#113253=CARTESIAN_POINT('Origin',(0.186162053929598,2.41070043126948,0.04428467012911));
#113254=CARTESIAN_POINT('Origin',(0.171087174909335,2.55351792627012,0.0799066088981509));
#113255=CARTESIAN_POINT('Ctrl Pts',(-6.806997118,2.492226207,-2.495453915));
#113256=CARTESIAN_POINT('Ctrl Pts',(-6.943490059,2.42647128,-2.123134053));
#113257=CARTESIAN_POINT('Ctrl Pts',(-7.038560935,2.361474582,-1.73814843));
#113258=CARTESIAN_POINT('Ctrl Pts',(-7.03950748604824,2.36082745750497,
-1.73431541025369));
#113259=CARTESIAN_POINT('Ctrl Pts',(-7.04045403709647,2.36018033300993,
-1.73048239050737));
#113260=CARTESIAN_POINT('Ctrl Pts',(-6.953271806,2.492226207,-2.811051617));
#113261=CARTESIAN_POINT('Ctrl Pts',(-7.10702688,2.42647128,-2.430731022));
#113262=CARTESIAN_POINT('Ctrl Pts',(-7.218384296,2.361474582,-2.035909664));
#113263=CARTESIAN_POINT('Ctrl Pts',(-7.2194930001929,2.36082745750497,-2.03197871704752));
#113264=CARTESIAN_POINT('Ctrl Pts',(-7.2206017043858,2.36018033300993,-2.02804777009504));
#113265=CARTESIAN_POINT('',(-7.12847261325636,2.36147458056998,-1.8870290554756));
#113266=CARTESIAN_POINT('Ctrl Pts',(-7.03667218785752,2.36016764195642,
-1.7457968342631));
#113267=CARTESIAN_POINT('Ctrl Pts',(-7.03761656142876,2.36082111197821,
-1.74197263213155));
#113268=CARTESIAN_POINT('Ctrl Pts',(-7.038560935,2.361474582,-1.73814843));
#113269=CARTESIAN_POINT('Ctrl Pts',(-7.133103396,2.426894312,-1.355302603));
#113270=CARTESIAN_POINT('Ctrl Pts',(-7.185562962,2.492218586,-0.964460949));
#113271=CARTESIAN_POINT('Ctrl Pts',(-7.3346288266832,2.36016764195642,-1.56629703347739));
#113272=CARTESIAN_POINT('Ctrl Pts',(-7.33547549834161,2.36082111197821,
-1.56231105123869));
#113273=CARTESIAN_POINT('Ctrl Pts',(-7.33632217,2.361474582,-1.558325069));
#113274=CARTESIAN_POINT('Ctrl Pts',(-7.421083566,2.426894312,-1.159283226));
#113275=CARTESIAN_POINT('Ctrl Pts',(-7.462063081,2.492218586,-0.753402005000001));
#113276=CARTESIAN_POINT('',(-7.33632214870979,2.36147458096336,-1.5583250651542));
#113277=CARTESIAN_POINT('',(-7.43271022552165,2.45202942683029,-1.00240649998123));
#113278=CARTESIAN_POINT('Origin',(0.190327760252029,2.41071410057973,0.0323555341147232));
#113279=CARTESIAN_POINT('Ctrl Pts',(-7.18493685111934,2.49144077631594,
-0.969114347424825));
#113280=CARTESIAN_POINT('Ctrl Pts',(-7.22616677029348,2.48454521311534,
-0.97469480841737));
#113281=CARTESIAN_POINT('Ctrl Pts',(-7.26745230369469,2.47781843920833,
-0.980261154015143));
#113282=CARTESIAN_POINT('Ctrl Pts',(-7.35003003316461,2.46469207982352,
-0.991355508541588));
#113283=CARTESIAN_POINT('Ctrl Pts',(-7.39136930313058,2.45828501819801,
-0.996889839059943));
#113284=CARTESIAN_POINT('Ctrl Pts',(-7.43271021980434,2.45202942663669,
-1.00240650126442));
#113285=CARTESIAN_POINT('',(-7.18744155484115,2.36147458031212,-1.64823673929096));
#113286=CARTESIAN_POINT('Origin',(-1.77548947766226E-12,2.45311202899944,
-2.20662247155112E-13));
#113287=CARTESIAN_POINT('',(-7.43360839853097,2.27159573080751,-0.99572394410361));
#113288=CARTESIAN_POINT('Ctrl Pts',(-7.43360839709804,2.27159573313597,
-0.995723952718445));
#113289=CARTESIAN_POINT('Ctrl Pts',(-7.42961813203507,2.27631121121225,
-1.02551340564437));
#113290=CARTESIAN_POINT('Ctrl Pts',(-7.42545135009482,2.28101755502214,
-1.05525978226996));
#113291=CARTESIAN_POINT('Ctrl Pts',(-7.42110920294122,2.28571428598379,
-1.0849599999488));
#113292=CARTESIAN_POINT('Ctrl Pts',(-7.39918750952311,2.30942612443413,
-1.2349040331654));
#113293=CARTESIAN_POINT('Ctrl Pts',(-7.37264222487351,2.33338329510612,
-1.3846962719971));
#113294=CARTESIAN_POINT('Ctrl Pts',(-7.34146551075498,2.35752259707394,
-1.53391139070376));
#113295=CARTESIAN_POINT('Ctrl Pts',(-7.3397648315689,2.35883938781293,-1.54205102484443));
#113296=CARTESIAN_POINT('Ctrl Pts',(-7.33805038360176,2.36015671957836,
-1.55018894037855));
#113297=CARTESIAN_POINT('Ctrl Pts',(-7.33632217002799,2.36147458179854,
-1.55832506789888));
#113298=CARTESIAN_POINT('',(-7.48728287696558,2.36147458149276,-0.436571979715356));
#113299=CARTESIAN_POINT('Origin',(0.191329551311815,2.410700463604,0.00322996651999273));
#113300=CARTESIAN_POINT('Origin',(0.184264765178604,2.55351789729557,0.0412597353890298));
#113301=CARTESIAN_POINT('Ctrl Pts',(-7.184302134,2.492226207,-0.973808422));
#113302=CARTESIAN_POINT('Ctrl Pts',(-7.23756618199999,2.42647128,-0.580851245));
#113303=CARTESIAN_POINT('Ctrl Pts',(-7.247653825,2.361474582,-0.184428943));
#113304=CARTESIAN_POINT('Ctrl Pts',(-7.24775426026954,2.36082745750497,
-0.180482056621221));
#113305=CARTESIAN_POINT('Ctrl Pts',(-7.24785469553907,2.36018033300993,
-0.176535170242441));
#113306=CARTESIAN_POINT('Ctrl Pts',(-7.395001179,2.492226207,-1.250582891));
#113307=CARTESIAN_POINT('Ctrl Pts',(-7.463403859,2.42647128,-0.846101184));
#113308=CARTESIAN_POINT('Ctrl Pts',(-7.487282879,2.361474582,-0.436571978));
#113309=CARTESIAN_POINT('Ctrl Pts',(-7.48752062490456,2.36082745750497,
-0.432494595782302));
#113310=CARTESIAN_POINT('Ctrl Pts',(-7.48775837080912,2.36018033300993,
-0.428417213564603));
#113311=CARTESIAN_POINT('',(-7.36746835163083,2.36147458056998,-0.310500469259762));
#113312=CARTESIAN_POINT('Ctrl Pts',(-7.24745341654421,2.36016764195642,
-0.192304556630875));
#113313=CARTESIAN_POINT('Ctrl Pts',(-7.2475536207721,2.36082111197821,-0.188366749815437));
#113314=CARTESIAN_POINT('Ctrl Pts',(-7.247653825,2.361474582,-0.184428943));
#113315=CARTESIAN_POINT('Ctrl Pts',(-7.25768540000001,2.426894312,0.209789996));
#113316=CARTESIAN_POINT('Ctrl Pts',(-7.224899088,2.492218586,0.602771245));
#113317=CARTESIAN_POINT('Ctrl Pts',(-7.49985684282223,2.36016764195642,
0.0470505078652194));
#113318=CARTESIAN_POINT('Ctrl Pts',(-7.49982685141112,2.36082111197821,
0.0511253094326098));
#113319=CARTESIAN_POINT('Ctrl Pts',(-7.49979686,2.361474582,0.055200111));
#113320=CARTESIAN_POINT('Ctrl Pts',(-7.49679438100001,2.426894312,0.463133772));
#113321=CARTESIAN_POINT('Ctrl Pts',(-7.449563353,2.492218586,0.868335101));
#113322=CARTESIAN_POINT('',(-7.49979683838437,2.3614745809634,0.0552001102070129));
#113323=CARTESIAN_POINT('',(-7.47442535691804,2.45202942686423,0.61884219623295));
#113324=CARTESIAN_POINT('Origin',(0.192833561135066,2.41071405963099,-0.0093157574649749));
#113325=CARTESIAN_POINT('Ctrl Pts',(-7.22528795810139,2.49144077637022,
0.598092045178347));
#113326=CARTESIAN_POINT('Ctrl Pts',(-7.26675357866323,2.48454521316813,
0.601505266194621));
#113327=CARTESIAN_POINT('Ctrl Pts',(-7.30827047909649,2.47781843922539,
0.604944228024006));
#113328=CARTESIAN_POINT('Ctrl Pts',(-7.3913025451355,2.46469207985685,0.611861024276025));
#113329=CARTESIAN_POINT('Ctrl Pts',(-7.43286504331232,2.45828501823807,
0.615342804424006));
#113330=CARTESIAN_POINT('Ctrl Pts',(-7.47442535151781,2.4520294266883,0.618842193790386));
#113331=CARTESIAN_POINT('',(-7.37372534259178,2.36147458031212,-0.0646144055263606));
#113332=CARTESIAN_POINT('Origin',(-3.64291929955129E-14,2.45311202899967,
-8.74747865288461E-14));
#113333=CARTESIAN_POINT('',(-7.47386597965565,2.27159573081918,0.625561598277514));
#113334=CARTESIAN_POINT('Ctrl Pts',(-7.47386598001059,2.27159573315804,
0.625561589457456));
#113335=CARTESIAN_POINT('Ctrl Pts',(-7.47637285672591,2.27631121121701,
0.595610808312338));
#113336=CARTESIAN_POINT('Ctrl Pts',(-7.47869808334634,2.28101755501974,
0.565664150456018));
#113337=CARTESIAN_POINT('Ctrl Pts',(-7.48084212200374,2.28571428600819,
0.53572487394781));
#113338=CARTESIAN_POINT('Ctrl Pts',(-7.49166650280563,2.30942617277422,
0.384573624658953));
#113339=CARTESIAN_POINT('Ctrl Pts',(-7.49794273879163,2.33338339250487,
0.232576683279268));
#113340=CARTESIAN_POINT('Ctrl Pts',(-7.49957174307246,2.35752274425865,
0.0801477478569495));
#113341=CARTESIAN_POINT('Ctrl Pts',(-7.49966060121233,2.358839485976,0.0718331278021478));
#113342=CARTESIAN_POINT('Ctrl Pts',(-7.49973564405799,2.36015676867945,
0.0635172263906127));
#113343=CARTESIAN_POINT('Ctrl Pts',(-7.49979685979061,2.36147458179854,
0.0552001120813991));
#113344=CARTESIAN_POINT('',(-7.40608443439015,2.36147458149275,1.1831793268725));
#113345=CARTESIAN_POINT('Origin',(0.187550563654373,2.41070042117061,-0.0379757253984499));
#113346=CARTESIAN_POINT('Origin',(0.188826312576141,2.55351788305839,0.000683636489218209));
#113347=CARTESIAN_POINT('Ctrl Pts',(-7.225677168,2.492226207,0.59337127));
#113348=CARTESIAN_POINT('Ctrl Pts',(-7.193221754,2.42647128,0.988591523));
#113349=CARTESIAN_POINT('Ctrl Pts',(-7.117854477,2.361474582,1.377914237));
#113350=CARTESIAN_POINT('Ctrl Pts',(-7.117104100249,2.36082745750497,1.38179043798336));
#113351=CARTESIAN_POINT('Ctrl Pts',(-7.11635372349801,2.36018033300993,
1.38566663896671));
#113352=CARTESIAN_POINT('Ctrl Pts',(-7.490948515,2.492226207,0.368361701));
#113353=CARTESIAN_POINT('Ctrl Pts',(-7.470800368,2.42647128,0.778091405));
#113354=CARTESIAN_POINT('Ctrl Pts',(-7.406084436,2.361474582,1.183179329));
#113355=CARTESIAN_POINT('Ctrl Pts',(-7.4054401068863,2.36082745750497,1.18721249262722));
#113356=CARTESIAN_POINT('Ctrl Pts',(-7.40479577777259,2.36018033300993,
1.19124565625443));
#113357=CARTESIAN_POINT('',(-7.26196945802254,2.36147458056998,1.28054677436567));
#113358=CARTESIAN_POINT('Ctrl Pts',(-7.11935177812158,2.36016764195642,
1.37017966895271));
#113359=CARTESIAN_POINT('Ctrl Pts',(-7.1186031275608,2.36082111197821,1.37404695297636));
#113360=CARTESIAN_POINT('Ctrl Pts',(-7.117854477,2.361474582,1.377914237));
#113361=CARTESIAN_POINT('Ctrl Pts',(-7.04290610000001,2.426894312,1.765073048));
#113362=CARTESIAN_POINT('Ctrl Pts',(-6.926406962,2.492218586,2.141818525));
#113363=CARTESIAN_POINT('Ctrl Pts',(-7.31439988922279,2.36016764195642,
1.65819802060071));
#113364=CARTESIAN_POINT('Ctrl Pts',(-7.31349463711139,2.36082111197821,
1.66217110830036));
#113365=CARTESIAN_POINT('Ctrl Pts',(-7.312589385,2.361474582,1.666144196));
#113366=CARTESIAN_POINT('Ctrl Pts',(-7.22196342400001,2.426894312,2.06389515));
#113367=CARTESIAN_POINT('Ctrl Pts',(-7.088730323,2.492218586,2.449469822));
#113368=CARTESIAN_POINT('',(-7.31258936405879,2.36147458096341,1.66614419057183));
#113369=CARTESIAN_POINT('',(-7.16664466774274,2.45202942698552,2.21115451601479));
#113370=CARTESIAN_POINT('Origin',(0.186322575069613,2.41071418679769,-0.050551483569205));
#113371=CARTESIAN_POINT('Ctrl Pts',(-6.92779263031738,2.49144077640028,
2.13733231839907));
#113372=CARTESIAN_POINT('Ctrl Pts',(-6.96755506628153,2.48454521316664,
2.14957962298675));
#113373=CARTESIAN_POINT('Ctrl Pts',(-7.00736204944851,2.47781843924576,
2.16186309014197));
#113374=CARTESIAN_POINT('Ctrl Pts',(-7.08696596546045,2.46469207986141,
2.18646761539597));
#113375=CARTESIAN_POINT('Ctrl Pts',(-7.12680827580072,2.45828501824705,
2.19880270199693));
#113376=CARTESIAN_POINT('Ctrl Pts',(-7.16664466189622,2.45202942670426,
2.21115451533576));
#113377=CARTESIAN_POINT('',(-7.21522192883811,2.36147458031212,1.5220292267485));
#113378=CARTESIAN_POINT('Ctrl Pts',(-6.929187568,2.492226207,2.132805581));
#113379=CARTESIAN_POINT('Ctrl Pts',(-6.812530272,2.42647128,2.511808849));
#113380=CARTESIAN_POINT('Ctrl Pts',(-6.655232165,2.361474582,2.875827678));
#113381=CARTESIAN_POINT('Ctrl Pts',(-6.65366606301029,2.36082745750497,
2.87945194674207));
#113382=CARTESIAN_POINT('Ctrl Pts',(-6.65209996102059,2.36018033300993,
2.88307621548415));
#113383=CARTESIAN_POINT('Ctrl Pts',(-7.236627425,2.492226207,1.970082109));
#113384=CARTESIAN_POINT('Ctrl Pts',(-7.128870556,2.42647128,2.365901304));
#113385=CARTESIAN_POINT('Ctrl Pts',(-6.978585717,2.361474582,2.747606485));
#113386=CARTESIAN_POINT('Ctrl Pts',(-6.97708944098073,2.36082745750497,
2.75140684378909));
#113387=CARTESIAN_POINT('Ctrl Pts',(-6.97559316496146,2.36018033300993,
2.75520720257818));
#113388=CARTESIAN_POINT('',(-6.97858570553615,2.36147458149004,2.74760648257101));
#113389=CARTESIAN_POINT('Origin',(0.184554745902666,2.55351828260427,-0.0399231627928354));
#113390=CARTESIAN_POINT('',(-6.81690894434307,2.36147458056998,2.81171707339485));
#113391=CARTESIAN_POINT('Origin',(9.54097911787244E-14,2.45311202899978,
-1.24683249835833E-13));
#113392=CARTESIAN_POINT('',(-7.16465389442683,2.27159573166205,2.21759657512164));
#113393=CARTESIAN_POINT('Ctrl Pts',(-7.16465389665266,2.27159573308995,
2.21759656681736));
#113394=CARTESIAN_POINT('Ctrl Pts',(-7.17354069681518,2.27631121118133,
2.18888492264391));
#113395=CARTESIAN_POINT('Ctrl Pts',(-7.18224920728836,2.28101755500656,
2.16013825594367));
#113396=CARTESIAN_POINT('Ctrl Pts',(-7.19077917892545,2.28571428597853,
2.13135984807086));
#113397=CARTESIAN_POINT('Ctrl Pts',(-7.23384342168401,2.30942610672504,
1.9860697577258));
#113398=CARTESIAN_POINT('Ctrl Pts',(-7.27264767649734,2.33338325938208,
1.83897603880896));
#113399=CARTESIAN_POINT('Ctrl Pts',(-7.30700624033689,2.35752254308601,
1.69046141520244));
#113400=CARTESIAN_POINT('Ctrl Pts',(-7.30888051535824,2.35883935180626,
1.68235987607438));
#113401=CARTESIAN_POINT('Ctrl Pts',(-7.31074157218808,2.36015670156782,
1.67425411523461));
#113402=CARTESIAN_POINT('Ctrl Pts',(-7.31258938456305,2.36147458179854,
1.6661441970111));
#113403=CARTESIAN_POINT('Origin',(0.17499824870831,2.41070077462701,-0.0774045721351185));
#113404=CARTESIAN_POINT('Ctrl Pts',(-6.65835716353885,2.36016764195642,
2.86859581532773));
#113405=CARTESIAN_POINT('Ctrl Pts',(-6.65679466426943,2.36082111197821,
2.87221174666387));
#113406=CARTESIAN_POINT('Ctrl Pts',(-6.655232165,2.361474582,2.875827678));
#113407=CARTESIAN_POINT('Ctrl Pts',(-6.49880834,2.426894312,3.237823246));
#113408=CARTESIAN_POINT('Ctrl Pts',(-6.304043745,2.492218586,3.580716752));
#113409=CARTESIAN_POINT('Ctrl Pts',(-6.78692972648235,2.36016764195642,
3.19181003665553));
#113410=CARTESIAN_POINT('Ctrl Pts',(-6.78519154224117,2.36082111197821,
3.19549563332777));
#113411=CARTESIAN_POINT('Ctrl Pts',(-6.783453358,2.361474582,3.19918123));
#113412=CARTESIAN_POINT('Ctrl Pts',(-6.609441483,2.426894312,3.568151085));
#113413=CARTESIAN_POINT('Ctrl Pts',(-6.396436141,2.492218586,3.916070057));
#113414=CARTESIAN_POINT('',(-6.78345333872078,2.36147458096338,3.19918122017551));
#113415=CARTESIAN_POINT('',(-6.71934275718553,2.36147458031212,3.03750446354416));
#113416=CARTESIAN_POINT('',(-6.52375963646868,2.45202942685875,3.70007571388178));
#113417=CARTESIAN_POINT('Origin',(0.17109954117571,2.41071407661823,-0.089423536925872));
#113418=CARTESIAN_POINT('Ctrl Pts',(-6.30636141922389,2.49144077637438,
3.57663330860409));
#113419=CARTESIAN_POINT('Ctrl Pts',(-6.34256142319105,2.48454521312223,
3.59714202627954));
#113420=CARTESIAN_POINT('Ctrl Pts',(-6.37879715856625,2.47781843924882,
3.61769563722942));
#113421=CARTESIAN_POINT('Ctrl Pts',(-6.45125073361651,2.46469207983837,
3.65883741112242));
#113422=CARTESIAN_POINT('Ctrl Pts',(-6.48750987377411,2.45828501822364,
3.67944902918302));
#113423=CARTESIAN_POINT('Ctrl Pts',(-6.52375963243751,2.45202942668014,
3.70007570940484));
#113424=CARTESIAN_POINT('Origin',(-1.38821246165044E-12,2.45311202899956,
8.14018991102117E-13));
#113425=CARTESIAN_POINT('',(-6.22477608441886,2.36147458149275,4.18355861340272));
#113426=CARTESIAN_POINT('Origin',(0.171661065249297,2.5535178799818,-0.0786655937107383));
#113427=CARTESIAN_POINT('',(-6.52043055591603,2.27159573079198,3.70593920125996));
#113428=CARTESIAN_POINT('Ctrl Pts',(-6.52043055998516,2.27159573312279,
3.70593919351544));
#113429=CARTESIAN_POINT('Ctrl Pts',(-6.53528174642073,2.2763112112019,3.67980921105351));
#113430=CARTESIAN_POINT('Ctrl Pts',(-6.54996634030221,2.28101755501622,
3.6536066978739));
#113431=CARTESIAN_POINT('Ctrl Pts',(-6.5644833929722,2.28571428599651,3.62733480496704));
#113432=CARTESIAN_POINT('Ctrl Pts',(-6.63777403314015,2.30942615217881,
3.49469880110261));
#113433=CARTESIAN_POINT('Ctrl Pts',(-6.70729199307885,2.33338335102282,
3.35938555588206));
#113434=CARTESIAN_POINT('Ctrl Pts',(-6.77277363651984,2.35752268157398,
3.2217289252915));
#113435=CARTESIAN_POINT('Ctrl Pts',(-6.77634555739711,2.35883944416923,
3.21421997214277));
#113436=CARTESIAN_POINT('Ctrl Pts',(-6.77990547750036,2.36015674776775,
3.20670405495281));
#113437=CARTESIAN_POINT('Ctrl Pts',(-6.78345335735591,2.36147458179854,
3.19918123089353));
#113438=CARTESIAN_POINT('Origin',(0.154270784383641,2.41070044892372,-0.113216334444677));
#113439=CARTESIAN_POINT('Ctrl Pts',(-6.308696859,2.492226207,3.572512274));
#113440=CARTESIAN_POINT('Ctrl Pts',(-6.113292446,2.42647128,3.917576786));
#113441=CARTESIAN_POINT('Ctrl Pts',(-5.881418593,2.361474582,4.239270613));
#113442=CARTESIAN_POINT('Ctrl Pts',(-5.87910999495346,2.36082745750497,
4.24247348271121));
#113443=CARTESIAN_POINT('Ctrl Pts',(-5.87680139690693,2.36018033300993,
4.24567635242242));
#113444=CARTESIAN_POINT('Ctrl Pts',(-6.643929679,2.492226207,3.479683667));
#113445=CARTESIAN_POINT('Ctrl Pts',(-6.453602679,2.42647128,3.843084288));
#113446=CARTESIAN_POINT('Ctrl Pts',(-6.224776085,2.361474582,4.183558616));
#113447=CARTESIAN_POINT('Ctrl Pts',(-6.22249782627842,2.36082745750497,
4.18694846939808));
#113448=CARTESIAN_POINT('Ctrl Pts',(-6.22021956755684,2.36018033300993,
4.19033832279615));
#113449=CARTESIAN_POINT('',(-6.05309734400731,2.36147458056997,4.21141460730296));
#113450=CARTESIAN_POINT('Ctrl Pts',(-5.88602516750172,2.36016764195642,
4.23287960957504));
#113451=CARTESIAN_POINT('Ctrl Pts',(-5.88372188025086,2.36082111197821,
4.23607511128752));
#113452=CARTESIAN_POINT('Ctrl Pts',(-5.881418593,2.361474582,4.239270613));
#113453=CARTESIAN_POINT('Ctrl Pts',(-5.650833524,2.426894312,4.559176427));
#113454=CARTESIAN_POINT('Ctrl Pts',(-5.386910449,2.492218586,4.852184643));
#113455=CARTESIAN_POINT('Ctrl Pts',(-5.9421102725929,2.36016764195642,4.57617656251187));
#113456=CARTESIAN_POINT('Ctrl Pts',(-5.93962043179645,2.36082111197821,
4.57940233375593));
#113457=CARTESIAN_POINT('Ctrl Pts',(-5.93713059100001,2.361474582,4.582628105));
#113458=CARTESIAN_POINT('Ctrl Pts',(-5.68786940500001,2.426894312,4.905564241));
#113459=CARTESIAN_POINT('Ctrl Pts',(-5.405051715,2.492218586,5.199559208));
#113460=CARTESIAN_POINT('',(-5.93713057428633,2.36147458096336,4.58262809126086));
#113461=CARTESIAN_POINT('',(-5.57583085666585,2.45202942684484,5.01598548058866));
#113462=CARTESIAN_POINT('Origin',(0.14787568222294,2.41071408521665,-0.124114020875486));
#113463=CARTESIAN_POINT('Ctrl Pts',(-5.39005175674965,2.4914407764098,4.84869489944713));
#113464=CARTESIAN_POINT('Ctrl Pts',(-5.42099665665192,2.48454521318188,
4.87650606538268));
#113465=CARTESIAN_POINT('Ctrl Pts',(-5.4519668020571,2.47781843928518,4.90436875641983));
#113466=CARTESIAN_POINT('Ctrl Pts',(-5.51388218768978,2.46469207987048,
4.96012403546337));
#113467=CARTESIAN_POINT('Ctrl Pts',(-5.54486272088388,2.4582850182284,4.98804840880374));
#113468=CARTESIAN_POINT('Ctrl Pts',(-5.57583085399527,2.45202942665872,
5.01598547540733));
#113469=CARTESIAN_POINT('',(-5.90927458573466,2.36147458031211,4.41094936739357));
#113470=CARTESIAN_POINT('Origin',(-1.13103970633688E-12,2.45311202899944,
1.05774763947686E-12));
#113471=CARTESIAN_POINT('',(-5.5713191313085,2.27159573083506,5.02099622960137));
#113472=CARTESIAN_POINT('Ctrl Pts',(-5.57131913694017,2.27159573319232,
5.02099622266133));
#113473=CARTESIAN_POINT('Ctrl Pts',(-5.5914402845158,2.27631121122797,4.99866971064512));
#113474=CARTESIAN_POINT('Ctrl Pts',(-5.61141432647901,2.28101755501943,
4.97623655128185));
#113475=CARTESIAN_POINT('Ctrl Pts',(-5.63123965890202,2.28571428598273,
4.95369961782458));
#113476=CARTESIAN_POINT('Ctrl Pts',(-5.731329636829,2.30942615505832,4.83991987603559));
#113477=CARTESIAN_POINT('Ctrl Pts',(-5.82831066571407,2.33338335700141,
4.72271447127471));
#113478=CARTESIAN_POINT('Ctrl Pts',(-5.92185350248422,2.35752269062246,
4.6023527781534));
#113479=CARTESIAN_POINT('Ctrl Pts',(-5.9269561050895,2.35883945020424,4.59578725255997));
#113480=CARTESIAN_POINT('Ctrl Pts',(-5.93204848460138,2.36015675078659,
4.58921234597057));
#113481=CARTESIAN_POINT('Ctrl Pts',(-5.93713059017888,2.36147458179854,
4.58262810573419));
#113482=CARTESIAN_POINT('',(-5.17990284201352,2.36147458149274,5.42389219232862));
#113483=CARTESIAN_POINT('Origin',(0.126325665247499,2.41070046202241,-0.143732892703099));
#113484=CARTESIAN_POINT('Origin',(0.150736867158598,2.55351783920603,-0.113728427993419));
#113485=CARTESIAN_POINT('Ctrl Pts',(-5.393218496,2.492226207,4.845172263));
#113486=CARTESIAN_POINT('Ctrl Pts',(-5.12820386,2.42647128,5.140163186));
#113487=CARTESIAN_POINT('Ctrl Pts',(-4.832596425,2.361474582,5.404489966));
#113488=CARTESIAN_POINT('Ctrl Pts',(-4.82965327837888,2.36082745750497,
5.40712167406049));
#113489=CARTESIAN_POINT('Ctrl Pts',(-4.82671013175777,2.36018033300993,
5.40975338212096));
#113490=CARTESIAN_POINT('Ctrl Pts',(-5.740569165,2.492226207,4.826579084));
#113491=CARTESIAN_POINT('Ctrl Pts',(-5.476571513,2.42647128,5.140568922));
#113492=CARTESIAN_POINT('Ctrl Pts',(-5.179902842,2.361474582,5.423892195));
#113493=CARTESIAN_POINT('Ctrl Pts',(-5.17694912942966,2.36082745750497,
5.42671303722142));
#113494=CARTESIAN_POINT('Ctrl Pts',(-5.17399541685932,2.36018033300993,
5.42953387944285));
#113495=CARTESIAN_POINT('',(-5.00624963993739,2.36147458056997,5.41419107454764));
#113496=CARTESIAN_POINT('Ctrl Pts',(-4.83846917719169,2.36016764195642,
5.39923865803316));
#113497=CARTESIAN_POINT('Ctrl Pts',(-4.83553280109584,2.36082111197821,
5.40186431201658));
#113498=CARTESIAN_POINT('Ctrl Pts',(-4.83259642500001,2.361474582,5.404489966));
#113499=CARTESIAN_POINT('Ctrl Pts',(-4.538632012,2.426894312,5.667347586));
#113500=CARTESIAN_POINT('Ctrl Pts',(-4.217891208,2.492218586,5.896769773));
#113501=CARTESIAN_POINT('Ctrl Pts',(-4.81944434632715,2.36016764195642,
5.74656615832854));
#113502=CARTESIAN_POINT('Ctrl Pts',(-4.81631927116357,2.36082111197821,
5.74918127066428));
#113503=CARTESIAN_POINT('Ctrl Pts',(-4.813194196,2.361474582,5.751796383));
#113504=CARTESIAN_POINT('Ctrl Pts',(-4.500338875,2.426894312,6.01359866500001));
#113505=CARTESIAN_POINT('Ctrl Pts',(-4.160933077,2.492218586,6.23992275));
#113506=CARTESIAN_POINT('',(-4.81319418262263,2.36147458096339,5.75179636599494));
#113507=CARTESIAN_POINT('',(-4.36718242293266,2.45202942683089,6.09735334139361));
#113508=CARTESIAN_POINT('Origin',(0.117737553260419,2.41071407554446,-0.153001151993558));
#113509=CARTESIAN_POINT('Ctrl Pts',(-4.2217092652745,2.49144077645184,5.89403690575462));
#113510=CARTESIAN_POINT('Ctrl Pts',(-4.24595211176852,2.48454521320699,
5.92785010093519));
#113511=CARTESIAN_POINT('Ctrl Pts',(-4.27020853744412,2.47781843925731,
5.96171904380918));
#113512=CARTESIAN_POINT('Ctrl Pts',(-4.31869063871647,2.46469207984206,
6.02948077314091));
#113513=CARTESIAN_POINT('Ctrl Pts',(-4.34294394942702,2.45828501820144,
6.06341218901115));
#113514=CARTESIAN_POINT('Ctrl Pts',(-4.36718242130856,2.45202942663775,
6.09735333570621));
#113515=CARTESIAN_POINT('',(-4.82289530257678,2.36147458031212,5.57814318135047));
#113516=CARTESIAN_POINT('Origin',(-3.28946939132102E-13,2.45311202899922,
5.1911600018606E-13));
#113517=CARTESIAN_POINT('',(-4.36169901639869,2.27159573075345,6.10127705382252));
#113518=CARTESIAN_POINT('Ctrl Pts',(-4.36169902333983,2.27159573307932,
6.10127704857741));
#113519=CARTESIAN_POINT('Ctrl Pts',(-4.38614929003948,2.27631121117809,
6.08379797009143));
#113520=CARTESIAN_POINT('Ctrl Pts',(-4.41047881627064,2.28101755500682,
6.06618311407453));
#113521=CARTESIAN_POINT('Ctrl Pts',(-4.434685417972,2.28571428599309,6.04843494196295));
#113522=CARTESIAN_POINT('Ctrl Pts',(-4.55689457609569,2.30942614485292,
5.95883173353127));
#113523=CARTESIAN_POINT('Ctrl Pts',(-4.67680388863052,2.33338333625891,
5.86521462189015));
#113524=CARTESIAN_POINT('Ctrl Pts',(-4.79403390338584,2.35752265926315,
5.76777590841553));
#113525=CARTESIAN_POINT('Ctrl Pts',(-4.80042865478654,2.35883942928929,
5.76246074786749));
#113526=CARTESIAN_POINT('Ctrl Pts',(-4.80681543861544,2.36015674032481,
5.75713422780452));
#113527=CARTESIAN_POINT('Ctrl Pts',(-4.81319419504025,2.36147458179854,
5.75179638354049));
#113528=CARTESIAN_POINT('',(-3.89282309958484,2.36147458149274,6.4106106013945));
#113529=CARTESIAN_POINT('Origin',(0.0924741257365813,2.41070046819418,-0.1675290846441));
#113530=CARTESIAN_POINT('Origin',(0.122764507635105,2.553517885663,-0.143473533098674));
#113531=CARTESIAN_POINT('Ctrl Pts',(-4.22555923,2.492226207,5.891277382));
#113532=CARTESIAN_POINT('Ctrl Pts',(-3.90332616,2.42647128,6.122401268));
#113533=CARTESIAN_POINT('Ctrl Pts',(-3.557807419,2.361474582,6.317001375));
#113534=CARTESIAN_POINT('Ctrl Pts',(-3.55436734207803,2.36082745750497,
6.31893886567032));
#113535=CARTESIAN_POINT('Ctrl Pts',(-3.55092726515605,2.36018033300993,
6.32087635634062));
#113536=CARTESIAN_POINT('Ctrl Pts',(-4.568786018,2.492226207,5.947789028));
#113537=CARTESIAN_POINT('Ctrl Pts',(-4.243461951,2.42647128,6.197686266));
#113538=CARTESIAN_POINT('Ctrl Pts',(-3.892823099,2.361474582,6.41061060400001));
#113539=CARTESIAN_POINT('Ctrl Pts',(-3.88933204488461,2.36082745750497,
6.41273053561112));
#113540=CARTESIAN_POINT('Ctrl Pts',(-3.88584099076922,2.36018033300993,
6.41485046722225));
#113541=CARTESIAN_POINT('',(-3.72531526656647,2.36147458056997,6.36380598507066));
#113542=CARTESIAN_POINT('Ctrl Pts',(-3.56467174548097,2.36016764195642,
6.31313530783206));
#113543=CARTESIAN_POINT('Ctrl Pts',(-3.56123958224049,2.36082111197821,
6.31506834141603));
#113544=CARTESIAN_POINT('Ctrl Pts',(-3.557807419,2.361474582,6.317001375));
#113545=CARTESIAN_POINT('Ctrl Pts',(-3.214209113,2.426894312,6.51051987));
#113546=CARTESIAN_POINT('Ctrl Pts',(-2.851648061,2.492218586,6.665628503));
#113547=CARTESIAN_POINT('Ctrl Pts',(-3.47142655900055,2.36016764195642,
6.64825270764319));
#113548=CARTESIAN_POINT('Ctrl Pts',(-3.46781237450027,2.36082111197821,
6.6501348813216));
#113549=CARTESIAN_POINT('Ctrl Pts',(-3.46419819,2.361474582,6.652017055));
#113550=CARTESIAN_POINT('Ctrl Pts',(-3.1023775,2.426894312,6.840443899));
#113551=CARTESIAN_POINT('Ctrl Pts',(-2.722253834,2.492218586,6.988514439));
#113552=CARTESIAN_POINT('',(-3.46419818055662,2.36147458096339,6.65201703555471));
#113553=CARTESIAN_POINT('',(-2.95432939283039,2.45202942682624,6.89361573653466));
#113554=CARTESIAN_POINT('Origin',(0.0820942584082386,2.41071412403309,-0.174734328481542));
#113555=CARTESIAN_POINT('Ctrl Pts',(-2.8559643401511,2.49144077638546,6.66378029826372));
#113556=CARTESIAN_POINT('Ctrl Pts',(-2.87237156518068,2.48454521313266,
6.70201445509764));
#113557=CARTESIAN_POINT('Ctrl Pts',(-2.88878006762336,2.47781843920517,
6.7403059752111));
#113558=CARTESIAN_POINT('Ctrl Pts',(-2.92156191563384,2.46469207979522,
6.81690569143143));
#113559=CARTESIAN_POINT('Ctrl Pts',(-2.9379539459407,2.45828501817635,6.85525755431668));
#113560=CARTESIAN_POINT('Ctrl Pts',(-2.95432939247112,2.45202942663078,
6.89361573063811));
#113561=CARTESIAN_POINT('',(-3.51100279528937,2.36147458031211,6.48450921998705));
#113562=CARTESIAN_POINT('Origin',(5.55111512312578E-13,2.45311202900067,
-1.28586377656781E-12));
#113563=CARTESIAN_POINT('',(-2.94813070274797,2.27159573080254,6.89626894453793));
#113564=CARTESIAN_POINT('Ctrl Pts',(-2.94813071078491,2.27159573316313,
6.89626894059832));
#113565=CARTESIAN_POINT('Ctrl Pts',(-2.97576682895059,2.27631121120737,
6.88445459749243));
#113566=CARTESIAN_POINT('Ctrl Pts',(-3.00331421772734,2.28101755500858,
6.87248169581864));
#113567=CARTESIAN_POINT('Ctrl Pts',(-3.03077021493258,2.28571428598784,
6.86035217002096));
#113568=CARTESIAN_POINT('Ctrl Pts',(-3.16938408801206,2.30942612020512,
6.79911525570395));
#113569=CARTESIAN_POINT('Ctrl Pts',(-3.3066147584816,2.33338328651352,6.73346389045273));
#113570=CARTESIAN_POINT('Ctrl Pts',(-3.44205030695843,2.35752258408356,
6.66350430934275));
#113571=CARTESIAN_POINT('Ctrl Pts',(-3.44943829583462,2.35883937914905,
6.65968802467572));
#113572=CARTESIAN_POINT('Ctrl Pts',(-3.45682094517355,2.36015671524464,
6.65585893279283));
#113573=CARTESIAN_POINT('Ctrl Pts',(-3.4641981889465,2.36147458179854,6.65201705532155));
#113574=CARTESIAN_POINT('',(-2.42371927611264,2.36147458149276,7.09757598358083));
#113575=CARTESIAN_POINT('Origin',(0.0542983013924922,2.4107004966354,-0.183491481210859));
#113576=CARTESIAN_POINT('Origin',(0.0890517491531923,2.55351788318359,-0.166509867032308));
#113577=CARTESIAN_POINT('Ctrl Pts',(-2.860317511,2.492226207,6.661912919));
#113578=CARTESIAN_POINT('Ctrl Pts',(-2.495933268,2.42647128,6.818362672));
#113579=CARTESIAN_POINT('Ctrl Pts',(-2.116659292,2.361474582,6.93413682));
#113580=CARTESIAN_POINT('Ctrl Pts',(-2.1128831389376,2.36082745750497,6.93528949835702));
#113581=CARTESIAN_POINT('Ctrl Pts',(-2.1091069858752,2.36018033300993,6.93644217671405));
#113582=CARTESIAN_POINT('Ctrl Pts',(-3.183371514,2.492226207,6.790886967));
#113583=CARTESIAN_POINT('Ctrl Pts',(-2.811932824,2.42647128,6.965006689));
#113584=CARTESIAN_POINT('Ctrl Pts',(-2.423719275,2.361474582,7.097575986));
#113585=CARTESIAN_POINT('Ctrl Pts',(-2.4198541171598,2.36082745750497,7.09889588134881));
#113586=CARTESIAN_POINT('Ctrl Pts',(-2.4159889593196,2.36018033300993,7.10021577669761));
#113587=CARTESIAN_POINT('',(-2.2701892918417,2.36147458056998,7.0158564003008));
#113588=CARTESIAN_POINT('Ctrl Pts',(-2.12419422451128,2.36016764195642,
6.93183676660004));
#113589=CARTESIAN_POINT('Ctrl Pts',(-2.12042675825564,2.36082111197821,
6.93298679330001));
#113590=CARTESIAN_POINT('Ctrl Pts',(-2.116659292,2.361474582,6.93413682));
#113591=CARTESIAN_POINT('Ctrl Pts',(-1.739493367,2.426894312,7.049267482));
#113592=CARTESIAN_POINT('Ctrl Pts',(-1.352065021,2.492218586,7.122809851));
#113593=CARTESIAN_POINT('Ctrl Pts',(-1.96108872313987,2.36016764195642,
7.23907434966039));
#113594=CARTESIAN_POINT('Ctrl Pts',(-1.95715442456993,2.36082111197821,
7.2401355763302));
#113595=CARTESIAN_POINT('Ctrl Pts',(-1.953220126,2.361474582,7.241196803));
#113596=CARTESIAN_POINT('Ctrl Pts',(-1.559352402,2.426894312,7.347437579));
#113597=CARTESIAN_POINT('Ctrl Pts',(-1.156285027,2.492218586,7.41033096));
#113598=CARTESIAN_POINT('',(-1.95322012100067,2.36147458096337,7.24119678195224));
#113599=CARTESIAN_POINT('',(-1.40333520372143,2.45202942685434,7.36754032174613));
#113600=CARTESIAN_POINT('Origin',(0.0426122198937216,2.41071409218959,-0.18829692376378));
#113601=CARTESIAN_POINT('Ctrl Pts',(-1.3566776972798,2.49144077638316,7.121932728778));
#113602=CARTESIAN_POINT('Ctrl Pts',(-1.36448211673127,2.48454521316821,
7.16280006073904));
#113603=CARTESIAN_POINT('Ctrl Pts',(-1.37227545238057,2.47781843928024,
7.20372368937314));
#113604=CARTESIAN_POINT('Ctrl Pts',(-1.38782420408007,2.46469207987779,
7.28557967538297));
#113605=CARTESIAN_POINT('Ctrl Pts',(-1.39558848094723,2.45828501824256,
7.32655869521264));
#113606=CARTESIAN_POINT('Ctrl Pts',(-1.40333520459521,2.45202942667326,
7.36754031585559));
#113607=CARTESIAN_POINT('',(-2.03493969893267,2.36147458031212,7.08766681439043));
#113608=CARTESIAN_POINT('Origin',(-8.35919874986324E-14,2.45311202900044,
5.48606299277665E-13));
#113609=CARTESIAN_POINT('',(-1.39671107471047,2.27159573078887,7.36879896398992));
#113610=CARTESIAN_POINT('Ctrl Pts',(-1.39671108335984,2.27159573313922,
7.36879896191029));
#113611=CARTESIAN_POINT('Ctrl Pts',(-1.42624081901485,2.27631121119733,
7.36320178012557));
#113612=CARTESIAN_POINT('Ctrl Pts',(-1.45571798513491,2.28101755500643,
7.35743067251521));
#113613=CARTESIAN_POINT('Ctrl Pts',(-1.48513956595445,2.28571428599273,
7.3514869560092));
#113614=CARTESIAN_POINT('Ctrl Pts',(-1.6336769181982,2.30942613108789,7.32147959850119));
#113615=CARTESIAN_POINT('Ctrl Pts',(-1.781812381869,2.33338330844784,7.28686364542245));
#113616=CARTESIAN_POINT('Ctrl Pts',(-1.92912083042035,2.35752261723028,
7.24765429772187));
#113617=CARTESIAN_POINT('Ctrl Pts',(-1.9371564131139,2.35883940125587,7.24551545260534));
#113618=CARTESIAN_POINT('Ctrl Pts',(-1.94518953431861,2.36015672630246,
7.24336295208475));
#113619=CARTESIAN_POINT('Ctrl Pts',(-1.953220124902,2.36147458179854,7.24119680308756));
#113620=CARTESIAN_POINT('',(-0.841285032614847,2.36147458149274,7.45266660087847));
#113621=CARTESIAN_POINT('Origin',(0.0135835823357038,2.41070044829264,-0.190873985324191));
#113622=CARTESIAN_POINT('Origin',(0.0511750907285721,2.55351789526579,-0.181760610305085));
#113623=CARTESIAN_POINT('Ctrl Pts',(-1.361330525,2.492226207,7.121044811));
#113624=CARTESIAN_POINT('Ctrl Pts',(-0.971833309999999,2.42647128,7.195505015));
#113625=CARTESIAN_POINT('Ctrl Pts',(-0.576538529,2.361474582,7.22703973500001));
#113626=CARTESIAN_POINT('Ctrl Pts',(-0.572602868521616,2.36082745750497,
7.22735370309967));
#113627=CARTESIAN_POINT('Ctrl Pts',(-0.568667208043231,2.36018033300993,
7.22766767119934));
#113628=CARTESIAN_POINT('Ctrl Pts',(-1.649106096,2.492226207,7.31645058));
#113629=CARTESIAN_POINT('Ctrl Pts',(-1.248920843,2.42647128,7.40665114));
#113630=CARTESIAN_POINT('Ctrl Pts',(-0.841285031000001,2.361474582,7.452666603));
#113631=CARTESIAN_POINT('Ctrl Pts',(-0.837226499918957,2.36082745750497,
7.45312474524682));
#113632=CARTESIAN_POINT('Ctrl Pts',(-0.833167968837915,2.36018033300993,
7.45358288749364));
#113633=CARTESIAN_POINT('',(-0.708911788726928,2.36147458056998,7.33985316815712));
#113634=CARTESIAN_POINT('Origin',(2.954450920023E-15,2.45311202899978,-8.63024929298462E-14));
#113635=CARTESIAN_POINT('',(0.220017211027225,2.27159573079591,7.49677213352331));
#113636=CARTESIAN_POINT('',(-0.350911660640484,2.36147458096338,7.49178621436893));
#113637=CARTESIAN_POINT('Ctrl Pts',(0.220017202257164,2.27159573312873,
7.49677213346454));
#113638=CARTESIAN_POINT('Ctrl Pts',(0.189974626846442,2.27631121120357,
7.49765383118156));
#113639=CARTESIAN_POINT('Ctrl Pts',(0.159946002989426,2.28101755501591,
7.49835436841248));
#113640=CARTESIAN_POINT('Ctrl Pts',(0.129934559153272,2.28571428596736,
7.49887438293933));
#113641=CARTESIAN_POINT('Ctrl Pts',(-0.0215804301581485,2.30942607826874,
7.50149971437863));
#113642=CARTESIAN_POINT('Ctrl Pts',(-0.173693637262223,2.33338320200953,
7.4995378236021));
#113643=CARTESIAN_POINT('Ctrl Pts',(-0.325986608252011,2.35752245638422,
7.49291216606165));
#113644=CARTESIAN_POINT('Ctrl Pts',(-0.334294450196394,2.3588392939815,
7.49255072511486));
#113645=CARTESIAN_POINT('Ctrl Pts',(-0.342602823753382,2.36015667264389,
7.49217541774316));
#113646=CARTESIAN_POINT('Ctrl Pts',(-0.350911659908851,2.36147458179854,
7.49178623584948));
#113647=CARTESIAN_POINT('Origin',(-0.0277662652684496,2.4107004765019,-0.18933166728919));
#113648=CARTESIAN_POINT('Origin',(0.00113769343467042,2.41071408166251,
-0.193055184199305));
#113649=CARTESIAN_POINT('Ctrl Pts',(-0.584391742461101,2.36016764195642,
7.22641324335268));
#113650=CARTESIAN_POINT('Ctrl Pts',(-0.58046513573055,2.36082111197821,
7.22672648917634));
#113651=CARTESIAN_POINT('Ctrl Pts',(-0.576538529,2.361474582,7.227039735));
#113652=CARTESIAN_POINT('Ctrl Pts',(-0.183440845,2.426894312,7.25839918));
#113653=CARTESIAN_POINT('Ctrl Pts',(0.210739078,2.492218586,7.246936528));
#113654=CARTESIAN_POINT('Ctrl Pts',(-0.359052559442651,2.36016764195642,
7.49140492024465));
#113655=CARTESIAN_POINT('Ctrl Pts',(-0.354982110221325,2.36082111197821,
7.49159557812232));
#113656=CARTESIAN_POINT('Ctrl Pts',(-0.350911661,2.361474582,7.491786236));
#113657=CARTESIAN_POINT('Ctrl Pts',(0.056586281,2.426894312,7.510873243));
#113658=CARTESIAN_POINT('Ctrl Pts',(0.463750383,2.492218586,7.485648641));
#113659=CARTESIAN_POINT('',(-0.46372508454669,2.36147458031212,7.35941298615868));
#113660=CARTESIAN_POINT('Ctrl Pts',(-1.16911722834105,3.52699760873882,
7.40832185973167));
#113661=CARTESIAN_POINT('Ctrl Pts',(-1.16504783117053,3.52633876186941,
7.40895947636584));
#113662=CARTESIAN_POINT('Ctrl Pts',(-1.160978434,3.525679915,7.40959709300001));
#113663=CARTESIAN_POINT('Ctrl Pts',(-0.754960220000001,3.459944422,7.47321437));
#113664=CARTESIAN_POINT('Ctrl Pts',(-0.344421845,3.395197164,7.492087399));
#113665=CARTESIAN_POINT('Ctrl Pts',(-1.36439911743497,3.52699760873882,
7.12046195559663));
#113666=CARTESIAN_POINT('Ctrl Pts',(-1.36048769671748,3.52633876186941,
7.12120699579831));
#113667=CARTESIAN_POINT('Ctrl Pts',(-1.356576276,3.525679915,7.121952036));
#113668=CARTESIAN_POINT('Ctrl Pts',(-0.966319934,3.459944422,7.196287344));
#113669=CARTESIAN_POINT('Ctrl Pts',(-0.570277963,3.395197164,7.227536444));
#113670=CARTESIAN_POINT('',(-0.596501776703425,3.43511457442473,7.47624139567237));
#113671=CARTESIAN_POINT('',(-1.16097843672315,3.52567991457199,7.40959709383369));
#113672=CARTESIAN_POINT('Origin',(0.0448629934745826,3.62494886961495,-0.183552747796982));
#113673=CARTESIAN_POINT('',(-1.25877736262446,3.52567991373767,7.26577456317908));
#113674=CARTESIAN_POINT('Ctrl Pts',(-0.596501780179129,3.43511457412329,
7.47624139542084));
#113675=CARTESIAN_POINT('Ctrl Pts',(-0.592954403265114,3.42888807477894,
7.4346863736556));
#113676=CARTESIAN_POINT('Ctrl Pts',(-0.589386786366554,3.42251694825873,
7.39313242858002));
#113677=CARTESIAN_POINT('Ctrl Pts',(-0.582214640223985,3.40947716052633,
7.31011921060845));
#113678=CARTESIAN_POINT('Ctrl Pts',(-0.578606272435709,3.4028015174756,
7.26861546467834));
#113679=CARTESIAN_POINT('Ctrl Pts',(-0.574977340862851,3.39596551404509,
7.22716410908228));
#113680=CARTESIAN_POINT('Ctrl Pts',(-2.426773305,3.395189501,7.096532345));
#113681=CARTESIAN_POINT('Ctrl Pts',(-2.041496927,3.460370723,7.228283796));
#113682=CARTESIAN_POINT('Ctrl Pts',(-1.644221332,3.525679915,7.317549878));
#113683=CARTESIAN_POINT('Ctrl Pts',(-2.119643019,3.395189501,6.93322533));
#113684=CARTESIAN_POINT('Ctrl Pts',(-1.743232708,3.460370723,7.048302433));
#113685=CARTESIAN_POINT('Ctrl Pts',(-1.356576276,3.525679915,7.121952036));
#113686=CARTESIAN_POINT('',(-1.64422134204873,3.52567991637276,7.31754987448137));
#113687=CARTESIAN_POINT('',(-1.50039881645216,3.52567991706905,7.21975095441222));
#113688=CARTESIAN_POINT('',(-2.18972679882163,3.43511457319675,7.17322077734424));
#113689=CARTESIAN_POINT('Origin',(0.0491103654982606,3.48214117966952,-0.186710050349461));
#113690=CARTESIAN_POINT('Ctrl Pts',(-2.11516133959162,3.39596551405412,
6.934593896648));
#113691=CARTESIAN_POINT('Ctrl Pts',(-2.12761629753411,3.40280154624219,
6.97429619650466));
#113692=CARTESIAN_POINT('Ctrl Pts',(-2.14006244103257,3.4094772188388,7.01405410403077));
#113693=CARTESIAN_POINT('Ctrl Pts',(-2.16491218325618,3.42251694822848,
7.09358436376503));
#113694=CARTESIAN_POINT('Ctrl Pts',(-2.17732926107205,3.42888807475033,
7.13339986851063));
#113695=CARTESIAN_POINT('Ctrl Pts',(-2.18972680351047,3.43511457408882,
7.17322077574496));
#113696=CARTESIAN_POINT('Ctrl Pts',(-2.73435412840025,3.52699760873882,
6.98379376576679));
#113697=CARTESIAN_POINT('Ctrl Pts',(-2.73051694020013,3.52633876186941,
6.98529127538339));
#113698=CARTESIAN_POINT('Ctrl Pts',(-2.726679752,3.525679915,6.986788785));
#113699=CARTESIAN_POINT('Ctrl Pts',(-2.343829852,3.459944422,7.13620064));
#113700=CARTESIAN_POINT('Ctrl Pts',(-1.94694678,3.395197164,7.242886043));
#113701=CARTESIAN_POINT('Ctrl Pts',(-2.86318906447492,3.52699760873882,
6.66068403319031));
#113702=CARTESIAN_POINT('Ctrl Pts',(-2.85952925223746,3.52633876186941,
6.66225249459515));
#113703=CARTESIAN_POINT('Ctrl Pts',(-2.85586944,3.525679915,6.663820956));
#113704=CARTESIAN_POINT('Ctrl Pts',(-2.49071697,3.459944422,6.820311923));
#113705=CARTESIAN_POINT('Ctrl Pts',(-2.110651872,3.395197164,6.935967753));
#113706=CARTESIAN_POINT('',(-2.72667975481357,3.52567991457199,6.98678878525083));
#113707=CARTESIAN_POINT('Origin',(0.0832725405001064,3.6249488517541,-0.16961717234676));
#113708=CARTESIAN_POINT('',(-2.7912746031623,3.52567991373766,6.82530486757091));
#113709=CARTESIAN_POINT('Origin',(2.41451823812522E-13,3.61749373599956,
-9.03357250114922E-13));
#113710=CARTESIAN_POINT('',(-2.19122982986197,3.61640598740785,7.17276179905093));
#113711=CARTESIAN_POINT('Origin',(0.0575818226972896,3.62499778718194,-0.183734944048718));
#113712=CARTESIAN_POINT('Origin',(0.0761123372709183,3.48215430157035,-0.17577726192358));
#113713=CARTESIAN_POINT('Ctrl Pts',(-3.895581376,3.395189501,6.408934837));
#113714=CARTESIAN_POINT('Ctrl Pts',(-3.547635213,3.460370723,6.620429044));
#113715=CARTESIAN_POINT('Ctrl Pts',(-3.178837269,3.525679915,6.793010644));
#113716=CARTESIAN_POINT('Ctrl Pts',(-3.560525444,3.395189501,6.315469782));
#113717=CARTESIAN_POINT('Ctrl Pts',(-3.217653573,3.460370723,6.508773536));
#113718=CARTESIAN_POINT('Ctrl Pts',(-2.85586944,3.525679915,6.663820956));
#113719=CARTESIAN_POINT('',(-3.17883727810971,3.52567991637269,6.79301063840168));
#113720=CARTESIAN_POINT('',(-3.01735336610406,3.52567991706893,6.72841579479618));
#113721=CARTESIAN_POINT('',(-3.68056263161433,3.43511457320845,6.53478832800663));
#113722=CARTESIAN_POINT('Origin',(0.0880994187286996,3.4821411487701,-0.171787782088027));
#113723=CARTESIAN_POINT('Ctrl Pts',(-3.55644274523096,3.39596551401258,
6.31776978074831));
#113724=CARTESIAN_POINT('Ctrl Pts',(-3.57714133398142,3.40280154619979,
6.35386641498873));
#113725=CARTESIAN_POINT('Ctrl Pts',(-3.59784326871524,3.40947721887761,
6.39001925214229));
#113726=CARTESIAN_POINT('Ctrl Pts',(-3.63920869283814,3.42251694825907,
6.46234817839716));
#113727=CARTESIAN_POINT('Ctrl Pts',(-3.65989462299297,3.428888074784,6.4985635140514));
#113728=CARTESIAN_POINT('Ctrl Pts',(-3.68056263589092,3.43511457412385,
6.53478832540929));
#113729=CARTESIAN_POINT('Ctrl Pts',(-4.17173566914475,3.52699760873882,
6.23271123756692));
#113730=CARTESIAN_POINT('Ctrl Pts',(-4.16831011257238,3.52633876186941,
6.23499861828346));
#113731=CARTESIAN_POINT('Ctrl Pts',(-4.164884556,3.525679915,6.237285999));
#113732=CARTESIAN_POINT('Ctrl Pts',(-3.823104606,3.459944422,6.4655061));
#113733=CARTESIAN_POINT('Ctrl Pts',(-3.458434647,3.395197164,6.655015386));
#113734=CARTESIAN_POINT('Ctrl Pts',(-4.22809947406292,3.52699760873882,
5.88945992881435));
#113735=CARTESIAN_POINT('Ctrl Pts',(-4.22486239903146,3.52633876186941,
5.89177847190718));
#113736=CARTESIAN_POINT('Ctrl Pts',(-4.221625324,3.525679915,5.894097015));
#113737=CARTESIAN_POINT('Ctrl Pts',(-3.898650847,3.459944422,6.125426297));
#113738=CARTESIAN_POINT('Ctrl Pts',(-3.552334045,3.395197164,6.32008092));
#113739=CARTESIAN_POINT('',(-4.16488455880619,3.52567991457199,6.23728599863403));
#113740=CARTESIAN_POINT('Origin',(0.117788269120822,3.62494884602207,-0.147750345564207));
#113741=CARTESIAN_POINT('',(-4.19325494636514,3.52567991373767,6.06569150259974));
#113742=CARTESIAN_POINT('Origin',(4.6447221069279E-13,3.61749373599978,
-9.05091973590899E-13));
#113743=CARTESIAN_POINT('',(-3.68193185568054,3.61640598737383,6.5340169729667));
#113744=CARTESIAN_POINT('Origin',(0.0957330761232028,3.62499780219289,-0.16706076477176));
#113745=CARTESIAN_POINT('Origin',(0.112119826861367,3.48215433084305,-0.155305859871593));
#113746=CARTESIAN_POINT('Ctrl Pts',(-5.182236391,3.395189501,5.421662659));
#113747=CARTESIAN_POINT('Ctrl Pts',(-4.887890019,3.460370723,5.703010389));
#113748=CARTESIAN_POINT('Ctrl Pts',(-4.564814309,3.525679915,5.950837783));
#113749=CARTESIAN_POINT('Ctrl Pts',(-4.83492165700001,3.395189501,5.402409886));
#113750=CARTESIAN_POINT('Ctrl Pts',(-4.541620533,3.460370723,5.664901623));
#113751=CARTESIAN_POINT('Ctrl Pts',(-4.221625324,3.525679915,5.894097015));
#113752=CARTESIAN_POINT('',(-4.56481431668058,3.52567991637268,5.95083777557618));
#113753=CARTESIAN_POINT('',(-4.39321982671409,3.52567991706893,5.92246739142331));
#113754=CARTESIAN_POINT('',(-4.99929944581776,3.43511457319354,5.59079643925668));
#113755=CARTESIAN_POINT('Origin',(0.122968880900439,3.48214118309511,-0.148832566926366));
#113756=CARTESIAN_POINT('Ctrl Pts',(-4.83142884122636,3.39596551396059,
5.40553377138989));
#113757=CARTESIAN_POINT('Ctrl Pts',(-4.8594032178137,3.40280154614786,5.43633690171973));
#113758=CARTESIAN_POINT('Ctrl Pts',(-4.88739294392432,3.40947721879129,
5.46719420151078));
#113759=CARTESIAN_POINT('Ctrl Pts',(-4.94333984841411,3.42251694818979,
5.5289397744007));
#113760=CARTESIAN_POINT('Ctrl Pts',(-4.97132737958918,3.42888807472649,
5.55986155220594));
#113761=CARTESIAN_POINT('Ctrl Pts',(-4.99929944939275,3.43511457407926,
5.59079643584581));
#113762=CARTESIAN_POINT('Ctrl Pts',(-5.42801715776659,3.53021247069526,
5.17641922555657));
#113763=CARTESIAN_POINT('Ctrl Pts',(-5.41819957354462,3.52794619284766,
5.1866364165488));
#113764=CARTESIAN_POINT('Ctrl Pts',(-5.40838198932263,3.525679915,5.19685360754093));
#113765=CARTESIAN_POINT('Ctrl Pts',(-5.1236138442468,3.459944422,5.49321271798337));
#113766=CARTESIAN_POINT('Ctrl Pts',(-4.80816917351001,3.395197164,5.75668240936443));
#113767=CARTESIAN_POINT('Ctrl Pts',(-5.40830271729218,3.53021247069526,
4.82840678376583));
#113768=CARTESIAN_POINT('Ctrl Pts',(-5.39914270864615,3.52794619284766,
4.83858921588293));
#113769=CARTESIAN_POINT('Ctrl Pts',(-5.3899827,3.525679915,4.848771648));
#113770=CARTESIAN_POINT('Ctrl Pts',(-5.124288145,3.459944422,5.144122545));
#113771=CARTESIAN_POINT('Ctrl Pts',(-4.827913027,3.395197164,5.408674126));
#113772=CARTESIAN_POINT('',(-5.40834399215434,3.52567991457842,5.19613464520341));
#113773=CARTESIAN_POINT('Origin',(0.146796449455316,3.62494884986666,-0.118975073921826));
#113774=CARTESIAN_POINT('',(-5.3991633482704,3.52567991373767,5.02245314433429));
#113775=CARTESIAN_POINT('Origin',(1.20129600711394E-13,3.61749373600033,
-1.42681005899092E-13));
#113776=CARTESIAN_POINT('',(-5.00047084026899,3.61640598737486,5.58974877539373));
#113777=CARTESIAN_POINT('Origin',(0.129407994724612,3.62499781851073,-0.142575166282169));
#113778=CARTESIAN_POINT('Origin',(0.142884588065562,3.48215430997448,-0.127572317519105));
#113779=CARTESIAN_POINT('Ctrl Pts',(-6.226575793,3.395189501,4.180879561));
#113780=CARTESIAN_POINT('Ctrl Pts',(-5.99959252,3.460370723,4.518925306));
#113781=CARTESIAN_POINT('Ctrl Pts',(-5.737345705,3.525679915,4.830410362));
#113782=CARTESIAN_POINT('Ctrl Pts',(-5.88324230700001,3.395189501,4.236739308));
#113783=CARTESIAN_POINT('Ctrl Pts',(-5.653226364,3.460370723,4.556145206));
#113784=CARTESIAN_POINT('Ctrl Pts',(-5.3899827,3.525679915,4.848771648));
#113785=CARTESIAN_POINT('',(-5.73734571087744,3.52567991637269,4.83041035311642));
#113786=CARTESIAN_POINT('',(-5.56366421084652,3.52567991706893,4.83959099540472));
#113787=CARTESIAN_POINT('',(-6.08427457474554,3.43511457319035,4.38538512284339));
#113788=CARTESIAN_POINT('Origin',(0.15208886535066,3.48214117880472,-0.118918515677711));
#113789=CARTESIAN_POINT('Ctrl Pts',(-5.88050269398345,3.39596551395666,
4.24054101087128));
#113790=CARTESIAN_POINT('Ctrl Pts',(-5.91444480768252,3.40280154613216,
4.26461031711559));
#113791=CARTESIAN_POINT('Ctrl Pts',(-5.94841355696679,3.40947721878168,
4.28872922669257));
#113792=CARTESIAN_POINT('Ctrl Pts',(-6.01632592701229,3.42251694817642,
4.33700429172433));
#113793=CARTESIAN_POINT('Ctrl Pts',(-6.05030639351071,3.42888807471328,
4.36118664364647));
#113794=CARTESIAN_POINT('Ctrl Pts',(-6.08427457749733,3.43511457406995,
4.38538511875428));
#113795=CARTESIAN_POINT('Ctrl Pts',(-6.41389025267975,3.53021247057256,
3.88853418349163));
#113796=CARTESIAN_POINT('Ctrl Pts',(-6.40649859234271,3.52794619278631,
3.90062299231468));
#113797=CARTESIAN_POINT('Ctrl Pts',(-6.39910693200571,3.525679915,3.91271180113778));
#113798=CARTESIAN_POINT('Ctrl Pts',(-6.18470495565505,3.459944422,4.26335893388248));
#113799=CARTESIAN_POINT('Ctrl Pts',(-5.93327340240695,3.395197164,4.58848012970719));
#113800=CARTESIAN_POINT('Ctrl Pts',(-6.31982433736954,3.53021247057255,
3.5528961003417));
#113801=CARTESIAN_POINT('Ctrl Pts',(-6.31306740668471,3.52794619278631,
3.56480960367085));
#113802=CARTESIAN_POINT('Ctrl Pts',(-6.306310476,3.525679915,3.576723107));
#113803=CARTESIAN_POINT('Ctrl Pts',(-6.110319423,3.459944422,3.922285341));
#113804=CARTESIAN_POINT('Ctrl Pts',(-5.877744161,3.395197164,4.244363742));
#113805=CARTESIAN_POINT('',(-6.39891526807721,3.52567991503086,3.91201781576554));
#113806=CARTESIAN_POINT('Origin',(0.168940701023456,3.62494882504361,-0.0846367114639096));
#113807=CARTESIAN_POINT('',(-6.35261287342922,3.52567991373767,3.74437045883377));
#113808=CARTESIAN_POINT('Origin',(6.48352899146332E-13,3.61749373600089,
-4.36716635077161E-13));
#113809=CARTESIAN_POINT('',(-6.08519336544766,3.61640598741484,4.38411013764515));
#113810=CARTESIAN_POINT('Origin',(0.157031971607143,3.62499783912985,-0.111422941150182));
#113811=CARTESIAN_POINT('Origin',(0.166968276007746,3.48215435135676,-0.0938737837871401));
#113812=CARTESIAN_POINT('Ctrl Pts',(-6.97976743,3.395189501,2.744603181));
#113813=CARTESIAN_POINT('Ctrl Pts',(-6.830760744,3.460370723,3.123540298));
#113814=CARTESIAN_POINT('Ctrl Pts',(-6.641605193,3.525679915,3.48411832));
#113815=CARTESIAN_POINT('Ctrl Pts',(-6.656469085,3.395189501,2.872963509));
#113816=CARTESIAN_POINT('Ctrl Pts',(-6.50049361399999,3.460370723,3.234348502));
#113817=CARTESIAN_POINT('Ctrl Pts',(-6.306310476,3.525679915,3.576723107));
#113818=CARTESIAN_POINT('',(-6.64160519682503,3.52567991637272,3.48411831007144));
#113819=CARTESIAN_POINT('',(-6.47395784058869,3.52567991706893,3.5304207023348));
#113820=CARTESIAN_POINT('',(-6.8847557866728,3.43511457320295,2.97491807196946));
#113821=CARTESIAN_POINT('Origin',(0.174096893675357,3.48214111904205,-0.0834435547269661));
#113822=CARTESIAN_POINT('Ctrl Pts',(-6.65461077687043,3.3959655139869,2.87726526591025));
#113823=CARTESIAN_POINT('Ctrl Pts',(-6.69293353213603,3.40280154617958,
2.89347529396363));
#113824=CARTESIAN_POINT('Ctrl Pts',(-6.73129296357907,3.40947721884582,
2.90972803983227));
#113825=CARTESIAN_POINT('Ctrl Pts',(-6.80799529206524,3.42251694823562,
2.94227530850979));
#113826=CARTESIAN_POINT('Ctrl Pts',(-6.84637980495893,3.42888807476465,
2.9585874946168));
#113827=CARTESIAN_POINT('Ctrl Pts',(-6.88475578849858,3.43511457410741,
2.97491806733411));
#113828=CARTESIAN_POINT('Ctrl Pts',(-7.09985696847863,3.53021247071098,
2.41882560302897));
#113829=CARTESIAN_POINT('Ctrl Pts',(-7.09523685747579,3.52794619285552,
2.4322207711079));
#113830=CARTESIAN_POINT('Ctrl Pts',(-7.09061674647308,3.525679915,2.44561593918682));
#113831=CARTESIAN_POINT('Ctrl Pts',(-6.95660613795883,3.459944422,2.8341552241401));
#113832=CARTESIAN_POINT('Ctrl Pts',(-6.78094436032421,3.395197164,3.205725619537));
#113833=CARTESIAN_POINT('Ctrl Pts',(-6.93583799490026,3.53021247071098,
2.11125594298556));
#113834=CARTESIAN_POINT('Ctrl Pts',(-6.93180008845007,3.52794619285552,
2.12434345599278));
#113835=CARTESIAN_POINT('Ctrl Pts',(-6.927762182,3.525679915,2.137430969));
#113836=CARTESIAN_POINT('Ctrl Pts',(-6.810638957,3.459944422,2.517046433));
#113837=CARTESIAN_POINT('Ctrl Pts',(-6.652738511,3.395197164,2.881591627));
#113838=CARTESIAN_POINT('',(-7.09028037716511,3.52567991503086,2.44497938085858));
#113839=CARTESIAN_POINT('Origin',(0.183185218093685,3.62494884872823,-0.0463406396412325));
#113840=CARTESIAN_POINT('',(-7.00902128040432,3.52567991373767,2.29120517214497));
#113841=CARTESIAN_POINT('Origin',(-4.28043017697277E-13,3.61749373599989,
1.12540185503995E-13));
#113842=CARTESIAN_POINT('',(-6.88537901244733,3.61640598739985,2.97347538228457));
#113843=CARTESIAN_POINT('Origin',(0.177313480335798,3.6249978219611,-0.0750607932934111));
#113844=CARTESIAN_POINT('Origin',(0.183244805852569,3.48215435875214,-0.0557858511365902));
#113845=CARTESIAN_POINT('Ctrl Pts',(-7.4065929,3.395189501,1.179992206));
#113846=CARTESIAN_POINT('Ctrl Pts',(-7.342530186,3.460370723,1.582102018));
#113847=CARTESIAN_POINT('Ctrl Pts',(-7.235310603,3.525679915,1.974912778));
#113848=CARTESIAN_POINT('Ctrl Pts',(-7.118446767,3.395189501,1.374851129));
#113849=CARTESIAN_POINT('Ctrl Pts',(-7.043805007,3.460370723,1.761317258));
#113850=CARTESIAN_POINT('Ctrl Pts',(-6.927762182,3.525679915,2.137430969));
#113851=CARTESIAN_POINT('',(-7.23531060460634,3.52567991637269,1.97491276746508));
#113852=CARTESIAN_POINT('',(-7.08153639604615,3.52567991706893,2.05617186128694));
#113853=CARTESIAN_POINT('',(-7.36331346968431,3.43511457321339,1.42534715830193));
#113854=CARTESIAN_POINT('Origin',(0.187964634940831,3.48214115787911,-0.0440670445990793));
#113855=CARTESIAN_POINT('Ctrl Pts',(-7.1175566558214,3.39596551405672,1.37945179479932));
#113856=CARTESIAN_POINT('Ctrl Pts',(-7.15846812332044,3.40280154624432,
1.38704458171414));
#113857=CARTESIAN_POINT('Ctrl Pts',(-7.19942459238286,3.40947721888432,
1.39467120346668));
#113858=CARTESIAN_POINT('Ctrl Pts',(-7.2813303637261,3.42251694827523,1.40996880173583));
#113859=CARTESIAN_POINT('Ctrl Pts',(-7.32232410578099,3.42888807479856,
1.41764808237601));
#113860=CARTESIAN_POINT('Ctrl Pts',(-7.36331347047552,3.43511457413836,
1.42534715334153));
#113861=CARTESIAN_POINT('Ctrl Pts',(-7.45384226280907,3.53021247049811,
0.836015428641415));
#113862=CARTESIAN_POINT('Ctrl Pts',(-7.4522097326595,3.52794619274909,0.850090611749254));
#113863=CARTESIAN_POINT('Ctrl Pts',(-7.4505772025098,3.525679915,0.864165794857096));
#113864=CARTESIAN_POINT('Ctrl Pts',(-7.40322414780592,3.459944422,1.27242956615997));
#113865=CARTESIAN_POINT('Ctrl Pts',(-7.31154589717169,3.395197164,1.673074941636));
#113866=CARTESIAN_POINT('Ctrl Pts',(-7.22753957586448,3.53021247049811,
0.570895806820382));
#113867=CARTESIAN_POINT('Ctrl Pts',(-7.22640950193228,3.52794619274909,
0.584545370910196));
#113868=CARTESIAN_POINT('Ctrl Pts',(-7.225279428,3.525679915,0.598194935));
#113869=CARTESIAN_POINT('Ctrl Pts',(-7.192500583,3.459944422,0.994113231));
#113870=CARTESIAN_POINT('Ctrl Pts',(-7.116658202,3.395197164,1.38407949));
#113871=CARTESIAN_POINT('',(-7.45011185602574,3.52567991503086,0.863616428380273));
#113872=CARTESIAN_POINT('Origin',(0.188864586681895,3.6249488631317,-0.00587786011865737));
#113873=CARTESIAN_POINT('',(-7.337695642267,3.52567991373765,0.730905678799971));
#113874=CARTESIAN_POINT('Origin',(-4.90493062832442E-13,3.61749373599933,
2.90566182226115E-14));
#113875=CARTESIAN_POINT('',(-7.36361198950021,3.61640598739899,1.423804222735));
#113876=CARTESIAN_POINT('Origin',(0.189303689547513,3.62499782970624,-0.0351887269185508));
#113877=CARTESIAN_POINT('Origin',(0.190953314121111,3.48215429853827,-0.0150894401907962));
#113878=CARTESIAN_POINT('Ctrl Pts',(-7.487094318,3.395189501,-0.439793892));
#113879=CARTESIAN_POINT('Ctrl Pts',(-7.510971078,3.460370723,-0.033313594));
#113880=CARTESIAN_POINT('Ctrl Pts',(-7.490700931,3.525679915,0.373362509));
#113881=CARTESIAN_POINT('Ctrl Pts',(-7.24757379,3.395189501,-0.187547762));
#113882=CARTESIAN_POINT('Ctrl Pts',(-7.25775590700001,3.460370723,0.205928776));
#113883=CARTESIAN_POINT('Ctrl Pts',(-7.225279428,3.525679915,0.598194935));
#113884=CARTESIAN_POINT('',(-7.49070093030407,3.52567991637267,0.373362498359974));
#113885=CARTESIAN_POINT('',(-7.35799018033778,3.52567991706892,0.485778709310209));
#113886=CARTESIAN_POINT('',(-7.49757079857549,3.43511457319164,-0.190871404225564));
#113887=CARTESIAN_POINT('Origin',(0.193043078825646,3.48214121353905,-0.00262994821670431));
#113888=CARTESIAN_POINT('Ctrl Pts',(-7.24769349603453,3.39596551408267,
-0.182863309194341));
#113889=CARTESIAN_POINT('Ctrl Pts',(-7.28928070096139,3.4028015462638,-0.184242793530343));
#113890=CARTESIAN_POINT('Ctrl Pts',(-7.3309191285908,3.40947721885932,-0.185598908098326));
#113891=CARTESIAN_POINT('Ctrl Pts',(-7.41419852000121,3.42251694823117,
-0.188266278868783));
#113892=CARTESIAN_POINT('Ctrl Pts',(-7.45588466949589,3.42888807474393,
-0.189578978324019));
#113893=CARTESIAN_POINT('Ctrl Pts',(-7.4975707982911,3.43511457407353,-0.190871409149947));
#113894=CARTESIAN_POINT('Ctrl Pts',(-7.46075164741015,3.52699760873882,
-0.766324157850277));
#113895=CARTESIAN_POINT('Ctrl Pts',(-7.46116801620508,3.52633876186941,
-0.762226208925139));
#113896=CARTESIAN_POINT('Ctrl Pts',(-7.461584385,3.525679915,-0.75812826));
#113897=CARTESIAN_POINT('Ctrl Pts',(-7.503126979,3.459944422,-0.349261336));
#113898=CARTESIAN_POINT('Ctrl Pts',(-7.49974623,3.395197164,0.061696714));
#113899=CARTESIAN_POINT('Ctrl Pts',(-7.18388626403411,3.52699760873882,
-0.9769040688728));
#113900=CARTESIAN_POINT('Ctrl Pts',(-7.18441845151706,3.52633876186941,
-0.9729580489364));
#113901=CARTESIAN_POINT('Ctrl Pts',(-7.184950639,3.525679915,-0.969012029));
#113902=CARTESIAN_POINT('Ctrl Pts',(-7.238048875,3.459944422,-0.5753036));
#113903=CARTESIAN_POINT('Ctrl Pts',(-7.247810865,3.395197164,-0.178150666));
#113904=CARTESIAN_POINT('',(-7.46158438599956,3.52567991457199,-0.758128262633195));
#113905=CARTESIAN_POINT('Origin',(0.185712522317807,3.62494885578236,0.0348598660157013));
#113906=CARTESIAN_POINT('',(-7.32326751109379,3.52567991373765,-0.863570152184889));
#113907=CARTESIAN_POINT('Origin',(-1.25507243486922E-12,3.617493736,5.41830035699631E-14));
#113908=CARTESIAN_POINT('',(-7.49753065353308,3.61640598744037,-0.192442439414313));
#113909=CARTESIAN_POINT('Origin',(0.19244229328369,3.62499780846281,0.00632866299894386));
#113910=CARTESIAN_POINT('Origin',(0.189732559278504,3.48215432117043,0.0263126537729071));
#113911=CARTESIAN_POINT('Ctrl Pts',(-7.217507527,3.395189501,-2.039015717));
#113912=CARTESIAN_POINT('Ctrl Pts',(-7.32820731,3.460370723,-1.6471715));
#113913=CARTESIAN_POINT('Ctrl Pts',(-7.39583440900001,3.525679915,-1.245645776));
#113914=CARTESIAN_POINT('Ctrl Pts',(-7.037812317,3.395189501,-1.741177127));
#113915=CARTESIAN_POINT('Ctrl Pts',(-7.132342206,3.460370723,-1.359088706));
#113916=CARTESIAN_POINT('Ctrl Pts',(-7.184950639,3.525679915,-0.969012029));
#113917=CARTESIAN_POINT('',(-7.39583440602979,3.52567991637266,-1.2456457862268));
#113918=CARTESIAN_POINT('',(-7.29039252209027,3.52567991706892,-1.10732891507321));
#113919=CARTESIAN_POINT('',(-7.28125005028088,3.43511457321144,-1.7981650321231));
#113920=CARTESIAN_POINT('Origin',(0.18909539415706,3.4821411876723,0.0389301375708813));
#113921=CARTESIAN_POINT('Ctrl Pts',(-7.03893624352272,3.39596551401659,
-1.73662792835121));
#113922=CARTESIAN_POINT('Ctrl Pts',(-7.07925461423005,3.40280154619732,
-1.74691518075888));
#113923=CARTESIAN_POINT('Ctrl Pts',(-7.11962803441265,3.40947721887202,
-1.75719062129386));
#113924=CARTESIAN_POINT('Ctrl Pts',(-7.20038699401208,3.42251694825527,
-1.77769823777738));
#113925=CARTESIAN_POINT('Ctrl Pts',(-7.24081635299754,3.42888807478671,
-1.78794153696337));
#113926=CARTESIAN_POINT('Ctrl Pts',(-7.28125004891864,3.43511457413287,
-1.7981650369495));
#113927=CARTESIAN_POINT('Ctrl Pts',(-7.121586378581,3.52699760873882,-2.3522489903306));
#113928=CARTESIAN_POINT('Ctrl Pts',(-7.12287395079049,3.52633876186941,
-2.3483363561653));
#113929=CARTESIAN_POINT('Ctrl Pts',(-7.124161523,3.525679915,-2.344423722));
#113930=CARTESIAN_POINT('Ctrl Pts',(-7.252627177,3.459944422,-1.95404631));
#113931=CARTESIAN_POINT('Ctrl Pts',(-7.337669301,3.395197164,-1.551969469));
#113932=CARTESIAN_POINT('Ctrl Pts',(-6.80592549724464,3.52699760873882,
-2.49838778720026));
#113933=CARTESIAN_POINT('Ctrl Pts',(-6.80729352012233,3.52633876186941,
-2.49464842760013));
#113934=CARTESIAN_POINT('Ctrl Pts',(-6.808661543,3.525679915,-2.490909068));
#113935=CARTESIAN_POINT('Ctrl Pts',(-6.945154046,3.459944422,-2.117819875));
#113936=CARTESIAN_POINT('Ctrl Pts',(-7.040063948,3.395197164,-1.732050695));
#113937=CARTESIAN_POINT('',(-7.12416152340778,3.52567991457199,-2.34442372478951));
#113938=CARTESIAN_POINT('Origin',(0.17387673225741,3.62494889075051,0.0739675469353931));
#113939=CARTESIAN_POINT('',(-6.96641153046295,3.52567991373765,-2.41766640231041));
#113940=CARTESIAN_POINT('Origin',(9.87057657830803E-13,3.61749373599967,
1.99384779520084E-13));
#113941=CARTESIAN_POINT('',(-7.28087311717066,3.61640598742399,-1.79969070725064));
#113942=CARTESIAN_POINT('Origin',(0.186582973251562,3.62499781993517,0.0475501875947812));
#113943=CARTESIAN_POINT('Origin',(0.179640094615405,3.48215430651884,0.0664843171575019));
#113944=CARTESIAN_POINT('Ctrl Pts',(-6.61043810600001,3.395189501,-3.542895433));
#113945=CARTESIAN_POINT('Ctrl Pts',(-6.802784713,3.460370723,-3.184009497));
#113946=CARTESIAN_POINT('Ctrl Pts',(-6.955146889,3.525679915,-2.806409048));
#113947=CARTESIAN_POINT('Ctrl Pts',(-6.498970563,3.395189501,-3.213390985));
#113948=CARTESIAN_POINT('Ctrl Pts',(-6.673428112,3.460370723,-2.860556712));
#113949=CARTESIAN_POINT('Ctrl Pts',(-6.808661543,3.525679915,-2.490909068));
#113950=CARTESIAN_POINT('',(-6.95514688390027,3.52567991637267,-2.80640905739783));
#113951=CARTESIAN_POINT('',(-6.88190421143205,3.52567991706892,-2.64865906986872));
#113952=CARTESIAN_POINT('',(-6.72446614188422,3.43511457320662,-3.32137846142375));
#113953=CARTESIAN_POINT('Origin',(0.176305530987173,3.48214118240383,0.0786698416026864));
#113954=CARTESIAN_POINT('Ctrl Pts',(-6.5010461556297,3.39596551395717,-3.20918975482681));
#113955=CARTESIAN_POINT('Ctrl Pts',(-6.5382102399609,3.40280150749901,-3.22790364916677));
#113956=CARTESIAN_POINT('Ctrl Pts',(-6.57543059806044,3.40947714036133,
-3.24661782840647));
#113957=CARTESIAN_POINT('Ctrl Pts',(-6.64989337480597,3.4225169482316,-3.28400700244851));
#113958=CARTESIAN_POINT('Ctrl Pts',(-6.68717551126765,3.42888807476634,
-3.30270193613753));
#113959=CARTESIAN_POINT('Ctrl Pts',(-6.72446613952633,3.4351145741185,-3.32137846582763));
#113960=CARTESIAN_POINT('Ctrl Pts',(-6.44942364563877,3.52699760873882,
-3.82818527497923));
#113961=CARTESIAN_POINT('Ctrl Pts',(-6.45152221581939,3.52633876186941,
-3.82464090598961));
#113962=CARTESIAN_POINT('Ctrl Pts',(-6.45362078600001,3.525679915,-3.821096537));
#113963=CARTESIAN_POINT('Ctrl Pts',(-6.66300258900001,3.459944422,-3.46746225));
#113964=CARTESIAN_POINT('Ctrl Pts',(-6.83249111,3.395197164,-3.093067285));
#113965=CARTESIAN_POINT('Ctrl Pts',(-6.10972721891902,3.52699760873882,
-3.90304966995008));
#113966=CARTESIAN_POINT('Ctrl Pts',(-6.11186710995951,3.52633876186941,
-3.89969181897504));
#113967=CARTESIAN_POINT('Ctrl Pts',(-6.114007001,3.525679915,-3.896333968));
#113968=CARTESIAN_POINT('Ctrl Pts',(-6.327511533,3.459944422,-3.561309246));
#113969=CARTESIAN_POINT('Ctrl Pts',(-6.503131465,3.395197164,-3.204961958));
#113970=CARTESIAN_POINT('',(-6.45362078579712,3.52567991457199,-3.82109653981316));
#113971=CARTESIAN_POINT('Origin',(0.153910590139191,3.62494886094461,0.109616489232645));
#113972=CARTESIAN_POINT('',(-6.28381388945075,3.52567991373765,-3.8587152590941));
#113973=CARTESIAN_POINT('Origin',(-4.33680868994202E-14,3.61749373599989,
-3.81639164714898E-14));
#113974=CARTESIAN_POINT('',(-6.72377004630369,3.61640598738303,-3.3227874378953));
#113975=CARTESIAN_POINT('Origin',(0.171998886139176,3.62499783308384,0.086548303390474));
#113976=CARTESIAN_POINT('Origin',(0.161148226261515,3.48215433566803,0.103547355812011));
#113977=CARTESIAN_POINT('Ctrl Pts',(-5.694271946,3.395189501,-4.881113296));
#113978=CARTESIAN_POINT('Ctrl Pts',(-5.959271464,3.460370723,-4.571966749));
#113979=CARTESIAN_POINT('Ctrl Pts',(-6.189244432,3.525679915,-4.235947753));
#113980=CARTESIAN_POINT('Ctrl Pts',(-5.656244168,3.395189501,-4.535350253));
#113981=CARTESIAN_POINT('Ctrl Pts',(-5.902471935,3.460370723,-4.228268264));
#113982=CARTESIAN_POINT('Ctrl Pts',(-6.114007001,3.525679915,-3.896333968));
#113983=CARTESIAN_POINT('',(-6.18924442501214,3.52567991637268,-4.2359477610336));
#113984=CARTESIAN_POINT('',(-6.15162570948743,3.52567991706892,-4.06614087110926));
#113985=CARTESIAN_POINT('',(-5.85325367059049,3.43511457319961,-4.68928792510928));
#113986=CARTESIAN_POINT('Origin',(0.155271798014792,3.48214117390607,0.114730992146767));
#113987=CARTESIAN_POINT('Ctrl Pts',(-5.65917437478212,3.39596551399065,
-4.53169343554281));
#113988=CARTESIAN_POINT('Ctrl Pts',(-5.6914466679652,3.40280151145959,-4.55795900404419));
#113989=CARTESIAN_POINT('Ctrl Pts',(-5.72377386047523,3.4094771483571,-4.58423694989676));
#113990=CARTESIAN_POINT('Ctrl Pts',(-5.78845813222718,3.42251694823204,
-4.63675924951398));
#113991=CARTESIAN_POINT('Ctrl Pts',(-5.82084977501639,3.42888807475903,
-4.66303166331845));
#113992=CARTESIAN_POINT('Ctrl Pts',(-5.85325366736076,3.43511457409759,
-4.68928792888226));
#113993=CARTESIAN_POINT('Ctrl Pts',(-5.47569303132712,3.52699760873882,
-5.12511987112299));
#113994=CARTESIAN_POINT('Ctrl Pts',(-5.47850447266356,3.52633876186941,
-5.1221094980615));
#113995=CARTESIAN_POINT('Ctrl Pts',(-5.481315914,3.525679915,-5.119099125));
#113996=CARTESIAN_POINT('Ctrl Pts',(-5.761823405,3.459944422,-4.818743509));
#113997=CARTESIAN_POINT('Ctrl Pts',(-6.007833229,3.395197164,-4.489536712));
#113998=CARTESIAN_POINT('Ctrl Pts',(-5.12784488643437,3.52699760873882,
-5.12520928693362));
#113999=CARTESIAN_POINT('Ctrl Pts',(-5.13065658671719,3.52633876186941,
-5.12238995396681));
#114000=CARTESIAN_POINT('Ctrl Pts',(-5.133468287,3.525679915,-5.119570621));
#114001=CARTESIAN_POINT('Ctrl Pts',(-5.41400161399999,3.459944422,-4.83827575400001));
#114002=CARTESIAN_POINT('Ctrl Pts',(-5.66211978200001,3.395197164,-4.528012762));
#114003=CARTESIAN_POINT('',(-5.48131591317618,3.52567991457198,-5.11909912771447));
#114004=CARTESIAN_POINT('Origin',(0.126747988885264,3.62494886090853,0.140139977388261));
#114005=CARTESIAN_POINT('',(-5.30739209512788,3.52567991373765,-5.11933487856947));
#114006=CARTESIAN_POINT('Origin',(-1.0698907038087E-12,3.61749373600011,
-7.5764047813287E-13));
#114007=CARTESIAN_POINT('',(-5.85227096105507,3.61640598736084,-4.69051432075499));
#114008=CARTESIAN_POINT('Origin',(0.149372346596961,3.62499785970808,0.121499565334746));
#114009=CARTESIAN_POINT('Origin',(0.135121027998427,3.48215431755388,0.135768561324429));
#114010=CARTESIAN_POINT('Ctrl Pts',(-4.511847958,3.395189501,-5.991095726));
#114011=CARTESIAN_POINT('Ctrl Pts',(-4.83710930400001,3.460370723,-5.746143917));
#114012=CARTESIAN_POINT('Ctrl Pts',(-5.133939783,3.525679915,-5.467418248));
#114013=CARTESIAN_POINT('Ctrl Pts',(-4.549038082,3.395189501,-5.645241583));
#114014=CARTESIAN_POINT('Ctrl Pts',(-4.855522731,3.460370723,-5.398270692));
#114015=CARTESIAN_POINT('Ctrl Pts',(-5.133468287,3.525679915,-5.119570621));
#114016=CARTESIAN_POINT('',(-5.13393977442977,3.52567991637268,-5.46741825438338));
#114017=CARTESIAN_POINT('',(-5.1337040258707,3.52567991706892,-5.29349444335373));
#114018=CARTESIAN_POINT('',(-4.70834956261549,3.43511457319619,-5.83793149756705));
#114019=CARTESIAN_POINT('Origin',(0.126977794753728,3.48214118365086,0.1454274058658));
#114020=CARTESIAN_POINT('Ctrl Pts',(-4.5526858901545,3.39596551408124,-5.64230016839406));
#114021=CARTESIAN_POINT('Ctrl Pts',(-4.57855748562481,3.40280154627411,
-5.67488941720374));
#114022=CARTESIAN_POINT('Ctrl Pts',(-4.6044800535483,3.40947721887663,-5.70750257674678));
#114023=CARTESIAN_POINT('Ctrl Pts',(-4.65636102058536,3.42251694824849,
-5.7727017880457));
#114024=CARTESIAN_POINT('Ctrl Pts',(-4.6823475723423,3.42888807476058,-5.80532321301078));
#114025=CARTESIAN_POINT('Ctrl Pts',(-4.70834955866205,3.43511457408713,
-5.83793150054941));
#114026=CARTESIAN_POINT('Ctrl Pts',(-4.23007233058158,3.53021247063215,
-6.19396273343257));
#114027=CARTESIAN_POINT('Ctrl Pts',(-4.24174323385752,3.5279461928161,-6.18592743858956));
#114028=CARTESIAN_POINT('Ctrl Pts',(-4.25341413713345,3.525679915,-6.17789214374671));
#114029=CARTESIAN_POINT('Ctrl Pts',(-4.59193952671718,3.459944422,-5.94482095355766));
#114030=CARTESIAN_POINT('Ctrl Pts',(-4.9029716747628,3.395197164,-5.67615643917439));
#114031=CARTESIAN_POINT('Ctrl Pts',(-3.88983386413708,3.53021247063215,
-6.11820585342734));
#114032=CARTESIAN_POINT('Ctrl Pts',(-3.90136408256857,3.5279461928161,-6.1108138482137));
#114033=CARTESIAN_POINT('Ctrl Pts',(-3.912894301,3.525679915,-6.103421843));
#114034=CARTESIAN_POINT('Ctrl Pts',(-4.247338996,3.459944422,-5.889009866));
#114035=CARTESIAN_POINT('Ctrl Pts',(-4.556353671,3.395197164,-5.639338722));
#114036=CARTESIAN_POINT('',(-4.25271079329089,3.52567991457841,-6.17773833197232));
#114037=CARTESIAN_POINT('Origin',(0.0936588060901228,3.6249488395768,0.164110744318613));
#114038=CARTESIAN_POINT('',(-4.0828025445562,3.52567991373765,-6.14058008928441));
#114039=CARTESIAN_POINT('Origin',(5.87637577487143E-13,3.61749373599967,
5.98045918343004E-13));
#114040=CARTESIAN_POINT('',(-4.70712619026899,3.61640598741786,-5.83891796682443));
#114041=CARTESIAN_POINT('Origin',(0.119761026413497,3.62499782828964,0.150769287755076));
#114042=CARTESIAN_POINT('Origin',(0.102775544221599,3.48215432461251,0.161641131742404));
#114043=CARTESIAN_POINT('Ctrl Pts',(-3.118454975,3.395189501,-6.820941179));
#114044=CARTESIAN_POINT('Ctrl Pts',(-3.488769289,3.460370723,-6.651637782));
#114045=CARTESIAN_POINT('Ctrl Pts',(-3.838577816,3.525679915,-6.443238343));
#114046=CARTESIAN_POINT('Ctrl Pts',(-3.229124031,3.395189501,-6.491167691));
#114047=CARTESIAN_POINT('Ctrl Pts',(-3.581534681,3.460370723,-6.315855982));
#114048=CARTESIAN_POINT('Ctrl Pts',(-3.912894301,3.525679915,-6.103421843));
#114049=CARTESIAN_POINT('',(-3.83857780625908,3.52567991637269,-6.44323834739284));
#114050=CARTESIAN_POINT('',(-3.87573604768084,3.52567991706892,-6.2733300996842));
#114051=CARTESIAN_POINT('',(-3.34328826263611,3.43511457320309,-6.71359988169517));
#114052=CARTESIAN_POINT('Origin',(0.092746564593766,3.48214115952456,0.169323927841567));
#114053=CARTESIAN_POINT('Ctrl Pts',(-3.23331887271315,3.39596551408552,
-6.48907921575685));
#114054=CARTESIAN_POINT('Ctrl Pts',(-3.25157987957208,3.40280154624054,
-6.52646817421398));
#114055=CARTESIAN_POINT('Ctrl Pts',(-3.2698855272556,3.40947721889246,-6.56389144238755));
#114056=CARTESIAN_POINT('Ctrl Pts',(-3.30653764307364,3.42251694824908,
-6.63871920666186));
#114057=CARTESIAN_POINT('Ctrl Pts',(-3.32490400166039,3.42888807476787,
-6.67616430135315));
#114058=CARTESIAN_POINT('Ctrl Pts',(-3.3432882581064,3.43511457410804,-6.71359988376915));
#114059=CARTESIAN_POINT('Ctrl Pts',(-2.79965669493376,3.53021247058043,
-6.9584918377492));
#114060=CARTESIAN_POINT('Ctrl Pts',(-2.81278208969923,3.52794619279024,
-6.95315330291087));
#114061=CARTESIAN_POINT('Ctrl Pts',(-2.82590748446468,3.525679915,-6.94781476807245));
#114062=CARTESIAN_POINT('Ctrl Pts',(-3.20662175499411,3.459944422,-6.79296560482672));
#114063=CARTESIAN_POINT('Ctrl Pts',(-3.56813707398946,3.395197164,-6.59744503542102));
#114064=CARTESIAN_POINT('Ctrl Pts',(-2.48365830439741,3.53021247058043,
-6.81136489805072));
#114065=CARTESIAN_POINT('Ctrl Pts',(-2.49650801519868,3.52794619279024,
-6.80662437002537));
#114066=CARTESIAN_POINT('Ctrl Pts',(-2.509357726,3.525679915,-6.801883842));
#114067=CARTESIAN_POINT('Ctrl Pts',(-2.882075527,3.459944422,-6.664380422));
#114068=CARTESIAN_POINT('Ctrl Pts',(-3.237537527,3.395197164,-6.486975471));
#114069=CARTESIAN_POINT('',(-2.82525364939956,3.52567991457841,-6.94751335419762));
#114070=CARTESIAN_POINT('Origin',(0.0561901832822947,3.62494885801425,0.18040787680095));
#114071=CARTESIAN_POINT('',(-2.66730568478583,3.52567991373765,-6.87469859929902));
#114072=CARTESIAN_POINT('Origin',(2.77555756156289E-13,3.61749373600011,
4.81385764583564E-13));
#114073=CARTESIAN_POINT('',(-3.34188142941271,3.61640598742155,-6.71430029892485));
#114074=CARTESIAN_POINT('Origin',(0.084550252916929,3.62499779247149,0.172989665277615));
#114075=CARTESIAN_POINT('Origin',(0.0656247367693708,3.48215435022122,0.179955946192594));
#114076=CARTESIAN_POINT('Ctrl Pts',(-1.579246502,3.395189501,-7.331847004));
#114077=CARTESIAN_POINT('Ctrl Pts',(-1.9772983,3.460370723,-7.24610845700001));
#114078=CARTESIAN_POINT('Ctrl Pts',(-2.363728217,3.525679915,-7.117779774));
#114079=CARTESIAN_POINT('Ctrl Pts',(-1.75821973,3.395189501,-7.033574012));
#114080=CARTESIAN_POINT('Ctrl Pts',(-2.14007805,3.460370723,-6.938118866));
#114081=CARTESIAN_POINT('Ctrl Pts',(-2.509357726,3.525679915,-6.801883842));
#114082=CARTESIAN_POINT('',(-2.36372820654411,3.52567991637267,-7.11777977618988));
#114083=CARTESIAN_POINT('',(-2.43654295949688,3.52567991706892,-6.95983181220213));
#114084=CARTESIAN_POINT('',(-1.82189851888345,3.43511457319319,-7.2753477966558));
#114085=CARTESIAN_POINT('Origin',(0.0541785171027137,3.48214119170741,0.185302837168355));
#114086=CARTESIAN_POINT('Ctrl Pts',(-1.76276545876253,3.39596551404128,
-7.03243613129102));
#114087=CARTESIAN_POINT('Ctrl Pts',(-1.77256201256658,3.40280154620986,
-7.07287653324826));
#114088=CARTESIAN_POINT('Ctrl Pts',(-1.78239478793438,3.40947721887428,
-7.11336003930642));
#114089=CARTESIAN_POINT('Ctrl Pts',(-1.80210424016613,3.42251694823007,
-7.1943174933698));
#114090=CARTESIAN_POINT('Ctrl Pts',(-1.81199161497598,3.42888807474745,
-7.23483536672764));
#114091=CARTESIAN_POINT('Ctrl Pts',(-1.82189851405562,3.43511457407837,
-7.27534779770035));
#114092=CARTESIAN_POINT('Ctrl Pts',(-1.23833222316151,3.53021247064798,
-7.39764959851806));
#114093=CARTESIAN_POINT('Ctrl Pts',(-1.25229838088162,3.52794619282402,
-7.3952574474943));
#114094=CARTESIAN_POINT('Ctrl Pts',(-1.26626453860173,3.525679915,-7.3928652964705));
#114095=CARTESIAN_POINT('Ctrl Pts',(-1.67136591378173,3.459944422,-7.32347873441115));
#114096=CARTESIAN_POINT('Ctrl Pts',(-2.06646034810027,3.395197164,-7.21024443357577));
#114097=CARTESIAN_POINT('Ctrl Pts',(-0.961349642372511,3.53021247064798,
-7.18603209133051));
#114098=CARTESIAN_POINT('Ctrl Pts',(-0.974918007686249,3.52794619282402,
-7.18416470216521));
#114099=CARTESIAN_POINT('Ctrl Pts',(-0.988486373,3.525679915,-7.182297313));
#114100=CARTESIAN_POINT('Ctrl Pts',(-1.38204941,3.459944422,-7.128131956));
#114101=CARTESIAN_POINT('Ctrl Pts',(-1.767337726,3.395197164,-7.031288457));
#114102=CARTESIAN_POINT('',(-1.26569078444363,3.52567991503086,-7.39243037450837));
#114103=CARTESIAN_POINT('Origin',(0.016094124521488,3.62494885332331,0.188269188525618));
#114104=CARTESIAN_POINT('',(-1.12708857585279,3.52567991373765,-7.28736384418274));
#114105=CARTESIAN_POINT('Origin',(-1.69677639993981E-13,3.61749373599967,
-5.16947595841089E-13));
#114106=CARTESIAN_POINT('',(-1.82037400765982,3.61640598742735,-7.27572941129027));
#114107=CARTESIAN_POINT('Origin',(0.0453858973627483,3.62499779203663,0.187121226497711));
#114108=CARTESIAN_POINT('Origin',(0.0254052502516719,3.48215431679144,0.189856002383667));
#114109=CARTESIAN_POINT('Ctrl Pts',(0.033805781,3.395189501,-7.499923811));
#114110=CARTESIAN_POINT('Ctrl Pts',(-0.373371039,3.460370723,-7.501759154));
#114111=CARTESIAN_POINT('Ctrl Pts',(-0.778353314,3.525679915,-7.459501734));
#114112=CARTESIAN_POINT('Ctrl Pts',(-0.205103028,3.395189501,-7.247098229));
#114113=CARTESIAN_POINT('Ctrl Pts',(-0.598553747,3.460370723,-7.23596302300001));
#114114=CARTESIAN_POINT('Ctrl Pts',(-0.988486373,3.525679915,-7.182297313));
#114115=CARTESIAN_POINT('',(-0.883419830874176,3.52567991706892,-7.32089952502357));
#114116=CARTESIAN_POINT('Ctrl Pts',(-0.20978709063981,3.39596551406428,
-7.24696414900821));
#114117=CARTESIAN_POINT('Ctrl Pts',(-0.210661115511315,3.40280154621224,
-7.28856504635459));
#114118=CARTESIAN_POINT('Ctrl Pts',(-0.211561248997317,3.40947721886393,
-7.33021582659437));
#114119=CARTESIAN_POINT('Ctrl Pts',(-0.213406445784567,3.42251694821776,
-7.41351749006351));
#114120=CARTESIAN_POINT('Ctrl Pts',(-0.214352514266222,3.42888807473786,
-7.45521357138656));
#114121=CARTESIAN_POINT('Ctrl Pts',(-0.215318820514567,3.43511457407938,
-7.4969085347325));
#114122=CARTESIAN_POINT('Ctrl Pts',(0.361283325361629,3.52699760873882,
-7.49129776665977));
#114123=CARTESIAN_POINT('Ctrl Pts',(0.357168844680815,3.52633876186941,
-7.49149166632988));
#114124=CARTESIAN_POINT('Ctrl Pts',(0.353054364,3.525679915,-7.491685566));
#114125=CARTESIAN_POINT('Ctrl Pts',(-0.057461992,3.459944422,-7.511031625));
#114126=CARTESIAN_POINT('Ctrl Pts',(-0.467634306,3.395197164,-7.48540701300001));
#114127=CARTESIAN_POINT('Ctrl Pts',(0.586543593611081,3.52699760873882,
-7.22623899646124));
#114128=CARTESIAN_POINT('Ctrl Pts',(0.582574548805541,3.52633876186941,
-7.22655677023062));
#114129=CARTESIAN_POINT('Ctrl Pts',(0.578605504,3.525679915,-7.226874544));
#114130=CARTESIAN_POINT('Ctrl Pts',(0.182599802,3.459944422,-7.258579962));
#114131=CARTESIAN_POINT('Ctrl Pts',(-0.214499177,3.395197164,-7.246826209));
#114132=CARTESIAN_POINT('',(0.46582994172268,3.52567991373765,-7.35928005451117));
#114133=CARTESIAN_POINT('Ctrl Pts',(1.645277344,3.395189501,-7.317312516));
#114134=CARTESIAN_POINT('Ctrl Pts',(1.248014636,3.460370723,-7.40663593));
#114135=CARTESIAN_POINT('Ctrl Pts',(0.843416526,3.525679915,-7.45242568300001));
#114136=CARTESIAN_POINT('Ctrl Pts',(1.357604063,3.395189501,-7.121756188));
#114137=CARTESIAN_POINT('Ctrl Pts',(0.970958263,3.460370723,-7.195461591));
#114138=CARTESIAN_POINT('Ctrl Pts',(0.578605504000001,3.525679915,-7.226874544));
#114139=CARTESIAN_POINT('',(0.843416536403176,3.52567991637269,-7.45242568060099));
#114140=CARTESIAN_POINT('',(0.711011027658161,3.52567991706892,-7.33965011227377));
#114141=CARTESIAN_POINT('',(1.40132893743346,3.43511457320505,-7.36792216210267));
#114142=CARTESIAN_POINT('Origin',(-0.0286356026579147,3.48214115263802,
0.190925565646907));
#114143=CARTESIAN_POINT('Ctrl Pts',(1.35300068819012,3.39596551399878,-7.12263217758401));
#114144=CARTESIAN_POINT('Ctrl Pts',(1.36109001433851,3.40280150691475,-7.16344812417094));
#114145=CARTESIAN_POINT('Ctrl Pts',(1.36916456012132,3.40947713912844,-7.2043183690547));
#114146=CARTESIAN_POINT('Ctrl Pts',(1.38526999695604,3.42251694824015,-7.28606964857968));
#114147=CARTESIAN_POINT('Ctrl Pts',(1.39330947210524,3.42888807476758,-7.32699427545928));
#114148=CARTESIAN_POINT('Ctrl Pts',(1.40132894230255,3.43511457411378,-7.36792216101036));
#114149=CARTESIAN_POINT('Ctrl Pts',(1.96324430040488,3.52699760873882,-7.23849015173953));
#114150=CARTESIAN_POINT('Ctrl Pts',(1.95926769670244,3.52633876186941,-7.23956400986976));
#114151=CARTESIAN_POINT('Ctrl Pts',(1.955291093,3.525679915,-7.240637868));
#114152=CARTESIAN_POINT('Ctrl Pts',(1.558531213,3.459944422,-7.34778050900001));
#114153=CARTESIAN_POINT('Ctrl Pts',(1.152439965,3.395197164,-7.41092991));
#114154=CARTESIAN_POINT('Ctrl Pts',(2.12625830857137,3.52699760873882,-6.93120400959201));
#114155=CARTESIAN_POINT('Ctrl Pts',(2.12245036978568,3.52633876186941,-6.93236758129601));
#114156=CARTESIAN_POINT('Ctrl Pts',(2.118642431,3.525679915,-6.933531153));
#114157=CARTESIAN_POINT('Ctrl Pts',(1.738710849,3.459944422,-7.049624836));
#114158=CARTESIAN_POINT('Ctrl Pts',(1.348369115,3.395197164,-7.123510422));
#114159=CARTESIAN_POINT('',(1.95529109576274,3.52567991457198,-7.24063786855863));
#114160=CARTESIAN_POINT('Origin',(-0.0644455688419812,3.62494888378541,
0.177626244271242));
#114161=CARTESIAN_POINT('',(2.03696676943704,3.52567991373765,-7.08708450836245));
#114162=CARTESIAN_POINT('Origin',(-4.66206934168767E-14,3.61749373599911,
-4.90059381963448E-14));
#114163=CARTESIAN_POINT('',(1.40287278194271,3.61640598739338,-7.36762838021731));
#114164=CARTESIAN_POINT('Origin',(-0.0373790373297064,3.62499777786392,
0.18888364588575));
#114165=CARTESIAN_POINT('Origin',(-0.056661309098946,3.48215429044633,0.182976075754221));
#114166=CARTESIAN_POINT('Ctrl Pts',(3.179817567,3.395189501,-6.792551821));
#114167=CARTESIAN_POINT('Ctrl Pts',(2.811044533,3.460370723,-6.965186642));
#114168=CARTESIAN_POINT('Ctrl Pts',(2.425749146,3.525679915,-7.09688249));
#114169=CARTESIAN_POINT('Ctrl Pts',(2.856831098,3.395189501,-6.663408743));
#114170=CARTESIAN_POINT('Ctrl Pts',(2.495069344,3.460370723,-6.818508373));
#114171=CARTESIAN_POINT('Ctrl Pts',(2.118642431,3.525679915,-6.933531153));
#114172=CARTESIAN_POINT('',(2.4257491556452,3.52567991637267,-7.09688248541667));
#114173=CARTESIAN_POINT('',(2.27219580059861,3.52567991706892,-7.01520681758131));
#114174=CARTESIAN_POINT('',(2.95245211611529,3.43511457319795,-6.89441993772619));
#114175=CARTESIAN_POINT('Origin',(-0.0690095232738826,3.48214119981529,
0.180306178259331));
#114176=CARTESIAN_POINT('Ctrl Pts',(2.85252365852958,3.39596551411236,-6.66525384212721));
#114177=CARTESIAN_POINT('Ctrl Pts',(2.8691981784591,3.40280154625929,-6.70337678750105));
#114178=CARTESIAN_POINT('Ctrl Pts',(2.88586994819414,3.40947721890447,-6.74155596804241));
#114179=CARTESIAN_POINT('Ctrl Pts',(2.9191727537913,3.42251694824652,-6.81793328812538));
#114180=CARTESIAN_POINT('Ctrl Pts',(2.93582185555585,3.42888807475833,-6.8561728703922));
#114181=CARTESIAN_POINT('Ctrl Pts',(2.95245212060851,3.43511457409255,-6.89441993562685));
#114182=CARTESIAN_POINT('Ctrl Pts',(3.47340615432972,3.52699760873882,-6.64721878366841));
#114183=CARTESIAN_POINT('Ctrl Pts',(3.46975336916486,3.52633876186941,-6.6491223878342));
#114184=CARTESIAN_POINT('Ctrl Pts',(3.466100584,3.525679915,-6.651025992));
#114185=CARTESIAN_POINT('Ctrl Pts',(3.10164923,3.459944422,-6.84095534300001));
#114186=CARTESIAN_POINT('Ctrl Pts',(2.718627424,3.395197164,-6.98992596));
#114187=CARTESIAN_POINT('Ctrl Pts',(3.566551547531,3.52699760873882,-6.31207362737036));
#114188=CARTESIAN_POINT('Ctrl Pts',(3.5630827697655,3.52633876186941,-6.31402858968518));
#114189=CARTESIAN_POINT('Ctrl Pts',(3.559613992,3.525679915,-6.315983552));
#114190=CARTESIAN_POINT('Ctrl Pts',(3.21352171,3.459944422,-6.511037088));
#114191=CARTESIAN_POINT('Ctrl Pts',(2.848189165,3.395197164,-6.667107205));
#114192=CARTESIAN_POINT('',(3.46610058684643,3.52567991457198,-6.65102599192097));
#114193=CARTESIAN_POINT('Origin',(-0.101123261420778,3.62494888976623,0.159619578785367));
#114194=CARTESIAN_POINT('',(3.51285729480366,3.52567991373765,-6.48350476831368));
#114195=CARTESIAN_POINT('Origin',(1.26634813746307E-13,3.61749373600033,
-2.15105711021124E-13));
#114196=CARTESIAN_POINT('',(2.95389671194755,3.61640598740987,-6.89380114360488));
#114197=CARTESIAN_POINT('Origin',(-0.0771095214129497,3.62499779838487,
0.176432218884227));
#114198=CARTESIAN_POINT('Origin',(-0.0946710417999042,3.48215430175332,
0.166517704383047));
#114199=CARTESIAN_POINT('Ctrl Pts',(4.565673054,3.395189501,-5.950178952));
#114200=CARTESIAN_POINT('Ctrl Pts',(4.242633113,3.460370723,-6.198052969));
#114201=CARTESIAN_POINT('Ctrl Pts',(3.894656432,3.525679915,-6.40949696));
#114202=CARTESIAN_POINT('Ctrl Pts',(4.222475885,3.395189501,-5.893487711));
#114203=CARTESIAN_POINT('Ctrl Pts',(3.902513756,3.460370723,-6.122729281));
#114204=CARTESIAN_POINT('Ctrl Pts',(3.559613992,3.525679915,-6.315983552));
#114205=CARTESIAN_POINT('',(3.8946564404075,3.52567991637268,-6.40949695345765));
#114206=CARTESIAN_POINT('',(3.72713522297332,3.52567991706892,-6.3627402495721));
#114207=CARTESIAN_POINT('',(4.36552191505787,3.43511457318807,-6.09854229996074));
#114208=CARTESIAN_POINT('Origin',(-0.106156408365024,3.48214118529408,0.161255378447459));
#114209=CARTESIAN_POINT('Ctrl Pts',(4.21866579300694,3.39596551405285,-5.89621564465874));
#114210=CARTESIAN_POINT('Ctrl Pts',(4.24314564013628,3.40280150761502,-5.92986257788553));
#114211=CARTESIAN_POINT('Ctrl Pts',(4.26763487249922,3.40947714050253,-5.96356499748966));
#114212=CARTESIAN_POINT('Ctrl Pts',(4.31657823714961,3.42251694821273,-6.03099794479326));
#114213=CARTESIAN_POINT('Ctrl Pts',(4.34105847192057,3.42888807472854,-6.06476444220809));
#114214=CARTESIAN_POINT('Ctrl Pts',(4.36552191896387,3.43511457406307,-6.09854229697054));
#114215=CARTESIAN_POINT('Ctrl Pts',(4.82115539691061,3.52699760873882,-5.74513085140018));
#114216=CARTESIAN_POINT('Ctrl Pts',(4.8179972304553,3.52633876186941,-5.74777519120009));
#114217=CARTESIAN_POINT('Ctrl Pts',(4.814839064,3.525679915,-5.750419531));
#114218=CARTESIAN_POINT('Ctrl Pts',(4.499737576,3.459944422,-6.01425470800001));
#114219=CARTESIAN_POINT('Ctrl Pts',(4.157694886,3.395197164,-6.242080842));
#114220=CARTESIAN_POINT('Ctrl Pts',(4.84007680111362,3.52699760873882,-5.39779769684762));
#114221=CARTESIAN_POINT('Ctrl Pts',(4.83710938055682,3.52633876186941,-5.40045263792381));
#114222=CARTESIAN_POINT('Ctrl Pts',(4.83414196,3.525679915,-5.403107579));
#114223=CARTESIAN_POINT('Ctrl Pts',(4.538071868,3.459944422,-5.668000483));
#114224=CARTESIAN_POINT('Ctrl Pts',(4.214831056,3.395197164,-5.898957465));
#114225=CARTESIAN_POINT('',(4.81483906674359,3.52567991457198,-5.75041953034411));
#114226=CARTESIAN_POINT('Origin',(-0.133072610412248,3.62494889177638,0.134149317188565));
#114227=CARTESIAN_POINT('',(4.82449051785211,3.52567991373766,-5.57676354993731));
#114228=CARTESIAN_POINT('Origin',(-1.58944038486375E-13,3.61749373599945,
2.90132501357121E-13));
#114229=CARTESIAN_POINT('',(4.36679971533011,3.61640598740656,-6.09762742744872));
#114230=CARTESIAN_POINT('Origin',(-0.113234348334703,3.62499780122883,0.155730897777955));
#114231=CARTESIAN_POINT('Origin',(-0.128254040349813,3.48215433246544,0.14227308511448));
#114232=CARTESIAN_POINT('Ctrl Pts',(5.738042744,3.395189501,-4.829582328));
#114233=CARTESIAN_POINT('Ctrl Pts',(5.475840884,3.460370723,-5.141105227));
#114234=CARTESIAN_POINT('Ctrl Pts',(5.181453912,3.525679915,-5.422410475));
#114235=CARTESIAN_POINT('Ctrl Pts',(5.390682393,3.395189501,-4.847993744));
#114236=CARTESIAN_POINT('Ctrl Pts',(5.127480962,3.460370723,-5.140658173));
#114237=CARTESIAN_POINT('Ctrl Pts',(4.83414196,3.525679915,-5.403107579));
#114238=CARTESIAN_POINT('',(5.18145391881129,3.52567991637267,-5.42241046679963));
#114239=CARTESIAN_POINT('',(5.00779794533496,3.52567991706892,-5.41275901836345));
#114240=CARTESIAN_POINT('',(5.57446476168392,3.4351145731887,-5.01750360199659));
#114241=CARTESIAN_POINT('Origin',(-0.138339562021414,3.48214118888366,0.134664725891545));
#114242=CARTESIAN_POINT('Ctrl Pts',(5.38754780344265,3.39596551400055,-4.85147695703864));
#114243=CARTESIAN_POINT('Ctrl Pts',(5.41868842773454,3.40280150893663,-4.87907480553435));
#114244=CARTESIAN_POINT('Ctrl Pts',(5.44985014661251,3.40947714325031,-4.90672482643989));
#114245=CARTESIAN_POINT('Ctrl Pts',(5.51214531987703,3.42251694820028,-4.96205984035383));
#114246=CARTESIAN_POINT('Ctrl Pts',(5.54331201925207,3.42888807472423,-4.98977436894406));
#114247=CARTESIAN_POINT('Ctrl Pts',(5.57446476485727,3.43511457406497,-5.0175035982347));
#114248=CARTESIAN_POINT('Ctrl Pts',(5.9558672539275,3.53021247061354,-4.5592029476204));
#114249=CARTESIAN_POINT('Ctrl Pts',(5.94721189361869,3.52794619280679,-4.57042171235928));
#114250=CARTESIAN_POINT('Ctrl Pts',(5.93855653331001,3.525679915,-4.58164047709804));
#114251=CARTESIAN_POINT('Ctrl Pts',(5.68749976732975,3.459944422,-4.90705116979723));
#114252=CARTESIAN_POINT('Ctrl Pts',(5.4023903318827,3.395197164,-5.2030819588396));
#114253=CARTESIAN_POINT('Ctrl Pts',(5.89864161721082,3.53021247061353,-4.21536207557745));
#114254=CARTESIAN_POINT('Ctrl Pts',(5.89063621960535,3.5279461928068,-4.22647518878876));
#114255=CARTESIAN_POINT('Ctrl Pts',(5.882630822,3.525679915,-4.237588302));
#114256=CARTESIAN_POINT('Ctrl Pts',(5.650426828,3.459944422,-4.559934474));
#114257=CARTESIAN_POINT('Ctrl Pts',(5.384392131,3.395197164,-4.85497903));
#114258=CARTESIAN_POINT('',(5.93844102538326,3.52567991457841,-4.5809298375767));
#114259=CARTESIAN_POINT('Origin',(-0.158799496831515,3.62494884927284,0.102406236496948));
#114260=CARTESIAN_POINT('',(5.91053592562699,3.52567991373765,-4.40925906729761));
#114261=CARTESIAN_POINT('Origin',(2.00794242344315E-13,3.617493736,-2.71050543121376E-13));
#114262=CARTESIAN_POINT('',(5.57551601667305,3.61640598737761,-5.01633542971883));
#114263=CARTESIAN_POINT('Origin',(-0.144064587206557,3.62499782023102,0.127748007484126));
#114264=CARTESIAN_POINT('Origin',(-0.155839937661904,3.48215431455712,0.111375903320868));
#114265=CARTESIAN_POINT('Ctrl Pts',(6.642107933,3.395189501,-3.483159803));
#114266=CARTESIAN_POINT('Ctrl Pts',(6.45300442,3.460370723,-3.843765118));
#114267=CARTESIAN_POINT('Ctrl Pts',(6.225972366,3.525679915,-4.181778103));
#114268=CARTESIAN_POINT('Ctrl Pts',(6.306826583,3.395189501,-3.575812977));
#114269=CARTESIAN_POINT('Ctrl Pts',(6.112692857,3.460370723,-3.918215602));
#114270=CARTESIAN_POINT('Ctrl Pts',(5.882630822,3.525679915,-4.237588302));
#114271=CARTESIAN_POINT('',(6.22597237087733,3.52567991637267,-4.1817780935345));
#114272=CARTESIAN_POINT('',(6.05430160126011,3.52567991706892,-4.20968319205863));
#114273=CARTESIAN_POINT('',(6.52275183160806,3.43511457319251,-3.7018520124256));
#114274=CARTESIAN_POINT('Origin',(-0.164054713654601,3.48214119996662,0.101777745563075));
#114275=CARTESIAN_POINT('Ctrl Pts',(6.304514067401,3.39596551400235,-3.57988859824468));
#114276=CARTESIAN_POINT('Ctrl Pts',(6.34085934616121,3.40280150582777,-3.60014690173996));
#114277=CARTESIAN_POINT('Ctrl Pts',(6.37723643965595,3.40947713692085,-3.62045162175645));
#114278=CARTESIAN_POINT('Ctrl Pts',(6.44997061389297,3.42251694820707,-3.66110133292935));
#114279=CARTESIAN_POINT('Ctrl Pts',(6.4863664575326,3.42888807473104,-3.68146799218158));
#114280=CARTESIAN_POINT('Ctrl Pts',(6.52275183390539,3.4351145740766,-3.70185200805483));
#114281=CARTESIAN_POINT('Ctrl Pts',(6.79671625250398,3.5302124705803,-3.17227591142549));
#114282=CARTESIAN_POINT('Ctrl Pts',(6.79067495253319,3.52794619279017,-3.18509303418759));
#114283=CARTESIAN_POINT('Ctrl Pts',(6.78463365256231,3.525679915,-3.19791015694976));
#114284=CARTESIAN_POINT('Ctrl Pts',(6.60940013367513,3.459944422,-3.56968271160645));
#114285=CARTESIAN_POINT('Ctrl Pts',(6.39459426724533,3.395197164,-3.9200825665283));
#114286=CARTESIAN_POINT('Ctrl Pts',(6.66691289494691,3.5302124705803,-2.84877566785109));
#114287=CARTESIAN_POINT('Ctrl Pts',(6.66148364997345,3.52794619279017,-2.86134988642553));
#114288=CARTESIAN_POINT('Ctrl Pts',(6.656054405,3.525679915,-2.873924105));
#114289=CARTESIAN_POINT('Ctrl Pts',(6.49857411,3.459944422,-3.238650998));
#114290=CARTESIAN_POINT('Ctrl Pts',(6.302185015,3.395197164,-3.583987171));
#114291=CARTESIAN_POINT('',(6.78436807904918,3.52567991503086,-3.19724096221395));
#114292=CARTESIAN_POINT('Origin',(-0.177101252742581,3.62494886858678,0.065874886723139));
#114293=CARTESIAN_POINT('',(6.72021124318548,3.52567991373765,-3.03558253094795));
#114294=CARTESIAN_POINT('Origin',(1.63410951437015E-12,3.61749373599922,
-9.50411624400793E-13));
#114295=CARTESIAN_POINT('',(6.52352738588612,3.61640598738353,-3.70048516261255));
#114296=CARTESIAN_POINT('Origin',(-0.168158374720755,3.62499780471484,0.0937916323317745));
#114297=CARTESIAN_POINT('Origin',(-0.176139459378517,3.4821543088949,0.0752712603977301));
#114298=CARTESIAN_POINT('Ctrl Pts',(7.235595536,3.395189501,-1.973868596));
#114299=CARTESIAN_POINT('Ctrl Pts',(7.128432643,3.460370723,-2.366694825));
#114300=CARTESIAN_POINT('Ctrl Pts',(6.979371271,3.525679915,-2.745610435));
#114301=CARTESIAN_POINT('Ctrl Pts',(6.928070572,3.395189501,-2.13643117));
#114302=CARTESIAN_POINT('Ctrl Pts',(6.812082027,3.460370723,-2.512561624));
#114303=CARTESIAN_POINT('Ctrl Pts',(6.656054405,3.525679915,-2.873924105));
#114304=CARTESIAN_POINT('',(6.97937127374582,3.52567991637268,-2.74561042469145));
#114305=CARTESIAN_POINT('',(6.81771284284578,3.52567991706892,-2.80976725824203));
#114306=CARTESIAN_POINT('',(7.16604227526424,3.43511457319985,-2.21310593709546));
#114307=CARTESIAN_POINT('Origin',(-0.182097970521191,3.48214116801236,0.0641311704411699));
#114308=CARTESIAN_POINT('Ctrl Pts',(6.9266882594647,3.39596551400351,-2.1409086281669));
#114309=CARTESIAN_POINT('Ctrl Pts',(6.9665387446434,3.40280150624475,-2.15288014373984));
#114310=CARTESIAN_POINT('Ctrl Pts',(7.00643027926497,3.40947713776356,-2.16489015161554));
#114311=CARTESIAN_POINT('Ctrl Pts',(7.0862024503661,3.42251694823578,-2.1889537961222));
#114312=CARTESIAN_POINT('Ctrl Pts',(7.12612560918764,3.4288880747598,-2.20102026370945));
#114313=CARTESIAN_POINT('Ctrl Pts',(7.16604227657517,3.4351145740985,-2.21310593230273));
#114314=CARTESIAN_POINT('Ctrl Pts',(7.31975835219288,3.53021247065002,-1.63701677804991));
#114315=CARTESIAN_POINT('Ctrl Pts',(7.31661359695517,3.52794619282504,-1.65083294474948));
#114316=CARTESIAN_POINT('Ctrl Pts',(7.31346884171736,3.525679915,-1.66464911144911));
#114317=CARTESIAN_POINT('Ctrl Pts',(7.22225229552072,3.459944422,-2.06539985760202));
#114318=CARTESIAN_POINT('Ctrl Pts',(7.08779408178921,3.395197164,-2.45378447035253));
#114319=CARTESIAN_POINT('Ctrl Pts',(7.12344673599801,3.53021247065002,-1.34898367557698));
#114320=CARTESIAN_POINT('Ctrl Pts',(7.12084750899901,3.52794619282504,-1.3624310432885));
#114321=CARTESIAN_POINT('Ctrl Pts',(7.118248282,3.525679915,-1.375878411));
#114322=CARTESIAN_POINT('Ctrl Pts',(7.04285528900001,3.459944422,-1.7659318));
#114323=CARTESIAN_POINT('Ctrl Pts',(6.925294731,3.395197164,-2.145412056));
#114324=CARTESIAN_POINT('',(7.31306561976193,3.52567991457841,-1.66405265299233));
#114325=CARTESIAN_POINT('Origin',(-0.187121738364304,3.62494885490083,0.0262631901970392));
#114326=CARTESIAN_POINT('',(7.21565695159502,3.52567991373765,-1.51996552892804));
#114327=CARTESIAN_POINT('Origin',(8.30065183254902E-13,3.61749373599978,
-2.65737952476197E-13));
#114328=CARTESIAN_POINT('',(7.16650586494504,3.6164059874119,-2.21160432283927));
#114329=CARTESIAN_POINT('Origin',(-0.184389231530323,3.62499784037748,0.0554497127867537));
#114330=CARTESIAN_POINT('Origin',(-0.188202325549108,3.48215429683246,0.035646622946475));
#114331=CARTESIAN_POINT('Ctrl Pts',(7.490754735,3.395189501,-0.372281487));
#114332=CARTESIAN_POINT('Ctrl Pts',(7.470543277,3.460370723,-0.778960512000001));
#114333=CARTESIAN_POINT('Ctrl Pts',(7.406422533,3.525679915,-1.181061074));
#114334=CARTESIAN_POINT('Ctrl Pts',(7.225365682,3.395189501,-0.597152216));
#114335=CARTESIAN_POINT('Ctrl Pts',(7.192945813,3.460370723,-0.989423057));
#114336=CARTESIAN_POINT('Ctrl Pts',(7.118248282,3.525679915,-1.375878411));
#114337=CARTESIAN_POINT('',(7.40642253346363,3.52567991637266,-1.18106106333763));
#114338=CARTESIAN_POINT('',(7.26233540970488,3.52567991706892,-1.27846972997522));
#114339=CARTESIAN_POINT('',(7.47425654613115,3.43511457318359,-0.620877487542569));
#114340=CARTESIAN_POINT('Origin',(-0.191626976407847,3.48214120369069,0.0234861444890657));
#114341=CARTESIAN_POINT('Ctrl Pts',(7.22497820779554,3.3959655139285,-0.601822150021933));
#114342=CARTESIAN_POINT('Ctrl Pts',(7.26647055793215,3.40280151035648,-0.604947103677359));
#114343=CARTESIAN_POINT('Ctrl Pts',(7.30801127578618,3.4094771461764,-0.60810082564552));
#114344=CARTESIAN_POINT('Ctrl Pts',(7.39109133582747,3.42251694818263,-0.614453212584922));
#114345=CARTESIAN_POINT('Ctrl Pts',(7.43267504712686,3.42888807471259,-0.617655273833398));
#114346=CARTESIAN_POINT('Ctrl Pts',(7.47425654638066,3.4351145740495,-0.620877482649554));
#114347=CARTESIAN_POINT('Ctrl Pts',(7.50053668693811,3.53021247056292,-0.0252125605125761));
#114348=CARTESIAN_POINT('Ctrl Pts',(7.50043552175035,3.52794619278149,-0.0393817420581123));
#114349=CARTESIAN_POINT('Ctrl Pts',(7.50033435656256,3.525679915,-0.0535509236036477));
#114350=CARTESIAN_POINT('Ctrl Pts',(7.49739996628298,3.459944422,-0.464541201103576));
#114351=CARTESIAN_POINT('Ctrl Pts',(7.44957652221862,3.395197164,-0.872750138705848));
#114352=CARTESIAN_POINT('Ctrl Pts',(7.24689612386501,3.53021247056292,0.213885293912943));
#114353=CARTESIAN_POINT('Ctrl Pts',(7.24724845193251,3.52794619278149,0.200193561456469));
#114354=CARTESIAN_POINT('Ctrl Pts',(7.24760078,3.525679915,0.186501829));
#114355=CARTESIAN_POINT('Ctrl Pts',(7.257820383,3.459944422,-0.210639594));
#114356=CARTESIAN_POINT('Ctrl Pts',(7.224585363,3.395197164,-0.606519857));
#114357=CARTESIAN_POINT('',(7.49981234078918,3.52567991457841,-0.0530550908287365));
#114358=CARTESIAN_POINT('Origin',(-0.188392868196582,3.62494885611011,-0.0145764597221847));
#114359=CARTESIAN_POINT('',(7.37370656042998,3.52567991373765,0.0667233722378182));
#114360=CARTESIAN_POINT('Origin',(-1.69569219776733E-13,3.61749373600011,
4.07626135536659E-14));
#114361=CARTESIAN_POINT('',(7.47438649539288,3.61640598739424,-0.619311321310272));
#114362=CARTESIAN_POINT('Origin',(-0.191998517910724,3.62499782284084,0.0145151197861249));
#114363=CARTESIAN_POINT('Origin',(-0.191465174249291,3.48215433943968,-0.00564471087924709));
#114364=CARTESIAN_POINT('Ctrl Pts',(7.395654567,3.395189501,1.24671309));
#114365=CARTESIAN_POINT('Ctrl Pts',(7.463339611,3.460370723,0.845197129));
#114366=CARTESIAN_POINT('Ctrl Pts',(7.487157709,3.525679915,0.43871339));
#114367=CARTESIAN_POINT('Ctrl Pts',(7.184810722,3.395189501,0.970048913));
#114368=CARTESIAN_POINT('Ctrl Pts',(7.23747544800001,3.460370723,0.579979832));
#114369=CARTESIAN_POINT('Ctrl Pts',(7.24760078,3.525679915,0.186501829));
#114370=CARTESIAN_POINT('',(7.4871577071628,3.52567991637267,0.438713400513138));
#114371=CARTESIAN_POINT('',(7.36737924396087,3.52567991706892,0.312607622205938));
#114372=CARTESIAN_POINT('',(7.43298288901529,3.43511457321003,1.00038250308341));
#114373=CARTESIAN_POINT('Origin',(-0.192195783444843,3.4821411629602,-0.0182570933746986));
#114374=CARTESIAN_POINT('Ctrl Pts',(7.18543620474245,3.39596551404374,0.965404863421029));
#114375=CARTESIAN_POINT('Ctrl Pts',(7.22663047529356,3.40280154623927,0.971272628899141));
#114376=CARTESIAN_POINT('Ctrl Pts',(7.26787819499172,3.40947721884971,0.977122699753423));
#114377=CARTESIAN_POINT('Ctrl Pts',(7.3503810057172,3.4225169482536,0.988778520276736));
#114378=CARTESIAN_POINT('Ctrl Pts',(7.39168086152302,3.42888807478171,0.994590590171426));
#114379=CARTESIAN_POINT('Ctrl Pts',(7.43298288818389,3.43511457412893,1.00038250802431));
#114380=CARTESIAN_POINT('Ctrl Pts',(7.33416218652337,3.52699760873882,1.56848107737335));
#114381=CARTESIAN_POINT('Ctrl Pts',(7.33501918076169,3.52633876186941,1.56445216818668));
#114382=CARTESIAN_POINT('Ctrl Pts',(7.335876175,3.525679915,1.560423259));
#114383=CARTESIAN_POINT('Ctrl Pts',(7.421381535,3.459944422,1.158444675));
#114384=CARTESIAN_POINT('Ctrl Pts',(7.462452985,3.395197164,0.749530155));
#114385=CARTESIAN_POINT('Ctrl Pts',(7.03615210583643,3.52699760873882,1.74789214721709));
#114386=CARTESIAN_POINT('Ctrl Pts',(7.03710781341822,3.52633876186941,1.74402679860854));
#114387=CARTESIAN_POINT('Ctrl Pts',(7.038063521,3.525679915,1.74016145));
#114388=CARTESIAN_POINT('Ctrl Pts',(7.133417862,3.459944422,1.354501886));
#114389=CARTESIAN_POINT('Ctrl Pts',(7.18606241200001,3.395197164,0.960732536));
#114390=CARTESIAN_POINT('',(7.33587617569046,3.52567991457198,1.56042326175562));
#114391=CARTESIAN_POINT('Origin',(-0.180854831178093,3.62494886848255,-0.0547345692229878));
#114392=CARTESIAN_POINT('',(7.18696984626822,3.52567991373765,1.65029236204186));
#114393=CARTESIAN_POINT('Origin',(4.76615275024628E-13,3.617493735999,8.23993651088983E-14));
#114394=CARTESIAN_POINT('',(7.43277311984018,3.61640598738135,1.00193998853182));
#114395=CARTESIAN_POINT('Origin',(-0.190630119290141,3.62499783977117,-0.0270982572358046));
#114396=CARTESIAN_POINT('Origin',(-0.185775199275259,3.48215434388086,-0.0466720506929474));
#114397=CARTESIAN_POINT('Ctrl Pts',(6.954741811,3.395189501,2.807412748));
#114398=CARTESIAN_POINT('Ctrl Pts',(7.107158479,3.460370723,2.429834291));
#114399=CARTESIAN_POINT('Ctrl Pts',(7.21780171200001,3.525679915,2.037974103));
#114400=CARTESIAN_POINT('Ctrl Pts',(6.808301998,3.395189501,2.491891632));
#114401=CARTESIAN_POINT('Ctrl Pts',(6.943588774,3.460370723,2.122263509));
#114402=CARTESIAN_POINT('Ctrl Pts',(7.038063521,3.525679915,1.74016145));
#114403=CARTESIAN_POINT('',(7.21780170794649,3.52567991637268,2.03797411287136));
#114404=CARTESIAN_POINT('',(7.12793261324207,3.52567991706892,1.88906778879299));
#114405=CARTESIAN_POINT('',(7.04415121226113,3.43511457319547,2.5748657198136));
#114406=CARTESIAN_POINT('Origin',(-0.18377778965417,3.48214119424527,-0.0591467200203382));
#114407=CARTESIAN_POINT('Ctrl Pts',(6.80991119058296,3.39596551402597,2.48749061798307));
#114408=CARTESIAN_POINT('Ctrl Pts',(6.84888096577829,3.40280154620957,2.50207674882005));
#114409=CARTESIAN_POINT('Ctrl Pts',(6.88790674453291,3.40947721884071,2.51665708881238));
#114410=CARTESIAN_POINT('Ctrl Pts',(6.96597502842747,3.422516948223,2.54577606831888));
#114411=CARTESIAN_POINT('Ctrl Pts',(7.00505989332313,3.42888807474518,2.5603305034797));
#114412=CARTESIAN_POINT('Ctrl Pts',(7.04415121041215,3.43511457408519,2.57486572440514));
#114413=CARTESIAN_POINT('Ctrl Pts',(6.82551648286577,3.52699760873882,3.10843893519605));
#114414=CARTESIAN_POINT('Ctrl Pts',(6.82721953743289,3.52633876186941,3.10468844809802));
#114415=CARTESIAN_POINT('Ctrl Pts',(6.828922592,3.525679915,3.100937961));
#114416=CARTESIAN_POINT('Ctrl Pts',(6.998842397,3.459944422,2.726738538));
#114417=CARTESIAN_POINT('Ctrl Pts',(7.126858153,3.395197164,2.33621336));
#114418=CARTESIAN_POINT('Ctrl Pts',(6.49590563527169,3.52699760873882,3.21959211607213));
#114419=CARTESIAN_POINT('Ctrl Pts',(6.49766993463585,3.52633876186941,3.21602258603607));
#114420=CARTESIAN_POINT('Ctrl Pts',(6.49943423400001,3.525679915,3.212453056));
#114421=CARTESIAN_POINT('Ctrl Pts',(6.67546465,3.459944422,2.856308362));
#114422=CARTESIAN_POINT('Ctrl Pts',(6.81152717,3.395197164,2.483062143));
#114423=CARTESIAN_POINT('',(6.8289225920729,3.52567991457198,3.10093796384888));
#114424=CARTESIAN_POINT('Origin',(-0.16486016511682,3.62494886692739,-0.0923333130057202));
#114425=CARTESIAN_POINT('',(6.66417840968742,3.52567991373765,3.15669551549326));
#114426=CARTESIAN_POINT('Origin',(4.53630188967935E-13,3.61749373599956,
2.83410447887711E-13));
#114427=CARTESIAN_POINT('',(7.04361153473072,3.61640598744859,2.5763416980588));
#114428=CARTESIAN_POINT('Origin',(-0.180347906024595,3.62499782659915,-0.0674445278942343));
#114429=CARTESIAN_POINT('Origin',(-0.171399078671139,3.48215430569431,-0.0855171968849683));
#114430=CARTESIAN_POINT('Ctrl Pts',(6.188633058,3.395189501,4.236840907));
#114431=CARTESIAN_POINT('Ctrl Pts',(6.41865451600001,3.460370723,3.900855103));
#114432=CARTESIAN_POINT('Ctrl Pts',(6.610949329,3.525679915,3.541941413));
#114433=CARTESIAN_POINT('Ctrl Pts',(6.11344464,3.395189501,3.897216268));
#114434=CARTESIAN_POINT('Ctrl Pts',(6.325027606,3.460370723,3.565312503));
#114435=CARTESIAN_POINT('Ctrl Pts',(6.499434234,3.525679915,3.212453056));
#114436=CARTESIAN_POINT('',(6.61094932292316,3.5256799163727,3.5419414217492));
#114437=CARTESIAN_POINT('',(6.55519177567553,3.52567991706895,3.37719724580539));
#114438=CARTESIAN_POINT('',(6.3259428542007,3.43511457320914,4.02895107699497));
#114439=CARTESIAN_POINT('Origin',(-0.166766302908787,3.48214114189395,-0.0972706717238127));
#114440=CARTESIAN_POINT('Ctrl Pts',(6.11596229871932,3.39596551408696,3.89326407601825));
#114441=CARTESIAN_POINT('Ctrl Pts',(6.15088539530709,3.40280154630567,3.91588654109528));
#114442=CARTESIAN_POINT('Ctrl Pts',(6.18586443049033,3.4094772188707,3.93851538946913));
#114443=CARTESIAN_POINT('Ctrl Pts',(6.25584780142413,3.42251694827702,3.98373595685815));
#114444=CARTESIAN_POINT('Ctrl Pts',(6.29089011047695,3.42888807479301,4.00635220799284));
#114445=CARTESIAN_POINT('Ctrl Pts',(6.32594285137405,3.43511457412576,4.02895108112679));
#114446=CARTESIAN_POINT('Ctrl Pts',(5.99771721408108,3.52699760873882,4.50304964280461));
#114447=CARTESIAN_POINT('Ctrl Pts',(6.00018669604054,3.52633876186941,4.4997529464023));
#114448=CARTESIAN_POINT('Ctrl Pts',(6.002656178,3.525679915,4.49645625));
#114449=CARTESIAN_POINT('Ctrl Pts',(6.249045167,3.459944422,4.167533137));
#114450=CARTESIAN_POINT('Ctrl Pts',(6.458019356,3.395197164,3.813657824));
#114451=CARTESIAN_POINT('Ctrl Pts',(5.65191783706956,3.52699760873882,4.54074753539395));
#114452=CARTESIAN_POINT('Ctrl Pts',(5.65440823153479,3.52633876186941,4.53764073119698));
#114453=CARTESIAN_POINT('Ctrl Pts',(5.656898626,3.525679915,4.534533927));
#114454=CARTESIAN_POINT('Ctrl Pts',(5.90537413,3.459944422,4.224557034));
#114455=CARTESIAN_POINT('Ctrl Pts',(6.118492488,3.395197164,3.889286524));
#114456=CARTESIAN_POINT('',(6.00265617747834,3.52567991457199,4.49645625278509));
#114457=CARTESIAN_POINT('Origin',(-0.141156974556259,3.62494888824675,-0.125614739924113));
#114458=CARTESIAN_POINT('',(5.82977739726156,3.52567991373766,4.51549509461761));
#114459=CARTESIAN_POINT('Origin',(5.3776427755281E-14,3.61749373599911,
-6.24500451351651E-14));
#114460=CARTESIAN_POINT('',(6.32509850206447,3.6164059874287,4.03027653313337));
#114461=CARTESIAN_POINT('Origin',(-0.161633041163872,3.62499779048983,-0.104637270481759));
#114462=CARTESIAN_POINT('Origin',(-0.149008033408268,3.48215434141335,-0.120363473142919));
#114463=CARTESIAN_POINT('Ctrl Pts',(5.133150701,3.395189501,5.468159094));
#114464=CARTESIAN_POINT('Ctrl Pts',(5.430021402,3.460370723,5.189476265));
#114465=CARTESIAN_POINT('Ctrl Pts',(5.69497630300001,3.525679915,4.880291478));
#114466=CARTESIAN_POINT('Ctrl Pts',(5.132729405,3.395189501,5.120311403));
#114467=CARTESIAN_POINT('Ctrl Pts',(5.410715178,3.460370723,4.841651446));
#114468=CARTESIAN_POINT('Ctrl Pts',(5.656898626,3.525679915,4.534533927));
#114469=CARTESIAN_POINT('',(5.69497629518052,3.52567991637268,4.88029148524294));
#114470=CARTESIAN_POINT('',(5.67593745638144,3.52567991706893,4.70741271228891));
#114471=CARTESIAN_POINT('',(5.31194043917964,3.4351145732143,5.29464716000112));
#114472=CARTESIAN_POINT('Origin',(-0.141957109364025,3.48214116166584,-0.130846379632369));
#114473=CARTESIAN_POINT('Ctrl Pts',(5.13603780670984,3.39596551408558,5.1169928331588));
#114474=CARTESIAN_POINT('Ctrl Pts',(5.16528125939142,3.40280154629497,5.14659383098163));
#114475=CARTESIAN_POINT('Ctrl Pts',(5.19457797078606,3.40947721888794,5.17621308816852));
#114476=CARTESIAN_POINT('Ctrl Pts',(5.2532040840705,3.42251694828979,5.2354207798644));
#114477=CARTESIAN_POINT('Ctrl Pts',(5.28256529793846,3.42888807480765,5.26504133623591));
#114478=CARTESIAN_POINT('Ctrl Pts',(5.31194043551467,3.4351145741414,5.29464716344254));
#114479=CARTESIAN_POINT('Ctrl Pts',(4.87496063697409,3.53021247068103,5.70030219065627));
#114480=CARTESIAN_POINT('Ctrl Pts',(4.88569435681569,3.52794619284054,5.69105215235571));
#114481=CARTESIAN_POINT('Ctrl Pts',(4.89642807665729,3.525679915,5.68180211405501));
#114482=CARTESIAN_POINT('Ctrl Pts',(5.20776958690419,3.459944422,5.41349616449876));
#114483=CARTESIAN_POINT('Ctrl Pts',(5.48793070797208,3.395197164,5.11277808154849));
#114484=CARTESIAN_POINT('Ctrl Pts',(4.52852590289775,3.53021247068103,5.66177564884319));
#114485=CARTESIAN_POINT('Ctrl Pts',(4.53918931444891,3.52794619284054,5.65318033992153));
#114486=CARTESIAN_POINT('Ctrl Pts',(4.549852726,3.525679915,5.644585031));
#114487=CARTESIAN_POINT('Ctrl Pts',(4.859154879,3.459944422,5.395270115));
#114488=CARTESIAN_POINT('Ctrl Pts',(5.139363898,3.395197164,5.11365219));
#114489=CARTESIAN_POINT('',(4.89571222559471,3.52567991503086,5.68172524922569));
#114490=CARTESIAN_POINT('Origin',(-0.110853255847381,3.62494888055425,-0.153022410279826));
#114491=CARTESIAN_POINT('',(4.7227824735572,3.52567991373765,5.66315514195599));
#114492=CARTESIAN_POINT('Origin',(-7.41594285980085E-13,3.61749373599945,
-6.34041430469523E-13));
#114493=CARTESIAN_POINT('',(5.31083089400444,3.61640598738723,5.29576011612747));
#114494=CARTESIAN_POINT('Origin',(-0.135360135003075,3.62499784668088,-0.136937159235024));
#114495=CARTESIAN_POINT('Origin',(-0.119649928874311,3.48215430814406,-0.149581986761579));
#114496=CARTESIAN_POINT('Ctrl Pts',(3.837647923,3.395189501,6.443792239));
#114497=CARTESIAN_POINT('Ctrl Pts',(4.187486522,3.460370723,6.235443285));
#114498=CARTESIAN_POINT('Ctrl Pts',(4.512712514,3.525679915,5.990444538));
#114499=CARTESIAN_POINT('Ctrl Pts',(3.912013447,3.395189501,6.103986467));
#114500=CARTESIAN_POINT('Ctrl Pts',(4.243403721,3.460370723,5.89160015));
#114501=CARTESIAN_POINT('Ctrl Pts',(4.549852726,3.525679915,5.644585031));
#114502=CARTESIAN_POINT('',(4.5127125047959,3.52567991637267,5.99044454340971));
#114503=CARTESIAN_POINT('',(4.53128260996699,3.52567991706892,5.81751479231475));
#114504=CARTESIAN_POINT('',(4.04955759272161,3.43511457319818,6.31277142654194));
#114505=CARTESIAN_POINT('Origin',(-0.110510112930169,3.48214119229473,-0.158303805610382));
#114506=CARTESIAN_POINT('Ctrl Pts',(3.91595789455974,3.39596551410652,6.10145669238762));
#114507=CARTESIAN_POINT('Ctrl Pts',(3.93815431206374,3.40280154626537,6.13665211314041));
#114508=CARTESIAN_POINT('Ctrl Pts',(3.96039881813328,3.40947721889377,6.17187681583231));
#114509=CARTESIAN_POINT('Ctrl Pts',(4.00492638196425,3.42251694824804,6.2423031459704));
#114510=CARTESIAN_POINT('Ctrl Pts',(4.02723360296451,3.42888807475989,6.27754298333113));
#114511=CARTESIAN_POINT('Ctrl Pts',(4.04955758846055,3.43511457409361,6.31277142908387));
#114512=CARTESIAN_POINT('Ctrl Pts',(3.53559029459435,3.53021247059306,6.61500472694062));
#114513=CARTESIAN_POINT('Ctrl Pts',(3.54806155060326,3.52794619279656,6.60827838200748));
#114514=CARTESIAN_POINT('Ctrl Pts',(3.56053280661218,3.525679915,6.60155203707424));
#114515=CARTESIAN_POINT('Ctrl Pts',(3.92227317371199,3.459944422,6.4064481530995));
#114516=CARTESIAN_POINT('Ctrl Pts',(4.26052978288272,3.395197164,6.17298705222511));
#114517=CARTESIAN_POINT('Ctrl Pts',(3.20553707987759,3.53021247059306,6.50290568697574));
#114518=CARTESIAN_POINT('Ctrl Pts',(3.21779892393879,3.52794619279656,6.4968036499879));
#114519=CARTESIAN_POINT('Ctrl Pts',(3.230060768,3.525679915,6.490701613));
#114520=CARTESIAN_POINT('Ctrl Pts',(3.585726947,3.459944422,6.313706361));
#114521=CARTESIAN_POINT('Ctrl Pts',(3.919924364,3.395197164,6.098909163));
#114522=CARTESIAN_POINT('',(3.55985021551222,3.52567991503086,6.60132308264157));
#114523=CARTESIAN_POINT('Origin',(-0.0753663511695235,3.62494888555094,
-0.173275155946407));
#114524=CARTESIAN_POINT('',(3.39495548913079,3.52567991373766,6.54601234906258));
#114525=CARTESIAN_POINT('Origin',(4.4799233767101E-13,3.617493736,7.91467585914418E-13));
#114526=CARTESIAN_POINT('',(4.04823473517133,3.61640598738359,6.313619843195));
#114527=CARTESIAN_POINT('Origin',(-0.10275807953716,3.62499778990581,-0.162834087887939));
#114528=CARTESIAN_POINT('Origin',(-0.0846966427635254,3.48215434346587,
-0.171805656129049));
#114529=CARTESIAN_POINT('Ctrl Pts',(2.362700993,3.395189501,7.118120821));
#114530=CARTESIAN_POINT('Ctrl Pts',(2.749149426,3.460370723,6.989847907));
#114531=CARTESIAN_POINT('Ctrl Pts',(3.119439304,3.525679915,6.82049107000001));
#114532=CARTESIAN_POINT('Ctrl Pts',(2.508376089,3.395189501,6.802245908));
#114533=CARTESIAN_POINT('Ctrl Pts',(2.877675422,3.460370723,6.66606417800001));
#114534=CARTESIAN_POINT('Ctrl Pts',(3.230060768,3.525679915,6.490701613));
#114535=CARTESIAN_POINT('',(3.1194392938772,3.52567991637269,6.82049107327703));
#114536=CARTESIAN_POINT('',(3.17475002452162,3.52567991706892,6.65559634697524));
#114537=CARTESIAN_POINT('',(2.59782193401564,3.43511457318079,7.03571751640869));
#114538=CARTESIAN_POINT('Origin',(-0.0738957832790441,3.48214118551873,
-0.178359144995427));
#114539=CARTESIAN_POINT('Ctrl Pts',(2.51277214422329,3.39596551412194,6.80062321811182));
#114540=CARTESIAN_POINT('Ctrl Pts',(2.52688364670092,3.40280154628805,6.83976736312154));
#114541=CARTESIAN_POINT('Ctrl Pts',(2.54103581861051,3.40947721886961,6.87895044276729));
#114542=CARTESIAN_POINT('Ctrl Pts',(2.56938277353199,3.42251694822021,6.95730235429953));
#114543=CARTESIAN_POINT('Ctrl Pts',(2.58359294074119,3.42888807472082,6.99651369683442));
#114544=CARTESIAN_POINT('Ctrl Pts',(2.59782192937818,3.43511457404109,7.03571751795521));
#114545=CARTESIAN_POINT('Ctrl Pts',(2.03089968052327,3.53021247053072,7.22039699483326));
#114546=CARTESIAN_POINT('Ctrl Pts',(2.04452533064616,3.5279461927654,7.21650885952546));
#114547=CARTESIAN_POINT('Ctrl Pts',(2.05815098076905,3.525679915,7.21262072421754));
#114548=CARTESIAN_POINT('Ctrl Pts',(2.45337562708328,3.459944422,7.09984174574432));
#114549=CARTESIAN_POINT('Ctrl Pts',(2.8339112193165,3.395197164,6.94455400749315));
#114550=CARTESIAN_POINT('Ctrl Pts',(1.73266090633112,3.53021247053073,7.03996708343377));
#114551=CARTESIAN_POINT('Ctrl Pts',(1.74594783266555,3.52794619276539,7.03664364271693));
#114552=CARTESIAN_POINT('Ctrl Pts',(1.759234759,3.525679915,7.033320202));
#114553=CARTESIAN_POINT('Ctrl Pts',(2.144634407,3.459944422,6.936920715));
#114554=CARTESIAN_POINT('Ctrl Pts',(2.517193523,3.395197164,6.798987922));
#114555=CARTESIAN_POINT('',(2.05753356667625,3.52567991503086,7.21225038558017));
#114556=CARTESIAN_POINT('Origin',(-0.0363553141379602,3.62494885502381,
-0.18542562761704));
#114557=CARTESIAN_POINT('',(1.90838416002549,3.52567991373765,7.12278529450262));
#114558=CARTESIAN_POINT('Origin',(3.02709246557953E-13,3.61749373599945,
9.86623976961809E-13));
#114559=CARTESIAN_POINT('',(2.59634761954239,3.61640598744957,7.03626172285194));
#114560=CARTESIAN_POINT('Origin',(-0.0653511308448051,3.62499783906402,
-0.181117100456151));
#114561=CARTESIAN_POINT('Origin',(-0.0457833834977586,3.48215431398279,
-0.185996321826775));
#114562=CARTESIAN_POINT('Ctrl Pts',(0.77727679,3.395189501,7.459613984));
#114563=CARTESIAN_POINT('Ctrl Pts',(1.182265159,3.460370723,7.41741501));
#114564=CARTESIAN_POINT('Ctrl Pts',(1.580304579,3.525679915,7.331619019));
#114565=CARTESIAN_POINT('Ctrl Pts',(0.987449852,3.395189501,7.182439891));
#114566=CARTESIAN_POINT('Ctrl Pts',(1.377390219,3.460370723,7.128830454));
#114567=CARTESIAN_POINT('Ctrl Pts',(1.759234759,3.525679915,7.033320202));
#114568=CARTESIAN_POINT('',(1.58030456839241,3.52567991637267,7.33161902003236));
#114569=CARTESIAN_POINT('',(1.66976965661296,3.52567991706892,7.18246961337972));
#114570=CARTESIAN_POINT('',(1.02461500936863,3.43511457320313,7.42968127573517));
#114571=CARTESIAN_POINT('Origin',(-0.0338261750837945,3.48214117583839,
-0.190074447514669));
#114572=CARTESIAN_POINT('Ctrl Pts',(0.992091959997785,3.39596551403114,
7.18180016033055));
#114573=CARTESIAN_POINT('Ctrl Pts',(0.997458679230474,3.4028015076774,7.22306246019008));
#114574=CARTESIAN_POINT('Ctrl Pts',(1.00285674279637,3.40947714064642,7.26437149719111));
#114575=CARTESIAN_POINT('Ctrl Pts',(1.01369768213607,3.42251694824779,7.34698583753522));
#114576=CARTESIAN_POINT('Ctrl Pts',(1.0191463441452,3.42888807477032,7.38833520666078));
#114577=CARTESIAN_POINT('Ctrl Pts',(1.02461500441485,3.43511457410805,7.42968127625411));
#114578=CARTESIAN_POINT('Ctrl Pts',(0.431246454934853,3.53021247045305,
7.48817152328426));
#114579=CARTESIAN_POINT('Ctrl Pts',(0.445389378855488,3.52794619272655,
7.48730340245222));
#114580=CARTESIAN_POINT('Ctrl Pts',(0.459532302776112,3.525679915,7.48643528162022));
#114581=CARTESIAN_POINT('Ctrl Pts',(0.86976096341033,3.459944422,7.46125462957233));
#114582=CARTESIAN_POINT('Ctrl Pts',(1.27478211834841,3.395197164,7.391401337075));
#114583=CARTESIAN_POINT('Ctrl Pts',(0.178767434650042,3.53021247045304,
7.24784744324904));
#114584=CARTESIAN_POINT('Ctrl Pts',(0.192458161325023,3.52794619272655,
7.2474579991246));
#114585=CARTESIAN_POINT('Ctrl Pts',(0.206148888,3.525679915,7.247068555));
#114586=CARTESIAN_POINT('Ctrl Pts',(0.603261147,3.459944422,7.23577236600001));
#114587=CARTESIAN_POINT('Ctrl Pts',(0.99676151,3.395197164,7.181153563));
#114588=CARTESIAN_POINT('',(0.459008935823992,3.52567991457841,7.48594087527957));
#114589=CARTESIAN_POINT('Origin',(0.00435568230947841,3.62494884631261,
-0.188905893396506));
#114590=CARTESIAN_POINT('',(0.332578908769786,3.52567991373766,7.366504715349));
#114591=CARTESIAN_POINT('Origin',(6.15284732885524E-15,3.617493736,-4.04190569902596E-13));
#114592=CARTESIAN_POINT('',(1.02305817476536,3.61640598740894,7.42989582457253));
#114593=CARTESIAN_POINT('Origin',(-0.024888475145801,3.62499784137454,-0.19093145372851));
#114594=CARTESIAN_POINT('Origin',(-0.00472925965781933,3.4821543278721,
-0.191489718375762));
#114595=CARTESIAN_POINT('Origin',(4.78505852562899E-14,3.61749373599978,
-1.58293517182884E-13));
#114596=CARTESIAN_POINT('',(-0.598068333136022,3.6164059873872,7.47611625540621));
#114597=CARTESIAN_POINT('',(-0.0327234426153162,3.52567991637269,7.499928609745));
#114598=CARTESIAN_POINT('Origin',(0.0167380089118564,3.62499783159569,-0.19181783794649));
#114599=CARTESIAN_POINT('Origin',(0.0365459621040783,3.4821543444113,-0.188029733640196));
#114600=CARTESIAN_POINT('Origin',(0.00782484508443366,3.48214246272938,
-0.19290238903462));
#114601=CARTESIAN_POINT('Ctrl Pts',(-0.844492011,3.395189501,7.452303888));
#114602=CARTESIAN_POINT('Ctrl Pts',(-0.439900514,3.460370723,7.49815203));
#114603=CARTESIAN_POINT('Ctrl Pts',(-0.032723432,3.525679915,7.499928611));
#114604=CARTESIAN_POINT('Ctrl Pts',(-0.579648442,3.395189501,7.226790967));
#114605=CARTESIAN_POINT('Ctrl Pts',(-0.18730022,3.460370723,7.258260542));
#114606=CARTESIAN_POINT('Ctrl Pts',(0.206148888,3.525679915,7.247068555));
#114607=CARTESIAN_POINT('',(0.0867127152835091,3.52567991706892,7.37349858314955));
#114608=CARTESIAN_POINT('Ctrl Pts',(-0.029487061,2.231898283,7.499942034));
#114609=CARTESIAN_POINT('Ctrl Pts',(0.376600717,2.296352134,7.501538624));
#114610=CARTESIAN_POINT('Ctrl Pts',(0.780486766,2.361474582,7.459278813));
#114611=CARTESIAN_POINT('Ctrl Pts',(0.209276124,2.231898283,7.246978923));
#114612=CARTESIAN_POINT('Ctrl Pts',(0.601667098,2.296352134,7.235647572));
#114613=CARTESIAN_POINT('Ctrl Pts',(0.990540534,2.361474582,7.18201430300001));
#114614=CARTESIAN_POINT('',(0.213937949141283,2.23266407427649,7.24684279847903));
#114615=CARTESIAN_POINT('Origin',(-0.0350318282142846,2.4106890065044,-0.193902277117336));
#114616=CARTESIAN_POINT('Ctrl Pts',(0.213937947891224,2.23266407474045,
7.24684279881095));
#114617=CARTESIAN_POINT('Ctrl Pts',(0.215059230318048,2.23947867583925,
7.28843449958464));
#114618=CARTESIAN_POINT('Ctrl Pts',(0.216123655395898,2.24612512499677,
7.33008178274923));
#114619=CARTESIAN_POINT('Ctrl Pts',(0.218146489019095,2.25909150516261,
7.41337727741362));
#114620=CARTESIAN_POINT('Ctrl Pts',(0.219106098113739,2.26541917072379,
7.4550752107625));
#114621=CARTESIAN_POINT('Ctrl Pts',(0.220017220171437,2.27159573038441,
7.49677213338445));
#114622=CARTESIAN_POINT('Ctrl Pts',(1.267805044,2.361474582,7.392068071));
#114623=CARTESIAN_POINT('Ctrl Pts',(1.504915875,2.323357812,7.351401467));
#114624=CARTESIAN_POINT('Ctrl Pts',(1.738933089,2.285714286,7.295622778));
#114625=CARTESIAN_POINT('Ctrl Pts',(1.905464967,2.258926311,7.255929416));
#114626=CARTESIAN_POINT('Ctrl Pts',(2.070012238,2.231887255,7.208678751));
#114627=CARTESIAN_POINT('Ctrl Pts',(0.990540534000001,2.361474582,7.182014303));
#114628=CARTESIAN_POINT('Ctrl Pts',(1.220913599,2.323357812,7.150241342));
#114629=CARTESIAN_POINT('Ctrl Pts',(1.448776863,2.285714286,7.103769816));
#114630=CARTESIAN_POINT('Ctrl Pts',(1.610929454,2.258926311,7.07069964));
#114631=CARTESIAN_POINT('Ctrl Pts',(1.771404205,2.231887255,7.030265083));
#114632=CARTESIAN_POINT('',(1.76679318276177,2.23266407430095,7.03142530562253));
#114633=CARTESIAN_POINT('Ctrl Pts',(1.76679318313451,2.2326640749721,7.03142530665601));
#114634=CARTESIAN_POINT('Ctrl Pts',(1.66111643034258,2.2504649376073,7.05797880923018));
#114635=CARTESIAN_POINT('Ctrl Pts',(1.55505543246003,2.26815682580635,7.08209485553649));
#114636=CARTESIAN_POINT('Ctrl Pts',(1.44877686378956,2.28571428590264,7.10376981601217));
#114637=CARTESIAN_POINT('Ctrl Pts',(1.29741506427075,2.31071959718532,7.13463926700789));
#114638=CARTESIAN_POINT('Ctrl Pts',(1.14451922017561,2.33599777478011,7.16077762395494));
#114639=CARTESIAN_POINT('Ctrl Pts',(0.990540544201328,2.36147458031212,
7.18201430159304));
#114640=CARTESIAN_POINT('Ctrl Pts',(1.82645774549815,2.27159573035706,7.2742045682774));
#114641=CARTESIAN_POINT('Ctrl Pts',(1.81660431901047,2.26541917066066,7.23367836058223));
#114642=CARTESIAN_POINT('Ctrl Pts',(1.80670332189861,2.25909150510592,7.19316158924002));
#114643=CARTESIAN_POINT('Ctrl Pts',(1.78682148080259,2.24612497437885,7.11224740650066));
#114644=CARTESIAN_POINT('Ctrl Pts',(1.77682912854049,2.23947860190669,7.07180313520404));
#114645=CARTESIAN_POINT('Ctrl Pts',(1.76679318370471,2.23266407485744,7.03142530641884));
#114646=CARTESIAN_POINT('Ctrl Pts',(1.583468171,2.231898283,7.330936403));
#114647=CARTESIAN_POINT('Ctrl Pts',(1.980405062,2.296352134,7.245198798));
#114648=CARTESIAN_POINT('Ctrl Pts',(2.365763869,2.361474582,7.117103436));
#114649=CARTESIAN_POINT('Ctrl Pts',(1.762269613,2.231898283,7.032560402));
#114650=CARTESIAN_POINT('Ctrl Pts',(2.1430508,2.296352134,6.937141511));
#114651=CARTESIAN_POINT('Ctrl Pts',(2.511303023,2.361474582,6.801165865));
#114652=CARTESIAN_POINT('Origin',(-0.0758960812681775,2.41068907463865,
-0.181838198609218));
#114653=CARTESIAN_POINT('Ctrl Pts',(2.827240594,2.361474582,6.946705019));
#114654=CARTESIAN_POINT('Ctrl Pts',(3.050065787,2.323357812,6.85601735800001));
#114655=CARTESIAN_POINT('Ctrl Pts',(3.26662104,2.285714286,6.75123596));
#114656=CARTESIAN_POINT('Ctrl Pts',(3.420726596,2.258926311,6.676671176));
#114657=CARTESIAN_POINT('Ctrl Pts',(3.571269346,2.231887255,6.595152406));
#114658=CARTESIAN_POINT('Ctrl Pts',(2.511303023,2.361474582,6.801165865));
#114659=CARTESIAN_POINT('Ctrl Pts',(2.729459846,2.323357812,6.720612339));
#114660=CARTESIAN_POINT('Ctrl Pts',(2.94200579,2.285714286,6.626243425));
#114661=CARTESIAN_POINT('Ctrl Pts',(3.093258233,2.258926311,6.559088397));
#114662=CARTESIAN_POINT('Ctrl Pts',(3.241288939,2.231887255,6.485101851));
#114663=CARTESIAN_POINT('',(3.2370351332511,2.23266407427388,6.487226180923));
#114664=CARTESIAN_POINT('Ctrl Pts',(3.23703513419218,2.23266407494668,6.48722618256281));
#114665=CARTESIAN_POINT('Ctrl Pts',(3.13953726152733,2.25046493790256,6.53587625704972));
#114666=CARTESIAN_POINT('Ctrl Pts',(3.04114014799221,2.26815682610644,6.58222846268839));
#114667=CARTESIAN_POINT('Ctrl Pts',(2.94200578976456,2.28571428604824,6.62624342513513));
#114668=CARTESIAN_POINT('Ctrl Pts',(2.80081876472916,2.31071959711799,6.68892947768875));
#114669=CARTESIAN_POINT('Ctrl Pts',(2.65711651507422,2.3359977746946,6.74732482159475));
#114670=CARTESIAN_POINT('Ctrl Pts',(2.51130303266037,2.36147458031212,6.80116586143295));
#114671=CARTESIAN_POINT('Ctrl Pts',(3.34749513650598,2.27159573034486,6.71150328220306));
#114672=CARTESIAN_POINT('Ctrl Pts',(3.32916014099096,2.26541917064281,6.67404275010762));
#114673=CARTESIAN_POINT('Ctrl Pts',(3.31078071561367,2.25909150509045,6.63660166006047));
#114674=CARTESIAN_POINT('Ctrl Pts',(3.27396951324641,2.24612496366142,6.56185315251622));
#114675=CARTESIAN_POINT('Ctrl Pts',(3.25551646985988,2.23947859656426,6.52450253886267));
#114676=CARTESIAN_POINT('Ctrl Pts',(3.23703513444457,2.23266407473202,6.48722618166756));
#114677=CARTESIAN_POINT('Ctrl Pts',(3.122382191,2.231898283,6.819144334));
#114678=CARTESIAN_POINT('Ctrl Pts',(3.491607867,2.296352134,6.650081528));
#114679=CARTESIAN_POINT('Ctrl Pts',(3.840420483,2.361474582,6.442140212));
#114680=CARTESIAN_POINT('Ctrl Pts',(3.232861335,2.231898283,6.489307173));
#114681=CARTESIAN_POINT('Ctrl Pts',(3.584227827,2.296352134,6.314262424));
#114682=CARTESIAN_POINT('Ctrl Pts',(3.914639774,2.361474582,6.10230247));
#114683=CARTESIAN_POINT('Origin',(-0.113211494847705,2.41068900069649,-0.16127150375959));
#114684=CARTESIAN_POINT('Ctrl Pts',(4.254477516,2.361474582,6.176521761));
#114685=CARTESIAN_POINT('Ctrl Pts',(4.452598014,2.323357812,6.040053497));
#114686=CARTESIAN_POINT('Ctrl Pts',(4.641565421,2.285714286,5.891168852));
#114687=CARTESIAN_POINT('Ctrl Pts',(4.776038851,2.258926311,5.785219212));
#114688=CARTESIAN_POINT('Ctrl Pts',(4.90553787,2.231887255,5.673244064));
#114689=CARTESIAN_POINT('Ctrl Pts',(3.914639774,2.361474582,6.10230247));
#114690=CARTESIAN_POINT('Ctrl Pts',(4.110379585,2.323357812,5.976734973));
#114691=CARTESIAN_POINT('Ctrl Pts',(4.297669796,2.285714286,5.838881257));
#114692=CARTESIAN_POINT('Ctrl Pts',(4.430949694,2.258926311,5.740781472));
#114693=CARTESIAN_POINT('Ctrl Pts',(4.559614604,2.231887255,5.636702463));
#114694=CARTESIAN_POINT('',(4.55591691843822,2.23266407431282,5.63969157044102));
#114695=CARTESIAN_POINT('Ctrl Pts',(4.55591691922223,2.23266407495794,5.63969157124384));
#114696=CARTESIAN_POINT('Ctrl Pts',(4.47115682192384,2.25046493763,5.70816339437997));
#114697=CARTESIAN_POINT('Ctrl Pts',(4.38502453261706,2.26815682582794,5.77458438244212));
#114698=CARTESIAN_POINT('Ctrl Pts',(4.29766979662721,2.28571428587394,5.83888125653835));
#114699=CARTESIAN_POINT('Ctrl Pts',(4.17325929344737,2.31071959707719,5.93045278120617));
#114700=CARTESIAN_POINT('Ctrl Pts',(4.04546999514317,2.33599777466947,6.01837461000912));
#114701=CARTESIAN_POINT('Ctrl Pts',(3.91463978266786,2.36147458031209,6.10230246443955));
#114702=CARTESIAN_POINT('Ctrl Pts',(4.71200737576558,2.27159573036368,5.83497956214766));
#114703=CARTESIAN_POINT('Ctrl Pts',(4.68604813524469,2.26541917068898,5.80233631873936));
#114704=CARTESIAN_POINT('Ctrl Pts',(4.66004968284631,2.25909150510957,5.76972161364608));
#114705=CARTESIAN_POINT('Ctrl Pts',(4.60803103341143,2.24612512498883,5.70463481466443));
#114706=CARTESIAN_POINT('Ctrl Pts',(4.58197979005519,2.23947867584863,5.6721238638597));
#114707=CARTESIAN_POINT('Ctrl Pts',(4.5559169200463,2.23266407478488,5.63969157057813));
#114708=CARTESIAN_POINT('Ctrl Pts',(4.51529709,2.231898283,5.988496655));
#114709=CARTESIAN_POINT('Ctrl Pts',(4.839546969,2.296352134,5.744013838));
#114710=CARTESIAN_POINT('Ctrl Pts',(5.135503304,2.361474582,5.465949672));
#114711=CARTESIAN_POINT('Ctrl Pts',(4.552288053,2.231898283,5.642621154));
#114712=CARTESIAN_POINT('Ctrl Pts',(4.857810345,2.296352134,5.396135444));
#114713=CARTESIAN_POINT('Ctrl Pts',(5.13493232,2.361474582,5.118102194));
#114714=CARTESIAN_POINT('Origin',(-0.145233333309196,2.41068900203097,-0.13316399617367));
#114715=CARTESIAN_POINT('Ctrl Pts',(5.482779798,2.361474582,5.11753121));
#114716=CARTESIAN_POINT('Ctrl Pts',(5.646931706,2.323357812,4.94166344799999));
#114717=CARTESIAN_POINT('Ctrl Pts',(5.799475362,2.285714286,4.755637236));
#114718=CARTESIAN_POINT('Ctrl Pts',(5.908028837,2.258926311,4.623256827));
#114719=CARTESIAN_POINT('Ctrl Pts',(6.010428894,2.231887255,4.486061135));
#114720=CARTESIAN_POINT('Ctrl Pts',(5.13493232,2.361474582,5.118102194));
#114721=CARTESIAN_POINT('Ctrl Pts',(5.299102543,2.323357812,4.953392122));
#114722=CARTESIAN_POINT('Ctrl Pts',(5.452379538,2.285714286,4.77849949));
#114723=CARTESIAN_POINT('Ctrl Pts',(5.561454873,2.258926311,4.654041985));
#114724=CARTESIAN_POINT('Ctrl Pts',(5.664737759,2.231887255,4.52473713300001));
#114725=CARTESIAN_POINT('',(5.66176909176001,2.23266407433869,4.52845125015997));
#114726=CARTESIAN_POINT('Ctrl Pts',(5.66176909332444,2.23266407511861,4.52845125124809));
#114727=CARTESIAN_POINT('Ctrl Pts',(5.59371005768589,2.25046493777582,4.61354315659389));
#114728=CARTESIAN_POINT('Ctrl Pts',(5.52387004230441,2.26815682591767,4.69692715478952));
#114729=CARTESIAN_POINT('Ctrl Pts',(5.45237953861184,2.28571428586119,4.77849948935201));
#114730=CARTESIAN_POINT('Ctrl Pts',(5.35056285566987,2.31071959699885,4.89467470310772));
#114731=CARTESIAN_POINT('Ctrl Pts',(5.24466179475073,2.33599777457497,5.00801189012035));
#114732=CARTESIAN_POINT('Ctrl Pts',(5.13493232726982,2.36147458031211,5.11810218670628));
#114733=CARTESIAN_POINT('Ctrl Pts',(5.85619138690653,2.27159573036205,4.68561868236548));
#114734=CARTESIAN_POINT('Ctrl Pts',(5.82382172662383,2.26541917069934,4.6593190892797));
#114735=CARTESIAN_POINT('Ctrl Pts',(5.79141990591579,2.25909150509652,4.63305579658063));
#114736=CARTESIAN_POINT('Ctrl Pts',(5.72662492635262,2.24612497303148,4.58067254904189));
#114737=CARTESIAN_POINT('Ctrl Pts',(5.69419425737027,2.23947860122615,4.5545222619207));
#114738=CARTESIAN_POINT('Ctrl Pts',(5.66176909363111,2.23266407484144,4.52845125000692));
#114739=CARTESIAN_POINT('Ctrl Pts',(5.697081715,2.231898283,4.87783352800001));
#114740=CARTESIAN_POINT('Ctrl Pts',(5.961194234,2.296352134,4.569362444));
#114741=CARTESIAN_POINT('Ctrl Pts',(6.190455698,2.361474582,4.2341774));
#114742=CARTESIAN_POINT('Ctrl Pts',(5.658854841,2.231898283,4.53209244));
#114743=CARTESIAN_POINT('Ctrl Pts',(5.90424705100001,2.296352134,4.225691167));
#114744=CARTESIAN_POINT('Ctrl Pts',(6.115121138,2.361474582,3.894585148));
#114745=CARTESIAN_POINT('Origin',(-0.170464169393162,2.41068905305429,-0.0988298170244395));
#114746=CARTESIAN_POINT('Ctrl Pts',(6.45471339,2.361474582,3.819250588));
#114747=CARTESIAN_POINT('Ctrl Pts',(6.577221147,2.323357812,3.612206708));
#114748=CARTESIAN_POINT('Ctrl Pts',(6.686208281,2.285714286,3.397737309));
#114749=CARTESIAN_POINT('Ctrl Pts',(6.763765961,2.258926311,3.245116092));
#114750=CARTESIAN_POINT('Ctrl Pts',(6.834278944,2.231887255,3.089114974));
#114751=CARTESIAN_POINT('Ctrl Pts',(6.115121138,2.361474582,3.894585148));
#114752=CARTESIAN_POINT('Ctrl Pts',(6.240045355,2.323357812,3.69843416));
#114753=CARTESIAN_POINT('Ctrl Pts',(6.352142073,2.285714286,3.494680397));
#114754=CARTESIAN_POINT('Ctrl Pts',(6.431912603,2.258926311,3.349684667));
#114755=CARTESIAN_POINT('Ctrl Pts',(6.50498407100001,2.231887255,3.201200124));
#114756=CARTESIAN_POINT('',(6.50288323569477,2.23266407432216,3.20546558258028));
#114757=CARTESIAN_POINT('Ctrl Pts',(6.50288323697012,2.23266407502953,3.2054655830801));
#114758=CARTESIAN_POINT('Ctrl Pts',(6.45470762816993,2.25046493780333,3.30319876787987));
#114759=CARTESIAN_POINT('Ctrl Pts',(6.40442552820004,2.26815682598676,3.39964683318256));
#114760=CARTESIAN_POINT('Ctrl Pts',(6.35214207326452,2.28571428606369,3.49468039721292));
#114761=CARTESIAN_POINT('Ctrl Pts',(6.27768004475488,2.31071959737376,3.63002707721038));
#114762=CARTESIAN_POINT('Ctrl Pts',(6.19861903637983,2.33599777477379,3.76348010121415));
#114763=CARTESIAN_POINT('Ctrl Pts',(6.11512114353184,2.36147458031213,3.89458513931412));
#114764=CARTESIAN_POINT('Ctrl Pts',(6.72654639743712,2.27159573032736,3.31716348119342));
#114765=CARTESIAN_POINT('Ctrl Pts',(6.68927988679343,2.26541917067551,3.29843727796667));
#114766=CARTESIAN_POINT('Ctrl Pts',(6.65198977122115,2.25909150509326,3.2797534400945));
#114767=CARTESIAN_POINT('Ctrl Pts',(6.57744881346161,2.24612497317182,3.24252388941654));
#114768=CARTESIAN_POINT('Ctrl Pts',(6.5401548165271,2.23947860131222,3.22395661652792));
#114769=CARTESIAN_POINT('Ctrl Pts',(6.50288323776577,2.23266407482983,3.205465581897));
#114770=CARTESIAN_POINT('Ctrl Pts',(6.612477132,2.231898283,3.539088327));
#114771=CARTESIAN_POINT('Ctrl Pts',(6.804102681,2.296352134,3.18105274));
#114772=CARTESIAN_POINT('Ctrl Pts',(6.955949263,2.361474582,2.804419699));
#114773=CARTESIAN_POINT('Ctrl Pts',(6.500819867,2.231898283,3.209648121));
#114774=CARTESIAN_POINT('Ctrl Pts',(6.67460772600001,2.296352134,2.857658268));
#114775=CARTESIAN_POINT('Ctrl Pts',(6.809373687,2.361474582,2.488961628));
#114776=CARTESIAN_POINT('Origin',(-0.187724371365596,2.41068903802582,-0.059874491679216));
#114777=CARTESIAN_POINT('Ctrl Pts',(7.124831758,2.361474582,2.342386053));
#114778=CARTESIAN_POINT('Ctrl Pts',(7.199967038,2.323357812,2.113847197));
#114779=CARTESIAN_POINT('Ctrl Pts',(7.260301532,2.285714286,1.880962961));
#114780=CARTESIAN_POINT('Ctrl Pts',(7.303236907,2.258926311,1.715237335));
#114781=CARTESIAN_POINT('Ctrl Pts',(7.338565706,2.231887255,1.547725229));
#114782=CARTESIAN_POINT('Ctrl Pts',(6.809373687,2.361474582,2.488961628));
#114783=CARTESIAN_POINT('Ctrl Pts',(6.889210582,2.323357812,2.270541528));
#114784=CARTESIAN_POINT('Ctrl Pts',(6.954885505,2.285714286,2.047453934));
#114785=CARTESIAN_POINT('Ctrl Pts',(7.001621248,2.258926311,1.888699818));
#114786=CARTESIAN_POINT('Ctrl Pts',(7.04106455800001,2.231887255,1.727978555));
#114787=CARTESIAN_POINT('',(7.03992978615661,2.23266407431315,1.73259590695452));
#114788=CARTESIAN_POINT('Ctrl Pts',(7.03992978791672,2.23266407503294,1.73259590726661));
#114789=CARTESIAN_POINT('Ctrl Pts',(7.01389024407878,2.25046493769433,1.83840047597408));
#114790=CARTESIAN_POINT('Ctrl Pts',(6.98551719494212,2.2681568258671,1.94340280424178));
#114791=CARTESIAN_POINT('Ctrl Pts',(6.95488550524722,2.28571428596627,2.04745393369742));
#114792=CARTESIAN_POINT('Ctrl Pts',(6.91125989250801,2.31071959731997,2.19564341897167));
#114793=CARTESIAN_POINT('Ctrl Pts',(6.86273574210138,2.33599777471104,2.34297216457218));
#114794=CARTESIAN_POINT('Ctrl Pts',(6.80937369053531,2.36147458031212,2.48896161832797));
#114795=CARTESIAN_POINT('Ctrl Pts',(7.28237557417371,2.27159573035333,1.7936014024457));
#114796=CARTESIAN_POINT('Ctrl Pts',(7.24195475347828,2.26541917064691,1.78332420566177));
#114797=CARTESIAN_POINT('Ctrl Pts',(7.20151998735164,2.25909150506858,1.7730934581438));
#114798=CARTESIAN_POINT('Ctrl Pts',(7.12071848928356,2.24612497095763,1.75275841277512));
#114799=CARTESIAN_POINT('Ctrl Pts',(7.08030499745313,2.2394786001742,1.74264234112778));
#114800=CARTESIAN_POINT('Ctrl Pts',(7.03992978796534,2.23266407477575,1.73259590593616));
#114801=CARTESIAN_POINT('Ctrl Pts',(7.218680466,2.231898283,2.034859288));
#114802=CARTESIAN_POINT('Ctrl Pts',(7.328858849,2.296352134,1.644000547));
#114803=CARTESIAN_POINT('Ctrl Pts',(7.39619037200001,2.361474582,1.24353045));
#114804=CARTESIAN_POINT('Ctrl Pts',(7.03881378000001,2.231898283,1.737124223));
#114805=CARTESIAN_POINT('Ctrl Pts',(7.13287116300001,2.296352134,1.356004445));
#114806=CARTESIAN_POINT('Ctrl Pts',(7.185227491,2.361474582,0.96695703));
#114807=CARTESIAN_POINT('Origin',(-0.196206385030984,2.41068903913982,-0.0181194093584404));
#114808=CARTESIAN_POINT('Ctrl Pts',(7.461800912,2.361474582,0.755994149));
#114809=CARTESIAN_POINT('Ctrl Pts',(7.486050472,2.323357812,0.516646541000001));
#114810=CARTESIAN_POINT('Ctrl Pts',(7.494911153,2.285714286,0.276236876));
#114811=CARTESIAN_POINT('Ctrl Pts',(7.501216611,2.258926311,0.105155986));
#114812=CARTESIAN_POINT('Ctrl Pts',(7.499709291,2.231887255,-0.066034427));
#114813=CARTESIAN_POINT('Ctrl Pts',(7.18522749100001,2.361474582,0.96695703));
#114814=CARTESIAN_POINT('Ctrl Pts',(7.216243979,2.323357812,0.736480897));
#114815=CARTESIAN_POINT('Ctrl Pts',(7.23242622,2.285714286,0.5044908));
#114816=CARTESIAN_POINT('Ctrl Pts',(7.243941865,2.258926311,0.339401464));
#114817=CARTESIAN_POINT('Ctrl Pts',(7.247912692,2.231887255,0.173958629));
#114818=CARTESIAN_POINT('',(7.2477970451692,2.23266407429643,0.178711971874644));
#114819=CARTESIAN_POINT('Ctrl Pts',(7.24779704645978,2.23266407497284,0.178711971795929));
#114820=CARTESIAN_POINT('Ctrl Pts',(7.24511114718299,2.25046493769331,0.287640621109034));
#114821=CARTESIAN_POINT('Ctrl Pts',(7.23997384111706,2.26815682588451,0.396287419958082));
#114822=CARTESIAN_POINT('Ctrl Pts',(7.23242622039952,2.2857142860497,0.504490799940314));
#114823=CARTESIAN_POINT('Ctrl Pts',(7.2216769093882,2.31071959743364,0.658593914725088));
#114824=CARTESIAN_POINT('Ctrl Pts',(7.20595855182678,2.33599777477318,0.812909454265743));
#114825=CARTESIAN_POINT('Ctrl Pts',(7.18522749238694,2.36147458029557,0.966957019694019));
#114826=CARTESIAN_POINT('Ctrl Pts',(7.49768896349729,2.27159573034331,0.186172514983504));
#114827=CARTESIAN_POINT('Ctrl Pts',(7.45600386576791,2.26541917068799,0.184824874870608));
#114828=CARTESIAN_POINT('Ctrl Pts',(7.41431513363566,2.25909150511074,0.183525596002686));
#114829=CARTESIAN_POINT('Ctrl Pts',(7.33103228497458,2.24612512496663,0.181035935895053));
#114830=CARTESIAN_POINT('Ctrl Pts',(7.28938845439867,2.23947867582963,0.179844061553129));
#114831=CARTESIAN_POINT('Ctrl Pts',(7.24779704649391,2.23266407474667,0.178711970411905));
#114832=CARTESIAN_POINT('Ctrl Pts',(7.487346326,2.231898283,0.435482491));
#114833=CARTESIAN_POINT('Ctrl Pts',(7.51092572300001,2.296352134,0.030076714));
#114834=CARTESIAN_POINT('Ctrl Pts',(7.49059384,2.361474582,-0.375504901));
#114835=CARTESIAN_POINT('Ctrl Pts',(7.247680585,2.231898283,0.183374327));
#114836=CARTESIAN_POINT('Ctrl Pts',(7.257609471,2.296352134,-0.209054639));
#114837=CARTESIAN_POINT('Ctrl Pts',(7.225108044,2.361474582,-0.600261405));
#114838=CARTESIAN_POINT('Origin',(-0.195514704584165,2.41068902671274,0.024482796679206));
#114839=CARTESIAN_POINT('Ctrl Pts',(7.449864548,2.361474582,-0.865747201));
#114840=CARTESIAN_POINT('Ctrl Pts',(7.422094506,2.323357812,-1.104711934));
#114841=CARTESIAN_POINT('Ctrl Pts',(7.379067058,2.285714286,-1.341405739));
#114842=CARTESIAN_POINT('Ctrl Pts',(7.348447764,2.258926311,-1.509842339));
#114843=CARTESIAN_POINT('Ctrl Pts',(7.310174806,2.231887255,-1.676706386));
#114844=CARTESIAN_POINT('Ctrl Pts',(7.22510804400001,2.361474582,-0.600261405));
#114845=CARTESIAN_POINT('Ctrl Pts',(7.205853827,2.323357812,-0.832016762));
#114846=CARTESIAN_POINT('Ctrl Pts',(7.171786724,2.285714286,-1.062061763));
#114847=CARTESIAN_POINT('Ctrl Pts',(7.147543812,2.258926311,-1.225766926));
#114848=CARTESIAN_POINT('Ctrl Pts',(7.115856484,2.231887255,-1.38819541));
#114849=CARTESIAN_POINT('',(7.11676536944114,2.23266407431948,-1.38352833649661));
#114850=CARTESIAN_POINT('Ctrl Pts',(7.11676537048806,2.23266407505902,-1.38352833682321));
#114851=CARTESIAN_POINT('Ctrl Pts',(7.13755870587416,2.25046493778714,-1.27656898971806));
#114852=CARTESIAN_POINT('Ctrl Pts',(7.15589735726919,2.26815682595888,-1.16935792323182));
#114853=CARTESIAN_POINT('Ctrl Pts',(7.17178672398835,2.28571428598712,-1.06206176307869));
#114854=CARTESIAN_POINT('Ctrl Pts',(7.19441633923325,2.31071959711604,-0.909250710690481));
#114855=CARTESIAN_POINT('Ctrl Pts',(7.21223874829608,2.33599777471621,-0.755163999525554));
#114856=CARTESIAN_POINT('Ctrl Pts',(7.22510804314739,2.36147458031212,-0.600261415262548));
#114857=CARTESIAN_POINT('Ctrl Pts',(7.36241874941791,2.27159573033712,-1.42996159172988));
#114858=CARTESIAN_POINT('Ctrl Pts',(7.32141852321828,2.26541917064899,-1.42231666083323));
#114859=CARTESIAN_POINT('Ctrl Pts',(7.28042514401651,2.25909150509139,-1.4146237181863));
#114860=CARTESIAN_POINT('Ctrl Pts',(7.19855320613131,2.2461249677874,-1.39915163326171));
#114861=CARTESIAN_POINT('Ctrl Pts',(7.15762729706395,2.23947859868821,-1.39136354853802));
#114862=CARTESIAN_POINT('Ctrl Pts',(7.11676537024756,2.23266407490757,-1.38352833763891));
#114863=CARTESIAN_POINT('Ctrl Pts',(7.405912192,2.231898283,-1.184256983));
#114864=CARTESIAN_POINT('Ctrl Pts',(7.341790058,2.296352134,-1.585253472));
#114865=CARTESIAN_POINT('Ctrl Pts',(7.234745464,2.361474582,-1.97698206));
#114866=CARTESIAN_POINT('Ctrl Pts',(7.1176539,2.231898283,-1.378949948));
#114867=CARTESIAN_POINT('Ctrl Pts',(7.042990027,2.296352134,-1.764338561));
#114868=CARTESIAN_POINT('Ctrl Pts',(6.92715057400001,2.361474582,-2.139412284));
#114869=CARTESIAN_POINT('Origin',(-0.185680398792335,2.41068904855154,0.0659402369516504));
#114870=CARTESIAN_POINT('Ctrl Pts',(7.089580798,2.361474582,-2.447007174));
#114871=CARTESIAN_POINT('Ctrl Pts',(7.011089651,2.323357812,-2.674415306));
#114872=CARTESIAN_POINT('Ctrl Pts',(6.918185988,2.285714286,-2.896325712));
#114873=CARTESIAN_POINT('Ctrl Pts',(6.852073667,2.258926311,-3.054242115));
#114874=CARTESIAN_POINT('Ctrl Pts',(6.778824671,2.231887255,-3.208977419));
#114875=CARTESIAN_POINT('Ctrl Pts',(6.927150574,2.361474582,-2.139412284));
#114876=CARTESIAN_POINT('Ctrl Pts',(6.85852596,2.323357812,-2.361610241));
#114877=CARTESIAN_POINT('Ctrl Pts',(6.775802451,2.285714286,-2.578953498));
#114878=CARTESIAN_POINT('Ctrl Pts',(6.716934554,2.258926311,-2.733619816));
#114879=CARTESIAN_POINT('Ctrl Pts',(6.651070736,2.231887255,-2.885438973));
#114880=CARTESIAN_POINT('',(6.65296165417311,2.23266407429542,-2.88107639695278));
#114881=CARTESIAN_POINT('Ctrl Pts',(6.65296165572569,2.2326640749522,-2.88107639774204));
#114882=CARTESIAN_POINT('Ctrl Pts',(6.69626195237868,2.25046493781858,-2.78108765271941));
#114883=CARTESIAN_POINT('Ctrl Pts',(6.7372190663883,2.26815682601796,-2.68032538955622));
#114884=CARTESIAN_POINT('Ctrl Pts',(6.77580245113989,2.28571428600938,-2.5789534982117));
#114885=CARTESIAN_POINT('Ctrl Pts',(6.83075285835864,2.31071959717538,-2.43457978113306));
#114886=CARTESIAN_POINT('Ctrl Pts',(6.88128267700351,2.33599777462944,-2.28792682359601));
#114887=CARTESIAN_POINT('Ctrl Pts',(6.92715057096117,2.36147458031212,-2.13941229383932));
#114888=CARTESIAN_POINT('Ctrl Pts',(6.88289001768539,2.2715957303853,-2.97923228418401));
#114889=CARTESIAN_POINT('Ctrl Pts',(6.84449178839268,2.26541917071604,-2.96295225085749));
#114890=CARTESIAN_POINT('Ctrl Pts',(6.80611056655863,2.25909150509519,-2.94662680000792));
#114891=CARTESIAN_POINT('Ctrl Pts',(6.72947874958299,2.24612496091193,-2.91391637996682));
#114892=CARTESIAN_POINT('Ctrl Pts',(6.69118389512109,2.23947859526083,-2.89751252473308));
#114893=CARTESIAN_POINT('Ctrl Pts',(6.65296165534006,2.23266407482084,-2.88107639831275));
#114894=CARTESIAN_POINT('Ctrl Pts',(6.978185836,2.231898283,-2.748621917));
#114895=CARTESIAN_POINT('Ctrl Pts',(6.82936045,2.296352134,-3.126458967));
#114896=CARTESIAN_POINT('Ctrl Pts',(6.640608432,2.361474582,-3.486017736));
#114897=CARTESIAN_POINT('Ctrl Pts',(6.65481363,2.231898283,-2.876796057));
#114898=CARTESIAN_POINT('Ctrl Pts',(6.499048197,2.296352134,-3.237123972));
#114899=CARTESIAN_POINT('Ctrl Pts',(6.305287243,2.361474582,-3.578526622));
#114900=CARTESIAN_POINT('Origin',(-0.167164222466163,2.41068902856424,0.104314448275361));
#114901=CARTESIAN_POINT('Ctrl Pts',(6.397796129,2.361474582,-3.913847811));
#114902=CARTESIAN_POINT('Ctrl Pts',(6.272254035,2.323357812,-4.119065991));
#114903=CARTESIAN_POINT('Ctrl Pts',(6.133818231,2.285714286,-4.315816714));
#114904=CARTESIAN_POINT('Ctrl Pts',(6.03530422,2.258926311,-4.455828924));
#114905=CARTESIAN_POINT('Ctrl Pts',(5.93050422900001,2.231887255,-4.59120023400001));
#114906=CARTESIAN_POINT('Ctrl Pts',(6.30528724300001,2.361474582,-3.578526622));
#114907=CARTESIAN_POINT('Ctrl Pts',(6.190501041,2.323357812,-3.780777451));
#114908=CARTESIAN_POINT('Ctrl Pts',(6.062989186,2.285714286,-3.975256234));
#114909=CARTESIAN_POINT('Ctrl Pts',(5.972248902,2.258926311,-4.113651681));
#114910=CARTESIAN_POINT('Ctrl Pts',(5.875288312,2.231887255,-4.247762617));
#114911=CARTESIAN_POINT('',(5.87807284653492,2.23266407431278,-4.24390852719617));
#114912=CARTESIAN_POINT('Ctrl Pts',(5.87807284777009,2.23266407494115,-4.24390852821457));
#114913=CARTESIAN_POINT('Ctrl Pts',(5.94185543176464,2.25046493763868,-4.1555657488572));
#114914=CARTESIAN_POINT('Ctrl Pts',(6.00351589915871,2.26815682584352,-4.06596382001813));
#114915=CARTESIAN_POINT('Ctrl Pts',(6.06298918606306,2.28571428599601,-3.97525623438882));
#114916=CARTESIAN_POINT('Ctrl Pts',(6.14769096577208,2.31071959740257,-3.84607060732515));
#114917=CARTESIAN_POINT('Ctrl Pts',(6.22856547567653,2.33599777468241,-3.71370873206035));
#114918=CARTESIAN_POINT('Ctrl Pts',(6.30528723791706,2.36147458031212,-3.57852663095604));
#114919=CARTESIAN_POINT('Ctrl Pts',(6.08152499814079,2.27159573036892,-4.38919738580205));
#114920=CARTESIAN_POINT('Ctrl Pts',(6.0475242237988,2.26541917066132,-4.36504348623608));
#114921=CARTESIAN_POINT('Ctrl Pts',(6.01354982319035,2.25909150506665,-4.34084888729227));
#114922=CARTESIAN_POINT('Ctrl Pts',(5.94574154086183,2.24612498991411,-4.29242975155489));
#114923=CARTESIAN_POINT('Ctrl Pts',(5.91186826160298,2.23947860946582,-4.26817708978734));
#114924=CARTESIAN_POINT('Ctrl Pts',(5.87807284692885,2.23266407475115,-4.24390852816372));
#114925=CARTESIAN_POINT('Ctrl Pts',(6.224167265,2.231898283,-4.184464345));
#114926=CARTESIAN_POINT('Ctrl Pts',(5.997597537,2.296352134,-4.521474716));
#114927=CARTESIAN_POINT('Ctrl Pts',(5.73596393,2.361474582,-4.832051096));
#114928=CARTESIAN_POINT('Ctrl Pts',(5.88080167,2.231898283,-4.240126379));
#114929=CARTESIAN_POINT('Ctrl Pts',(5.651218096,2.296352134,-4.558545065));
#114930=CARTESIAN_POINT('Ctrl Pts',(5.38859568799999,2.361474582,-4.850313032));
#114931=CARTESIAN_POINT('Origin',(-0.140831315020765,2.41068907822503,0.137810861324849));
#114932=CARTESIAN_POINT('Ctrl Pts',(5.406857624,2.361474582,-5.197681275));
#114933=CARTESIAN_POINT('Ctrl Pts',(5.240134792,2.323357812,-5.371113728));
#114934=CARTESIAN_POINT('Ctrl Pts',(5.062639951,2.285714286,-5.533504923));
#114935=CARTESIAN_POINT('Ctrl Pts',(4.936330656,2.258926311,-5.649066125));
#114936=CARTESIAN_POINT('Ctrl Pts',(4.804880001,2.231887255,-5.75874362900001));
#114937=CARTESIAN_POINT('Ctrl Pts',(5.388595688,2.361474582,-4.850313032));
#114938=CARTESIAN_POINT('Ctrl Pts',(5.233015174,2.323357812,-5.023159709));
#114939=CARTESIAN_POINT('Ctrl Pts',(5.066677286,2.285714286,-5.185680407));
#114940=CARTESIAN_POINT('Ctrl Pts',(4.948307528,2.258926311,-5.301333767));
#114941=CARTESIAN_POINT('Ctrl Pts',(4.824783936,2.231887255,-5.411465603));
#114942=CARTESIAN_POINT('',(4.82833188580182,2.23266407432321,-5.40830021117995));
#114943=CARTESIAN_POINT('Ctrl Pts',(4.82833188697985,2.23266407514971,-5.40830021270223));
#114944=CARTESIAN_POINT('Ctrl Pts',(4.90961435553651,2.25046493782872,-5.33573420872998));
#114945=CARTESIAN_POINT('Ctrl Pts',(4.98909500158218,2.26815682596581,-5.26148230116632));
#114946=CARTESIAN_POINT('Ctrl Pts',(5.06667728571463,2.28571428593542,-5.18568040727882));
#114947=CARTESIAN_POINT('Ctrl Pts',(5.17716987488111,2.31071959712958,-5.07772344732761));
#114948=CARTESIAN_POINT('Ctrl Pts',(5.28460747541412,2.33599777470134,-4.9658417475096));
#114949=CARTESIAN_POINT('Ctrl Pts',(5.38859568103647,2.36147458029396,-4.85031303973633));
#114950=CARTESIAN_POINT('Ctrl Pts',(4.99579462933249,2.27159573035622,-5.5939284962985));
#114951=CARTESIAN_POINT('Ctrl Pts',(4.96778114863446,2.26541917067387,-5.5630301401288));
#114952=CARTESIAN_POINT('Ctrl Pts',(4.93980217415092,2.25909150509699,-5.53209770567045));
#114953=CARTESIAN_POINT('Ctrl Pts',(4.88398774231265,2.24612495461544,-5.47023363762829));
#114954=CARTESIAN_POINT('Ctrl Pts',(4.85612008818721,2.23947859218347,-5.43926632584869));
#114955=CARTESIAN_POINT('Ctrl Pts',(4.82833188556729,2.23266407483626,-5.40830021364951));
#114956=CARTESIAN_POINT('Ctrl Pts',(5.179113551,2.231898283,-5.424645871));
#114957=CARTESIAN_POINT('Ctrl Pts',(4.88539363,2.296352134,-5.70507133300001));
#114958=CARTESIAN_POINT('Ctrl Pts',(4.563112129,2.361474582,-5.952143118));
#114959=CARTESIAN_POINT('Ctrl Pts',(4.831809961,2.231898283,-5.405193105));
#114960=CARTESIAN_POINT('Ctrl Pts',(4.539143318,2.296352134,-5.666813656));
#114961=CARTESIAN_POINT('Ctrl Pts',(4.219939387,2.361474582,-5.895304196));
#114962=CARTESIAN_POINT('Origin',(-0.107913617262737,2.41068904470201,0.164863647007863));
#114963=CARTESIAN_POINT('Ctrl Pts',(4.163100466,2.361474582,-6.238476938));
#114964=CARTESIAN_POINT('Ctrl Pts',(3.96299267,2.323357812,-6.372014157));
#114965=CARTESIAN_POINT('Ctrl Pts',(3.754738253,2.285714286,-6.492452591));
#114966=CARTESIAN_POINT('Ctrl Pts',(3.606539757,2.258926311,-6.578159272));
#114967=CARTESIAN_POINT('Ctrl Pts',(3.454584923,2.231887255,-6.657014572));
#114968=CARTESIAN_POINT('Ctrl Pts',(4.219939387,2.361474582,-5.895304196));
#114969=CARTESIAN_POINT('Ctrl Pts',(4.030839333,2.323357812,-6.030664602));
#114970=CARTESIAN_POINT('Ctrl Pts',(3.833453187,2.285714286,-6.153627927));
#114971=CARTESIAN_POINT('Ctrl Pts',(3.692988795,2.258926311,-6.241131377));
#114972=CARTESIAN_POINT('Ctrl Pts',(3.548678026,2.231887255,-6.322134471));
#114973=CARTESIAN_POINT('',(3.55282349234905,2.23266407432664,-6.31980578879384));
#114974=CARTESIAN_POINT('Ctrl Pts',(3.55282349310941,2.23266407512854,-6.3198057904137));
#114975=CARTESIAN_POINT('Ctrl Pts',(3.64780516867989,2.25046493775314,-6.26640966745086));
#114976=CARTESIAN_POINT('Ctrl Pts',(3.7413895667195,2.26815682589727,-6.21097971756903));
#114977=CARTESIAN_POINT('Ctrl Pts',(3.83345318643646,2.28571428589253,-6.15362792735106));
#114978=CARTESIAN_POINT('Ctrl Pts',(3.96457007518036,2.31071959710664,-6.07194758186058));
#114979=CARTESIAN_POINT('Ctrl Pts',(4.09354710207664,2.33599777463646,-5.98577752262925));
#114980=CARTESIAN_POINT('Ctrl Pts',(4.21993937862631,2.36147458031212,-5.89530420199401));
#114981=CARTESIAN_POINT('Ctrl Pts',(3.67646645566478,2.27159573037149,-6.53709372734915));
#114982=CARTESIAN_POINT('Ctrl Pts',(3.65575014805859,2.26541917073199,-6.50089568752884));
#114983=CARTESIAN_POINT('Ctrl Pts',(3.63507486542068,2.25909150510569,-6.46467178342126));
#114984=CARTESIAN_POINT('Ctrl Pts',(3.5938643406885,2.24612497056415,-6.39225569889695));
#114985=CARTESIAN_POINT('Ctrl Pts',(3.57330524632176,2.23947860000625,-6.35602161625964));
#114986=CARTESIAN_POINT('Ctrl Pts',(3.55282349163871,2.2326640748214,-6.31980579073514));
#114987=CARTESIAN_POINT('Ctrl Pts',(3.891890244,2.231898283,-6.41117698500001));
#114988=CARTESIAN_POINT('Ctrl Pts',(3.544754146,2.296352134,-6.621905155));
#114989=CARTESIAN_POINT('Ctrl Pts',(3.176894277,2.361474582,-6.793919543));
#114990=CARTESIAN_POINT('Ctrl Pts',(3.556888188,2.231898283,-6.317519008));
#114991=CARTESIAN_POINT('Ctrl Pts',(3.214823244,2.296352134,-6.510108339));
#114992=CARTESIAN_POINT('Ctrl Pts',(2.853963411,2.361474582,-6.664637488));
#114993=CARTESIAN_POINT('Origin',(-0.0699498367566476,2.41068901350358,
0.184207422519518));
#114994=CARTESIAN_POINT('Ctrl Pts',(2.724681357,2.361474582,-6.98756835400001));
#114995=CARTESIAN_POINT('Ctrl Pts',(2.500545415,2.323357812,-7.074966286));
#114996=CARTESIAN_POINT('Ctrl Pts',(2.271269168,2.285714286,-7.147820393));
#114997=CARTESIAN_POINT('Ctrl Pts',(2.108111067,2.258926311,-7.199665003));
#114998=CARTESIAN_POINT('Ctrl Pts',(1.942757295,2.231887255,-7.244010912));
#114999=CARTESIAN_POINT('Ctrl Pts',(2.853963411,2.361474582,-6.664637488));
#115000=CARTESIAN_POINT('Ctrl Pts',(2.640185925,2.323357812,-6.75618232100001));
#115001=CARTESIAN_POINT('Ctrl Pts',(2.420981077,2.285714286,-6.833838645));
#115002=CARTESIAN_POINT('Ctrl Pts',(2.264990009,2.258926311,-6.88910062));
#115003=CARTESIAN_POINT('Ctrl Pts',(2.106639876,2.231887255,-6.937187358));
#115004=CARTESIAN_POINT('',(2.11118902096935,2.23266407433893,-6.93580427183575));
#115005=CARTESIAN_POINT('Ctrl Pts',(2.11118902140619,2.23266407505294,-6.93580427367143));
#115006=CARTESIAN_POINT('Ctrl Pts',(2.2154286670018,2.25046493793859,-6.90407477398938));
#115007=CARTESIAN_POINT('Ctrl Pts',(2.31874091402043,2.26815682610242,-6.87005862536604));
#115008=CARTESIAN_POINT('Ctrl Pts',(2.42098107672611,2.28571428598661,-6.8338386454385));
#115009=CARTESIAN_POINT('Ctrl Pts',(2.5665913847569,2.31071959703924,-6.78225419630704));
#115010=CARTESIAN_POINT('Ctrl Pts',(2.71107701654516,2.33599777463872,-6.72582499334375));
#115011=CARTESIAN_POINT('Ctrl Pts',(2.85396340153355,2.36147458031212,-6.66463749205377));
#115012=CARTESIAN_POINT('Ctrl Pts',(2.18523079690101,2.27159573033634,-7.17459172099152));
#115013=CARTESIAN_POINT('Ctrl Pts',(2.17278033336348,2.2654191706762,-7.13478657730633));
#115014=CARTESIAN_POINT('Ctrl Pts',(2.16037549591216,2.25909150508723,-7.09496499356541));
#115015=CARTESIAN_POINT('Ctrl Pts',(2.13569578957734,2.24612498190645,-7.01538298196319));
#115016=CARTESIAN_POINT('Ctrl Pts',(2.12340660065055,2.23947860556987,-6.9755763973687));
#115017=CARTESIAN_POINT('Ctrl Pts',(2.11118902034456,2.23266407481316,-6.93580427345659));
#115018=CARTESIAN_POINT('Ctrl Pts',(2.422686474,2.231898283,-7.097928589));
#115019=CARTESIAN_POINT('Ctrl Pts',(2.038365897,2.296352134,-7.229106051));
#115020=CARTESIAN_POINT('Ctrl Pts',(1.64212838,2.361474582,-7.31801984));
#115021=CARTESIAN_POINT('Ctrl Pts',(2.115650277,2.231898283,-6.934444744));
#115022=CARTESIAN_POINT('Ctrl Pts',(1.740181607,2.296352134,-7.04899759200001));
#115023=CARTESIAN_POINT('Ctrl Pts',(1.354539278,2.361474582,-7.122339738));
#115024=CARTESIAN_POINT('Origin',(-0.0287152926699252,2.41068906715292,
0.194937925583135));
#115025=CARTESIAN_POINT('Ctrl Pts',(1.158859176,2.361474582,-7.40992884));
#115026=CARTESIAN_POINT('Ctrl Pts',(0.921175436,2.323357812,-7.447100854));
#115027=CARTESIAN_POINT('Ctrl Pts',(0.68159806,2.285714286,-7.468964057));
#115028=CARTESIAN_POINT('Ctrl Pts',(0.511109446,2.258926311,-7.48452240000001));
#115029=CARTESIAN_POINT('Ctrl Pts',(0.340088494,2.231887255,-7.492285353));
#115030=CARTESIAN_POINT('Ctrl Pts',(1.354539278,2.361474582,-7.12233973800001));
#115031=CARTESIAN_POINT('Ctrl Pts',(1.126080358,2.323357812,-7.165788463));
#115032=CARTESIAN_POINT('Ctrl Pts',(0.895306583,2.285714286,-7.194506663));
#115033=CARTESIAN_POINT('Ctrl Pts',(0.731082809,2.258926311,-7.214943176));
#115034=CARTESIAN_POINT('Ctrl Pts',(0.566097586,2.231887255,-7.227865074));
#115035=CARTESIAN_POINT('',(0.570837697299746,2.23266407433622,-7.22749225539564));
#115036=CARTESIAN_POINT('Ctrl Pts',(0.570837697322891,2.2326640750753,-7.22749225722226));
#115037=CARTESIAN_POINT('Ctrl Pts',(0.67946118151483,2.25046493771607,-7.21891301886173));
#115038=CARTESIAN_POINT('Ctrl Pts',(0.787670512609784,2.26815682588018,
-7.20790122760538));
#115039=CARTESIAN_POINT('Ctrl Pts',(0.895306582512715,2.28571428592052,
-7.19450666306064));
#115040=CARTESIAN_POINT('Ctrl Pts',(1.04860173579021,2.31071959723866,-7.17543014161265));
#115041=CARTESIAN_POINT('Ctrl Pts',(1.20183998314738,2.33599777462408,-7.15138036210171));
#115042=CARTESIAN_POINT('Ctrl Pts',(1.35453926788343,2.36147458031212,-7.12233973992399));
#115043=CARTESIAN_POINT('Ctrl Pts',(0.591816174293166,2.27159573037352,
-7.4766137796155));
#115044=CARTESIAN_POINT('Ctrl Pts',(0.588213725050591,2.26541917069486,
-7.43506277642082));
#115045=CARTESIAN_POINT('Ctrl Pts',(0.584659369354717,2.25909150512078,
-7.39350552607491));
#115046=CARTESIAN_POINT('Ctrl Pts',(0.577664433621786,2.24612496820187,
-7.31047860262288));
#115047=CARTESIAN_POINT('Ctrl Pts',(0.574219802158501,2.23947859887087,
-7.26896090857373));
#115048=CARTESIAN_POINT('Ctrl Pts',(0.570837696147924,2.23266407485203,
-7.22749225711022));
#115049=CARTESIAN_POINT('Ctrl Pts',(0.840200577,2.231898283,-7.45278894));
#115050=CARTESIAN_POINT('Ctrl Pts',(0.436665925,2.296352134,-7.498281983));
#115051=CARTESIAN_POINT('Ctrl Pts',(0.030578384,2.361474582,-7.49993766400001));
#115052=CARTESIAN_POINT('Ctrl Pts',(0.57548691,2.231898283,-7.22712355100001));
#115053=CARTESIAN_POINT('Ctrl Pts',(0.184171013,2.296352134,-7.258283552));
#115054=CARTESIAN_POINT('Ctrl Pts',(-0.208221606,2.361474582,-7.247009298));
#115055=CARTESIAN_POINT('Origin',(0.0138619466249593,2.41068905855906,0.196553253636468));
#115056=CARTESIAN_POINT('Ctrl Pts',(-0.461149972000001,2.361474582,-7.485809288));
#115057=CARTESIAN_POINT('Ctrl Pts',(-0.701267683,2.323357812,-7.47101726400001));
#115058=CARTESIAN_POINT('Ctrl Pts',(-0.939943815,2.285714286,-7.440867263));
#115059=CARTESIAN_POINT('Ctrl Pts',(-1.109791084,2.258926311,-7.419411849));
#115060=CARTESIAN_POINT('Ctrl Pts',(-1.278482467,2.231887255,-7.390228859));
#115061=CARTESIAN_POINT('Ctrl Pts',(-0.208221606,2.361474582,-7.247009298));
#115062=CARTESIAN_POINT('Ctrl Pts',(-0.440679476,2.323357812,-7.240330301));
#115063=CARTESIAN_POINT('Ctrl Pts',(-0.672231452,2.285714286,-7.218767545));
#115064=CARTESIAN_POINT('Ctrl Pts',(-0.837009012,2.258926311,-7.203423007));
#115065=CARTESIAN_POINT('Ctrl Pts',(-1.000914798,2.231887255,-7.180575852));
#115066=CARTESIAN_POINT('',(-0.996205363460386,2.23266407429648,-7.18123073377563));
#115067=CARTESIAN_POINT('Ctrl Pts',(-0.996205363775867,2.2326640749913,
-7.18123073522375));
#115068=CARTESIAN_POINT('Ctrl Pts',(-0.888277152906397,2.25046493778098,
-7.19620291315496));
#115069=CARTESIAN_POINT('Ctrl Pts',(-0.780230486021345,2.26815682597183,
-7.20871037895824));
#115070=CARTESIAN_POINT('Ctrl Pts',(-0.672231451769396,2.28571428607959,
-7.21876754526045));
#115071=CARTESIAN_POINT('Ctrl Pts',(-0.51841936674453,2.31071959735153,
-7.23309094942261));
#115072=CARTESIAN_POINT('Ctrl Pts',(-0.363593751971703,2.33599777473477,
-7.24254513359495));
#115073=CARTESIAN_POINT('Ctrl Pts',(-0.208221616445147,2.36147458028728,
-7.24700929769989));
#115074=CARTESIAN_POINT('Ctrl Pts',(-1.02927111432502,2.27159573037741,
-7.42903768812546));
#115075=CARTESIAN_POINT('Ctrl Pts',(-1.02385710290779,2.26541917069792,
-7.38768370412906));
#115076=CARTESIAN_POINT('Ctrl Pts',(-1.01839477945185,2.25909150513843,
-7.34633395778414));
#115077=CARTESIAN_POINT('Ctrl Pts',(-1.00737797669102,2.2461251250009,-7.2637454516772));
#115078=CARTESIAN_POINT('Ctrl Pts',(-1.00181692800756,2.2394786758839,-7.2224573914154));
#115079=CARTESIAN_POINT('Ctrl Pts',(-0.996205364803582,2.2326640748218,
-7.18123073508118));
#115080=CARTESIAN_POINT('Ctrl Pts',(-0.781572165,2.231898283,-7.459165164));
#115081=CARTESIAN_POINT('Ctrl Pts',(-1.18545206,2.296352134,-7.416846584));
#115082=CARTESIAN_POINT('Ctrl Pts',(-1.582401422,2.361474582,-7.331166738));
#115083=CARTESIAN_POINT('Ctrl Pts',(-0.991585586000001,2.231898283,-7.181870093));
#115084=CARTESIAN_POINT('Ctrl Pts',(-1.380451213,2.296352134,-7.128180239));
#115085=CARTESIAN_POINT('Ctrl Pts',(-1.76124628,2.361474582,-7.032816757));
#115086=CARTESIAN_POINT('Origin',(0.0557910479257062,2.41068902562531,0.188978279005378));
#115087=CARTESIAN_POINT('Ctrl Pts',(-2.05959626,2.361474582,-7.211661615));
#115088=CARTESIAN_POINT('Ctrl Pts',(-2.290920304,2.323357812,-7.14559720900001));
#115089=CARTESIAN_POINT('Ctrl Pts',(-2.517534962,2.285714286,-7.064843786));
#115090=CARTESIAN_POINT('Ctrl Pts',(-2.678799016,2.258926311,-7.007377845));
#115091=CARTESIAN_POINT('Ctrl Pts',(-2.837273008,2.231887255,-6.942613476));
#115092=CARTESIAN_POINT('Ctrl Pts',(-1.76124628,2.361474582,-7.032816757));
#115093=CARTESIAN_POINT('Ctrl Pts',(-1.986833627,2.323357812,-6.976322341));
#115094=CARTESIAN_POINT('Ctrl Pts',(-2.208336691,2.285714286,-6.905486881));
#115095=CARTESIAN_POINT('Ctrl Pts',(-2.365963221,2.258926311,-6.855078784));
#115096=CARTESIAN_POINT('Ctrl Pts',(-2.521125518,2.231887255,-6.79753088400001));
#115097=CARTESIAN_POINT('',(-2.5166669678886,2.23266407430148,-6.79918284460187));
#115098=CARTESIAN_POINT('Ctrl Pts',(-2.51666696834917,2.23266407497599,
-6.79918284552874));
#115099=CARTESIAN_POINT('Ctrl Pts',(-2.41448063483361,2.25046493773397,
-6.83700635708861));
#115100=CARTESIAN_POINT('Ctrl Pts',(-2.31164877451872,2.2681568259284,-6.87244824524909));
#115101=CARTESIAN_POINT('Ctrl Pts',(-2.20833669139914,2.28571428594652,
-6.90548688094287));
#115102=CARTESIAN_POINT('Ctrl Pts',(-2.06119975667221,2.3107195970458,-6.95254046229072));
#115103=CARTESIAN_POINT('Ctrl Pts',(-1.91202624773585,2.33599777477677,
-6.99505654399887));
#115104=CARTESIAN_POINT('Ctrl Pts',(-1.76124628998941,2.36147458031212,
-7.03281675449832));
#115105=CARTESIAN_POINT('Ctrl Pts',(-2.60223082985633,2.27159573036453,
-7.03408805099112));
#115106=CARTESIAN_POINT('Ctrl Pts',(-2.58805351088558,2.26541917068779,
-6.99486475257262));
#115107=CARTESIAN_POINT('Ctrl Pts',(-2.57382992027057,2.25909150510029,
-6.95565597813173));
#115108=CARTESIAN_POINT('Ctrl Pts',(-2.54531627113145,2.24612497696501,
-6.87736573852533));
#115109=CARTESIAN_POINT('Ctrl Pts',(-2.53100969657328,2.23947860318275,
-6.83823890827247));
#115110=CARTESIAN_POINT('Ctrl Pts',(-2.51666696900843,2.23266407487449,
-6.79918284534824));
#115111=CARTESIAN_POINT('Ctrl Pts',(-2.366799461,2.231898283,-7.116759116));
#115112=CARTESIAN_POINT('Ctrl Pts',(-2.752139625,2.296352134,-6.988607681));
#115113=CARTESIAN_POINT('Ctrl Pts',(-3.121389897,2.361474582,-6.819598603));
#115114=CARTESIAN_POINT('Ctrl Pts',(-2.512292641,2.231898283,-6.800800371));
#115115=CARTESIAN_POINT('Ctrl Pts',(-2.880525075,2.296352134,-6.66477114200001));
#115116=CARTESIAN_POINT('Ctrl Pts',(-3.231917035,2.361474582,-6.489777522));
#115117=CARTESIAN_POINT('Origin',(0.0951113206744036,2.41068903468273,0.172566421100852));
#115118=CARTESIAN_POINT('Ctrl Pts',(-3.561738116,2.361474582,-6.600304659));
#115119=CARTESIAN_POINT('Ctrl Pts',(-3.773452038,2.323357812,-6.48605697100001));
#115120=CARTESIAN_POINT('Ctrl Pts',(-3.977408972,2.285714286,-6.358476065));
#115121=CARTESIAN_POINT('Ctrl Pts',(-4.122549284,2.258926311,-6.267686641));
#115122=CARTESIAN_POINT('Ctrl Pts',(-4.263395817,2.231887255,-6.170369204));
#115123=CARTESIAN_POINT('Ctrl Pts',(-3.231917035,2.361474582,-6.489777522));
#115124=CARTESIAN_POINT('Ctrl Pts',(-3.440085645,2.323357812,-6.386109302));
#115125=CARTESIAN_POINT('Ctrl Pts',(-3.641182561,2.285714286,-6.269313324));
#115126=CARTESIAN_POINT('Ctrl Pts',(-3.78428762,2.258926311,-6.18619869600001));
#115127=CARTESIAN_POINT('Ctrl Pts',(-3.923451211,2.231887255,-6.096640927));
#115128=CARTESIAN_POINT('',(-3.91945202178794,2.23266407430098,-6.09921272207512));
#115129=CARTESIAN_POINT('Ctrl Pts',(-3.91945202254244,2.23266407500049,
-6.09921272303784));
#115130=CARTESIAN_POINT('Ctrl Pts',(-3.82778568593043,2.25046493774357,
-6.15811898272353));
#115131=CARTESIAN_POINT('Ctrl Pts',(-3.73497693549523,2.26815682593041,
-6.214838069248));
#115132=CARTESIAN_POINT('Ctrl Pts',(-3.64118256128412,2.28571428597374,
-6.26931332395667));
#115133=CARTESIAN_POINT('Ctrl Pts',(-3.50760073483172,2.31071959716862,
-6.34689691106505));
#115134=CARTESIAN_POINT('Ctrl Pts',(-3.37105452079006,2.33599777477738,
-6.42048688524898));
#115135=CARTESIAN_POINT('Ctrl Pts',(-3.23191704421808,2.36147458031212,
-6.48977751740939));
#115136=CARTESIAN_POINT('Ctrl Pts',(-4.05351312369268,2.2715957303518,-6.31023227389436));
#115137=CARTESIAN_POINT('Ctrl Pts',(-4.03123541291977,2.26541917067448,
-6.27497369889219));
#115138=CARTESIAN_POINT('Ctrl Pts',(-4.00891563465973,2.25909150511891,
-6.23973925558646));
#115139=CARTESIAN_POINT('Ctrl Pts',(-3.96423904170362,2.24612512499576,
-6.1694097929572));
#115140=CARTESIAN_POINT('Ctrl Pts',(-3.94185556402805,2.23947867587992,
-6.13427278807419));
#115141=CARTESIAN_POINT('Ctrl Pts',(-3.9194520233861,2.23266407483665,-6.09921272249569));
#115142=CARTESIAN_POINT('Ctrl Pts',(-3.841357845,2.231898283,-6.44158132));
#115143=CARTESIAN_POINT('Ctrl Pts',(-4.190140199,2.296352134,-6.23358925));
#115144=CARTESIAN_POINT('Ctrl Pts',(-4.51442565,2.361474582,-5.989153617));
#115145=CARTESIAN_POINT('Ctrl Pts',(-3.915527685,2.231898283,-6.101732783));
#115146=CARTESIAN_POINT('Ctrl Pts',(-4.245908786,2.296352134,-5.88972475300001));
#115147=CARTESIAN_POINT('Ctrl Pts',(-4.551466941,2.361474582,-5.643283502));
#115148=CARTESIAN_POINT('Origin',(0.129984324614556,2.41068904740896,0.148085736443294));
#115149=CARTESIAN_POINT('Ctrl Pts',(-4.897337056,2.361474582,-5.680324793));
#115150=CARTESIAN_POINT('Ctrl Pts',(-5.079541349,2.323357812,-5.523235918));
#115151=CARTESIAN_POINT('Ctrl Pts',(-5.251303759,2.285714286,-5.35479307));
#115152=CARTESIAN_POINT('Ctrl Pts',(-5.373533729,2.258926311,-5.234925376));
#115153=CARTESIAN_POINT('Ctrl Pts',(-5.490166976,2.231887255,-5.109605325));
#115154=CARTESIAN_POINT('Ctrl Pts',(-4.551466941,2.361474582,-5.643283502));
#115155=CARTESIAN_POINT('Ctrl Pts',(-4.732483083,2.323357812,-5.49728889));
#115156=CARTESIAN_POINT('Ctrl Pts',(-4.903770781,2.285714286,-5.339993645));
#115157=CARTESIAN_POINT('Ctrl Pts',(-5.025662935,2.258926311,-5.228058833));
#115158=CARTESIAN_POINT('Ctrl Pts',(-5.142320686,2.231887255,-5.110678816));
#115159=CARTESIAN_POINT('',(-5.13896785483513,2.23266407435047,-5.11405019176887));
#115160=CARTESIAN_POINT('Ctrl Pts',(-5.13896785595135,2.23266407511824,
-5.11405019270273));
#115161=CARTESIAN_POINT('Ctrl Pts',(-5.0621077315837,2.25046493787097,-5.19128480983772));
#115162=CARTESIAN_POINT('Ctrl Pts',(-4.98366172519896,2.2681568260187,-5.26662897364023));
#115163=CARTESIAN_POINT('Ctrl Pts',(-4.90377078122153,2.28571428595199,
-5.3399936447995));
#115164=CARTESIAN_POINT('Ctrl Pts',(-4.78999020241981,2.31071959705392,
-5.44447951406395));
#115165=CARTESIAN_POINT('Ctrl Pts',(-4.67245603173986,2.3359977748075,-5.54570239561369));
#115166=CARTESIAN_POINT('Ctrl Pts',(-4.55146694901571,2.36147458031212,
-5.6432834955351));
#115167=CARTESIAN_POINT('Ctrl Pts',(-5.31525764932166,2.27159573038573,
-5.2913170492895));
#115168=CARTESIAN_POINT('Ctrl Pts',(-5.28592122760232,2.26541917071696,
-5.26167184967998));
#115169=CARTESIAN_POINT('Ctrl Pts',(-5.25654890930045,2.25909150511919,
-5.23205926051504));
#115170=CARTESIAN_POINT('Ctrl Pts',(-5.19779733318026,2.24612496134411,
-5.17297746284238));
#115171=CARTESIAN_POINT('Ctrl Pts',(-5.16838414603642,2.23947859552117,
-5.14347412631359));
#115172=CARTESIAN_POINT('Ctrl Pts',(-5.13896785724193,2.23266407489063,
-5.11405019171443));
#115173=CARTESIAN_POINT('Ctrl Pts',(-5.136298605,2.231898283,-5.465202342));
#115174=CARTESIAN_POINT('Ctrl Pts',(-5.432214475,2.296352134,-5.187095114));
#115175=CARTESIAN_POINT('Ctrl Pts',(-5.696371877,2.361474582,-4.878662465));
#115176=CARTESIAN_POINT('Ctrl Pts',(-5.135677006,2.231898283,-5.117354951));
#115177=CARTESIAN_POINT('Ctrl Pts',(-5.41275852000001,2.296352134,-4.83928138000001));
#115178=CARTESIAN_POINT('Ctrl Pts',(-5.658195312,2.361474582,-4.532915818));
#115179=CARTESIAN_POINT('Origin',(0.15877967775259,2.41068903813253,0.116681024699704));
#115180=CARTESIAN_POINT('Ctrl Pts',(-6.003941959,2.361474582,-4.494739253));
#115181=CARTESIAN_POINT('Ctrl Pts',(-6.14811695100001,2.323357812,-4.302154492));
#115182=CARTESIAN_POINT('Ctrl Pts',(-6.279653419,2.285714286,-4.100725903));
#115183=CARTESIAN_POINT('Ctrl Pts',(-6.373257709,2.258926311,-3.957384819));
#115184=CARTESIAN_POINT('Ctrl Pts',(-6.460224029,2.231887255,-3.80992198));
#115185=CARTESIAN_POINT('Ctrl Pts',(-5.658195312,2.361474582,-4.532915818));
#115186=CARTESIAN_POINT('Ctrl Pts',(-5.803594871,2.323357812,-4.351421359));
#115187=CARTESIAN_POINT('Ctrl Pts',(-5.93706413,2.285714286,-4.160981797));
#115188=CARTESIAN_POINT('Ctrl Pts',(-6.032043837,2.258926311,-4.025460749));
#115189=CARTESIAN_POINT('Ctrl Pts',(-6.120740961,2.231887255,-3.885747044));
#115190=CARTESIAN_POINT('',(-6.11819126292683,2.23266407432955,-3.88976035831329));
#115191=CARTESIAN_POINT('Ctrl Pts',(-6.11819126454179,2.23266407512976,
-3.8897603591851));
#115192=CARTESIAN_POINT('Ctrl Pts',(-6.05973124664646,2.25046493787191,
-3.98171192826723));
#115193=CARTESIAN_POINT('Ctrl Pts',(-5.99931603244148,2.26815682601324,
-4.07215815960735));
#115194=CARTESIAN_POINT('Ctrl Pts',(-5.93706413017151,2.28571428595903,
-4.16098179678812));
#115195=CARTESIAN_POINT('Ctrl Pts',(-5.84840505098194,2.31071959712034,
-4.2874843062922));
#115196=CARTESIAN_POINT('Ctrl Pts',(-5.75537869179094,2.33599777473392,
-4.41160702508984));
#115197=CARTESIAN_POINT('Ctrl Pts',(-5.65819531864777,2.36147458025728,
-4.53291580970195));
#115198=CARTESIAN_POINT('Ctrl Pts',(-6.32846663464899,2.27159573037118,
-4.02498572048494));
#115199=CARTESIAN_POINT('Ctrl Pts',(-6.2934432405714,2.26541917070497,-4.00234007259233));
#115200=CARTESIAN_POINT('Ctrl Pts',(-6.25839179936662,2.2590915051017,-3.97973398939621));
#115201=CARTESIAN_POINT('Ctrl Pts',(-6.18831295557712,2.24612496007342,
-3.93466333912423));
#115202=CARTESIAN_POINT('Ctrl Pts',(-6.15324509058793,2.23947859485753,
-3.9121727422877));
#115203=CARTESIAN_POINT('Ctrl Pts',(-6.11819126522844,2.23266407483229,
-3.88976035771312));
#115204=CARTESIAN_POINT('Ctrl Pts',(-6.191071751,2.231898283,-4.233276576));
#115205=CARTESIAN_POINT('Ctrl Pts',(-6.42028444,2.296352134,-3.898058176));
#115206=CARTESIAN_POINT('Ctrl Pts',(-6.61196208500001,2.361474582,-3.540050477));
#115207=CARTESIAN_POINT('Ctrl Pts',(-6.115687778,2.231898283,-3.893695289));
#115208=CARTESIAN_POINT('Ctrl Pts',(-6.326513683,2.296352134,-3.562558589));
#115209=CARTESIAN_POINT('Ctrl Pts',(-6.50035275900001,2.361474582,-3.210594028));
#115210=CARTESIAN_POINT('Origin',(0.180150236420007,2.4106890271346,0.0798200253204628));
#115211=CARTESIAN_POINT('Ctrl Pts',(-6.829809208,2.361474582,-3.098984701));
#115212=CARTESIAN_POINT('Ctrl Pts',(-6.929213439,2.323357812,-2.879909103));
#115213=CARTESIAN_POINT('Ctrl Pts',(-7.014373465,2.285714286,-2.65491335));
#115214=CARTESIAN_POINT('Ctrl Pts',(-7.074975242,2.258926311,-2.494801346));
#115215=CARTESIAN_POINT('Ctrl Pts',(-7.128208186,2.231887255,-2.332090918));
#115216=CARTESIAN_POINT('Ctrl Pts',(-6.50035275900001,2.361474582,-3.210594028));
#115217=CARTESIAN_POINT('Ctrl Pts',(-6.60333701300001,2.323357812,-3.002086202));
#115218=CARTESIAN_POINT('Ctrl Pts',(-6.692746959,2.285714286,-2.787407065));
#115219=CARTESIAN_POINT('Ctrl Pts',(-6.756373074,2.258926311,-2.634636595));
#115220=CARTESIAN_POINT('Ctrl Pts',(-6.812962191,2.231887255,-2.479122059));
#115221=CARTESIAN_POINT('',(-6.81133484766748,2.23266407431936,-2.48358965366023));
#115222=CARTESIAN_POINT('Ctrl Pts',(-6.8113348493112,2.23266407506945,-2.48358965412914));
#115223=CARTESIAN_POINT('Ctrl Pts',(-6.7740084640474,2.25046493778705,-2.58595862225407));
#115224=CARTESIAN_POINT('Ctrl Pts',(-6.73444899030339,2.26815682595422,
-2.68727775611435));
#115225=CARTESIAN_POINT('Ctrl Pts',(-6.69274695897743,2.2857142860095,-2.78740706505419));
#115226=CARTESIAN_POINT('Ctrl Pts',(-6.63335497939657,2.31071959724752,
-2.93001109840022));
#115227=CARTESIAN_POINT('Ctrl Pts',(-6.56918624068048,2.33599777467704,
-3.07122981342259));
#115228=CARTESIAN_POINT('Ctrl Pts',(-6.50035276356033,2.36147458031212,
-3.2105940187669));
#115229=CARTESIAN_POINT('Ctrl Pts',(-7.04576355357195,2.27159573036992,
-2.57045053283274));
#115230=CARTESIAN_POINT('Ctrl Pts',(-7.00669084185951,2.26541917066254,
-2.55586332198084));
#115231=CARTESIAN_POINT('Ctrl Pts',(-6.96759924437638,2.25909150507993,
-2.54132078029164));
#115232=CARTESIAN_POINT('Ctrl Pts',(-6.88947012216532,2.24612498904905,
-2.5123688015418));
#115233=CARTESIAN_POINT('Ctrl Pts',(-6.8503872175269,2.23947860905116,-2.49794254199318));
#115234=CARTESIAN_POINT('Ctrl Pts',(-6.81133484909264,2.23266407477659,
-2.48358965283265));
#115235=CARTESIAN_POINT('Ctrl Pts',(-6.956357263,2.231898283,-2.803407502));
#115236=CARTESIAN_POINT('Ctrl Pts',(-7.108149039,2.296352134,-2.42675237));
#115237=CARTESIAN_POINT('Ctrl Pts',(-7.218384296,2.361474582,-2.035909664));
#115238=CARTESIAN_POINT('Ctrl Pts',(-6.809735786,2.231898283,-2.487970763));
#115239=CARTESIAN_POINT('Ctrl Pts',(-6.944448097,2.296352134,-2.119254517));
#115240=CARTESIAN_POINT('Ctrl Pts',(-7.038560935,2.361474582,-1.73814843));
#115241=CARTESIAN_POINT('Origin',(0.193097256276927,2.41068906716603,0.0392268638322035));
#115242=CARTESIAN_POINT('Ctrl Pts',(-7.33632217,2.361474582,-1.558325069));
#115243=CARTESIAN_POINT('Ctrl Pts',(-7.386307607,2.323357812,-1.323002365));
#115244=CARTESIAN_POINT('Ctrl Pts',(-7.421109203,2.285714286,-1.08496));
#115245=CARTESIAN_POINT('Ctrl Pts',(-7.445874796,2.258926311,-0.915563734));
#115246=CARTESIAN_POINT('Ctrl Pts',(-7.462885252,2.231887255,-0.745213877));
#115247=CARTESIAN_POINT('Ctrl Pts',(-7.038560935,2.361474582,-1.73814843));
#115248=CARTESIAN_POINT('Ctrl Pts',(-7.094314455,2.323357812,-1.51237683));
#115249=CARTESIAN_POINT('Ctrl Pts',(-7.135484378,2.285714286,-1.283496277));
#115250=CARTESIAN_POINT('Ctrl Pts',(-7.164781814,2.258926311,-1.120619762));
#115251=CARTESIAN_POINT('Ctrl Pts',(-7.18661688100001,2.231887255,-0.956576082));
#115252=CARTESIAN_POINT('',(-7.18598798505211,2.23266407432236,-0.96128905722973));
#115253=CARTESIAN_POINT('Ctrl Pts',(-7.18598798657416,2.23266407502328,
-0.961289057317811));
#115254=CARTESIAN_POINT('Ctrl Pts',(-7.17154057331441,2.25046493780431,
-1.06928876573398));
#115255=CARTESIAN_POINT('Ctrl Pts',(-7.1546865971327,2.26815682598154,-1.17674323189176));
#115256=CARTESIAN_POINT('Ctrl Pts',(-7.13548437813034,2.28571428597987,
-1.28349627680228));
#115257=CARTESIAN_POINT('Ctrl Pts',(-7.10813660149529,2.31071959718438,
-1.43553382661598));
#115258=CARTESIAN_POINT('Ctrl Pts',(-7.07582594134178,2.33599777472798,
-1.58724530929748));
#115259=CARTESIAN_POINT('Ctrl Pts',(-7.03856093751762,2.36147458027879,
-1.73814841980497));
#115260=CARTESIAN_POINT('Ctrl Pts',(-7.43360839986752,2.2715957303976,-0.995723935096617));
#115261=CARTESIAN_POINT('Ctrl Pts',(-7.39231336732167,2.26541917070341,
-0.98987724314556));
#115262=CARTESIAN_POINT('Ctrl Pts',(-7.35100949311984,2.25909150512737,
-0.984078235985104));
#115263=CARTESIAN_POINT('Ctrl Pts',(-7.26848306530838,2.24612497315279,
-0.972598576198767));
#115264=CARTESIAN_POINT('Ctrl Pts',(-7.22721273214972,2.23947860128824,
-0.966911271517868));
#115265=CARTESIAN_POINT('Ctrl Pts',(-7.18598798672256,2.23266407482623,
-0.961289056131126));
#115266=CARTESIAN_POINT('Ctrl Pts',(-7.396371241,2.231898283,-1.24245421));
#115267=CARTESIAN_POINT('Ctrl Pts',(-7.46364449,2.296352134,-0.84197432));
#115268=CARTESIAN_POINT('Ctrl Pts',(-7.487282879,2.361474582,-0.436571978));
#115269=CARTESIAN_POINT('Ctrl Pts',(-7.185368118,2.231898283,-0.96591149));
#115270=CARTESIAN_POINT('Ctrl Pts',(-7.237667836,2.296352134,-0.57685646));
#115271=CARTESIAN_POINT('Ctrl Pts',(-7.247653825,2.361474582,-0.184428943));
#115272=CARTESIAN_POINT('Origin',(0.197015451126664,2.41068906325541,-0.00320043539546667));
#115273=CARTESIAN_POINT('Ctrl Pts',(-7.49979686,2.361474582,0.055200111));
#115274=CARTESIAN_POINT('Ctrl Pts',(-7.49802624,2.323357812,0.295766492));
#115275=CARTESIAN_POINT('Ctrl Pts',(-7.480842122,2.285714286,0.535724874));
#115276=CARTESIAN_POINT('Ctrl Pts',(-7.46861352000001,2.258926311,0.706484620000001));
#115277=CARTESIAN_POINT('Ctrl Pts',(-7.448606097,2.231887255,0.876508537));
#115278=CARTESIAN_POINT('Ctrl Pts',(-7.247653825,2.361474582,-0.184428943));
#115279=CARTESIAN_POINT('Ctrl Pts',(-7.253569639,2.323357812,0.048049601));
#115280=CARTESIAN_POINT('Ctrl Pts',(-7.244574478,2.285714286,0.28042937));
#115281=CARTESIAN_POINT('Ctrl Pts',(-7.238173321,2.258926311,0.445796006));
#115282=CARTESIAN_POINT('Ctrl Pts',(-7.224233354,2.231887255,0.61069833));
#115283=CARTESIAN_POINT('',(-7.2246323116338,2.23266407427139,0.605960348384108));
#115284=CARTESIAN_POINT('Ctrl Pts',(-7.22463231308464,2.23266407487673,
0.605960348605037));
#115285=CARTESIAN_POINT('Ctrl Pts',(-7.23373941730284,2.25046493768212,
0.497379846342098));
#115286=CARTESIAN_POINT('Ctrl Pts',(-7.24037901137527,2.26815682590636,
0.388814498640126));
#115287=CARTESIAN_POINT('Ctrl Pts',(-7.24457447820918,2.28571428599811,
0.280429370238197));
#115288=CARTESIAN_POINT('Ctrl Pts',(-7.25054965718974,2.31071959731194,
0.126067410023992));
#115289=CARTESIAN_POINT('Ctrl Pts',(-7.25160788627812,2.3359977747573,-0.0290429788908016));
#115290=CARTESIAN_POINT('Ctrl Pts',(-7.24765382527071,2.36147458025578,
-0.18442893236182));
#115291=CARTESIAN_POINT('Ctrl Pts',(-7.47386597901761,2.27159573040534,
0.625561607462204));
#115292=CARTESIAN_POINT('Ctrl Pts',(-7.43227953564301,2.26541917071843,
0.62239439562222));
#115293=CARTESIAN_POINT('Ctrl Pts',(-7.39069470784731,2.25909150510652,
0.619178713156272));
#115294=CARTESIAN_POINT('Ctrl Pts',(-7.30762990237436,2.24612497119073,
0.612649241444927));
#115295=CARTESIAN_POINT('Ctrl Pts',(-7.26610185095944,2.23947860030007,
0.60933167900063));
#115296=CARTESIAN_POINT('Ctrl Pts',(-7.22463231290839,2.23266407477602,
0.605960349071764));
#115297=CARTESIAN_POINT('Ctrl Pts',(-7.49053912,2.231898283,0.376594861));
#115298=CARTESIAN_POINT('Ctrl Pts',(-7.47014822,2.296352134,0.782173513));
#115299=CARTESIAN_POINT('Ctrl Pts',(-7.406084436,2.361474582,1.183179329));
#115300=CARTESIAN_POINT('Ctrl Pts',(-7.225020623,2.231898283,0.601312732));
#115301=CARTESIAN_POINT('Ctrl Pts',(-7.192462271,2.296352134,0.992514764));
#115302=CARTESIAN_POINT('Ctrl Pts',(-7.117854477,2.361474582,1.377914237));
#115303=CARTESIAN_POINT('Origin',(0.191721477608199,2.41068901772705,-0.045478126261897));
#115304=CARTESIAN_POINT('Ctrl Pts',(-7.312589385,2.361474582,1.666144196));
#115305=CARTESIAN_POINT('Ctrl Pts',(-7.2591455,2.323357812,1.900705638));
#115306=CARTESIAN_POINT('Ctrl Pts',(-7.190779179,2.285714286,2.131359848));
#115307=CARTESIAN_POINT('Ctrl Pts',(-7.142128177,2.258926311,2.295498538));
#115308=CARTESIAN_POINT('Ctrl Pts',(-7.086038399,2.231887255,2.457246386));
#115309=CARTESIAN_POINT('Ctrl Pts',(-7.117854477,2.361474582,1.377914237));
#115310=CARTESIAN_POINT('Ctrl Pts',(-7.073655968,2.323357812,1.606229286));
#115311=CARTESIAN_POINT('Ctrl Pts',(-7.014916327,2.285714286,1.831242452));
#115312=CARTESIAN_POINT('Ctrl Pts',(-6.973115887,2.258926311,1.991366848));
#115313=CARTESIAN_POINT('Ctrl Pts',(-6.92405270400001,2.231887255,2.149417167));
#115314=CARTESIAN_POINT('',(-6.92546085993488,2.232664074283,2.14487572022464));
#115315=CARTESIAN_POINT('Ctrl Pts',(-6.92546086172287,2.23266407495847,
2.14487572089392));
#115316=CARTESIAN_POINT('Ctrl Pts',(-6.95769664487577,2.25046493772654,
2.04079152850569));
#115317=CARTESIAN_POINT('Ctrl Pts',(-6.98751934933272,2.26815682591951,
1.93619169499266));
#115318=CARTESIAN_POINT('Ctrl Pts',(-7.0149163272947,2.28571428602102,1.8312424523213));
#115319=CARTESIAN_POINT('Ctrl Pts',(-7.05393506896648,2.31071959734436,
1.68177387550864));
#115320=CARTESIAN_POINT('Ctrl Pts',(-7.08831270552657,2.33599777462343,
1.53051737006403));
#115321=CARTESIAN_POINT('Ctrl Pts',(-7.11785447504281,2.36147458031212,
1.37791424711019));
#115322=CARTESIAN_POINT('Ctrl Pts',(-7.16465389193971,2.27159573037728,
2.21759658403499));
#115323=CARTESIAN_POINT('Ctrl Pts',(-7.12472057326613,2.26541917070527,
2.20556356386122));
#115324=CARTESIAN_POINT('Ctrl Pts',(-7.08479925216011,2.25909150510694,
2.19348355357122));
#115325=CARTESIAN_POINT('Ctrl Pts',(-7.0050800612742,2.24612496508977,2.16925024806764));
#115326=CARTESIAN_POINT('Ctrl Pts',(-6.96523611042108,2.23947859730079,
2.1570829508967));
#115327=CARTESIAN_POINT('Ctrl Pts',(-6.92546086106448,2.23266407478612,
2.14487572124463));
#115328=CARTESIAN_POINT('Ctrl Pts',(-7.234457715,2.231898283,1.978034774));
#115329=CARTESIAN_POINT('Ctrl Pts',(-7.127356121,2.296352134,2.369747783));
#115330=CARTESIAN_POINT('Ctrl Pts',(-6.978585717,2.361474582,2.747606485));
#115331=CARTESIAN_POINT('Ctrl Pts',(-6.926839193,2.231898283,2.140420238));
#115332=CARTESIAN_POINT('Ctrl Pts',(-6.810945164,2.296352134,2.515477101));
#115333=CARTESIAN_POINT('Ctrl Pts',(-6.655232165,2.361474582,2.875827678));
#115334=CARTESIAN_POINT('Origin',(0.177462767707922,2.41068904305774,-0.0856293542727959));
#115335=CARTESIAN_POINT('Ctrl Pts',(-6.783453358,2.361474582,3.19918123));
#115336=CARTESIAN_POINT('Ctrl Pts',(-6.680835185,2.323357812,3.4167699));
#115337=CARTESIAN_POINT('Ctrl Pts',(-6.564483393,2.285714286,3.627334805));
#115338=CARTESIAN_POINT('Ctrl Pts',(-6.481684858,2.258926311,3.777177496));
#115339=CARTESIAN_POINT('Ctrl Pts',(-6.392135422,2.231887255,3.923086125));
#115340=CARTESIAN_POINT('Ctrl Pts',(-6.655232165,2.361474582,2.875827678));
#115341=CARTESIAN_POINT('Ctrl Pts',(-6.562986005,2.323357812,3.089303476));
#115342=CARTESIAN_POINT('Ctrl Pts',(-6.457248486,2.285714286,3.296428672));
#115343=CARTESIAN_POINT('Ctrl Pts',(-6.382003305,2.258926311,3.44382359));
#115344=CARTESIAN_POINT('Ctrl Pts',(-6.30011104500001,2.231887255,3.587631646));
#115345=CARTESIAN_POINT('',(-6.30246255593898,2.23266407428407,3.58349908789824));
#115346=CARTESIAN_POINT('Ctrl Pts',(-6.30246255736635,2.23266407492913,
3.58349908883104));
#115347=CARTESIAN_POINT('Ctrl Pts',(-6.3563197106885,2.25046493770011,3.48877806770818));
#115348=CARTESIAN_POINT('Ctrl Pts',(-6.4079310492588,2.2681568259098,3.39303471968367));
#115349=CARTESIAN_POINT('Ctrl Pts',(-6.45724848585561,2.2857142859486,3.29642867228284));
#115350=CARTESIAN_POINT('Ctrl Pts',(-6.52748631567317,2.31071959719169,
3.15884246443922));
#115351=CARTESIAN_POINT('Ctrl Pts',(-6.5935759005777,2.33599777471149,3.01851242710723));
#115352=CARTESIAN_POINT('Ctrl Pts',(-6.65523216073996,2.36147458023972,
2.87582768785858));
#115353=CARTESIAN_POINT('Ctrl Pts',(-6.52043055152139,2.27159573038141,
3.7059392092535));
#115354=CARTESIAN_POINT('Ctrl Pts',(-6.48401759527572,2.26541917068676,
3.68560303129541));
#115355=CARTESIAN_POINT('Ctrl Pts',(-6.44762645771656,2.2590915050952,3.6652235410452));
#115356=CARTESIAN_POINT('Ctrl Pts',(-6.37498057901858,2.2461249788959,3.62441957076062));
#115357=CARTESIAN_POINT('Ctrl Pts',(-6.33868372537222,2.23947860406256,
3.6039714434621));
#115358=CARTESIAN_POINT('Ctrl Pts',(-6.30246255660136,2.23266407476234,
3.58349908877191));
#115359=CARTESIAN_POINT('Ctrl Pts',(-6.640101108,2.231898283,3.48698398));
#115360=CARTESIAN_POINT('Ctrl Pts',(-6.45129677200001,2.296352134,3.846515279));
#115361=CARTESIAN_POINT('Ctrl Pts',(-6.224776085,2.361474582,4.183558616));
#115362=CARTESIAN_POINT('Ctrl Pts',(-6.304766461,2.231898283,3.579444073));
#115363=CARTESIAN_POINT('Ctrl Pts',(-6.110955831,2.296352134,3.920818525));
#115364=CARTESIAN_POINT('Ctrl Pts',(-5.881418593,2.361474582,4.239270613));
#115365=CARTESIAN_POINT('Origin',(0.154905876767801,2.4106890658271,-0.121776562416487));
#115366=CARTESIAN_POINT('Ctrl Pts',(-5.937130591,2.361474582,4.582628105));
#115367=CARTESIAN_POINT('Ctrl Pts',(-5.790136441,2.323357812,4.773069799));
#115368=CARTESIAN_POINT('Ctrl Pts',(-5.631239659,2.285714286,4.953699618));
#115369=CARTESIAN_POINT('Ctrl Pts',(-5.518165158,2.258926311,5.082239832));
#115370=CARTESIAN_POINT('Ctrl Pts',(-5.399343297,2.231887255,5.20548671700001));
#115371=CARTESIAN_POINT('Ctrl Pts',(-5.881418593,2.361474582,4.239270613));
#115372=CARTESIAN_POINT('Ctrl Pts',(-5.745438112,2.323357812,4.427925268));
#115373=CARTESIAN_POINT('Ctrl Pts',(-5.597646882,2.285714286,4.607477551));
#115374=CARTESIAN_POINT('Ctrl Pts',(-5.492475341,2.258926311,4.73525096800001));
#115375=CARTESIAN_POINT('Ctrl Pts',(-5.381583195,2.231887255,4.858092456));
#115376=CARTESIAN_POINT('',(-5.38476810755608,2.23266407431186,4.85456202018608));
#115377=CARTESIAN_POINT('Ctrl Pts',(-5.38476810829647,2.23266407501123,
4.85456202100741));
#115378=CARTESIAN_POINT('Ctrl Pts',(-5.45772833098115,2.25046493773274,
4.77363322114774));
#115379=CARTESIAN_POINT('Ctrl Pts',(-5.52871501487491,2.26815682591559,
4.69122321183394));
#115380=CARTESIAN_POINT('Ctrl Pts',(-5.59764688191103,2.28571428597216,
4.6074775513424));
#115381=CARTESIAN_POINT('Ctrl Pts',(-5.69581955863213,2.3107195972295,4.48820709001268));
#115382=CARTESIAN_POINT('Ctrl Pts',(-5.79053081512901,2.33599777465455,
4.36536519804431));
#115383=CARTESIAN_POINT('Ctrl Pts',(-5.88141858688418,2.36147458028567,
4.23927062148488));
#115384=CARTESIAN_POINT('Ctrl Pts',(-5.57131912513177,2.27159573041001,
5.02099623658654));
#115385=CARTESIAN_POINT('Ctrl Pts',(-5.54012916098098,2.26541917075981,
4.99330779807958));
#115386=CARTESIAN_POINT('Ctrl Pts',(-5.50896981593093,2.25909150513737,
4.96558174989394));
#115387=CARTESIAN_POINT('Ctrl Pts',(-5.44679396116879,2.24612496979083,
4.91011499786757));
#115388=CARTESIAN_POINT('Ctrl Pts',(-5.4157414743458,2.23947859965913,4.8823422066781));
#115389=CARTESIAN_POINT('Ctrl Pts',(-5.3847681076767,2.23266407485813,4.85456202185309));
#115390=CARTESIAN_POINT('Ctrl Pts',(-5.735260753,2.231898283,4.832885691));
#115391=CARTESIAN_POINT('Ctrl Pts',(-5.473581956,2.296352134,5.143423997));
#115392=CARTESIAN_POINT('Ctrl Pts',(-5.179902842,2.361474582,5.423892195));
#115393=CARTESIAN_POINT('Ctrl Pts',(-5.387889857,2.231898283,4.851097081));
#115394=CARTESIAN_POINT('Ctrl Pts',(-5.125224996,2.296352134,5.142826832));
#115395=CARTESIAN_POINT('Ctrl Pts',(-4.83259642500001,2.361474582,5.404489966));
#115396=CARTESIAN_POINT('Origin',(0.125105786846226,2.41068905209741,-0.152229557512465));
#115397=CARTESIAN_POINT('Ctrl Pts',(-4.813194196,2.361474582,5.751796383));
#115398=CARTESIAN_POINT('Ctrl Pts',(-4.628697353,2.323357812,5.906186259));
#115399=CARTESIAN_POINT('Ctrl Pts',(-4.434685418,2.285714286,6.048434942));
#115400=CARTESIAN_POINT('Ctrl Pts',(-4.29662219,2.258926311,6.149662283));
#115401=CARTESIAN_POINT('Ctrl Pts',(-4.15408388,2.231887255,6.244484536));
#115402=CARTESIAN_POINT('Ctrl Pts',(-4.832596425,2.361474582,5.404489966));
#115403=CARTESIAN_POINT('Ctrl Pts',(-4.659239917,2.323357812,5.559502196));
#115404=CARTESIAN_POINT('Ctrl Pts',(-4.476305531,2.285714286,5.703085901));
#115405=CARTESIAN_POINT('Ctrl Pts',(-4.346125334,2.258926311,5.805263274));
#115406=CARTESIAN_POINT('Ctrl Pts',(-4.211418497,2.231887255,5.901394263));
#115407=CARTESIAN_POINT('',(-4.21528788729399,2.23266407432337,5.89863102775519));
#115408=CARTESIAN_POINT('Ctrl Pts',(-4.21528788838403,2.23266407510249,
5.89863102949945));
#115409=CARTESIAN_POINT('Ctrl Pts',(-4.30393964099989,2.25046493788637,
5.83527859085858));
#115410=CARTESIAN_POINT('Ctrl Pts',(-4.39098241129342,2.26815682603576,
5.77005532067875));
#115411=CARTESIAN_POINT('Ctrl Pts',(-4.4763055306873,2.28571428593814,5.70308590133612));
#115412=CARTESIAN_POINT('Ctrl Pts',(-4.59782260737445,2.31071959704973,
5.6077081405588));
#115413=CARTESIAN_POINT('Ctrl Pts',(-4.71672694388695,2.3359977746627,5.50809834397294));
#115414=CARTESIAN_POINT('Ctrl Pts',(-4.83259641732343,2.36147458031211,
5.40448997286425));
#115415=CARTESIAN_POINT('Ctrl Pts',(-4.36169900909674,2.27159573034486,
6.10127705920046));
#115416=CARTESIAN_POINT('Ctrl Pts',(-4.33719044449114,2.26541917064638,
6.0675310404069));
#115417=CARTESIAN_POINT('Ctrl Pts',(-4.3127198683797,2.25909150506767,6.03375487391214));
#115418=CARTESIAN_POINT('Ctrl Pts',(-4.26392139898229,2.24612497942368,
5.96621898333419));
#115419=CARTESIAN_POINT('Ctrl Pts',(-4.23956521153354,2.23947860431857,
5.93242011068925));
#115420=CARTESIAN_POINT('Ctrl Pts',(-4.21528788699178,2.2326640747801,5.89863102936508));
#115421=CARTESIAN_POINT('Ctrl Pts',(-4.56224597900001,2.231898283,5.952807038));
#115422=CARTESIAN_POINT('Ctrl Pts',(-4.23992853,2.296352134,6.19983192400001));
#115423=CARTESIAN_POINT('Ctrl Pts',(-3.892823099,2.361474582,6.410610604));
#115424=CARTESIAN_POINT('Ctrl Pts',(-4.219081511,2.231898283,5.89591818099999));
#115425=CARTESIAN_POINT('Ctrl Pts',(-3.899844336,2.296352134,6.124362272));
#115426=CARTESIAN_POINT('Ctrl Pts',(-3.557807419,2.361474582,6.317001375));
#115427=CARTESIAN_POINT('Origin',(0.089456009380211,2.41068903096621,-0.17556451321962));
#115428=CARTESIAN_POINT('Ctrl Pts',(-3.46419819,2.361474582,6.652017055));
#115429=CARTESIAN_POINT('Ctrl Pts',(-3.250825521,2.323357812,6.763136014));
#115430=CARTESIAN_POINT('Ctrl Pts',(-3.030770215,2.285714286,6.86035217));
#115431=CARTESIAN_POINT('Ctrl Pts',(-2.874173942,2.258926311,6.929533359));
#115432=CARTESIAN_POINT('Ctrl Pts',(-2.714584117,2.231887255,6.991497198));
#115433=CARTESIAN_POINT('Ctrl Pts',(-3.557807419,2.361474582,6.31700137500001));
#115434=CARTESIAN_POINT('Ctrl Pts',(-3.355180843,2.323357812,6.43112298));
#115435=CARTESIAN_POINT('Ctrl Pts',(-3.145657109,2.285714286,6.532024292));
#115436=CARTESIAN_POINT('Ctrl Pts',(-2.996555338,2.258926311,6.603827921));
#115437=CARTESIAN_POINT('Ctrl Pts',(-2.84433255,2.231887255,6.668753433));
#115438=CARTESIAN_POINT('',(-2.84870549026514,2.23266407433,6.66688660531187));
#115439=CARTESIAN_POINT('Ctrl Pts',(-2.84870549087027,2.23266407513038,
6.66688660706084));
#115440=CARTESIAN_POINT('Ctrl Pts',(-2.94890351649421,2.25046493782023,
6.62407281963628));
#115441=CARTESIAN_POINT('Ctrl Pts',(-3.04793235054105,2.26815682595923,
6.57908605560133));
#115442=CARTESIAN_POINT('Ctrl Pts',(-3.14565710867187,2.28571428595922,
6.53202429239836));
#115443=CARTESIAN_POINT('Ctrl Pts',(-3.28483658331461,2.31071959718301,
6.46499899052546));
#115444=CARTESIAN_POINT('Ctrl Pts',(-3.42237416391989,2.33599777470832,
6.3932789329289));
#115445=CARTESIAN_POINT('Ctrl Pts',(-3.5578074100273,2.36147458031211,6.31700138005354));
#115446=CARTESIAN_POINT('Ctrl Pts',(-2.9481306941972,2.27159573037685,6.89626894828925));
#115447=CARTESIAN_POINT('Ctrl Pts',(-2.93144952302019,2.26541917074977,
6.85804327622383));
#115448=CARTESIAN_POINT('Ctrl Pts',(-2.9148119327911,2.25909150512727,6.81979632704012));
#115449=CARTESIAN_POINT('Ctrl Pts',(-2.88167293465899,2.24612512420583,
6.74335001312441));
#115450=CARTESIAN_POINT('Ctrl Pts',(-2.86515174144512,2.2394786754138,6.7051050243239));
#115451=CARTESIAN_POINT('Ctrl Pts',(-2.84870548936965,2.23266407486858,
6.66688660775785));
#115452=CARTESIAN_POINT('Ctrl Pts',(-3.175905654,2.231898283,6.79438174400001));
#115453=CARTESIAN_POINT('Ctrl Pts',(-2.808020759,2.296352134,6.966342602));
#115454=CARTESIAN_POINT('Ctrl Pts',(-2.423719275,2.361474582,7.097575986));
#115455=CARTESIAN_POINT('Ctrl Pts',(-2.852993603,2.231898283,6.665052701));
#115456=CARTESIAN_POINT('Ctrl Pts',(-2.492111289,2.296352134,6.819529339));
#115457=CARTESIAN_POINT('Ctrl Pts',(-2.116659292,2.361474582,6.93413682));
#115458=CARTESIAN_POINT('Origin',(0.0496234282576166,2.4106890156939,-0.190690422859716));
#115459=CARTESIAN_POINT('Ctrl Pts',(-1.953220126,2.361474582,7.241196803));
#115460=CARTESIAN_POINT('Ctrl Pts',(-1.720948701,2.323357812,7.303849046));
#115461=CARTESIAN_POINT('Ctrl Pts',(-1.485139566,2.285714286,7.351486956));
#115462=CARTESIAN_POINT('Ctrl Pts',(-1.317332516,2.258926311,7.385387158));
#115463=CARTESIAN_POINT('Ctrl Pts',(-1.148153419,2.231887255,7.411595221));
#115464=CARTESIAN_POINT('Ctrl Pts',(-2.116659292,2.361474582,6.93413682));
#115465=CARTESIAN_POINT('Ctrl Pts',(-1.894237241,2.323357812,7.002031601));
#115466=CARTESIAN_POINT('Ctrl Pts',(-1.667921256,2.285714286,7.055532488));
#115467=CARTESIAN_POINT('Ctrl Pts',(-1.506869744,2.258926311,7.093604914));
#115468=CARTESIAN_POINT('Ctrl Pts',(-1.344248775,2.231887255,7.124289104));
#115469=CARTESIAN_POINT('',(-1.34892079077827,2.23266407431317,7.12340597438253));
#115470=CARTESIAN_POINT('Ctrl Pts',(-1.34892079104794,2.2326640750857,7.12340597648489));
#115471=CARTESIAN_POINT('Ctrl Pts',(-1.45597994114529,2.25046493783544,
7.10313276514847));
#115472=CARTESIAN_POINT('Ctrl Pts',(-1.56236436026021,2.26815682598767,
7.08048603900714));
#115473=CARTESIAN_POINT('Ctrl Pts',(-1.66792125556938,2.28571428593661,
7.05553248817024));
#115474=CARTESIAN_POINT('Ctrl Pts',(-1.81825525022986,2.3107195971373,7.01999367250149));
#115475=CARTESIAN_POINT('Ctrl Pts',(-1.96799497131678,2.33599777477943,
6.97951690438721));
#115476=CARTESIAN_POINT('Ctrl Pts',(-2.11665928215075,2.36147458031212,
6.9341368230065));
#115477=CARTESIAN_POINT('Ctrl Pts',(-1.3967110656066,2.27159573036363,7.36879896579079));
#115478=CARTESIAN_POINT('Ctrl Pts',(-1.38863728042462,2.26541917071644,
7.32788102979332));
#115479=CARTESIAN_POINT('Ctrl Pts',(-1.38061063127253,2.25909150509517,
7.28695168286009));
#115480=CARTESIAN_POINT('Ctrl Pts',(-1.3646799069082,2.24612496514739,7.20516773311084));
#115481=CARTESIAN_POINT('Ctrl Pts',(-1.3567666176599,2.23947859731389,7.16426585760438));
#115482=CARTESIAN_POINT('Ctrl Pts',(-1.34892078967418,2.23266407477031,
7.12340597607662));
#115483=CARTESIAN_POINT('Ctrl Pts',(-1.64106351,2.231898283,7.31825871100001));
#115484=CARTESIAN_POINT('Ctrl Pts',(-1.244813059,2.296352134,7.407114842));
#115485=CARTESIAN_POINT('Ctrl Pts',(-0.841285031,2.361474582,7.452666603));
#115486=CARTESIAN_POINT('Ctrl Pts',(-1.353502885,2.231898283,7.122536763));
#115487=CARTESIAN_POINT('Ctrl Pts',(-0.967849888,2.296352134,7.195822793));
#115488=CARTESIAN_POINT('Ctrl Pts',(-0.576538529,2.361474582,7.227039735));
#115489=CARTESIAN_POINT('Origin',(0.00747050078381883,2.41068901051413,
-0.196900006855639));
#115490=CARTESIAN_POINT('Ctrl Pts',(-0.350911661,2.361474582,7.491786236));
#115491=CARTESIAN_POINT('Ctrl Pts',(-0.110602232,2.323357812,7.503042214));
#115492=CARTESIAN_POINT('Ctrl Pts',(0.129934559,2.285714286,7.498874383));
#115493=CARTESIAN_POINT('Ctrl Pts',(0.301105915,2.258926311,7.495908461));
#115494=CARTESIAN_POINT('Ctrl Pts',(0.471963657,2.231887255,7.48513529));
#115495=CARTESIAN_POINT('Ctrl Pts',(-0.576538529,2.361474582,7.22703973500001));
#115496=CARTESIAN_POINT('Ctrl Pts',(-0.344721211,2.323357812,7.245533007));
#115497=CARTESIAN_POINT('Ctrl Pts',(-0.112195259,2.285714286,7.249131826));
#115498=CARTESIAN_POINT('Ctrl Pts',(0.053275404,2.258926311,7.251692825));
#115499=CARTESIAN_POINT('Ctrl Pts',(0.218690579,2.231887255,7.246700934));
#115500=CARTESIAN_POINT('Ctrl Pts',(0.213937951383149,2.23266407437781,
7.24684279994555));
#115501=CARTESIAN_POINT('Ctrl Pts',(0.105023643191308,2.25046493706875,
7.25005811733432));
#115502=CARTESIAN_POINT('Ctrl Pts',(-0.00374194605548129,2.26815682549406,
7.25081036438579));
#115503=CARTESIAN_POINT('Ctrl Pts',(-0.112195259309469,2.28571428606866,
7.24913182611169));
#115504=CARTESIAN_POINT('Ctrl Pts',(-0.266654322558138,2.31071959712748,
7.24674125320845));
#115505=CARTESIAN_POINT('Ctrl Pts',(-0.4215945208895,2.3359977747927,7.23940042340816));
#115506=CARTESIAN_POINT('Ctrl Pts',(-0.576538518734711,2.36147458031212,
7.22703973581892));
#115507=CARTESIAN_POINT('Ctrl Pts',(-1.36436745820684,3.52436392548355,
7.12046798599309));
#115508=CARTESIAN_POINT('Ctrl Pts',(-1.36047186710342,3.52502192024177,
7.12121001099655));
#115509=CARTESIAN_POINT('Ctrl Pts',(-1.356576276,3.525679915,7.121952036));
#115510=CARTESIAN_POINT('Ctrl Pts',(-0.967402251,3.591414347,7.196081186));
#115511=CARTESIAN_POINT('Ctrl Pts',(-0.572468102,3.656498153,7.2273633));
#115512=CARTESIAN_POINT('Ctrl Pts',(-1.16908429046732,3.52436392548355,
7.40832702063338));
#115513=CARTESIAN_POINT('Ctrl Pts',(-1.16503136223366,3.52502192024177,
7.40896205681669));
#115514=CARTESIAN_POINT('Ctrl Pts',(-1.160978434,3.525679915,7.409597093));
#115515=CARTESIAN_POINT('Ctrl Pts',(-0.756086249,3.591414347,7.473037937));
#115516=CARTESIAN_POINT('Ctrl Pts',(-0.346692162,3.656498153,7.491982685));
#115517=CARTESIAN_POINT('',(-0.577160368164006,3.65572482702379,7.22699010131578));
#115518=CARTESIAN_POINT('Ctrl Pts',(-0.577160369470976,3.6557248264673,
7.22699010111248));
#115519=CARTESIAN_POINT('Ctrl Pts',(-0.58068380245636,3.64885401015902,
7.26844871272591));
#115520=CARTESIAN_POINT('Ctrl Pts',(-0.584188197121918,3.64214700170532,
7.30996068621342));
#115521=CARTESIAN_POINT('Ctrl Pts',(-0.591154981583553,3.62905099610467,
7.39298959490074));
#115522=CARTESIAN_POINT('Ctrl Pts',(-0.594621219303742,3.622654765003,7.43455243089213));
#115523=CARTESIAN_POINT('Ctrl Pts',(-0.598068334408679,3.6164059873883,
7.47611625530082));
#115524=CARTESIAN_POINT('Origin',(0.0440243728265652,3.48216462733526,-0.192296609468819));
#115525=CARTESIAN_POINT('Ctrl Pts',(-2.121755383,3.656505752,6.93257918100001));
#115526=CARTESIAN_POINT('Ctrl Pts',(-1.744320898,3.590992329,7.048095157));
#115527=CARTESIAN_POINT('Ctrl Pts',(-1.356576276,3.525679915,7.121952036));
#115528=CARTESIAN_POINT('Ctrl Pts',(-2.428935412,3.656505752,7.09579261));
#115529=CARTESIAN_POINT('Ctrl Pts',(-2.042615002,3.590992329,7.228032569));
#115530=CARTESIAN_POINT('Ctrl Pts',(-1.644221332,3.525679915,7.31754987800001));
#115531=CARTESIAN_POINT('',(-2.11725592263229,3.65572482705533,6.93395466884954));
#115532=CARTESIAN_POINT('Origin',(0.053364361895534,3.62499993732917,-0.192199315869914));
#115533=CARTESIAN_POINT('Ctrl Pts',(-2.1912298310443,3.61640598740892,7.17276179868612));
#115534=CARTESIAN_POINT('Ctrl Pts',(-2.17892831394179,3.62265476504301,
7.13291074101982));
#115535=CARTESIAN_POINT('Ctrl Pts',(-2.16660833371638,3.62905099621088,
7.09306475921216));
#115536=CARTESIAN_POINT('Ctrl Pts',(-2.14195551550789,3.64214708279692,
7.01347418081946));
#115537=CARTESIAN_POINT('Ctrl Pts',(-2.12960928518368,3.648854050219,6.97368633665899));
#115538=CARTESIAN_POINT('Ctrl Pts',(-2.11725592405794,3.65572482662799,
6.93395466915322));
#115539=CARTESIAN_POINT('Ctrl Pts',(-2.86315944180208,3.52436392548355,
6.6606967283916));
#115540=CARTESIAN_POINT('Ctrl Pts',(-2.85951444090104,3.52502192024177,
6.66225884219581));
#115541=CARTESIAN_POINT('Ctrl Pts',(-2.85586944,3.525679915,6.663820956));
#115542=CARTESIAN_POINT('Ctrl Pts',(-2.491729664,3.591414347,6.819877919));
#115543=CARTESIAN_POINT('Ctrl Pts',(-2.112753586,3.656498153,6.935327843));
#115544=CARTESIAN_POINT('Ctrl Pts',(-2.73432307002075,3.52436392548355,
6.98380588667783));
#115545=CARTESIAN_POINT('Ctrl Pts',(-2.73050141101038,3.52502192024177,
6.98529733583892));
#115546=CARTESIAN_POINT('Ctrl Pts',(-2.726679752,3.525679915,6.986788785));
#115547=CARTESIAN_POINT('Ctrl Pts',(-2.344891628,3.591414347,7.135786269));
#115548=CARTESIAN_POINT('Ctrl Pts',(-1.949141507,3.656498153,7.242295726));
#115549=CARTESIAN_POINT('Origin',(0.0843333478850994,3.48216454650792,-0.178337430489187));
#115550=CARTESIAN_POINT('Ctrl Pts',(-3.562449519,3.656505752,6.314384643));
#115551=CARTESIAN_POINT('Ctrl Pts',(-3.218671763,3.590992329,6.508337177));
#115552=CARTESIAN_POINT('Ctrl Pts',(-2.85586944,3.525679915,6.663820956));
#115553=CARTESIAN_POINT('Ctrl Pts',(-3.897533913,3.656505752,6.407747607));
#115554=CARTESIAN_POINT('Ctrl Pts',(-3.548673142,3.590992329,6.619943338));
#115555=CARTESIAN_POINT('Ctrl Pts',(-3.178837269,3.525679915,6.793010644));
#115556=CARTESIAN_POINT('',(-3.55835094254514,3.6557248270686,6.31669522457157));
#115557=CARTESIAN_POINT('Origin',(0.0934339420682495,3.62499996819879,-0.176234096549057));
#115558=CARTESIAN_POINT('Ctrl Pts',(-3.68193185676624,3.61640598737491,
6.53401697235091));
#115559=CARTESIAN_POINT('Ctrl Pts',(-3.66135114289402,3.62265476502698,
6.49774207271943));
#115560=CARTESIAN_POINT('Ctrl Pts',(-3.6407534887579,3.62905099620307,6.46147609934633));
#115561=CARTESIAN_POINT('Ctrl Pts',(-3.59956739575239,3.64214708992088,
6.38904589216658));
#115562=CARTESIAN_POINT('Ctrl Pts',(-3.57895661493682,3.64885405374133,
6.35284236110603));
#115563=CARTESIAN_POINT('Ctrl Pts',(-3.55835094491586,3.65572482666612,
6.31669522370334));
#115564=CARTESIAN_POINT('Ctrl Pts',(-4.22807327301959,3.52436392548355,
5.88947869519783));
#115565=CARTESIAN_POINT('Ctrl Pts',(-4.22484929850979,3.52502192024177,
5.89178785509892));
#115566=CARTESIAN_POINT('Ctrl Pts',(-4.221625324,3.525679915,5.894097015));
#115567=CARTESIAN_POINT('Ctrl Pts',(-3.899546568,3.591414347,6.124784741));
#115568=CARTESIAN_POINT('Ctrl Pts',(-3.554249061,3.656498153,6.319004163));
#115569=CARTESIAN_POINT('Ctrl Pts',(-4.17170794254552,3.52436392548355,
6.23272975173752));
#115570=CARTESIAN_POINT('Ctrl Pts',(-4.16829624927276,3.52502192024177,
6.23500787536876));
#115571=CARTESIAN_POINT('Ctrl Pts',(-4.164884556,3.525679915,6.23728599900001));
#115572=CARTESIAN_POINT('Ctrl Pts',(-3.82405248,3.591414347,6.464873166));
#115573=CARTESIAN_POINT('Ctrl Pts',(-3.460451162,3.656498153,6.653967069));
#115574=CARTESIAN_POINT('Origin',(0.120698810537666,3.48216456265301,-0.156038612835599));
#115575=CARTESIAN_POINT('Ctrl Pts',(-4.836567476,3.656505752,5.400936498));
#115576=CARTESIAN_POINT('Ctrl Pts',(-4.542521114,3.590992329,5.66425658500001));
#115577=CARTESIAN_POINT('Ctrl Pts',(-4.221625324,3.525679915,5.894097015));
#115578=CARTESIAN_POINT('Ctrl Pts',(-5.18388806,3.656505752,5.420083448));
#115579=CARTESIAN_POINT('Ctrl Pts',(-4.88879927000001,3.590992329,5.702312914));
#115580=CARTESIAN_POINT('Ctrl Pts',(-4.564814309,3.525679915,5.950837783));
#115581=CARTESIAN_POINT('',(-4.83306142853521,3.65572482707056,5.40407413172743));
#115582=CARTESIAN_POINT('Origin',(0.129134690010613,3.62499996686943,-0.152028384945294));
#115583=CARTESIAN_POINT('Ctrl Pts',(-5.00047084119201,3.61640598737593,
5.58974877456337));
#115584=CARTESIAN_POINT('Ctrl Pts',(-4.9725732618041,3.62265476502778,5.55874620709649));
#115585=CARTESIAN_POINT('Ctrl Pts',(-4.94466105705915,3.62905099620991,
5.52775599881448));
#115586=CARTESIAN_POINT('Ctrl Pts',(-4.88886753538952,3.64214708596028,
5.46587298098712));
#115587=CARTESIAN_POINT('Ctrl Pts',(-4.86095592515247,3.64885405180903,
5.43494656698116));
#115588=CARTESIAN_POINT('Ctrl Pts',(-4.83306143032981,3.65572482669157,
5.40407413074731));
#115589=CARTESIAN_POINT('Ctrl Pts',(-5.4082532696763,3.52114709502067,4.82846175061348));
#115590=CARTESIAN_POINT('Ctrl Pts',(-5.39911798483816,3.52341350501031,
4.8386166993068));
#115591=CARTESIAN_POINT('Ctrl Pts',(-5.3899827,3.525679915,4.848771648));
#115592=CARTESIAN_POINT('Ctrl Pts',(-5.125025008,3.591414347,5.143303435));
#115593=CARTESIAN_POINT('Ctrl Pts',(-4.8295518,3.656498153,5.407210872));
#115594=CARTESIAN_POINT('Ctrl Pts',(-5.42796399453673,3.52114709502066,
5.17647145195521));
#115595=CARTESIAN_POINT('Ctrl Pts',(-5.4181729145251,3.52341350501031,5.18666106539168));
#115596=CARTESIAN_POINT('Ctrl Pts',(-5.40838183451358,3.525679915,5.19685067882805));
#115597=CARTESIAN_POINT('Ctrl Pts',(-5.12440361073537,3.591414347,5.49238787403437));
#115598=CARTESIAN_POINT('Ctrl Pts',(-4.80991356956551,3.656498153,5.75522219454662));
#115599=CARTESIAN_POINT('Origin',(0.151420717534398,3.48216457228584,-0.126443930581133));
#115600=CARTESIAN_POINT('Ctrl Pts',(-5.884532912,3.656505752,4.234946565));
#115601=CARTESIAN_POINT('Ctrl Pts',(-5.653967226,3.590992329,4.55532165));
#115602=CARTESIAN_POINT('Ctrl Pts',(-5.3899827,3.525679915,4.848771648));
#115603=CARTESIAN_POINT('Ctrl Pts',(-6.22784936200001,3.656505752,4.178982211));
#115604=CARTESIAN_POINT('Ctrl Pts',(-6.000330577,3.590992329,4.518048676));
#115605=CARTESIAN_POINT('Ctrl Pts',(-5.737345705,3.525679915,4.830410362));
#115606=CARTESIAN_POINT('',(-5.88178333324202,3.65572482709196,4.23876453860927));
#115607=CARTESIAN_POINT('Origin',(0.158797259040004,3.62499998761159,-0.120713940849514));
#115608=CARTESIAN_POINT('Ctrl Pts',(-6.08519336616646,3.6164059874159,4.38411013664156));
#115609=CARTESIAN_POINT('Ctrl Pts',(-6.05128338114145,3.62265476506354,
4.35982954685296));
#115610=CARTESIAN_POINT('Ctrl Pts',(-6.01736176949393,3.62905099625138,
4.33556417130597));
#115611=CARTESIAN_POINT('Ctrl Pts',(-5.94956971260826,3.64214707386253,
4.28712194686511));
#115612=CARTESIAN_POINT('Ctrl Pts',(-5.91566236205225,3.6488540458823,4.26291872248395));
#115613=CARTESIAN_POINT('Ctrl Pts',(-5.88178333430147,3.65572482674346,
4.23876453754314));
#115614=CARTESIAN_POINT('Ctrl Pts',(-6.31978786236768,3.52114709501928,
3.55296041125809));
#115615=CARTESIAN_POINT('Ctrl Pts',(-6.31304916918384,3.52341350500961,
3.56484175912901));
#115616=CARTESIAN_POINT('Ctrl Pts',(-6.306310476,3.525679915,3.576723107));
#115617=CARTESIAN_POINT('Ctrl Pts',(-6.110862975,3.591414347,3.921326977));
#115618=CARTESIAN_POINT('Ctrl Pts',(-5.879030064,3.656498153,4.24258241));
#115619=CARTESIAN_POINT('Ctrl Pts',(-6.41384955991653,3.52114709501927,
3.88859661673224));
#115620=CARTESIAN_POINT('Ctrl Pts',(-6.40647785557602,3.52341350500961,
3.90065279546533));
#115621=CARTESIAN_POINT('Ctrl Pts',(-6.39910615123553,3.525679915,3.91270897419841));
#115622=CARTESIAN_POINT('Ctrl Pts',(-6.18529894082314,3.591414347,4.26238359815085));
#115623=CARTESIAN_POINT('Ctrl Pts',(-5.93466311169445,3.656498153,4.58667905973639));
#115624=CARTESIAN_POINT('Origin',(0.175062231256731,3.48216460447819,-0.0909367358897484));
#115625=CARTESIAN_POINT('Ctrl Pts',(-6.65734413,3.656505752,2.870935237));
#115626=CARTESIAN_POINT('Ctrl Pts',(-6.501040115,3.590992329,3.233384938));
#115627=CARTESIAN_POINT('Ctrl Pts',(-6.306310476,3.525679915,3.576723107));
#115628=CARTESIAN_POINT('Ctrl Pts',(-6.98060335100001,3.656505752,2.74247641));
#115629=CARTESIAN_POINT('Ctrl Pts',(-6.831293095,3.590992329,3.122525503));
#115630=CARTESIAN_POINT('Ctrl Pts',(-6.64160519300001,3.525679915,3.48411832));
#115631=CARTESIAN_POINT('',(-6.65547958607909,3.65572482707743,2.87525502706408));
#115632=CARTESIAN_POINT('Origin',(0.181034478709273,3.62499995426716,-0.0837549443061048));
#115633=CARTESIAN_POINT('Ctrl Pts',(-6.8853790129272,3.61640598740089,2.9734753811648));
#115634=CARTESIAN_POINT('Ctrl Pts',(-6.84704221537427,3.62265476505728,
2.95705210249716));
#115635=CARTESIAN_POINT('Ctrl Pts',(-6.8086973335704,3.629050996263,2.94064618172772));
#115636=CARTESIAN_POINT('Ctrl Pts',(-6.73207659066832,3.6421470704921,2.90790980639303));
#115637=CARTESIAN_POINT('Ctrl Pts',(-6.69375898669547,3.64885404423382,
2.89156151352313));
#115638=CARTESIAN_POINT('Ctrl Pts',(-6.65547958665254,3.6557248267469,2.87525502557864));
#115639=CARTESIAN_POINT('Ctrl Pts',(-6.93581619739237,3.52114709500757,
2.11132659215546));
#115640=CARTESIAN_POINT('Ctrl Pts',(-6.93178918969624,3.52341350500376,
2.12437878057777));
#115641=CARTESIAN_POINT('Ctrl Pts',(-6.927762182,3.525679915,2.137430969));
#115642=CARTESIAN_POINT('Ctrl Pts',(-6.810963781,3.591414347,2.515993627));
#115643=CARTESIAN_POINT('Ctrl Pts',(-6.653611416,3.656498153,2.87957551));
#115644=CARTESIAN_POINT('Ctrl Pts',(-7.09983064816225,3.52114709500757,
2.41889532507528));
#115645=CARTESIAN_POINT('Ctrl Pts',(-7.09522301220064,3.52341350500376,
2.43225433561989));
#115646=CARTESIAN_POINT('Ctrl Pts',(-7.09061537623906,3.525679915,2.44561334616444));
#115647=CARTESIAN_POINT('Ctrl Pts',(-6.95697656715272,3.591414347,2.83307500212556));
#115648=CARTESIAN_POINT('Ctrl Pts',(-6.78191440265768,3.656498153,3.20366791037357));
#115649=CARTESIAN_POINT('Origin',(0.19051800560537,3.48216457483211,-0.051177446463225));
#115650=CARTESIAN_POINT('Ctrl Pts',(-7.118865336,3.656505752,1.372682168));
#115651=CARTESIAN_POINT('Ctrl Pts',(-7.044131593,3.590992329,1.760258739));
#115652=CARTESIAN_POINT('Ctrl Pts',(-6.927762182,3.525679915,2.137430969));
#115653=CARTESIAN_POINT('Ctrl Pts',(-7.40695208500001,3.656505752,1.17773546));
#115654=CARTESIAN_POINT('Ctrl Pts',(-7.34283194100001,3.590992329,1.580996508));
#115655=CARTESIAN_POINT('Ctrl Pts',(-7.235310603,3.525679915,1.974912778));
#115656=CARTESIAN_POINT('',(-7.11797301064352,3.65572482706536,1.37730178611899));
#115657=CARTESIAN_POINT('Origin',(0.194806978521487,3.62499997097553,-0.0428797811535073));
#115658=CARTESIAN_POINT('Ctrl Pts',(-7.36361198972982,3.61640598740004,
1.42380422152945));
#115659=CARTESIAN_POINT('Ctrl Pts',(-7.32264096578964,3.62265476504334,
1.41600618821163));
#115660=CARTESIAN_POINT('Ctrl Pts',(-7.28166577807003,3.62905099623261,
1.40822684487029));
#115661=CARTESIAN_POINT('Ctrl Pts',(-7.1997989301185,3.64214708684124,1.39272700326385));
#115662=CARTESIAN_POINT('Ctrl Pts',(-7.15886282522454,3.64885405225192,
1.38499808700501));
#115663=CARTESIAN_POINT('Ctrl Pts',(-7.11797301143247,3.65572482669986,
1.37730178429856));
#115664=CARTESIAN_POINT('Ctrl Pts',(-7.22753347549519,3.52114709522439,
0.570969490054872));
#115665=CARTESIAN_POINT('Ctrl Pts',(-7.22640645174754,3.52341350511217,
0.584582212527431));
#115666=CARTESIAN_POINT('Ctrl Pts',(-7.225279428,3.525679915,0.598194935));
#115667=CARTESIAN_POINT('Ctrl Pts',(-7.19259149,3.591414347,0.993015212));
#115668=CARTESIAN_POINT('Ctrl Pts',(-7.117077294,3.656498153,1.38192286));
#115669=CARTESIAN_POINT('Ctrl Pts',(-7.4538315460106,3.52114709522438,0.836089178790157));
#115670=CARTESIAN_POINT('Ctrl Pts',(-7.45220342644917,3.52341350511217,
0.850126367903856));
#115671=CARTESIAN_POINT('Ctrl Pts',(-7.45057530688761,3.525679915,0.864163557017569));
#115672=CARTESIAN_POINT('Ctrl Pts',(-7.40335370095443,3.591414347,1.27129496701621));
#115673=CARTESIAN_POINT('Ctrl Pts',(-7.31205091454397,3.656498153,1.67085681056018));
#115674=CARTESIAN_POINT('Origin',(0.197065557393947,3.48216456643412,-0.00902521413211094));
#115675=CARTESIAN_POINT('Ctrl Pts',(-7.24751631,3.656505752,-0.189755993));
#115676=CARTESIAN_POINT('Ctrl Pts',(-7.25784730700001,3.590992329,0.204824799));
#115677=CARTESIAN_POINT('Ctrl Pts',(-7.225279428,3.525679915,0.598194935));
#115678=CARTESIAN_POINT('Ctrl Pts',(-7.486959971,3.656505752,-0.44207509));
#115679=CARTESIAN_POINT('Ctrl Pts',(-7.511028126,3.590992329,-0.034458126));
#115680=CARTESIAN_POINT('Ctrl Pts',(-7.490700931,3.525679915,0.373362509));
#115681=CARTESIAN_POINT('',(-7.24763792833492,3.65572482708963,-0.18505255615449));
#115682=CARTESIAN_POINT('Origin',(0.199470203544115,3.62499995356544,4.69240348278943E-7));
#115683=CARTESIAN_POINT('Ctrl Pts',(-7.49753065349767,3.61640598744145,
-0.192442440658621));
#115684=CARTESIAN_POINT('Ctrl Pts',(-7.45584116260823,3.62265476509222,
-0.191250601216073));
#115685=CARTESIAN_POINT('Ctrl Pts',(-7.41415162318376,3.62905099626916,
-0.190039613672391));
#115686=CARTESIAN_POINT('Ctrl Pts',(-7.33086684937623,3.64214707419444,
-0.187578127585177));
#115687=CARTESIAN_POINT('Ctrl Pts',(-7.28922627644256,3.64885404603143,
-0.186326292333282));
#115688=CARTESIAN_POINT('Ctrl Pts',(-7.24763792841524,3.65572482669476,
-0.185052557297352));
#115689=CARTESIAN_POINT('Ctrl Pts',(-7.18389057158659,3.52436392548355,
-0.976872129593754));
#115690=CARTESIAN_POINT('Ctrl Pts',(-7.1844206052933,3.52502192024177,-0.972942079296878));
#115691=CARTESIAN_POINT('Ctrl Pts',(-7.184950639,3.525679915,-0.969012029));
#115692=CARTESIAN_POINT('Ctrl Pts',(-7.23790161500001,3.591414347,-0.576395491));
#115693=CARTESIAN_POINT('Ctrl Pts',(-7.24775654700001,3.656498153,-0.180346967));
#115694=CARTESIAN_POINT('Ctrl Pts',(-7.46075501751712,3.52436392548355,
-0.766290988866588));
#115695=CARTESIAN_POINT('Ctrl Pts',(-7.46116970125857,3.52502192024177,
-0.762209624433295));
#115696=CARTESIAN_POINT('Ctrl Pts',(-7.461584385,3.525679915,-0.75812826));
#115697=CARTESIAN_POINT('Ctrl Pts',(-7.503011767,3.591414347,-0.350395266));
#115698=CARTESIAN_POINT('Ctrl Pts',(-7.499764582,3.656498153,0.0594240580000001));
#115699=CARTESIAN_POINT('Origin',(0.194398464463127,3.4821645223859,0.0335490630156204));
#115700=CARTESIAN_POINT('Ctrl Pts',(-7.037281477,3.656505752,-1.743321375));
#115701=CARTESIAN_POINT('Ctrl Pts',(-7.132194147,3.590992329,-1.360186522));
#115702=CARTESIAN_POINT('Ctrl Pts',(-7.184950639,3.525679915,-0.969012029));
#115703=CARTESIAN_POINT('Ctrl Pts',(-7.216885931,3.656505752,-2.041214701));
#115704=CARTESIAN_POINT('Ctrl Pts',(-7.328016983,3.590992329,-1.648301537));
#115705=CARTESIAN_POINT('Ctrl Pts',(-7.395834409,3.525679915,-1.245645776));
#115706=CARTESIAN_POINT('',(-7.03841135162036,3.65572482709059,-1.73875404613841));
#115707=CARTESIAN_POINT('Origin',(0.194806796920498,3.62499999752868,0.0428807018726299));
#115708=CARTESIAN_POINT('Ctrl Pts',(-7.28087311686949,3.61640598742508,
-1.79969070845467));
#115709=CARTESIAN_POINT('Ctrl Pts',(-7.24041451346179,3.62265476507037,
-1.78956472535037));
#115710=CARTESIAN_POINT('Ctrl Pts',(-7.19995997890244,3.6290509962478,-1.77942003139437));
#115711=CARTESIAN_POINT('Ctrl Pts',(-7.11915142346629,3.64214708718919,
-1.75911230892189));
#115712=CARTESIAN_POINT('Ctrl Pts',(-7.07875353435021,3.64885405242303,
-1.74893825936027));
#115713=CARTESIAN_POINT('Ctrl Pts',(-7.0384113518051,3.65572482670577,-1.73875404767568));
#115714=CARTESIAN_POINT('Ctrl Pts',(-6.80593657008117,3.52436392548355,
-2.49835752065326));
#115715=CARTESIAN_POINT('Ctrl Pts',(-6.80729905654059,3.52502192024177,
-2.49463329432663));
#115716=CARTESIAN_POINT('Ctrl Pts',(-6.808661543,3.525679915,-2.490909068));
#115717=CARTESIAN_POINT('Ctrl Pts',(-6.944775505,3.591414347,-2.118854581));
#115718=CARTESIAN_POINT('Ctrl Pts',(-7.03953876,3.656498153,-1.734183971));
#115719=CARTESIAN_POINT('Ctrl Pts',(-7.121596800251,3.52436392548355,-2.35221732129617));
#115720=CARTESIAN_POINT('Ctrl Pts',(-7.12287916162549,3.52502192024177,
-2.34832052164809));
#115721=CARTESIAN_POINT('Ctrl Pts',(-7.124161523,3.525679915,-2.344423722));
#115722=CARTESIAN_POINT('Ctrl Pts',(-7.25227089700001,3.591414347,-1.955128962));
#115723=CARTESIAN_POINT('Ctrl Pts',(-7.33719866900001,3.656498153,-1.554192937));
#115724=CARTESIAN_POINT('Origin',(0.182641489301882,3.48216454051536,0.0745546352115367));
#115725=CARTESIAN_POINT('Ctrl Pts',(-6.497991183,3.656505752,-3.215370987));
#115726=CARTESIAN_POINT('Ctrl Pts',(-6.673047516,3.590992329,-2.861597032));
#115727=CARTESIAN_POINT('Ctrl Pts',(-6.808661543,3.525679915,-2.490909068));
#115728=CARTESIAN_POINT('Ctrl Pts',(-6.609358326,3.656505752,-3.544909382));
#115729=CARTESIAN_POINT('Ctrl Pts',(-6.80235591100001,3.590992329,-3.1850722));
#115730=CARTESIAN_POINT('Ctrl Pts',(-6.955146889,3.525679915,-2.806409048));
#115731=CARTESIAN_POINT('',(-6.50007648309978,3.65572482710153,-3.21115332982368));
#115732=CARTESIAN_POINT('Origin',(0.181034151573773,3.6249999647383,0.0837558341557831));
#115733=CARTESIAN_POINT('Ctrl Pts',(-6.7237700457547,3.61640598738409,-3.32278743899844));
#115734=CARTESIAN_POINT('Ctrl Pts',(-6.6864341290363,3.62265476504407,-3.30420079200989));
#115735=CARTESIAN_POINT('Ctrl Pts',(-6.64910620829098,3.62905099623725,
-3.28559674629475));
#115736=CARTESIAN_POINT('Ctrl Pts',(-6.57455251052107,3.64214708041289,
-3.24839237571768));
#115737=CARTESIAN_POINT('Ctrl Pts',(-6.53728620099037,3.64885404908062,
-3.22977182764316));
#115738=CARTESIAN_POINT('Ctrl Pts',(-6.50007648257382,3.6557248266913,-3.21115333145444));
#115739=CARTESIAN_POINT('Ctrl Pts',(-6.10974453928919,3.52436392548355,
-3.90302249135112));
#115740=CARTESIAN_POINT('Ctrl Pts',(-6.11187577014459,3.52502192024177,
-3.89967822967556));
#115741=CARTESIAN_POINT('Ctrl Pts',(-6.114007001,3.525679915,-3.896333968));
#115742=CARTESIAN_POINT('Ctrl Pts',(-6.326919411,3.591414347,-3.562238386));
#115743=CARTESIAN_POINT('Ctrl Pts',(-6.502159964,3.656498153,-3.20693246));
#115744=CARTESIAN_POINT('Ctrl Pts',(-6.44944063157123,3.52436392548355,
-3.8281565867108));
#115745=CARTESIAN_POINT('Ctrl Pts',(-6.45153070878562,3.52502192024177,
-3.8246265618554));
#115746=CARTESIAN_POINT('Ctrl Pts',(-6.453620786,3.525679915,-3.821096537));
#115747=CARTESIAN_POINT('Ctrl Pts',(-6.6624219,3.591414347,-3.468443));
#115748=CARTESIAN_POINT('Ctrl Pts',(-6.831553502,3.656498153,-3.095137598));
#115749=CARTESIAN_POINT('Origin',(0.162344440831546,3.48216455730966,0.112074132583539));
#115750=CARTESIAN_POINT('Ctrl Pts',(-5.65486204400001,3.656505752,-4.537073425));
#115751=CARTESIAN_POINT('Ctrl Pts',(-5.9018766,3.590992329,-4.229202446));
#115752=CARTESIAN_POINT('Ctrl Pts',(-6.114007001,3.525679915,-3.896333968));
#115753=CARTESIAN_POINT('Ctrl Pts',(-5.692784471,3.656505752,-4.882848039));
#115754=CARTESIAN_POINT('Ctrl Pts',(-5.958624237,3.590992329,-4.572912427));
#115755=CARTESIAN_POINT('Ctrl Pts',(-6.189244432,3.525679915,-4.235947753));
#115756=CARTESIAN_POINT('',(-5.65780526222359,3.65572482709928,-4.53340265263039));
#115757=CARTESIAN_POINT('Origin',(0.158796591899044,3.6249999668739,0.120714626165824));
#115758=CARTESIAN_POINT('Ctrl Pts',(-5.85227096027948,3.6164059873619,-4.69051432171717));
#115759=CARTESIAN_POINT('Ctrl Pts',(-5.81980351626557,3.62265476501948,
-4.66433610172348));
#115760=CARTESIAN_POINT('Ctrl Pts',(-5.78734762151533,3.62905099620998,
-4.63814260870191));
#115761=CARTESIAN_POINT('Ctrl Pts',(-5.72253480594774,3.64214707671741,
-4.58578122911816));
#115762=CARTESIAN_POINT('Ctrl Pts',(-5.69014261976763,3.6488540472637,-4.5595848563537));
#115763=CARTESIAN_POINT('Ctrl Pts',(-5.65780526166865,3.65572482670257,
-4.53340265385012));
#115764=CARTESIAN_POINT('Ctrl Pts',(-5.12786764447628,3.52436392548355,
-5.1251864671127));
#115765=CARTESIAN_POINT('Ctrl Pts',(-5.13066796573815,3.52502192024177,
-5.12237854405635));
#115766=CARTESIAN_POINT('Ctrl Pts',(-5.133468287,3.525679915,-5.119570621));
#115767=CARTESIAN_POINT('Ctrl Pts',(-5.413223597,3.591414347,-4.839055883));
#115768=CARTESIAN_POINT('Ctrl Pts',(-5.660747395,3.656498153,-4.529728351));
#115769=CARTESIAN_POINT('Ctrl Pts',(-5.47571578726615,3.52436392548355,
-5.12509550503651));
#115770=CARTESIAN_POINT('Ctrl Pts',(-5.47851585063307,3.52502192024177,
-5.12209731501825));
#115771=CARTESIAN_POINT('Ctrl Pts',(-5.481315914,3.525679915,-5.119099125));
#115772=CARTESIAN_POINT('Ctrl Pts',(-5.76104546,3.591414347,-4.819576499));
#115773=CARTESIAN_POINT('Ctrl Pts',(-6.006472486,3.656498153,-4.491357064));
#115774=CARTESIAN_POINT('Origin',(0.134456337787808,3.48216453075468,0.144353208218625));
#115775=CARTESIAN_POINT('Ctrl Pts',(-4.54731784,3.656505752,-5.646627353));
#115776=CARTESIAN_POINT('Ctrl Pts',(-4.854740493,3.590992329,-5.399055054));
#115777=CARTESIAN_POINT('Ctrl Pts',(-5.133468287,3.525679915,-5.119570621));
#115778=CARTESIAN_POINT('Ctrl Pts',(-4.510022341,3.656505752,-5.992470149));
#115779=CARTESIAN_POINT('Ctrl Pts',(-4.836273917,3.590992329,-5.746928351));
#115780=CARTESIAN_POINT('Ctrl Pts',(-5.133939783,3.525679915,-5.467418248));
#115781=CARTESIAN_POINT('',(-4.55098135572124,3.65572482706278,-5.64367510519807));
#115782=CARTESIAN_POINT('Origin',(0.129133949453862,3.62499998608658,0.152028971897459));
#115783=CARTESIAN_POINT('Ctrl Pts',(-4.70712618881638,3.6164059874195,-5.83891796798881));
#115784=CARTESIAN_POINT('Ctrl Pts',(-4.681045359071,3.62265476505457,-5.8063722394639));
#115785=CARTESIAN_POINT('Ctrl Pts',(-4.65497909171544,3.62905099624552,
-5.77381407758711));
#115786=CARTESIAN_POINT('Ctrl Pts',(-4.60293773645466,3.64214707069617,
-5.70874406817838));
#115787=CARTESIAN_POINT('Ctrl Pts',(-4.5769342946032,3.64885404428948,-5.67619677349355));
#115788=CARTESIAN_POINT('Ctrl Pts',(-4.5509813544537,3.65572482666267,-5.64367510615619));
#115789=CARTESIAN_POINT('Ctrl Pts',(-3.8898961054492,3.52114709484942,-6.11816595059717));
#115790=CARTESIAN_POINT('Ctrl Pts',(-3.90139520322457,3.52341350492468,
-6.11079389679852));
#115791=CARTESIAN_POINT('Ctrl Pts',(-3.912894301,3.525679915,-6.103421843));
#115792=CARTESIAN_POINT('Ctrl Pts',(-4.246411465,3.591414347,-5.889604505));
#115793=CARTESIAN_POINT('Ctrl Pts',(-4.55464456900001,3.656498153,-5.640719178));
#115794=CARTESIAN_POINT('Ctrl Pts',(-4.23013246864957,3.52114709484942,
-6.1939187206583));
#115795=CARTESIAN_POINT('Ctrl Pts',(-4.24177187036649,3.52341350492468,
-6.18590511891521));
#115796=CARTESIAN_POINT('Ctrl Pts',(-4.25341127208348,3.525679915,-6.17789151717195));
#115797=CARTESIAN_POINT('Ctrl Pts',(-4.59099777905268,3.591414347,-5.9454668714277));
#115798=CARTESIAN_POINT('Ctrl Pts',(-4.90124848342061,3.656498153,-5.67764161846073));
#115799=CARTESIAN_POINT('Origin',(0.100281084784133,3.48216457830553,0.169882325752175));
#115800=CARTESIAN_POINT('Ctrl Pts',(-3.227146108,3.656505752,-6.492151261));
#115801=CARTESIAN_POINT('Ctrl Pts',(-3.580602117,3.590992329,-6.316453848));
#115802=CARTESIAN_POINT('Ctrl Pts',(-3.912894301,3.525679915,-6.103421843));
#115803=CARTESIAN_POINT('Ctrl Pts',(-3.116376579,3.656505752,-6.821891015));
#115804=CARTESIAN_POINT('Ctrl Pts',(-3.487784803,3.590992329,-6.652224292));
#115805=CARTESIAN_POINT('Ctrl Pts',(-3.838577816,3.525679915,-6.443238343));
#115806=CARTESIAN_POINT('',(-3.23135861876458,3.65572482706242,-6.49005558269118));
#115807=CARTESIAN_POINT('Origin',(0.0934331116377524,3.62499994453812,0.176234561179893));
#115808=CARTESIAN_POINT('Ctrl Pts',(-3.34188142830791,3.61640598742262,
-6.7143002994709));
#115809=CARTESIAN_POINT('Ctrl Pts',(-3.32340672345575,3.62265476506398,
-6.67690886461093));
#115810=CARTESIAN_POINT('Ctrl Pts',(-3.30494891336774,3.62905099624106,
-6.63950841770322));
#115811=CARTESIAN_POINT('Ctrl Pts',(-3.26811231382241,3.64214709583241,
-6.56477221270267));
#115812=CARTESIAN_POINT('Ctrl Pts',(-3.24971356186776,3.64885405664215,
-6.52739596079861));
#115813=CARTESIAN_POINT('Ctrl Pts',(-3.23135861705088,3.65572482665306,
-6.49005558433552));
#115814=CARTESIAN_POINT('Ctrl Pts',(-2.48372766966525,3.52114709510818,
-6.81133930780071));
#115815=CARTESIAN_POINT('Ctrl Pts',(-2.49654269783263,3.52341350505406,
-6.80661157490037));
#115816=CARTESIAN_POINT('Ctrl Pts',(-2.509357726,3.525679915,-6.801883842));
#115817=CARTESIAN_POINT('Ctrl Pts',(-2.881041851,3.591414347,-6.66476176600001));
#115818=CARTESIAN_POINT('Ctrl Pts',(-3.235571625,3.656498153,-6.487956247));
#115819=CARTESIAN_POINT('Ctrl Pts',(-2.79972488961055,3.52114709510818,
-6.95846178142387));
#115820=CARTESIAN_POINT('Ctrl Pts',(-2.81281485533693,3.52341350505406,
-6.95313766082784));
#115821=CARTESIAN_POINT('Ctrl Pts',(-2.82590482106331,3.525679915,-6.94781354023191));
#115822=CARTESIAN_POINT('Ctrl Pts',(-3.20556317169257,3.591414347,-6.79339397288846));
#115823=CARTESIAN_POINT('Ctrl Pts',(-3.56613489948184,3.656498153,-6.5985250570152));
#115824=CARTESIAN_POINT('Origin',(0.0614169840414003,3.48216457005707,0.187468286320412));
#115825=CARTESIAN_POINT('Ctrl Pts',(-1.756076611,3.656505752,-7.034109392));
#115826=CARTESIAN_POINT('Ctrl Pts',(-2.139038765,3.590992329,-6.93850228));
#115827=CARTESIAN_POINT('Ctrl Pts',(-2.509357726,3.525679915,-6.801883842));
#115828=CARTESIAN_POINT('Ctrl Pts',(-1.577012512,3.656505752,-7.332327839));
#115829=CARTESIAN_POINT('Ctrl Pts',(-1.976210748,3.590992329,-7.246469619));
#115830=CARTESIAN_POINT('Ctrl Pts',(-2.363728217,3.525679915,-7.117779774));
#115831=CARTESIAN_POINT('',(-1.76064114414197,3.65572482706168,-7.03296827468653));
#115832=CARTESIAN_POINT('Origin',(0.053363518657509,3.62499993664306,0.192199759904212));
#115833=CARTESIAN_POINT('Ctrl Pts',(-1.82037400642531,3.61640598742844,
-7.27572941159549));
#115834=CARTESIAN_POINT('Ctrl Pts',(-1.81036928315251,3.62265476507407,
-7.23524065217722));
#115835=CARTESIAN_POINT('Ctrl Pts',(-1.80038299703673,3.62905099622303,
-7.19474672351256));
#115836=CARTESIAN_POINT('Ctrl Pts',(-1.78047370801797,3.64214708508883,
-7.11383909568418));
#115837=CARTESIAN_POINT('Ctrl Pts',(-1.77053988931242,3.64885405136343,
-7.07338145667437));
#115838=CARTESIAN_POINT('Ctrl Pts',(-1.7606411424949,3.65572482666902,-7.03296827582325));
#115839=CARTESIAN_POINT('Ctrl Pts',(-0.96142288802051,3.5211470951993,-7.18602201069066));
#115840=CARTESIAN_POINT('Ctrl Pts',(-0.974954630510261,3.52341350509963,
-7.18415966184533));
#115841=CARTESIAN_POINT('Ctrl Pts',(-0.988486373,3.525679915,-7.182297313));
#115842=CARTESIAN_POINT('Ctrl Pts',(-1.380957923,3.591414347,-7.128282175));
#115843=CARTESIAN_POINT('Ctrl Pts',(-1.765206948,3.656498153,-7.031823692));
#115844=CARTESIAN_POINT('Ctrl Pts',(-1.23840528569355,3.5211470951993,-7.39763490453268));
#115845=CARTESIAN_POINT('Ctrl Pts',(-1.25233374354749,3.52341350509963,
-7.39524921465165));
#115846=CARTESIAN_POINT('Ctrl Pts',(-1.26626220140147,3.525679915,-7.3928635247706));
#115847=CARTESIAN_POINT('Ctrl Pts',(-1.6702399926727,3.591414347,-7.32366952361838));
#115848=CARTESIAN_POINT('Ctrl Pts',(-2.06427281173036,3.656498153,-7.21086879729882));
#115849=CARTESIAN_POINT('Origin',(0.019680936437359,3.48216458086525,0.196288130968899));
#115850=CARTESIAN_POINT('Ctrl Pts',(-0.202894923,3.656505752,-7.247160385));
#115851=CARTESIAN_POINT('Ctrl Pts',(-0.597456338000001,3.590992329,-7.23611405800001));
#115852=CARTESIAN_POINT('Ctrl Pts',(-0.988486373,3.525679915,-7.182297313));
#115853=CARTESIAN_POINT('Ctrl Pts',(0.036090908,3.656505752,-7.499913163));
#115854=CARTESIAN_POINT('Ctrl Pts',(-0.372231275,3.590992329,-7.501878081));
#115855=CARTESIAN_POINT('Ctrl Pts',(-0.778353314,3.525679915,-7.459501734));
#115856=CARTESIAN_POINT('',(-0.207598047069502,3.65572482706502,-7.24702718637008));
#115857=CARTESIAN_POINT('Origin',(0.010798619422784,3.62499991866262,0.199177593573561));
#115858=CARTESIAN_POINT('Ctrl Pts',(-0.213747918968888,3.6164059912397,
-7.49695347696992));
#115859=CARTESIAN_POINT('Ctrl Pts',(-0.212680986910659,3.62265476894078,
-7.45526060255481));
#115860=CARTESIAN_POINT('Ctrl Pts',(-0.211633172836877,3.62905099623971,
-7.41356666842584));
#115861=CARTESIAN_POINT('Ctrl Pts',(-0.209582099320455,3.64214709043449,
-7.33027067337734));
#115862=CARTESIAN_POINT('Ctrl Pts',(-0.208577724648146,3.64885405398644,
-7.28862345213346));
#115863=CARTESIAN_POINT('Ctrl Pts',(-0.207598044645775,3.65572482664597,
-7.24702718686974));
#115864=CARTESIAN_POINT('Ctrl Pts',(0.586511467990447,3.52436392548355,
-7.22624156853374));
#115865=CARTESIAN_POINT('Ctrl Pts',(0.582558485995224,3.52502192024177,
-7.22655805626688));
#115866=CARTESIAN_POINT('Ctrl Pts',(0.578605504000001,3.525679915,-7.226874544));
#115867=CARTESIAN_POINT('Ctrl Pts',(0.183698063,3.591414347,-7.258492032));
#115868=CARTESIAN_POINT('Ctrl Pts',(-0.212303156,3.656498153,-7.246890876));
#115869=CARTESIAN_POINT('Ctrl Pts',(0.361250022558109,3.52436392548355,
-7.49129933610564));
#115870=CARTESIAN_POINT('Ctrl Pts',(0.357152193279055,3.52502192024177,
-7.49149245105282));
#115871=CARTESIAN_POINT('Ctrl Pts',(0.353054364,3.525679915,-7.491685566));
#115872=CARTESIAN_POINT('Ctrl Pts',(-0.056323487,3.591414347,-7.510977971));
#115873=CARTESIAN_POINT('Ctrl Pts',(-0.465365977,3.656498153,-7.485548377));
#115874=CARTESIAN_POINT('Origin',(-0.0229753300832009,3.48216457544246,
0.195929666396335));
#115875=CARTESIAN_POINT('Ctrl Pts',(1.359773906,3.656505752,-7.121342214));
#115876=CARTESIAN_POINT('Ctrl Pts',(0.972062484,3.590992329,-7.19537318400001));
#115877=CARTESIAN_POINT('Ctrl Pts',(0.578605504,3.525679915,-7.226874544));
#115878=CARTESIAN_POINT('Ctrl Pts',(1.647506757,3.656505752,-7.316810882));
#115879=CARTESIAN_POINT('Ctrl Pts',(1.249153319,3.590992329,-7.406507061));
#115880=CARTESIAN_POINT('Ctrl Pts',(0.843416526,3.525679915,-7.452425683));
#115881=CARTESIAN_POINT('',(1.35515210503228,3.65572482705034,-7.12222316170083));
#115882=CARTESIAN_POINT('Origin',(-0.032271179737238,3.62499994809109,0.196842596556915));
#115883=CARTESIAN_POINT('Ctrl Pts',(1.40287278318669,3.61640598739448,-7.36762837997685));
#115884=CARTESIAN_POINT('Ctrl Pts',(1.39495203533521,3.62265476504023,-7.32668090293707));
#115885=CARTESIAN_POINT('Ctrl Pts',(1.38701238381459,3.62905099619008,-7.28573647595259));
#115886=CARTESIAN_POINT('Ctrl Pts',(1.37110933111604,3.6421470873043,-7.2039469941694));
#115887=CARTESIAN_POINT('Ctrl Pts',(1.36313730042969,3.64885405241763,-7.1630575408346));
#115888=CARTESIAN_POINT('Ctrl Pts',(1.35515210661499,3.65572482658934,-7.12222316207102));
#115889=CARTESIAN_POINT('Ctrl Pts',(2.12622748692775,3.52436392548355,-6.93121342759178));
#115890=CARTESIAN_POINT('Ctrl Pts',(2.12243495896388,3.52502192024177,-6.93237229029589));
#115891=CARTESIAN_POINT('Ctrl Pts',(2.118642431,3.525679915,-6.933531153));
#115892=CARTESIAN_POINT('Ctrl Pts',(1.739764532,3.591414347,-7.049302868));
#115893=CARTESIAN_POINT('Ctrl Pts',(1.350527695,3.656498153,-7.123101498));
#115894=CARTESIAN_POINT('Ctrl Pts',(1.96321211359414,3.52436392548355,-7.23849884360055));
#115895=CARTESIAN_POINT('Ctrl Pts',(1.95925160329707,3.52502192024177,-7.23956835580028));
#115896=CARTESIAN_POINT('Ctrl Pts',(1.955291093,3.525679915,-7.240637868));
#115897=CARTESIAN_POINT('Ctrl Pts',(1.559631566,3.591414347,-7.347483365));
#115898=CARTESIAN_POINT('Ctrl Pts',(1.154685651,3.656498153,-7.410580345));
#115899=CARTESIAN_POINT('Origin',(-0.0645573202639896,3.48216453713675,
0.186410085550968));
#115900=CARTESIAN_POINT('Ctrl Pts',(2.858861218,3.656505752,-6.662537995));
#115901=CARTESIAN_POINT('Ctrl Pts',(2.496128744,3.590992329,-6.818184657));
#115902=CARTESIAN_POINT('Ctrl Pts',(2.118642431,3.525679915,-6.933531153));
#115903=CARTESIAN_POINT('Ctrl Pts',(3.18188702,3.656505752,-6.791582657));
#115904=CARTESIAN_POINT('Ctrl Pts',(2.812128892,3.590992329,-6.96481600299999));
#115905=CARTESIAN_POINT('Ctrl Pts',(2.425749146,3.525679915,-7.09688249));
#115906=CARTESIAN_POINT('',(2.85453685021956,3.65572482706825,-6.66439189739295));
#115907=CARTESIAN_POINT('Origin',(-0.0738320489144723,3.62499994952612,
0.185303204393322));
#115908=CARTESIAN_POINT('Ctrl Pts',(2.95389671312415,3.61640598741098,-6.89380114309683));
#115909=CARTESIAN_POINT('Ctrl Pts',(2.93735865075867,3.62265476505422,-6.85551372191689));
#115910=CARTESIAN_POINT('Ctrl Pts',(2.92080278241446,3.62905099619161,-6.81723334327981));
#115911=CARTESIAN_POINT('Ctrl Pts',(2.88768921050766,3.64214708846666,-6.74077473349498));
#115912=CARTESIAN_POINT('Ctrl Pts',(2.87111353932749,3.64885405299546,-6.70255500733749));
#115913=CARTESIAN_POINT('Ctrl Pts',(2.85453685203003,3.65572482661415,-6.66439189733454));
#115914=CARTESIAN_POINT('Ctrl Pts',(3.56652347108936,3.52436392548355,-6.31208945091949));
#115915=CARTESIAN_POINT('Ctrl Pts',(3.56306873154468,3.52502192024177,-6.31403650145974));
#115916=CARTESIAN_POINT('Ctrl Pts',(3.559613992,3.525679915,-6.315983552));
#115917=CARTESIAN_POINT('Ctrl Pts',(3.214481544,3.591414347,-6.510496137));
#115918=CARTESIAN_POINT('Ctrl Pts',(2.850209373,3.656498153,-6.66624381));
#115919=CARTESIAN_POINT('Ctrl Pts',(3.47337658852555,3.52436392548355,-6.64723419152526));
#115920=CARTESIAN_POINT('Ctrl Pts',(3.46973858626278,3.52502192024177,-6.64913009176263));
#115921=CARTESIAN_POINT('Ctrl Pts',(3.466100584,3.525679915,-6.651025992));
#115922=CARTESIAN_POINT('Ctrl Pts',(3.10265998,3.591414347,-6.840428603));
#115923=CARTESIAN_POINT('Ctrl Pts',(2.720745461,3.656498153,-6.989101812));
#115924=CARTESIAN_POINT('Origin',(-0.103120705606788,3.48216456522747,0.168174104007248));
#115925=CARTESIAN_POINT('Ctrl Pts',(4.224271357,3.656505752,-5.892200905));
#115926=CARTESIAN_POINT('Ctrl Pts',(3.903478799,3.590992329,-6.122185394));
#115927=CARTESIAN_POINT('Ctrl Pts',(3.559613992,3.525679915,-6.315983552));
#115928=CARTESIAN_POINT('Ctrl Pts',(4.567485784,3.656505752,-5.948787575));
#115929=CARTESIAN_POINT('Ctrl Pts',(4.243612444,3.590992329,-6.19745789));
#115930=CARTESIAN_POINT('Ctrl Pts',(3.894656432,3.525679915,-6.40949695999999));
#115931=CARTESIAN_POINT('',(4.22044662440661,3.65572482707631,-5.89494107545148));
#115932=CARTESIAN_POINT('Origin',(-0.111940529212393,3.62500000250486,0.165099073719102));
#115933=CARTESIAN_POINT('Ctrl Pts',(4.36679971634736,3.61640598740763,-6.09762742671591));
#115934=CARTESIAN_POINT('Ctrl Pts',(4.34241764086447,3.62265476506328,-6.06379033863146));
#115935=CARTESIAN_POINT('Ctrl Pts',(4.31801968949399,3.62905099623956,-6.02996395608197));
#115936=CARTESIAN_POINT('Ctrl Pts',(4.26924399912361,3.64214707620876,-5.9624114087969));
#115937=CARTESIAN_POINT('Ctrl Pts',(4.24483972189627,3.64885404703329,-5.92864848400591));
#115938=CARTESIAN_POINT('Ctrl Pts',(4.22044662594176,3.65572482672606,-5.89494107440452));
#115939=CARTESIAN_POINT('Ctrl Pts',(4.84005278268171,3.52436392548355,-5.39781918605993));
#115940=CARTESIAN_POINT('Ctrl Pts',(4.83709737134085,3.52502192024177,-5.40046338252997));
#115941=CARTESIAN_POINT('Ctrl Pts',(4.83414196,3.525679915,-5.403107579));
#115942=CARTESIAN_POINT('Ctrl Pts',(4.538892973,3.591414347,-5.667265843));
#115943=CARTESIAN_POINT('Ctrl Pts',(4.216618428,3.656498153,-5.89767997));
#115944=CARTESIAN_POINT('Ctrl Pts',(4.82112983456621,3.52436392548355,-5.74515225479416));
#115945=CARTESIAN_POINT('Ctrl Pts',(4.8179844492831,3.52502192024177,-5.74778589289708));
#115946=CARTESIAN_POINT('Ctrl Pts',(4.814839064,3.525679915,-5.750419531));
#115947=CARTESIAN_POINT('Ctrl Pts',(4.500611462,3.591414347,-6.013523002));
#115948=CARTESIAN_POINT('Ctrl Pts',(4.159586238,3.656498153,-6.240820646));
#115949=CARTESIAN_POINT('Origin',(-0.136862052139013,3.48216458582086,0.142074134038869));
#115950=CARTESIAN_POINT('Ctrl Pts',(5.392159262,3.656505752,-4.846351049));
#115951=CARTESIAN_POINT('Ctrl Pts',(5.128306523,3.590992329,-5.13991954600001));
#115952=CARTESIAN_POINT('Ctrl Pts',(4.83414196,3.525679915,-5.403107579));
#115953=CARTESIAN_POINT('Ctrl Pts',(5.739513988,3.656505752,-4.82783379800001));
#115954=CARTESIAN_POINT('Ctrl Pts',(5.476669394,3.590992329,-5.140313533));
#115955=CARTESIAN_POINT('Ctrl Pts',(5.181453912,3.525679915,-5.422410475));
#115956=CARTESIAN_POINT('',(5.38901300557768,3.65572482710028,-4.84984935993923));
#115957=CARTESIAN_POINT('Origin',(-0.144814768043657,3.62499998182717,0.137175170862209));
#115958=CARTESIAN_POINT('Ctrl Pts',(5.57551601750765,3.61640598737869,-5.01633542878598));
#115959=CARTESIAN_POINT('Ctrl Pts',(5.54443000772658,3.62265476503998,-4.98853085853212));
#115960=CARTESIAN_POINT('Ctrl Pts',(5.51333079461945,3.62905099622165,-4.96074015636159));
#115961=CARTESIAN_POINT('Ctrl Pts',(5.4511736065851,3.64214708579882,-4.90525224101104));
#115962=CARTESIAN_POINT('Ctrl Pts',(5.42008188133836,3.64885405174569,-4.87752489447732));
#115963=CARTESIAN_POINT('Ctrl Pts',(5.38901300719692,3.65572482672889,-4.8498493588364));
#115964=CARTESIAN_POINT('Ctrl Pts',(5.89859840263569,3.52114709502404,-4.21542206610258));
#115965=CARTESIAN_POINT('Ctrl Pts',(5.8906146123179,3.52341350501199,-4.22650518405128));
#115966=CARTESIAN_POINT('Ctrl Pts',(5.882630822,3.525679915,-4.237588302));
#115967=CARTESIAN_POINT('Ctrl Pts',(5.651070811,3.591414347,-4.559040496));
#115968=CARTESIAN_POINT('Ctrl Pts',(5.385863092,3.656498153,-4.85334717));
#115969=CARTESIAN_POINT('Ctrl Pts',(5.95582004930385,3.52114709502404,-4.55926061542002));
#115970=CARTESIAN_POINT('Ctrl Pts',(5.94718805603239,3.52341350501199,-4.5704490988617));
#115971=CARTESIAN_POINT('Ctrl Pts',(5.93855606276091,3.525679915,-4.58163758230349));
#115972=CARTESIAN_POINT('Ctrl Pts',(5.68819572295812,3.591414347,-4.90614577273627));
#115973=CARTESIAN_POINT('Ctrl Pts',(5.40396662443608,3.656498153,-5.20144170171409));
#115974=CARTESIAN_POINT('Origin',(-0.164204111051689,3.48216453571289,0.109331279387648));
#115975=CARTESIAN_POINT('Ctrl Pts',(6.307915794,3.656505752,-3.573891204));
#115976=CARTESIAN_POINT('Ctrl Pts',(6.113340333,3.590992329,-3.917316773));
#115977=CARTESIAN_POINT('Ctrl Pts',(5.882630822,3.525679915,-4.237588302));
#115978=CARTESIAN_POINT('Ctrl Pts',(6.64316889699999,3.656505752,-3.481135878));
#115979=CARTESIAN_POINT('Ctrl Pts',(6.45364337,3.590992329,-3.842813829));
#115980=CARTESIAN_POINT('Ctrl Pts',(6.225972366,3.525679915,-4.181778103));
#115981=CARTESIAN_POINT('',(6.30559512823114,3.65572482705793,-3.57798407890505));
#115982=CARTESIAN_POINT('Origin',(-0.170917924835829,3.62499994017976,0.102837358193317));
#115983=CARTESIAN_POINT('Ctrl Pts',(6.52352738649046,3.6164059873846,-3.70048516154021));
#115984=CARTESIAN_POINT('Ctrl Pts',(6.48719098968864,3.62265476503472,-3.68001321990407));
#115985=CARTESIAN_POINT('Ctrl Pts',(6.45084467935911,3.629050996223,-3.65955766037544));
#115986=CARTESIAN_POINT('Ctrl Pts',(6.37821247405543,3.64214707787778,-3.61872900434467));
#115987=CARTESIAN_POINT('Ctrl Pts',(6.34188707287837,3.64885404782154,-3.59833369652542));
#115988=CARTESIAN_POINT('Ctrl Pts',(6.30559512916798,3.65572482665186,-3.57798407767736));
#115989=CARTESIAN_POINT('Ctrl Pts',(6.66688358641299,3.5211470952643,-2.84884354685972));
#115990=CARTESIAN_POINT('Ctrl Pts',(6.66146899570655,3.52341350513212,-2.86138382592987));
#115991=CARTESIAN_POINT('Ctrl Pts',(6.656054405,3.525679915,-2.873924105));
#115992=CARTESIAN_POINT('Ctrl Pts',(6.499010858,3.591414347,-3.237639483));
#115993=CARTESIAN_POINT('Ctrl Pts',(6.303270783,3.656498153,-3.582077251));
#115994=CARTESIAN_POINT('Ctrl Pts',(6.79668254788956,3.52114709526431,-3.17234237973408));
#115995=CARTESIAN_POINT('Ctrl Pts',(6.79065755929905,3.52341350513212,-3.18512490534756));
#115996=CARTESIAN_POINT('Ctrl Pts',(6.78463257070837,3.525679915,-3.19790743096098));
#115997=CARTESIAN_POINT('Ctrl Pts',(6.60988518347408,3.591414347,-3.56864887214242));
#115998=CARTESIAN_POINT('Ctrl Pts',(6.39578110022067,3.656498153,-3.91814180101807));
#115999=CARTESIAN_POINT('Origin',(-0.183868084565093,3.4821645266703,0.0714761343232284));
#116000=CARTESIAN_POINT('Ctrl Pts',(6.928721193,3.656505752,-2.134320179));
#116001=CARTESIAN_POINT('Ctrl Pts',(6.812521145,3.590992329,-2.511544621));
#116002=CARTESIAN_POINT('Ctrl Pts',(6.656054405,3.525679915,-2.873924105));
#116003=CARTESIAN_POINT('Ctrl Pts',(7.236196612,3.656505752,-1.971663914));
#116004=CARTESIAN_POINT('Ctrl Pts',(7.128852155,3.590992329,-2.365628421));
#116005=CARTESIAN_POINT('Ctrl Pts',(6.979371271,3.525679915,-2.745610435));
#116006=CARTESIAN_POINT('',(6.92733463065445,3.65572482707099,-2.13881623882443));
#116007=CARTESIAN_POINT('Origin',(-0.189028709533438,3.62499997568123,0.0636906784467089));
#116008=CARTESIAN_POINT('Ctrl Pts',(7.1665058654886,3.61640598741355,-2.21160432106036));
#116009=CARTESIAN_POINT('Ctrl Pts',(7.1266181312516,3.62265476504783,-2.1994222532773));
#116010=CARTESIAN_POINT('Ctrl Pts',(7.08672423682204,3.62905099624073,-2.1872583156536));
#116011=CARTESIAN_POINT('Ctrl Pts',(7.00701313044391,3.64214708572923,-2.16299797339197));
#116012=CARTESIAN_POINT('Ctrl Pts',(6.96715263420202,3.64885405168379,-2.15088839165116));
#116013=CARTESIAN_POINT('Ctrl Pts',(6.92733463189405,3.65572482668139,-2.13881623722737));
#116014=CARTESIAN_POINT('Ctrl Pts',(7.12343270488168,3.52114709501716,-1.34905626701452));
#116015=CARTESIAN_POINT('Ctrl Pts',(7.12084049344087,3.52341350500855,-1.36246733900726));
#116016=CARTESIAN_POINT('Ctrl Pts',(7.118248282,3.525679915,-1.375878411));
#116017=CARTESIAN_POINT('Ctrl Pts',(7.04306438,3.591414347,-1.764850046));
#116018=CARTESIAN_POINT('Ctrl Pts',(6.925944539,3.656498153,-2.14331338));
#116019=CARTESIAN_POINT('Ctrl Pts',(7.3197397245431,3.52114709501716,-1.63708893683821));
#116020=CARTESIAN_POINT('Ctrl Pts',(7.31660346185319,3.52341350500854,-1.65086780930878));
#116021=CARTESIAN_POINT('Ctrl Pts',(7.31346719916323,3.525679915,-1.66464668177927));
#116022=CARTESIAN_POINT('Ctrl Pts',(7.22250376037485,3.591414347,-2.06428591689887));
#116023=CARTESIAN_POINT('Ctrl Pts',(7.08853595975396,3.656498153,-2.45163394443485));
#116024=CARTESIAN_POINT('Origin',(-0.194934900058013,3.48216454405651,0.0302789327722805));
#116025=CARTESIAN_POINT('Ctrl Pts',(7.225547291,3.656505752,-0.594950714));
#116026=CARTESIAN_POINT('Ctrl Pts',(7.193156039,3.590992329,-0.988335434000001));
#116027=CARTESIAN_POINT('Ctrl Pts',(7.118248282,3.525679915,-1.375878411));
#116028=CARTESIAN_POINT('Ctrl Pts',(7.490867816,3.656505752,-0.369999136));
#116029=CARTESIAN_POINT('Ctrl Pts',(7.470723736,3.590992329,-0.777828857000001));
#116030=CARTESIAN_POINT('Ctrl Pts',(7.406422533,3.525679915,-1.181061074));
#116031=CARTESIAN_POINT('',(7.22515966529974,3.65572482707165,-0.599639729012796));
#116032=CARTESIAN_POINT('Origin',(-0.198301150914787,3.62499996314961,0.0215660772445236));
#116033=CARTESIAN_POINT('Ctrl Pts',(7.47438649549291,3.61640598739533,-0.619311320060682));
#116034=CARTESIAN_POINT('Ctrl Pts',(7.43281252968464,3.62265476505147,-0.615988746101276));
#116035=CARTESIAN_POINT('Ctrl Pts',(7.39123644540361,3.62905099622712,-0.612685202723241));
#116036=CARTESIAN_POINT('Ctrl Pts',(7.30817373059722,3.64214707835014,-0.60612758932348));
#116037=CARTESIAN_POINT('Ctrl Pts',(7.26664192340405,3.64885404807934,-0.60286994943576));
#116038=CARTESIAN_POINT('Ctrl Pts',(7.22515966554175,3.65572482670755,-0.599639727228977));
#116039=CARTESIAN_POINT('Ctrl Pts',(7.24689802585418,3.52114709524965,0.213811382512832));
#116040=CARTESIAN_POINT('Ctrl Pts',(7.2472494029271,3.5234135051248,0.200156605756419));
#116041=CARTESIAN_POINT('Ctrl Pts',(7.24760078,3.525679915,0.186501829));
#116042=CARTESIAN_POINT('Ctrl Pts',(7.25779204,3.591414347,-0.209538183));
#116043=CARTESIAN_POINT('Ctrl Pts',(7.224768825,3.656498153,-0.604330558));
#116044=CARTESIAN_POINT('Ctrl Pts',(7.50053400671784,3.52114709524965,-0.0252870375102526));
#116045=CARTESIAN_POINT('Ctrl Pts',(7.50043311840226,3.5234135051248,-0.0394179706665876));
#116046=CARTESIAN_POINT('Ctrl Pts',(7.50033223008661,3.525679915,-0.0535489038229223));
#116047=CARTESIAN_POINT('Ctrl Pts',(7.49740608852792,3.591414347,-0.463399246793597));
#116048=CARTESIAN_POINT('Ctrl Pts',(7.44983875710106,3.656498153,-0.870490409396995));
#116049=CARTESIAN_POINT('Origin',(-0.196886367454507,3.48216458971207,-0.0123342117782992));
#116050=CARTESIAN_POINT('Ctrl Pts',(7.184514827,3.656505752,0.972237985));
#116051=CARTESIAN_POINT('Ctrl Pts',(7.23744695100001,3.590992329,0.58108722));
#116052=CARTESIAN_POINT('Ctrl Pts',(7.24760078,3.525679915,0.186501829));
#116053=CARTESIAN_POINT('Ctrl Pts',(7.395274366,3.656505752,1.24896639));
#116054=CARTESIAN_POINT('Ctrl Pts',(7.463272578,3.590992329,0.84634112));
#116055=CARTESIAN_POINT('Ctrl Pts',(7.487157709,3.525679915,0.43871339));
#116056=CARTESIAN_POINT('',(7.18514426360252,3.65572482705992,0.967575269034057));
#116057=CARTESIAN_POINT('Origin',(-0.198300997752782,3.62499997613515,-0.0215670094842793));
#116058=CARTESIAN_POINT('Ctrl Pts',(7.43277311966718,3.61640598738244,1.00193998978875));
#116059=CARTESIAN_POINT('Ctrl Pts',(7.39145687490788,3.62265476503386,0.996247710126081));
#116060=CARTESIAN_POINT('Ctrl Pts',(7.35014265232034,3.62905099618932,0.990536389400853));
#116061=CARTESIAN_POINT('Ctrl Pts',(7.26761217221783,3.64214708344315,0.979084656609767));
#116062=CARTESIAN_POINT('Ctrl Pts',(7.22635107668164,3.64885405053422,0.973338026201712));
#116063=CARTESIAN_POINT('Ctrl Pts',(7.18514426386498,3.65572482661952,0.967575270475477));
#116064=CARTESIAN_POINT('Ctrl Pts',(7.03615984138259,3.52436392548355,1.74786086090946));
#116065=CARTESIAN_POINT('Ctrl Pts',(7.0371116811913,3.52502192024177,1.74401115545473));
#116066=CARTESIAN_POINT('Ctrl Pts',(7.038063521,3.525679915,1.74016145));
#116067=CARTESIAN_POINT('Ctrl Pts',(7.133153411,3.591414347,1.355571454));
#116068=CARTESIAN_POINT('Ctrl Pts',(7.185770951,3.656498153,0.962910089));
#116069=CARTESIAN_POINT('Ctrl Pts',(7.33416912307217,3.52436392548355,1.56844846720524));
#116070=CARTESIAN_POINT('Ctrl Pts',(7.33502264903608,3.52502192024177,1.56443586310262));
#116071=CARTESIAN_POINT('Ctrl Pts',(7.335876175,3.525679915,1.560423259));
#116072=CARTESIAN_POINT('Ctrl Pts',(7.421144399,3.591414347,1.159559501));
#116073=CARTESIAN_POINT('Ctrl Pts',(7.462225511,3.656498153,0.751791473));
#116074=CARTESIAN_POINT('Origin',(-0.189631658845381,3.48216453482775,-0.0543705811770401));
#116075=CARTESIAN_POINT('Ctrl Pts',(6.807542435,3.656505752,2.493965916));
#116076=CARTESIAN_POINT('Ctrl Pts',(6.943322888,3.590992329,2.12333888));
#116077=CARTESIAN_POINT('Ctrl Pts',(7.038063521,3.525679915,1.74016145));
#116078=CARTESIAN_POINT('Ctrl Pts',(6.953886107,3.656505752,2.809531636));
#116079=CARTESIAN_POINT('Ctrl Pts',(7.10684709,3.590992329,2.430937126));
#116080=CARTESIAN_POINT('Ctrl Pts',(7.217801712,3.525679915,2.037974103));
#116081=CARTESIAN_POINT('',(6.80915950247847,3.65572482704387,2.48954752166462));
#116082=CARTESIAN_POINT('Origin',(-0.189028489598825,3.62499993456761,-0.0636916109347949));
#116083=CARTESIAN_POINT('Ctrl Pts',(7.04361153430038,3.61640598744965,2.57634169922523));
#116084=CARTESIAN_POINT('Ctrl Pts',(7.00448491229197,3.62265476508227,2.56190073060411));
#116085=CARTESIAN_POINT('Ctrl Pts',(6.96536435829456,3.62905099623963,2.5474416007531));
#116086=CARTESIAN_POINT('Ctrl Pts',(6.88722514371671,3.6421470893655,2.51851597651896));
#116087=CARTESIAN_POINT('Ctrl Pts',(6.84816408409976,3.64885405342756,2.50403379027225));
#116088=CARTESIAN_POINT('Ctrl Pts',(6.8091595022488,3.65572482658445,2.48954752411671));
#116089=CARTESIAN_POINT('Ctrl Pts',(6.49591991560068,3.52436392548355,3.21956322413365));
#116090=CARTESIAN_POINT('Ctrl Pts',(6.49767707480033,3.52502192024177,3.21600814006683));
#116091=CARTESIAN_POINT('Ctrl Pts',(6.499434234,3.525679915,3.212453056));
#116092=CARTESIAN_POINT('Ctrl Pts',(6.674976456,3.591414347,2.857296075));
#116093=CARTESIAN_POINT('Ctrl Pts',(6.810774414,3.656498153,2.485126131));
#116094=CARTESIAN_POINT('Ctrl Pts',(6.82553026747355,3.52436392548355,3.10840857858364));
#116095=CARTESIAN_POINT('Ctrl Pts',(6.82722642973678,3.52502192024177,3.10467326979182));
#116096=CARTESIAN_POINT('Ctrl Pts',(6.828922592,3.525679915,3.100937961));
#116097=CARTESIAN_POINT('Ctrl Pts',(6.99837115,3.591414347,2.727776323));
#116098=CARTESIAN_POINT('Ctrl Pts',(7.126149882,3.656498153,2.33837291));
#116099=CARTESIAN_POINT('Origin',(-0.173510263844352,3.48216456917264,-0.0938646918006852));
#116100=CARTESIAN_POINT('Ctrl Pts',(6.112256925,3.656505752,3.899078773));
#116101=CARTESIAN_POINT('Ctrl Pts',(6.324536764,3.590992329,3.566305575));
#116102=CARTESIAN_POINT('Ctrl Pts',(6.499434234,3.525679915,3.212453056));
#116103=CARTESIAN_POINT('Ctrl Pts',(6.187341861,3.656505752,4.238726305));
#116104=CARTESIAN_POINT('Ctrl Pts',(6.41811333,3.590992329,3.901865214));
#116105=CARTESIAN_POINT('Ctrl Pts',(6.610949329,3.525679915,3.541941413));
#116106=CARTESIAN_POINT('',(6.11478601009459,3.65572482707945,3.89511130062054));
#116107=CARTESIAN_POINT('Origin',(-0.170917169114783,3.62499992226006,-0.102838001281196));
#116108=CARTESIAN_POINT('Ctrl Pts',(6.32509850137208,3.6164059874298,4.03027653421334));
#116109=CARTESIAN_POINT('Ctrl Pts',(6.28999101930424,3.62265476509319,4.00776212019126));
#116110=CARTESIAN_POINT('Ctrl Pts',(6.25489336773236,3.62905099624141,3.98523127410475));
#116111=CARTESIAN_POINT('Ctrl Pts',(6.18479924655914,3.64214707297698,3.94018434989972));
#116112=CARTESIAN_POINT('Ctrl Pts',(6.14976460795097,3.64885404539754,3.91764374585424));
#116113=CARTESIAN_POINT('Ctrl Pts',(6.11478600941526,3.6557248266398,3.89511130181848));
#116114=CARTESIAN_POINT('Ctrl Pts',(5.65193799443724,3.52436392548355,4.54072238877234));
#116115=CARTESIAN_POINT('Ctrl Pts',(5.65441831021862,3.52502192024177,4.53762815788617));
#116116=CARTESIAN_POINT('Ctrl Pts',(5.656898626,3.525679915,4.534533927));
#116117=CARTESIAN_POINT('Ctrl Pts',(5.904685021,3.591414347,4.225416708));
#116118=CARTESIAN_POINT('Ctrl Pts',(6.117313634,3.656498153,3.891140437));
#116119=CARTESIAN_POINT('Ctrl Pts',(5.9977372021746,3.52436392548355,4.5030229591959));
#116120=CARTESIAN_POINT('Ctrl Pts',(6.00019669008729,3.52502192024177,4.49973960459795));
#116121=CARTESIAN_POINT('Ctrl Pts',(6.002656178,3.525679915,4.49645625));
#116122=CARTESIAN_POINT('Ctrl Pts',(6.248361845,3.591414347,4.168445355));
#116123=CARTESIAN_POINT('Ctrl Pts',(6.45686340400001,3.656498153,3.815614628));
#116124=CARTESIAN_POINT('Origin',(-0.149275386552372,3.48216457406842,-0.128969635675024));
#116125=CARTESIAN_POINT('Ctrl Pts',(5.131169075,3.656505752,5.12187504));
#116126=CARTESIAN_POINT('Ctrl Pts',(5.410022329,3.590992329,4.842515785));
#116127=CARTESIAN_POINT('Ctrl Pts',(5.656898626,3.525679915,4.534533927));
#116128=CARTESIAN_POINT('Ctrl Pts',(5.131484387,3.656505752,5.469722844));
#116129=CARTESIAN_POINT('Ctrl Pts',(5.429275724,3.590992329,5.19034642200001));
#116130=CARTESIAN_POINT('Ctrl Pts',(5.694976303,3.525679915,4.880291478));
#116131=CARTESIAN_POINT('',(5.1344919203829,3.65572482709323,5.11854400289229));
#116132=CARTESIAN_POINT('Origin',(-0.144814243661942,3.62499997372534,-0.137175988992));
#116133=CARTESIAN_POINT('Ctrl Pts',(5.31083089269157,3.61640598739114,5.29576011741492));
#116134=CARTESIAN_POINT('Ctrl Pts',(5.28138452430637,3.62265468298331,5.26622539498499));
#116135=CARTESIAN_POINT('Ctrl Pts',(5.25195069654516,3.62905095586431,5.23667614406137));
#116136=CARTESIAN_POINT('Ctrl Pts',(5.19317884859688,3.64214708734628,5.1776139811862));
#116137=CARTESIAN_POINT('Ctrl Pts',(5.16380889825466,3.64885405250065,5.14806898668562));
#116138=CARTESIAN_POINT('Ctrl Pts',(5.13449191955353,3.65572482670683,5.11854400434703));
#116139=CARTESIAN_POINT('Ctrl Pts',(4.52858346663779,3.52114709512928,5.66172924920744));
#116140=CARTESIAN_POINT('Ctrl Pts',(4.53921809631889,3.52341350506461,5.65315714010372));
#116141=CARTESIAN_POINT('Ctrl Pts',(4.549852726,3.525679915,5.644585031));
#116142=CARTESIAN_POINT('Ctrl Pts',(4.858297077,3.591414347,5.395961552));
#116143=CARTESIAN_POINT('Ctrl Pts',(5.137814068,3.656498153,5.115209341));
#116144=CARTESIAN_POINT('Ctrl Pts',(4.87501566544565,3.52114709512928,5.70025193256472));
#116145=CARTESIAN_POINT('Ctrl Pts',(4.88572041302767,3.52341350506461,5.69102686673961));
#116146=CARTESIAN_POINT('Ctrl Pts',(4.89642516060955,3.525679915,5.68180180091448));
#116147=CARTESIAN_POINT('Ctrl Pts',(5.20690319506136,3.591414347,5.41424011548773));
#116148=CARTESIAN_POINT('Ctrl Pts',(5.48637819367963,3.656498153,5.11444086518291));
#116149=CARTESIAN_POINT('Origin',(-0.118060676874366,3.4821645603223,-0.158044115061321));
#116150=CARTESIAN_POINT('Ctrl Pts',(3.910153461,3.656505752,6.105178123));
#116151=CARTESIAN_POINT('Ctrl Pts',(4.242541264,3.590992329,5.89229533900001));
#116152=CARTESIAN_POINT('Ctrl Pts',(4.549852726,3.525679915,5.644585031));
#116153=CARTESIAN_POINT('Ctrl Pts',(3.835684406,3.656505752,6.44496122100001));
#116154=CARTESIAN_POINT('Ctrl Pts',(4.18657122,3.590992329,6.236132799));
#116155=CARTESIAN_POINT('Ctrl Pts',(4.512712514,3.525679915,5.990444538));
#116156=CARTESIAN_POINT('',(3.91411469504543,3.65572482704546,6.1026392772109));
#116157=CARTESIAN_POINT('Origin',(-0.111939653749157,3.6249999645308,-0.165099488252253));
#116158=CARTESIAN_POINT('Ctrl Pts',(4.04823473411853,3.61640598738466,6.31361984386591));
#116159=CARTESIAN_POINT('Ctrl Pts',(4.02582560354184,3.62265476502366,6.27844506607371));
#116160=CARTESIAN_POINT('Ctrl Pts',(4.00343229437542,3.62905099618508,6.24325950250079));
#116161=CARTESIAN_POINT('Ctrl Pts',(3.95873127978742,3.64214708044663,6.17294422349425));
#116162=CARTESIAN_POINT('Ctrl Pts',(3.93639927058861,3.64885404904875,6.13777628396584));
#116163=CARTESIAN_POINT('Ctrl Pts',(3.91411469397674,3.65572482660295,6.10263927839537));
#116164=CARTESIAN_POINT('Ctrl Pts',(3.20560327165695,3.52114709508196,6.50287274703964));
#116165=CARTESIAN_POINT('Ctrl Pts',(3.21783201982848,3.52341350504095,6.49678718001982));
#116166=CARTESIAN_POINT('Ctrl Pts',(3.230060768,3.525679915,6.490701613));
#116167=CARTESIAN_POINT('Ctrl Pts',(3.584740561,3.591414347,6.31419723));
#116168=CARTESIAN_POINT('Ctrl Pts',(3.918076027,3.656498153,6.100096741));
#116169=CARTESIAN_POINT('Ctrl Pts',(3.53565483972605,3.52114709508197,6.6149674737033));
#116170=CARTESIAN_POINT('Ctrl Pts',(3.54809243290119,3.52341350504095,6.60825928905035));
#116171=CARTESIAN_POINT('Ctrl Pts',(3.56053002607633,3.525679915,6.60155110439752));
#116172=CARTESIAN_POINT('Ctrl Pts',(3.92126711141813,3.591414347,6.40698846309505));
#116173=CARTESIAN_POINT('Ctrl Pts',(4.25865611687768,3.656498153,6.17427721525413));
#116174=CARTESIAN_POINT('Origin',(-0.0813257725780459,3.48216458113227,
-0.179728872209758));
#116175=CARTESIAN_POINT('Ctrl Pts',(2.506303418,3.656505752,6.803009862));
#116176=CARTESIAN_POINT('Ctrl Pts',(2.876683684,3.590992329,6.666557711));
#116177=CARTESIAN_POINT('Ctrl Pts',(3.230060768,3.525679915,6.490701613));
#116178=CARTESIAN_POINT('Ctrl Pts',(2.360532086,3.656505752,7.118840374));
#116179=CARTESIAN_POINT('Ctrl Pts',(2.748107298,3.590992329,6.99032453800001));
#116180=CARTESIAN_POINT('Ctrl Pts',(3.119439304,3.525679915,6.82049107000001));
#116181=CARTESIAN_POINT('',(2.51071781714977,3.65572482706423,6.8013819211087));
#116182=CARTESIAN_POINT('Origin',(-0.0738311105697187,3.62499995453911,
-0.185303373843084));
#116183=CARTESIAN_POINT('Ctrl Pts',(2.59634761838851,3.61640598745063,7.03626172327406));
#116184=CARTESIAN_POINT('Ctrl Pts',(2.58202393835233,3.6226547650867,6.99709201155439));
#116185=CARTESIAN_POINT('Ctrl Pts',(2.56771802844582,3.62905099626518,6.95791516722619));
#116186=CARTESIAN_POINT('Ctrl Pts',(2.53917783475695,3.64214706707844,6.87963450385756));
#116187=CARTESIAN_POINT('Ctrl Pts',(2.52492798746055,3.64885404252505,6.84048800649528));
#116188=CARTESIAN_POINT('Ctrl Pts',(2.51071781591352,3.65572482669336,6.80138192161454));
#116189=CARTESIAN_POINT('Ctrl Pts',(1.73273263100486,3.52114709502825,7.03994914305568));
#116190=CARTESIAN_POINT('Ctrl Pts',(1.74598369500246,3.5234135050141,7.03663467252785));
#116191=CARTESIAN_POINT('Ctrl Pts',(1.759234759,3.525679915,7.033320202));
#116192=CARTESIAN_POINT('Ctrl Pts',(2.14356556,3.591414347,6.937188064));
#116193=CARTESIAN_POINT('Ctrl Pts',(2.515133105,3.656498153,6.79975039700001));
#116194=CARTESIAN_POINT('Ctrl Pts',(2.03097072435524,3.52114709502825,7.22037448802775));
#116195=CARTESIAN_POINT('Ctrl Pts',(2.04455959505472,3.5234135050141,7.21649685182525));
#116196=CARTESIAN_POINT('Ctrl Pts',(2.05814846575428,3.525679915,7.21261921562272));
#116197=CARTESIAN_POINT('Ctrl Pts',(2.45227693435169,3.591414347,7.1001531504088));
#116198=CARTESIAN_POINT('Ctrl Pts',(2.83180401175584,3.656498153,6.94541122514516));
#116199=CARTESIAN_POINT('Origin',(-0.0407880620217441,3.48216455172988,
-0.193009651875642));
#116200=CARTESIAN_POINT('Ctrl Pts',(0.985261412,3.656505752,7.182740421));
#116201=CARTESIAN_POINT('Ctrl Pts',(1.376315572,3.590992329,7.129099254));
#116202=CARTESIAN_POINT('Ctrl Pts',(1.759234759,3.525679915,7.033320202));
#116203=CARTESIAN_POINT('Ctrl Pts',(0.775003908,3.656505752,7.459850464));
#116204=CARTESIAN_POINT('Ctrl Pts',(1.181144933,3.590992329,7.41765647));
#116205=CARTESIAN_POINT('Ctrl Pts',(1.580304579,3.525679915,7.331619019));
#116206=CARTESIAN_POINT('',(0.989922564157426,3.65572482707808,7.18209950545577));
#116207=CARTESIAN_POINT('Origin',(-0.032270264785814,3.62499995560225,-0.196842784054748));
#116208=CARTESIAN_POINT('Ctrl Pts',(1.02305817352954,3.61640598741002,7.42989582473919));
#116209=CARTESIAN_POINT('Ctrl Pts',(1.01748970331473,3.62265476506886,7.3885627112426));
#116210=CARTESIAN_POINT('Ctrl Pts',(1.01194012110595,3.62905099625209,7.34722645205932));
#116211=CARTESIAN_POINT('Ctrl Pts',(1.00089520291465,3.64214707546473,7.26464059626709));
#116212=CARTESIAN_POINT('Ctrl Pts',(0.995393852702379,3.64885404668247,
7.22334605429106));
#116213=CARTESIAN_POINT('Ctrl Pts',(0.989922562679225,3.65572482674932,
7.18209950578354));
#116214=CARTESIAN_POINT('Ctrl Pts',(0.178841338619978,3.52114709502879,
7.24784534093733));
#116215=CARTESIAN_POINT('Ctrl Pts',(0.192495113309986,3.52341350501437,
7.24745694796873));
#116216=CARTESIAN_POINT('Ctrl Pts',(0.206148888,3.525679915,7.247068555));
#116217=CARTESIAN_POINT('Ctrl Pts',(0.602159817,3.591414347,7.235803695));
#116218=CARTESIAN_POINT('Ctrl Pts',(0.994585354,3.656498153,7.181455282));
#116219=CARTESIAN_POINT('Ctrl Pts',(0.431320675651514,3.52114709502879,
7.4881648150128));
#116220=CARTESIAN_POINT('Ctrl Pts',(0.445425423261039,3.52341350501437,
7.48729904133021));
#116221=CARTESIAN_POINT('Ctrl Pts',(0.459530170870565,3.525679915,7.48643326764763));
#116222=CARTESIAN_POINT('Ctrl Pts',(0.868621014316521,3.591414347,7.46132256763059));
#116223=CARTESIAN_POINT('Ctrl Pts',(1.27253989906597,3.656498153,7.39178552538709));
#116224=CARTESIAN_POINT('Origin',(0.00165692198660666,3.48216459974148,
-0.197265124310521));
#116225=CARTESIAN_POINT('Ctrl Pts',(-0.581850323,3.656505752,7.226614021));
#116226=CARTESIAN_POINT('Ctrl Pts',(-0.188407526,3.590992329,7.25829204));
#116227=CARTESIAN_POINT('Ctrl Pts',(0.206148888,3.525679915,7.247068555));
#116228=CARTESIAN_POINT('Ctrl Pts',(-0.846762591,3.656505752,7.452046237));
#116229=CARTESIAN_POINT('Ctrl Pts',(-0.441046456,3.590992329,7.49814703));
#116230=CARTESIAN_POINT('Ctrl Pts',(-0.032723432,3.525679915,7.499928611));
#116231=CARTESIAN_POINT('Origin',(0.0107995551809671,3.62499992801169,-0.199177769006146));
#116232=CARTESIAN_POINT('Ctrl Pts',(0.206121509127986,2.23138000478158,
7.24707355226295));
#116233=CARTESIAN_POINT('Ctrl Pts',(0.210029728063993,2.23202203989079,
7.24695817563148));
#116234=CARTESIAN_POINT('Ctrl Pts',(0.213937947,2.232664075,7.24684279900001));
#116235=CARTESIAN_POINT('Ctrl Pts',(0.606333568,2.297126115,7.23525867700001));
#116236=CARTESIAN_POINT('Ctrl Pts',(0.995184151,2.362252267,7.181372327));
#116237=CARTESIAN_POINT('Ctrl Pts',(0.458980806959231,2.23138000478158,
7.48594697166454));
#116238=CARTESIAN_POINT('Ctrl Pts',(0.463017702979616,2.23202203989079,
7.48569508933227));
#116239=CARTESIAN_POINT('Ctrl Pts',(0.467054599,2.232664075,7.48544320700001));
#116240=CARTESIAN_POINT('Ctrl Pts',(0.872369743,2.297126115,7.460153548));
#116241=CARTESIAN_POINT('Ctrl Pts',(1.272584422,2.362252267,7.391246775));
#116242=CARTESIAN_POINT('',(0.467054605055031,2.23266407419427,7.48544320450419));
#116243=CARTESIAN_POINT('',(1.02641184425845,2.32233405367783,7.42943327080472));
#116244=CARTESIAN_POINT('Origin',(-0.0399076795548507,2.41067415053388,
-0.185339256409806));
#116245=CARTESIAN_POINT('Ctrl Pts',(0.990540536095505,2.36147458198366,
7.18201430225601));
#116246=CARTESIAN_POINT('Ctrl Pts',(0.996473310122438,2.35461430679531,
7.22319414246324));
#116247=CARTESIAN_POINT('Ctrl Pts',(1.00243339649902,2.34792815753381,7.26442562949533));
#116248=CARTESIAN_POINT('Ctrl Pts',(1.01438950164634,2.33489257429051,7.34688486757673));
#116249=CARTESIAN_POINT('Ctrl Pts',(1.02039254146659,2.32853549393583,7.38816102848141));
#116250=CARTESIAN_POINT('Ctrl Pts',(1.02641184256769,2.32233405371974,7.42943327094841));
#116251=CARTESIAN_POINT('',(0.340496287632723,2.23266407264717,7.36614300232361));
#116252=CARTESIAN_POINT('Origin',(-9.86623976961809E-15,2.32340998499933,
-2.43728648374741E-13));
#116253=CARTESIAN_POINT('',(1.02848533178705,2.14301213123783,7.42914651337806));
#116254=CARTESIAN_POINT('Origin',(-0.0453595884940869,2.01794103942791,
-0.181798662226462));
#116255=CARTESIAN_POINT('',(1.58818371752705,2.23266407449123,7.3299162650956));
#116256=CARTESIAN_POINT('Origin',(-0.0659827140321631,2.41052396785092,
-0.170978110656799));
#116257=CARTESIAN_POINT('Ctrl Pts',(1.02641184540738,2.3223340532383,7.42943327079627));
#116258=CARTESIAN_POINT('Ctrl Pts',(1.1035495486996,2.31006874162245,7.41877632682905));
#116259=CARTESIAN_POINT('Ctrl Pts',(1.18040467460891,2.29785936479557,7.40693385917979));
#116260=CARTESIAN_POINT('Ctrl Pts',(1.25692390206011,2.28571428601282,7.39392604080063));
#116261=CARTESIAN_POINT('Ctrl Pts',(1.36754346318794,2.26815682559423,7.37512136685907));
#116262=CARTESIAN_POINT('Ctrl Pts',(1.47802088647235,2.25046493734972,7.35378540900434));
#116263=CARTESIAN_POINT('Ctrl Pts',(1.58818372237067,2.23266407446841,7.32991626615202));
#116264=CARTESIAN_POINT('Ctrl Pts',(0.985822492000001,2.36225522,7.182663435));
#116265=CARTESIAN_POINT('Ctrl Pts',(1.218577958,2.323743665,7.15071768400001));
#116266=CARTESIAN_POINT('Ctrl Pts',(1.448776863,2.285714286,7.103769816));
#116267=CARTESIAN_POINT('Ctrl Pts',(1.608598834,2.259311335,7.071174957));
#116268=CARTESIAN_POINT('Ctrl Pts',(1.766793184,2.232664075,7.031425307));
#116269=CARTESIAN_POINT('Ctrl Pts',(1.77065896195487,2.23201289883432,7.03045394916905));
#116270=CARTESIAN_POINT('Ctrl Pts',(1.77452473990974,2.23136172266864,7.02948259133811));
#116271=CARTESIAN_POINT('Ctrl Pts',(0.775586635,2.36225522,7.459789901));
#116272=CARTESIAN_POINT('Ctrl Pts',(1.017322434,2.323743665,7.43465688100001));
#116273=CARTESIAN_POINT('Ctrl Pts',(1.256923902,2.285714286,7.393926041));
#116274=CARTESIAN_POINT('Ctrl Pts',(1.423273863,2.259311335,7.365647527));
#116275=CARTESIAN_POINT('Ctrl Pts',(1.588183719,2.232664075,7.329916267));
#116276=CARTESIAN_POINT('Ctrl Pts',(1.59221360303736,2.23201289883432,7.3290431061241));
#116277=CARTESIAN_POINT('Ctrl Pts',(1.59624348707472,2.23136172266864,7.32816994524821));
#116278=CARTESIAN_POINT('',(1.6774884429112,2.23266407357604,7.18067078900645));
#116279=CARTESIAN_POINT('Ctrl Pts',(1.7592090952449,2.23138000478158,7.03333096846917));
#116280=CARTESIAN_POINT('Ctrl Pts',(1.76300113962245,2.23202203989079,7.03237813773459));
#116281=CARTESIAN_POINT('Ctrl Pts',(1.766793184,2.232664075,7.031425307));
#116282=CARTESIAN_POINT('Ctrl Pts',(2.147524569,2.297126115,6.935758556));
#116283=CARTESIAN_POINT('Ctrl Pts',(2.51570007,2.362252267,6.799540658));
#116284=CARTESIAN_POINT('Ctrl Pts',(2.05750740624301,2.23138000478158,7.21226238556066));
#116285=CARTESIAN_POINT('Ctrl Pts',(2.06139577462151,2.23202203989079,7.21114857878033));
#116286=CARTESIAN_POINT('Ctrl Pts',(2.065284143,2.232664075,7.210034772));
#116287=CARTESIAN_POINT('Ctrl Pts',(2.455686715,2.297126115,7.098205596));
#116288=CARTESIAN_POINT('Ctrl Pts',(2.831731678,2.362252267,6.944875499));
#116289=CARTESIAN_POINT('',(2.06528414837267,2.23266407419428,7.21003476826059));
#116290=CARTESIAN_POINT('',(2.59952344630951,2.32233405371967,7.03508904333622));
#116291=CARTESIAN_POINT('Origin',(-0.0788171249275074,2.41067414467123,
-0.172427152005246));
#116292=CARTESIAN_POINT('Ctrl Pts',(2.51130302491251,2.36147458180911,6.8011658645237));
#116293=CARTESIAN_POINT('Ctrl Pts',(2.52594953276537,2.3546143112292,6.84010754589003));
#116294=CARTESIAN_POINT('Ctrl Pts',(2.54063381526986,2.34792816677927,6.8790937912037));
#116295=CARTESIAN_POINT('Ctrl Pts',(2.57003670947,2.33489257586038,6.95705501495986));
#116296=CARTESIAN_POINT('Ctrl Pts',(2.58477255187177,2.32853549717823,6.99607567507759));
#116297=CARTESIAN_POINT('Ctrl Pts',(2.59952344478407,2.32233405377372,7.03508904374644));
#116298=CARTESIAN_POINT('',(1.91603867764522,2.23266407264717,7.12073003569382));
#116299=CARTESIAN_POINT('Origin',(2.3115190317391E-13,2.32340998499989,
6.26668855696622E-13));
#116300=CARTESIAN_POINT('',(2.60148681280772,2.14301213126887,7.0343632519323));
#116301=CARTESIAN_POINT('Origin',(-0.0833804322487564,2.01794103357697,
-0.167797302228523));
#116302=CARTESIAN_POINT('',(3.12676819112557,2.23266407449122,6.8171343424829));
#116303=CARTESIAN_POINT('Origin',(-0.101195453099118,2.41052401725478,-0.152796690784625));
#116304=CARTESIAN_POINT('Ctrl Pts',(2.59952344744715,2.32233405329015,7.03508904319684));
#116305=CARTESIAN_POINT('Ctrl Pts',(2.67256678623818,2.31006874164898,7.00809892682557));
#116306=CARTESIAN_POINT('Ctrl Pts',(2.74507930171928,2.29785936480543,6.980011749429));
#116307=CARTESIAN_POINT('Ctrl Pts',(2.81701325564113,2.28571428610092,6.95085867462188));
#116308=CARTESIAN_POINT('Ctrl Pts',(2.92100414282236,2.26815682581014,6.90871370711777));
#116309=CARTESIAN_POINT('Ctrl Pts',(3.02431206591993,2.25046493734972,6.86412719177494));
#116310=CARTESIAN_POINT('Ctrl Pts',(3.12676819610958,2.23266407446841,6.81713434244728));
#116311=CARTESIAN_POINT('Ctrl Pts',(2.50683483,2.36225522,6.80281406));
#116312=CARTESIAN_POINT('Ctrl Pts',(2.727281211,2.323743665,6.721579638));
#116313=CARTESIAN_POINT('Ctrl Pts',(2.94200579,2.285714286,6.626243425));
#116314=CARTESIAN_POINT('Ctrl Pts',(3.09108428,2.259311335,6.560053617));
#116315=CARTESIAN_POINT('Ctrl Pts',(3.237035134,2.232664075,6.487226182));
#116316=CARTESIAN_POINT('Ctrl Pts',(3.24060171898795,2.23201289883432,6.48544650597028));
#116317=CARTESIAN_POINT('Ctrl Pts',(3.24416830397589,2.23136172266864,6.48366682994055));
#116318=CARTESIAN_POINT('Ctrl Pts',(2.36108817,2.36225522,7.118655958));
#116319=CARTESIAN_POINT('Ctrl Pts',(2.591769463,2.323743665,7.042144483));
#116320=CARTESIAN_POINT('Ctrl Pts',(2.817013256,2.285714286,6.950858675));
#116321=CARTESIAN_POINT('Ctrl Pts',(2.973395002,2.259311335,6.887480972));
#116322=CARTESIAN_POINT('Ctrl Pts',(3.126768193,2.232664075,6.817134344));
#116323=CARTESIAN_POINT('Ctrl Pts',(3.13051615682195,2.23201289883432,6.81541529117844));
#116324=CARTESIAN_POINT('Ctrl Pts',(3.13426412064389,2.23136172266864,6.81369623835689));
#116325=CARTESIAN_POINT('',(3.18190165554338,2.23266407357605,6.65218026680585));
#116326=CARTESIAN_POINT('Ctrl Pts',(3.2300380178948,2.23138000478159,6.49071764506209));
#116327=CARTESIAN_POINT('Ctrl Pts',(3.2335365759474,2.23202203989079,6.48897191353105));
#116328=CARTESIAN_POINT('Ctrl Pts',(3.237035134,2.232664075,6.48722618199999));
#116329=CARTESIAN_POINT('Ctrl Pts',(3.588299708,2.297126115,6.31195007300001));
#116330=CARTESIAN_POINT('Ctrl Pts',(3.918584648,2.362252267,6.099770025));
#116331=CARTESIAN_POINT('Ctrl Pts',(3.55982724710697,2.23138000478159,6.60134042570219));
#116332=CARTESIAN_POINT('Ctrl Pts',(3.56338527205348,2.23202203989079,6.5994167748511));
#116333=CARTESIAN_POINT('Ctrl Pts',(3.566943297,2.232664075,6.597493124));
#116334=CARTESIAN_POINT('Ctrl Pts',(3.924178506,2.297126115,6.40435344));
#116335=CARTESIAN_POINT('Ctrl Pts',(4.258470309,2.362252267,6.173769564));
#116336=CARTESIAN_POINT('',(3.5669433014604,2.23266407419313,6.59749311918321));
#116337=CARTESIAN_POINT('',(4.0510842215557,2.32233405368084,6.31179187167886));
#116338=CARTESIAN_POINT('Origin',(-0.114041131822303,2.41067409909671,-0.151452518478992));
#116339=CARTESIAN_POINT('Ctrl Pts',(3.91463977526644,2.36147458191302,6.10230246946548));
#116340=CARTESIAN_POINT('Ctrl Pts',(3.93731515696421,2.35461431419793,6.13718513497579));
#116341=CARTESIAN_POINT('Ctrl Pts',(3.96003700857577,2.3479281727242,6.17210320002542));
#116342=CARTESIAN_POINT('Ctrl Pts',(4.00551186472225,2.33489257415327,6.24192102140471));
#116343=CARTESIAN_POINT('Ctrl Pts',(4.02829148668957,2.32853549366127,6.27686164025753));
#116344=CARTESIAN_POINT('Ctrl Pts',(4.05108422007071,2.32233405372159,6.31179187253635));
#116345=CARTESIAN_POINT('',(3.40198922851562,2.23266407264367,6.54235964623195));
#116346=CARTESIAN_POINT('Origin',(-3.07046055247895E-13,2.32340998499933,
-6.88251539093798E-13));
#116347=CARTESIAN_POINT('',(4.05284566193626,2.14301213127652,6.31066098286521));
#116348=CARTESIAN_POINT('Origin',(-0.117502649176756,2.01794102805717,-0.145950205159407));
#116349=CARTESIAN_POINT('',(4.51914845885334,2.23266407449122,5.98559079590574));
#116350=CARTESIAN_POINT('Origin',(-0.131676465731563,2.41052406519318,-0.127470530570108));
#116351=CARTESIAN_POINT('Ctrl Pts',(4.05108422259417,2.32233405323947,6.3117918711683));
#116352=CARTESIAN_POINT('Ctrl Pts',(4.11661777123175,2.3100687416239,6.26973060984927));
#116353=CARTESIAN_POINT('Ctrl Pts',(4.18139707119067,2.29785936479657,6.2267120475812));
#116354=CARTESIAN_POINT('Ctrl Pts',(4.24538220001676,2.28571428600411,6.18277688176229));
#116355=CARTESIAN_POINT('Ctrl Pts',(4.33788191716383,2.26815682557287,6.11926227365498));
#116356=CARTESIAN_POINT('Ctrl Pts',(4.42918977469998,2.25046493734972,6.05351001663829));
#116357=CARTESIAN_POINT('Ctrl Pts',(4.51914846370308,2.23266407446841,5.98559079481506));
#116358=CARTESIAN_POINT('Ctrl Pts',(3.910630358,2.36225522,6.104872661));
#116359=CARTESIAN_POINT('Ctrl Pts',(4.108459826,2.323743665,5.978147999));
#116360=CARTESIAN_POINT('Ctrl Pts',(4.297669796,2.285714286,5.838881257));
#116361=CARTESIAN_POINT('Ctrl Pts',(4.429034062,2.259311335,5.74219146));
#116362=CARTESIAN_POINT('Ctrl Pts',(4.55591692,2.232664075,5.639691571));
#116363=CARTESIAN_POINT('Ctrl Pts',(4.55901754246412,2.23201289883432,5.6371867924711));
#116364=CARTESIAN_POINT('Ctrl Pts',(4.56211816492825,2.23136172266864,5.63468201394221));
#116365=CARTESIAN_POINT('Ctrl Pts',(3.836187846,2.36225522,6.444661575));
#116366=CARTESIAN_POINT('Ctrl Pts',(4.045028233,2.323743665,6.320349236));
#116367=CARTESIAN_POINT('Ctrl Pts',(4.2453822,2.285714286,6.182776882));
#116368=CARTESIAN_POINT('Ctrl Pts',(4.384483496,2.259311335,6.087263462));
#116369=CARTESIAN_POINT('Ctrl Pts',(4.519148461,2.232664075,5.985590797));
#116370=CARTESIAN_POINT('Ctrl Pts',(4.52243925395809,2.23201289883432,5.98310623325313));
#116371=CARTESIAN_POINT('Ctrl Pts',(4.52573004691619,2.23136172266864,5.98062166950626));
#116372=CARTESIAN_POINT('',(4.5375326835475,2.23266407357604,5.81264118942734));
#116373=CARTESIAN_POINT('Ctrl Pts',(4.54983395395533,2.23138000478158,5.64460557872374));
#116374=CARTESIAN_POINT('Ctrl Pts',(4.55287543697766,2.23202203989079,5.64214857486187));
#116375=CARTESIAN_POINT('Ctrl Pts',(4.55591692,2.232664075,5.639691571));
#116376=CARTESIAN_POINT('Ctrl Pts',(4.86128994,2.297126115,5.39300182));
#116377=CARTESIAN_POINT('Ctrl Pts',(5.138240564,2.362252267,5.114780924));
#116378=CARTESIAN_POINT('Ctrl Pts',(4.89569352152841,2.23138000478158,5.68174712431132));
#116379=CARTESIAN_POINT('Ctrl Pts',(4.89875483376421,2.23202203989079,5.67910357715566));
#116380=CARTESIAN_POINT('Ctrl Pts',(4.901816146,2.232664075,5.67646003));
#116381=CARTESIAN_POINT('Ctrl Pts',(5.209180072,2.297126115,5.411040834));
#116382=CARTESIAN_POINT('Ctrl Pts',(5.4860876,2.362252267,5.113985026));
#116383=CARTESIAN_POINT('',(4.90181614931828,2.23266407419428,5.67646002434556));
#116384=CARTESIAN_POINT('',(5.31322080074589,2.32233405367292,5.29336232676854));
#116385=CARTESIAN_POINT('Origin',(-0.143932727089013,2.41067416005679,-0.12339615861267));
#116386=CARTESIAN_POINT('Ctrl Pts',(5.13493232101444,2.36147458193287,5.1181021922724));
#116387=CARTESIAN_POINT('Ctrl Pts',(5.16457633450321,2.35461430775493,5.14729481144356));
#116388=CARTESIAN_POINT('Ctrl Pts',(5.19427334574813,2.34792815954324,5.1765120169118));
#116389=CARTESIAN_POINT('Ctrl Pts',(5.25369373417348,2.33489257381224,5.23492172925327));
#116390=CARTESIAN_POINT('Ctrl Pts',(5.28345198322634,2.32853549297563,5.26414851222337));
#116391=CARTESIAN_POINT('Ctrl Pts',(5.31322079946837,2.32233405371025,5.2933623279704));
#116392=CARTESIAN_POINT('',(4.72886654423971,2.23266407264716,5.65807579110616));
#116393=CARTESIAN_POINT('Origin',(-3.31765864780564E-13,2.32340998499933,
-3.35235311732518E-13));
#116394=CARTESIAN_POINT('',(5.31469795198158,2.14301213129531,5.29187922010486));
#116395=CARTESIAN_POINT('Origin',(-0.146130295056051,2.01794105968598,-0.117278192493951));
#116396=CARTESIAN_POINT('',(5.70021836766514,2.23266407449122,4.87416767540015));
#116397=CARTESIAN_POINT('Origin',(-0.156000037177539,2.41052396677109,-0.0961835375339043));
#116398=CARTESIAN_POINT('Ctrl Pts',(5.31322080163106,2.32233405322908,5.29336232599744));
#116399=CARTESIAN_POINT('Ctrl Pts',(5.36818028465233,2.31006874161876,5.23819665780963));
#116400=CARTESIAN_POINT('Ctrl Pts',(5.42219736154694,2.29785936479515,5.1822582110242));
#116401=CARTESIAN_POINT('Ctrl Pts',(5.47524179152955,2.28571428609777,5.12559531379656));
#116402=CARTESIAN_POINT('Ctrl Pts',(5.55192515209581,2.26815682580241,5.04368093717354));
#116403=CARTESIAN_POINT('Ctrl Pts',(5.62696349193861,2.25046493734972,4.95983744082139));
#116404=CARTESIAN_POINT('Ctrl Pts',(5.7002183721701,2.23266407446841,4.87416767328428));
#116405=CARTESIAN_POINT('Ctrl Pts',(5.131569157,2.36225522,5.121474201));
#116406=CARTESIAN_POINT('Ctrl Pts',(5.297531425,2.323743665,4.95518480299999));
#116407=CARTESIAN_POINT('Ctrl Pts',(5.452379538,2.285714286,4.77849949));
#116408=CARTESIAN_POINT('Ctrl Pts',(5.559887133,2.259311335,4.655830813));
#116409=CARTESIAN_POINT('Ctrl Pts',(5.661769094,2.232664075,4.52845125000001));
#116410=CARTESIAN_POINT('Ctrl Pts',(5.66425877229023,2.23201289883432,4.52533848961035));
#116411=CARTESIAN_POINT('Ctrl Pts',(5.66674845058047,2.23136172266864,4.5222257292207));
#116412=CARTESIAN_POINT('Ctrl Pts',(5.131911641,2.36225522,5.469321979));
#116413=CARTESIAN_POINT('Ctrl Pts',(5.30914597800001,2.323743665,5.303021483));
#116414=CARTESIAN_POINT('Ctrl Pts',(5.475241792,2.285714286,5.125595314));
#116415=CARTESIAN_POINT('Ctrl Pts',(5.59055841400001,2.259311335,5.002412278));
#116416=CARTESIAN_POINT('Ctrl Pts',(5.70021837,2.232664075,4.874167676));
#116417=CARTESIAN_POINT('Ctrl Pts',(5.70289811829972,2.23201289883432,4.87103377674732));
#116418=CARTESIAN_POINT('Ctrl Pts',(5.70557786659942,2.23136172266864,4.86789987749465));
#116419=CARTESIAN_POINT('',(5.68099372637676,2.23266407357604,4.70130946979503));
#116420=CARTESIAN_POINT('Ctrl Pts',(5.65688471072712,2.23138000478158,4.5345580288374));
#116421=CARTESIAN_POINT('Ctrl Pts',(5.65932690236356,2.23202203989079,4.5315046394187));
#116422=CARTESIAN_POINT('Ctrl Pts',(5.661769094,2.232664075,4.52845125));
#116423=CARTESIAN_POINT('Ctrl Pts',(5.906971658,2.297126115,4.221882796));
#116424=CARTESIAN_POINT('Ctrl Pts',(6.117638062,2.362252267,3.890630353));
#116425=CARTESIAN_POINT('Ctrl Pts',(6.00264260807393,2.23138000478158,4.49648164327883));
#116426=CARTESIAN_POINT('Ctrl Pts',(6.00506406403696,2.23202203989079,4.49324180913942));
#116427=CARTESIAN_POINT('Ctrl Pts',(6.00748552,2.232664075,4.490001975));
#116428=CARTESIAN_POINT('Ctrl Pts',(6.25060616700001,2.297126115,4.164713973));
#116429=CARTESIAN_POINT('Ctrl Pts',(6.457181533,2.362252267,3.815076231));
#116430=CARTESIAN_POINT('',(6.00748552200209,2.23266407419427,4.49000196877962));
#116431=CARTESIAN_POINT('',(6.32691708062088,2.32233405363403,4.0274210425946));
#116432=CARTESIAN_POINT('Origin',(-0.167094205500953,2.41067417005038,-0.0895699468138367));
#116433=CARTESIAN_POINT('Ctrl Pts',(6.11512113831182,2.36147458190962,3.89458514642993));
#116434=CARTESIAN_POINT('Ctrl Pts',(6.15034763234554,2.35461430951217,3.91672266572962));
#116435=CARTESIAN_POINT('Ctrl Pts',(6.18563116880774,2.34792816317999,3.9388728027073));
#116436=CARTESIAN_POINT('Ctrl Pts',(6.25621872661867,2.3348925730979,3.98314331589693));
#116437=CARTESIAN_POINT('Ctrl Pts',(6.29156414285186,2.32853549156021,4.00528965158357));
#116438=CARTESIAN_POINT('Ctrl Pts',(6.32691707962809,2.32233405366459,4.027421044131));
#116439=CARTESIAN_POINT('',(5.8346273159575,2.23266407264717,4.50922660090961));
#116440=CARTESIAN_POINT('Origin',(3.48679418671338E-13,2.32340998499922,
1.50270421106491E-13));
#116441=CARTESIAN_POINT('',(6.32804087298349,2.14301213123153,4.02565506642255));
#116442=CARTESIAN_POINT('Origin',(-0.167925446394461,2.01794106053296,-0.0831227669844309));
#116443=CARTESIAN_POINT('',(6.61475240058951,2.23266407449122,3.53483389192556));
#116444=CARTESIAN_POINT('Origin',(-0.173029777855993,2.41052396444191,-0.060399601320052));
#116445=CARTESIAN_POINT('Ctrl Pts',(6.32691708126275,2.32233405318557,4.02742104157157));
#116446=CARTESIAN_POINT('Ctrl Pts',(6.36873265401809,2.31006874159296,3.96173045210923));
#116447=CARTESIAN_POINT('Ctrl Pts',(6.40946172897266,2.29785936478348,3.89548774047974));
#116448=CARTESIAN_POINT('Ctrl Pts',(6.44908516184669,2.28571428602514,3.82874660589252));
#116449=CARTESIAN_POINT('Ctrl Pts',(6.5063665396354,2.26815682562442,3.73226268612071));
#116450=CARTESIAN_POINT('Ctrl Pts',(6.56162665075071,2.25046493734972,3.63424837905487));
#116451=CARTESIAN_POINT('Ctrl Pts',(6.61475240453563,2.23266407446841,3.53483388888147));
#116452=CARTESIAN_POINT('Ctrl Pts',(6.112561485,2.36225522,3.898601299));
#116453=CARTESIAN_POINT('Ctrl Pts',(6.23889634300001,2.323743665,3.700522674));
#116454=CARTESIAN_POINT('Ctrl Pts',(6.352142073,2.285714286,3.494680397));
#116455=CARTESIAN_POINT('Ctrl Pts',(6.43076606,2.259311335,3.351768692));
#116456=CARTESIAN_POINT('Ctrl Pts',(6.502883238,2.232664075,3.205465582));
#116457=CARTESIAN_POINT('Ctrl Pts',(6.50464555755743,2.23201289883432,3.20189038897088));
#116458=CARTESIAN_POINT('Ctrl Pts',(6.50640787711486,2.23136172266864,3.19831519594175));
#116459=CARTESIAN_POINT('Ctrl Pts',(6.187672952,2.36225522,4.238242965));
#116460=CARTESIAN_POINT('Ctrl Pts',(6.325013958,2.323743665,4.03773034));
#116461=CARTESIAN_POINT('Ctrl Pts',(6.449085162,2.285714286,3.828746606));
#116462=CARTESIAN_POINT('Ctrl Pts',(6.53522503500001,2.259311335,3.683653856));
#116463=CARTESIAN_POINT('Ctrl Pts',(6.614752403,2.232664075,3.534833892));
#116464=CARTESIAN_POINT('Ctrl Pts',(6.61669580455652,2.23201289883432,3.53119719488613));
#116465=CARTESIAN_POINT('Ctrl Pts',(6.61863920611304,2.23136172266864,3.52756049777226));
#116466=CARTESIAN_POINT('',(6.55881781646897,2.23266407357604,3.370149744845));
#116467=CARTESIAN_POINT('Ctrl Pts',(6.49942582582478,2.23138000478158,3.21247958576346));
#116468=CARTESIAN_POINT('Ctrl Pts',(6.5011545319124,2.23202203989079,3.20897258388173));
#116469=CARTESIAN_POINT('Ctrl Pts',(6.502883238,2.232664075,3.205465582));
#116470=CARTESIAN_POINT('Ctrl Pts',(6.676449947,2.297126115,2.853353225));
#116471=CARTESIAN_POINT('Ctrl Pts',(6.810981603,2.362252267,2.48455823));
#116472=CARTESIAN_POINT('Ctrl Pts',(6.82891479781365,2.23138000478158,3.10096567712822));
#116473=CARTESIAN_POINT('Ctrl Pts',(6.83058317290683,2.23202203989079,3.09728104706411));
#116474=CARTESIAN_POINT('Ctrl Pts',(6.832251548,2.232664075,3.093596417));
#116475=CARTESIAN_POINT('Ctrl Pts',(6.999760864,2.297126115,2.723649716));
#116476=CARTESIAN_POINT('Ctrl Pts',(7.126344834,2.362252267,2.337778712));
#116477=CARTESIAN_POINT('',(6.83225154862371,2.23266407419428,3.09359641048888));
#116478=CARTESIAN_POINT('',(7.04477374955499,2.32233405367244,2.57316202661038));
#116479=CARTESIAN_POINT('Origin',(-0.182442567298916,2.41067412336642,-0.05155556175439));
#116480=CARTESIAN_POINT('Ctrl Pts',(6.80937368739757,2.36147458196701,2.48896162643404));
#116481=CARTESIAN_POINT('Ctrl Pts',(6.84853550980437,2.35461431097957,2.50300892515723));
#116482=CARTESIAN_POINT('Ctrl Pts',(6.88775575231982,2.3479281660991,2.5170562837039));
#116483=CARTESIAN_POINT('Ctrl Pts',(6.96620988394452,2.33489257270089,2.54511754579731));
#116484=CARTESIAN_POINT('Ctrl Pts',(7.00548975460885,2.32853549069996,2.5591478939061));
#116485=CARTESIAN_POINT('Ctrl Pts',(7.04477374892139,2.3223340536994,2.57316202839838));
#116486=CARTESIAN_POINT('',(6.66756739925649,2.23266407264717,3.14953098625499));
#116487=CARTESIAN_POINT('Origin',(1.2641797331181E-12,2.32340998499933,
5.06756095419725E-13));
#116488=CARTESIAN_POINT('',(7.04549163556671,2.14301213123943,2.5711957558057));
#116489=CARTESIAN_POINT('Origin',(-0.181868274181169,2.01794103510997,-0.0450803477170658));
#116490=CARTESIAN_POINT('',(7.21998796362812,2.23266407449122,2.03021520441984));
#116491=CARTESIAN_POINT('Origin',(-0.181968764875902,2.4105239964154,-0.0217912721690444));
#116492=CARTESIAN_POINT('Ctrl Pts',(7.0447737499108,2.32233405321779,2.57316202540825));
#116493=CARTESIAN_POINT('Ctrl Pts',(7.07149016287349,2.3100687416172,2.50001813309078));
#116494=CARTESIAN_POINT('Ctrl Pts',(7.09702678981718,2.29785936479699,2.42656859183786));
#116495=CARTESIAN_POINT('Ctrl Pts',(7.1213764777493,2.28571428606199,2.35286996114428));
#116496=CARTESIAN_POINT('Ctrl Pts',(7.1565774577418,2.26815682571472,2.24632797948178));
#116497=CARTESIAN_POINT('Ctrl Pts',(7.18947543979843,2.25046493734972,2.13872590177396));
#116498=CARTESIAN_POINT('Ctrl Pts',(7.21998796682949,2.23266407446841,2.0302152006245));
#116499=CARTESIAN_POINT('Ctrl Pts',(6.807737232,2.36225522,2.493434134));
#116500=CARTESIAN_POINT('Ctrl Pts',(6.888537402,2.323743665,2.272828217));
#116501=CARTESIAN_POINT('Ctrl Pts',(6.954885505,2.285714286,2.047453934));
#116502=CARTESIAN_POINT('Ctrl Pts',(7.000949515,2.259311335,1.890981591));
#116503=CARTESIAN_POINT('Ctrl Pts',(7.039929788,2.232664075,1.732595906));
#116504=CARTESIAN_POINT('Ctrl Pts',(7.0408823446497,2.23201289883432,1.72872545241275));
#116505=CARTESIAN_POINT('Ctrl Pts',(7.04183490129941,2.23136172266864,1.7248549988255));
#116506=CARTESIAN_POINT('Ctrl Pts',(6.954105553,2.36225522,2.808988422));
#116507=CARTESIAN_POINT('Ctrl Pts',(7.045131315,2.323743665,2.583639413));
#116508=CARTESIAN_POINT('Ctrl Pts',(7.121376478,2.285714286,2.352869961));
#116509=CARTESIAN_POINT('Ctrl Pts',(7.174311796,2.259311335,2.192651873));
#116510=CARTESIAN_POINT('Ctrl Pts',(7.219987966,2.232664075,2.030215204));
#116511=CARTESIAN_POINT('Ctrl Pts',(7.22110414954922,2.23201289883432,2.0262457569617));
#116512=CARTESIAN_POINT('Ctrl Pts',(7.22222033309843,2.23136172266864,2.02227630992341));
#116513=CARTESIAN_POINT('',(7.12995887474965,2.23266407357604,1.88140556352814));
#116514=CARTESIAN_POINT('Ctrl Pts',(7.03806101166501,2.23138000478158,1.74018916767838));
#116515=CARTESIAN_POINT('Ctrl Pts',(7.0389953998325,2.23202203989079,1.73639253683919));
#116516=CARTESIAN_POINT('Ctrl Pts',(7.039929788,2.232664075,1.732595906));
#116517=CARTESIAN_POINT('Ctrl Pts',(7.133744856,2.297126115,1.351404028));
#116518=CARTESIAN_POINT('Ctrl Pts',(7.185851215,2.362252267,0.962310925));
#116519=CARTESIAN_POINT('Ctrl Pts',(7.3358745212548,2.23138000478158,1.56045200257577));
#116520=CARTESIAN_POINT('Ctrl Pts',(7.3367118041274,2.23202203989079,1.55649486578788));
#116521=CARTESIAN_POINT('Ctrl Pts',(7.337549087,2.232664075,1.552537729));
#116522=CARTESIAN_POINT('Ctrl Pts',(7.421614524,2.297126115,1.155230625));
#116523=CARTESIAN_POINT('Ctrl Pts',(7.462288171,2.362252267,0.751169259));
#116524=CARTESIAN_POINT('',(7.33754908621416,2.23266407419427,1.5525377224994));
#116525=CARTESIAN_POINT('',(7.43322462809307,2.32233405369076,0.998584814253996));
#116526=CARTESIAN_POINT('Origin',(-0.189259838612895,2.41067412263089,-0.0111304280783903));
#116527=CARTESIAN_POINT('Ctrl Pts',(7.18522749154915,2.3614745818536,0.966957027476653));
#116528=CARTESIAN_POINT('Ctrl Pts',(7.22649349810488,2.35461430893834,0.972257275442808));
#116529=CARTESIAN_POINT('Ctrl Pts',(7.26781657349002,2.34792816205629,0.977545023481249));
#116530=CARTESIAN_POINT('Ctrl Pts',(7.35046881019824,2.33489257229042,0.988084906829652));
#116531=CARTESIAN_POINT('Ctrl Pts',(7.39184645224129,2.32853548990041,0.99334322253187));
#116532=CARTESIAN_POINT('Ctrl Pts',(7.43322462785181,2.32233405371819,0.998584816191025));
#116533=CARTESIAN_POINT('',(7.18873944076293,2.23266407264717,1.64256680321968));
#116534=CARTESIAN_POINT('Origin',(-9.44556932669371E-13,2.32340998499944,
-1.57263525119022E-13));
#116535=CARTESIAN_POINT('',(7.43350303971341,2.14301213123584,0.996510189563523));
#116536=CARTESIAN_POINT('Origin',(-0.187307222202631,2.0179410143598,-0.00493008707019446));
#116537=CARTESIAN_POINT('',(7.48762491278476,2.23266407449122,0.430665910956783));
#116538=CARTESIAN_POINT('Origin',(-0.182398313896053,2.41052395036109,0.017836156865229));
#116539=CARTESIAN_POINT('Ctrl Pts',(7.43322462815202,2.32233405322792,0.998584812966175));
#116540=CARTESIAN_POINT('Ctrl Pts',(7.4435926514556,2.31006874162622,0.921407745357249));
#116541=CARTESIAN_POINT('Ctrl Pts',(7.45274276603645,2.29785936480243,0.844185793800922));
#116542=CARTESIAN_POINT('Ctrl Pts',(7.4606801448002,2.28571428603199,0.766975732997686));
#116543=CARTESIAN_POINT('Ctrl Pts',(7.47215476891025,2.2681568256412,0.655357473043764));
#116544=CARTESIAN_POINT('Ctrl Pts',(7.48115234803254,2.25046493734972,0.543198978937179));
#116545=CARTESIAN_POINT('Ctrl Pts',(7.48762491508439,2.23266407446841,0.430665906525027));
#116546=CARTESIAN_POINT('Ctrl Pts',(7.184590752,2.36225522,0.971676760000001));
#116547=CARTESIAN_POINT('Ctrl Pts',(7.21607810799999,2.323743665,0.738858839));
#116548=CARTESIAN_POINT('Ctrl Pts',(7.23242622,2.285714286,0.5044908));
#116549=CARTESIAN_POINT('Ctrl Pts',(7.243776351,2.259311335,0.341774293));
#116550=CARTESIAN_POINT('Ctrl Pts',(7.247797047,2.232664075,0.178711971));
#116551=CARTESIAN_POINT('Ctrl Pts',(7.24789530030652,2.23201289883432,0.174727234948065));
#116552=CARTESIAN_POINT('Ctrl Pts',(7.24799355361303,2.23136172266864,0.170742498896129));
#116553=CARTESIAN_POINT('Ctrl Pts',(7.39537190800001,2.36225522,1.248388701));
#116554=CARTESIAN_POINT('Ctrl Pts',(7.435826162,2.323743665,1.008740379));
#116555=CARTESIAN_POINT('Ctrl Pts',(7.460680145,2.285714286,0.766975733));
#116556=CARTESIAN_POINT('Ctrl Pts',(7.477935712,2.259311335,0.599123926));
#116557=CARTESIAN_POINT('Ctrl Pts',(7.487624915,2.232664075,0.43066591));
#116558=CARTESIAN_POINT('Ctrl Pts',(7.48786168898945,2.23201289883432,0.42654931996645));
#116559=CARTESIAN_POINT('Ctrl Pts',(7.4880984629789,2.23136172266864,0.4224327299329));
#116560=CARTESIAN_POINT('',(7.36771098063556,2.23266407357604,0.304688949312516));
#116561=CARTESIAN_POINT('Ctrl Pts',(7.24760428844329,2.23138000478158,0.186529438107579));
#116562=CARTESIAN_POINT('Ctrl Pts',(7.24770066772165,2.23202203989079,0.182620704553789));
#116563=CARTESIAN_POINT('Ctrl Pts',(7.247797047,2.232664075,0.178711971));
#116564=CARTESIAN_POINT('Ctrl Pts',(7.257473784,2.297126115,-0.213735319));
#116565=CARTESIAN_POINT('Ctrl Pts',(7.22471841,2.362252267,-0.604932968));
#116566=CARTESIAN_POINT('Ctrl Pts',(7.49981690556088,2.23138000478158,-0.0530266736009007));
#116567=CARTESIAN_POINT('Ctrl Pts',(7.49978394578045,2.23202203989079,-0.0570712858004503));
#116568=CARTESIAN_POINT('Ctrl Pts',(7.49975098600001,2.232664075,-0.061115898));
#116569=CARTESIAN_POINT('Ctrl Pts',(7.496441736,2.297126115,-0.467205767));
#116570=CARTESIAN_POINT('Ctrl Pts',(7.449303207,2.362252267,-0.870564034));
#116571=CARTESIAN_POINT('',(7.49975098383396,2.23266407419428,-0.0611159041764366));
#116572=CARTESIAN_POINT('',(7.47410618406036,2.32233405362781,-0.622685114197929));
#116573=CARTESIAN_POINT('Origin',(-0.187228056671962,2.41067415935372,0.0298150878062447));
#116574=CARTESIAN_POINT('Ctrl Pts',(7.22510804352427,2.36147458190683,-0.60026140704127));
#116575=CARTESIAN_POINT('Ctrl Pts',(7.26654867589849,2.35461430806005,-0.603956047999222));
#116576=CARTESIAN_POINT('Ctrl Pts',(7.30804235665987,2.34792816019782,-0.607675164886424));
#116577=CARTESIAN_POINT('Ctrl Pts',(7.39102797852344,2.33489257272257,-0.615149484637324));
#116578=CARTESIAN_POINT('Ctrl Pts',(7.43256861342513,2.32853549078482,-0.618909075139608));
#116579=CARTESIAN_POINT('Ctrl Pts',(7.47410618422981,2.32233405365464,-0.622685112329022));
#116580=CARTESIAN_POINT('',(7.3737740166168,2.23266407264717,0.0587980218521181));
#116581=CARTESIAN_POINT('Origin',(-1.03779831950312E-12,2.32340998499944,
3.63919235458338E-14));
#116582=CARTESIAN_POINT('',(7.47393210382702,2.14301213124514,-0.624771085990036));
#116583=CARTESIAN_POINT('Origin',(-0.18398813477026,2.01794104937221,0.0354506976473318));
#116584=CARTESIAN_POINT('',(7.40514884403309,2.23266407449122,-1.18902084260639));
#116585=CARTESIAN_POINT('Origin',(-0.17430000017074,2.41052401608581,0.0566294523303079));
#116586=CARTESIAN_POINT('Ctrl Pts',(7.47410618389678,2.32233405317591,-0.622685115421782));
#116587=CARTESIAN_POINT('Ctrl Pts',(7.46764102034714,2.31006874158847,-0.700286644744279));
#116588=CARTESIAN_POINT('Ctrl Pts',(7.45997677338716,2.29785936478234,-0.777670194344572));
#116589=CARTESIAN_POINT('Ctrl Pts',(7.45113069970861,2.28571428608203,-0.854781428739722));
#116590=CARTESIAN_POINT('Ctrl Pts',(7.43834242647713,2.26815682576385,-0.966256820570834));
#116591=CARTESIAN_POINT('Ctrl Pts',(7.42301888672561,2.25046493734972,-1.0777273253983));
#116592=CARTESIAN_POINT('Ctrl Pts',(7.40514884533586,2.23266407446841,-1.18902084741156));
#116593=CARTESIAN_POINT('Ctrl Pts',(7.225500794,2.36225522,-0.595515139));
#116594=CARTESIAN_POINT('Ctrl Pts',(7.206203021,2.323743665,-0.829658758));
#116595=CARTESIAN_POINT('Ctrl Pts',(7.171786724,2.285714286,-1.062061763));
#116596=CARTESIAN_POINT('Ctrl Pts',(7.147892255,2.259311335,-1.22341399));
#116597=CARTESIAN_POINT('Ctrl Pts',(7.11676537100001,2.232664075,-1.383528337));
#116598=CARTESIAN_POINT('Ctrl Pts',(7.11600472675467,2.23201289883432,-1.38744103371067));
#116599=CARTESIAN_POINT('Ctrl Pts',(7.11524408250935,2.23136172266864,-1.39135373042133));
#116600=CARTESIAN_POINT('Ctrl Pts',(7.490838891,2.36225522,-0.370584287));
#116601=CARTESIAN_POINT('Ctrl Pts',(7.47883004200001,2.323743665,-0.613326232999999));
#116602=CARTESIAN_POINT('Ctrl Pts',(7.4511307,2.285714286,-0.854781429));
#116603=CARTESIAN_POINT('Ctrl Pts',(7.43189966400001,2.259311335,-1.022418391));
#116604=CARTESIAN_POINT('Ctrl Pts',(7.405148846,2.232664075,-1.189020844));
#116605=CARTESIAN_POINT('Ctrl Pts',(7.40449513919885,2.23201289883432,-1.19309208984433));
#116606=CARTESIAN_POINT('Ctrl Pts',(7.40384143239769,2.23136172266864,-1.19716333568867));
#116607=CARTESIAN_POINT('',(7.26095711003851,2.23266407357604,-1.28627458181517));
#116608=CARTESIAN_POINT('Ctrl Pts',(7.11825764338815,2.23138000478158,-1.37585220051464));
#116609=CARTESIAN_POINT('Ctrl Pts',(7.11751150719407,2.23202203989079,-1.37969026875732));
#116610=CARTESIAN_POINT('Ctrl Pts',(7.116765371,2.232664075,-1.383528337));
#116611=CARTESIAN_POINT('Ctrl Pts',(7.041851304,2.297126115,-1.768880641));
#116612=CARTESIAN_POINT('Ctrl Pts',(6.925765802,2.362252267,-2.143890869));
#116613=CARTESIAN_POINT('Ctrl Pts',(7.3130761865187,2.23138000478158,-1.6640258809411));
#116614=CARTESIAN_POINT('Ctrl Pts',(7.31217452525935,2.23202203989079,-1.66796884697055));
#116615=CARTESIAN_POINT('Ctrl Pts',(7.31127286400001,2.232664075,-1.671911813));
#116616=CARTESIAN_POINT('Ctrl Pts',(7.220743665,2.297126115,-2.067796135));
#116617=CARTESIAN_POINT('Ctrl Pts',(7.087997104,2.362252267,-2.45159072));
#116618=CARTESIAN_POINT('',(7.31127286055811,2.23266407419428,-1.6719118185767));
#116619=CARTESIAN_POINT('',(7.1655068417734,2.32233405367377,-2.21483897860599));
#116620=CARTESIAN_POINT('Origin',(-0.176441304273448,2.41067412198656,0.0693664900664823));
#116621=CARTESIAN_POINT('Ctrl Pts',(6.92715057363297,2.36147458189601,-2.13941228615809));
#116622=CARTESIAN_POINT('Ctrl Pts',(6.96682809443332,2.35461431046545,-2.15192905488734));
#116623=CARTESIAN_POINT('Ctrl Pts',(7.00655215963655,2.34792816513596,-2.16448113041335));
#116624=CARTESIAN_POINT('Ctrl Pts',(7.08599089882905,2.33489257228985,-2.18962017048139));
#116625=CARTESIAN_POINT('Ctrl Pts',(7.12575213894984,2.32853548992283,-2.2022218732359));
#116626=CARTESIAN_POINT('Ctrl Pts',(7.16550684236562,2.32233405370095,-2.21483897675337));
#116627=CARTESIAN_POINT('',(7.21401911446521,2.23266407264717,-1.52772008933053));
#116628=CARTESIAN_POINT('Origin',(-1.05167610731094E-12,2.32340998500022,
2.90457762008867E-13));
#116629=CARTESIAN_POINT('',(7.16488840930825,2.14301213126003,-2.21683875915713));
#116630=CARTESIAN_POINT('Origin',(-0.172065475689857,2.01794104906444,0.0741738152460494));
#116631=CARTESIAN_POINT('',(6.97641624536834,2.23266407449123,-2.75311030322781));
#116632=CARTESIAN_POINT('Origin',(-0.158051170809693,2.41052394479208,0.0927747698878856));
#116633=CARTESIAN_POINT('Ctrl Pts',(7.1655068412746,2.32233405321481,-2.21483897978952));
#116634=CARTESIAN_POINT('Ctrl Pts',(7.14251079480109,2.3100687416172,-2.28923640953947));
#116635=CARTESIAN_POINT('Ctrl Pts',(7.1183905580205,2.29785936479817,-2.36316318834194));
#116636=CARTESIAN_POINT('Ctrl Pts',(7.09317466455831,2.28571428613813,-2.43656996049194));
#116637=CARTESIAN_POINT('Ctrl Pts',(7.05672145941097,2.26815682590133,-2.54269001813063));
#116638=CARTESIAN_POINT('Ctrl Pts',(7.0177933125215,2.25046493734972,-2.64826029694318));
#116639=CARTESIAN_POINT('Ctrl Pts',(6.97641624561796,2.23266407446841,-2.75311030818904));
#116640=CARTESIAN_POINT('Ctrl Pts',(6.92855444900001,2.36225522,-2.134861413));
#116641=CARTESIAN_POINT('Ctrl Pts',(6.859373891,2.323743665,-2.359382433));
#116642=CARTESIAN_POINT('Ctrl Pts',(6.775802451,2.285714286,-2.578953498));
#116643=CARTESIAN_POINT('Ctrl Pts',(6.717780663,2.259311335,-2.731396796));
#116644=CARTESIAN_POINT('Ctrl Pts',(6.65296165500001,2.232664075,-2.881076398));
#116645=CARTESIAN_POINT('Ctrl Pts',(6.65137768002123,2.23201289883432,-2.88473410199325));
#116646=CARTESIAN_POINT('Ctrl Pts',(6.64979370504246,2.23136172266864,-2.88839180598651));
#116647=CARTESIAN_POINT('Ctrl Pts',(7.236042573,2.36225522,-1.972229166));
#116648=CARTESIAN_POINT('Ctrl Pts',(7.172132141,2.323743665,-2.206714393));
#116649=CARTESIAN_POINT('Ctrl Pts',(7.093174665,2.285714286,-2.436569961));
#116650=CARTESIAN_POINT('Ctrl Pts',(7.038356248,2.259311335,-2.596153559));
#116651=CARTESIAN_POINT('Ctrl Pts',(6.976416247,2.232664075,-2.753110305));
#116652=CARTESIAN_POINT('Ctrl Pts',(6.97490262599906,2.23201289883432,-2.75694583976186));
#116653=CARTESIAN_POINT('Ctrl Pts',(6.97338900499812,2.23136172266864,-2.76078137452372));
#116654=CARTESIAN_POINT('',(6.81468895436952,2.23266407357604,-2.81709334334895));
#116655=CARTESIAN_POINT('Ctrl Pts',(6.65606918130503,2.23138000478158,-2.87390051977844));
#116656=CARTESIAN_POINT('Ctrl Pts',(6.65451541815251,2.23202203989079,-2.87748845888922));
#116657=CARTESIAN_POINT('Ctrl Pts',(6.652961655,2.232664075,-2.881076398));
#116658=CARTESIAN_POINT('Ctrl Pts',(6.496959684,2.297126115,-3.241315069));
#116659=CARTESIAN_POINT('Ctrl Pts',(6.302972082,2.362252267,-3.582602815));
#116660=CARTESIAN_POINT('Ctrl Pts',(6.78438415313431,2.23138000478158,-3.1972170876818));
#116661=CARTESIAN_POINT('Ctrl Pts',(6.78265595106716,2.23202203989079,-3.2008740388409));
#116662=CARTESIAN_POINT('Ctrl Pts',(6.780927749,2.232664075,-3.20453099));
#116663=CARTESIAN_POINT('Ctrl Pts',(6.607411645,2.297126115,-3.571698655));
#116664=CARTESIAN_POINT('Ctrl Pts',(6.395264134,2.362252267,-3.917983749));
#116665=CARTESIAN_POINT('',(6.78092774444002,2.23266407419428,-3.20453099470365));
#116666=CARTESIAN_POINT('',(6.52185636336245,2.32233405368499,-3.70342943434098));
#116667=CARTESIAN_POINT('Origin',(-0.157404492658647,2.41067413902249,0.105674428825331));
#116668=CARTESIAN_POINT('Ctrl Pts',(6.30528724150653,2.36147458185392,-3.57852662370195));
#116669=CARTESIAN_POINT('Ctrl Pts',(6.34134640862966,2.3546143066515,-3.5992802631257));
#116670=CARTESIAN_POINT('Ctrl Pts',(6.37744344503381,2.34792815738207,-3.62007839131622));
#116671=CARTESIAN_POINT('Ctrl Pts',(6.44962074858874,2.33489257385853,-3.66170664582743));
#116672=CARTESIAN_POINT('Ctrl Pts',(6.48574338974461,2.32853549307499,-3.68256121353421));
#116673=CARTESIAN_POINT('Ctrl Pts',(6.52185636417603,2.32233405372278,-3.70342943278937));
#116674=CARTESIAN_POINT('',(6.71694469595552,2.23266407264717,-3.0428037073431));
#116675=CARTESIAN_POINT('Origin',(-1.48535697630514E-12,2.32340998499956,
9.15933995315754E-13));
#116676=CARTESIAN_POINT('',(6.52082249544694,2.14301213121499,-3.70524951652264));
#116677=CARTESIAN_POINT('Origin',(-0.152097410899558,2.01794104260894,0.109428621450758));
#116678=CARTESIAN_POINT('',(6.22147417679742,2.23266407449122,-4.18846738491079));
#116679=CARTESIAN_POINT('Origin',(-0.134411997813026,2.41052396482033,0.124581958717048));
#116680=CARTESIAN_POINT('Ctrl Pts',(6.52185636285941,2.32233405324098,-3.70342943540267));
#116681=CARTESIAN_POINT('Ctrl Pts',(6.483404702948,2.3100687416266,-3.77114402426926));
#116682=CARTESIAN_POINT('Ctrl Pts',(6.44395631178173,2.29785936479879,-3.83815729788785));
#116683=CARTESIAN_POINT('Ctrl Pts',(6.40354966577465,2.28571428603063,-3.90442718890095));
#116684=CARTESIAN_POINT('Ctrl Pts',(6.34513604105734,2.26815682563787,-4.00022985843361));
#116685=CARTESIAN_POINT('Ctrl Pts',(6.28442352312462,2.25046493734972,-4.0949635606698));
#116686=CARTESIAN_POINT('Ctrl Pts',(6.22147417596399,2.23266407446841,-4.18846738981751));
#116687=CARTESIAN_POINT('Ctrl Pts',(6.307636598,2.36225522,-3.574383939));
#116688=CARTESIAN_POINT('Ctrl Pts',(6.191808061,2.323743665,-3.778784008));
#116689=CARTESIAN_POINT('Ctrl Pts',(6.062989186,2.285714286,-3.975256234));
#116690=CARTESIAN_POINT('Ctrl Pts',(5.973553112,2.259311335,-4.111662523));
#116691=CARTESIAN_POINT('Ctrl Pts',(5.878072847,2.232664075,-4.243908529));
#116692=CARTESIAN_POINT('Ctrl Pts',(5.87573960625175,2.23201289883432,-4.24714021012271));
#116693=CARTESIAN_POINT('Ctrl Pts',(5.87340636550352,2.23136172266864,-4.25037189124542));
#116694=CARTESIAN_POINT('Ctrl Pts',(6.642896946,2.36225522,-3.481654802));
#116695=CARTESIAN_POINT('Ctrl Pts',(6.530073313,2.323743665,-3.696919041));
#116696=CARTESIAN_POINT('Ctrl Pts',(6.403549666,2.285714286,-3.904427189));
#116697=CARTESIAN_POINT('Ctrl Pts',(6.315707117,2.259311335,-4.048495473));
#116698=CARTESIAN_POINT('Ctrl Pts',(6.221474178,2.232664075,-4.188467387));
#116699=CARTESIAN_POINT('Ctrl Pts',(6.21917141802021,2.23201289883432,-4.19188786528789));
#116700=CARTESIAN_POINT('Ctrl Pts',(6.21686865804042,2.23136172266864,-4.19530834357579));
#116701=CARTESIAN_POINT('',(6.04977351754298,2.23266407357604,-4.21618795076387));
#116702=CARTESIAN_POINT('Ctrl Pts',(5.88265032276119,2.23138000478158,-4.23756844513487));
#116703=CARTESIAN_POINT('Ctrl Pts',(5.8803615848806,2.23202203989079,-4.24073848706743));
#116704=CARTESIAN_POINT('Ctrl Pts',(5.878072847,2.232664075,-4.243908529));
#116705=CARTESIAN_POINT('Ctrl Pts',(5.64827745,2.297126115,-4.562189207));
#116706=CARTESIAN_POINT('Ctrl Pts',(5.385458394,2.362252267,-4.853796235));
#116707=CARTESIAN_POINT('Ctrl Pts',(5.93846185711766,2.23138000478158,-4.58090997634739));
#116708=CARTESIAN_POINT('Ctrl Pts',(5.93598792305883,2.23202203989079,-4.5841099176737));
#116709=CARTESIAN_POINT('Ctrl Pts',(5.933513989,2.232664075,-4.587309859));
#116710=CARTESIAN_POINT('Ctrl Pts',(5.685124401,2.297126115,-4.908592516));
#116711=CARTESIAN_POINT('Ctrl Pts',(5.403495721,2.362252267,-5.201176212));
#116712=CARTESIAN_POINT('',(5.93351398353206,2.23266407419428,-4.58730986262407));
#116713=CARTESIAN_POINT('',(5.57325113022134,2.3223340536832,-5.01885164571133));
#116714=CARTESIAN_POINT('Origin',(-0.131007258613514,2.41067415088804,0.137040855787069));
#116715=CARTESIAN_POINT('Ctrl Pts',(5.3885956869058,2.36147458187527,-4.85031303370965));
#116716=CARTESIAN_POINT('Ctrl Pts',(5.41935036612432,2.35461431232922,-4.87833309640803));
#116717=CARTESIAN_POINT('Ctrl Pts',(5.45013246168415,2.34792816896932,-4.90640474497083));
#116718=CARTESIAN_POINT('Ctrl Pts',(5.51167351162437,2.3348925735735,-4.9625757919582));
#116719=CARTESIAN_POINT('Ctrl Pts',(5.54246851123432,2.32853549252457,-4.99070809286661));
#116720=CARTESIAN_POINT('Ctrl Pts',(5.57325113138551,2.32233405371842,-5.01885164435842));
#116721=CARTESIAN_POINT('',(5.90579340922846,2.23266407264717,-4.41560920573176));
#116722=CARTESIAN_POINT('Origin',(-4.95697233260373E-13,2.32340998500067,
4.70110061989715E-13));
#116723=CARTESIAN_POINT('',(5.57185016995924,2.14301213124523,-5.02040692436461));
#116724=CARTESIAN_POINT('Origin',(-0.125017759930015,2.0179410069928,0.139566873922891));
#116725=CARTESIAN_POINT('',(5.1756228902727,2.23266407449123,-5.42797638770235));
#116726=CARTESIAN_POINT('Origin',(-0.104488342135182,2.41052403993646,0.150564189044248));
#116727=CARTESIAN_POINT('Ctrl Pts',(5.57325112946139,2.32233405323673,-5.01885164662856));
#116728=CARTESIAN_POINT('Ctrl Pts',(5.5211418130037,2.31006874162515,-5.0767171358636));
#116729=CARTESIAN_POINT('Ctrl Pts',(5.46820983040542,2.29785936479876,-5.13368343845998));
#116730=CARTESIAN_POINT('Ctrl Pts',(5.41450180158365,2.28571428604938,-5.18971774176479));
#116731=CARTESIAN_POINT('Ctrl Pts',(5.33685911222919,2.26815682568383,-5.27072339526756));
#116732=CARTESIAN_POINT('Ctrl Pts',(5.25720107397725,2.25046493734972,-5.35019087963778));
#116733=CARTESIAN_POINT('Ctrl Pts',(5.17562288840667,2.23266407446841,-5.42797639231399));
#116734=CARTESIAN_POINT('Ctrl Pts',(5.391780671,2.36225522,-4.846772245));
#116735=CARTESIAN_POINT('Ctrl Pts',(5.234720168,2.323743665,-5.021493842));
#116736=CARTESIAN_POINT('Ctrl Pts',(5.066677286,2.285714286,-5.185680407));
#116737=CARTESIAN_POINT('Ctrl Pts',(4.950008857,2.259311335,-5.29967148));
#116738=CARTESIAN_POINT('Ctrl Pts',(4.828331886,2.232664075,-5.408300213));
#116739=CARTESIAN_POINT('Ctrl Pts',(4.82535847922468,2.23201289883432,-5.41095476141654));
#116740=CARTESIAN_POINT('Ctrl Pts',(4.82238507244937,2.23136172266864,-5.41360930983306));
#116741=CARTESIAN_POINT('Ctrl Pts',(5.739136842,2.36225522,-4.828282128));
#116742=CARTESIAN_POINT('Ctrl Pts',(5.58267551400001,2.323743665,-5.014259863));
#116743=CARTESIAN_POINT('Ctrl Pts',(5.414501802,2.285714286,-5.189717742));
#116744=CARTESIAN_POINT('Ctrl Pts',(5.29774254,2.259311335,-5.311534238));
#116745=CARTESIAN_POINT('Ctrl Pts',(5.175622891,2.232664075,-5.42797639000001));
#116746=CARTESIAN_POINT('Ctrl Pts',(5.17263866655102,2.23201289883432,-5.43082187407841));
#116747=CARTESIAN_POINT('Ctrl Pts',(5.16965444210204,2.23136172266864,-5.43366735815682));
#116748=CARTESIAN_POINT('',(5.00197739498063,2.23266407357604,-5.41813829551714));
#116749=CARTESIAN_POINT('Ctrl Pts',(4.83416527354552,2.23138000478158,-5.40309237873128));
#116750=CARTESIAN_POINT('Ctrl Pts',(4.83124857977277,2.23202203989079,-5.40569629586564));
#116751=CARTESIAN_POINT('Ctrl Pts',(4.828331886,2.232664075,-5.40830021300001));
#116752=CARTESIAN_POINT('Ctrl Pts',(4.53548804,2.297126115,-5.669740449));
#116753=CARTESIAN_POINT('Ctrl Pts',(4.216126656,2.362252267,-5.898031538));
#116754=CARTESIAN_POINT('Ctrl Pts',(4.81486368430831,2.23138000478158,-5.75040460645348));
#116755=CARTESIAN_POINT('Ctrl Pts',(4.81175969665416,2.23202203989079,-5.75299791222674));
#116756=CARTESIAN_POINT('Ctrl Pts',(4.808655709,2.232664075,-5.755591218));
#116757=CARTESIAN_POINT('Ctrl Pts',(4.497007057,2.297126115,-6.015966045));
#116758=CARTESIAN_POINT('Ctrl Pts',(4.159065854,2.362252267,-6.241167457));
#116759=CARTESIAN_POINT('',(4.80865570287358,2.23266407419429,-5.75559122037632));
#116760=CARTESIAN_POINT('',(4.36404686809461,2.3223340536569,-6.09959793199742));
#116761=CARTESIAN_POINT('Origin',(-0.0984849361830059,2.41067415219992,
0.161999976496024));
#116762=CARTESIAN_POINT('Ctrl Pts',(4.21993938588018,2.36147458191207,-5.89530419738615));
#116763=CARTESIAN_POINT('Ctrl Pts',(4.24395154837877,2.35461431359499,-5.92928050741024));
#116764=CARTESIAN_POINT('Ctrl Pts',(4.26797939614879,2.34792817149799,-5.96331309003516));
#116765=CARTESIAN_POINT('Ctrl Pts',(4.31600654425107,2.33489257380625,-6.03140040752346));
#116766=CARTESIAN_POINT('Ctrl Pts',(4.34003395981166,2.32853549297441,-6.06549500410895));
#116767=CARTESIAN_POINT('Ctrl Pts',(4.36404686948249,2.3223340536942,-6.09959793093269));
#116768=CARTESIAN_POINT('',(4.81849378641155,2.23266407264717,-5.58194572507186));
#116769=CARTESIAN_POINT('Origin',(2.45246531416221E-13,2.32340998499944,
-3.56919355182228E-13));
#116770=CARTESIAN_POINT('',(4.36234432276977,2.14301213124795,-6.10081568386786));
#116771=CARTESIAN_POINT('Origin',(-0.0920919309245477,2.01794106337157,
0.163178683584191));
#116772=CARTESIAN_POINT('',(3.88776522976379,2.23266407449123,-6.4136792476037));
#116773=CARTESIAN_POINT('Origin',(-0.0696785071243489,2.41052398726883,
0.169505791714497));
#116774=CARTESIAN_POINT('Ctrl Pts',(4.36404686719633,2.32233405321387,-6.09959793274587));
#116775=CARTESIAN_POINT('Ctrl Pts',(4.30071646795032,2.31006874160842,-6.14490859616822));
#116776=CARTESIAN_POINT('Ctrl Pts',(4.23677593453902,2.29785936478988,-6.18916424668093));
#116777=CARTESIAN_POINT('Ctrl Pts',(4.17227785102704,2.28571428609381,-6.23234286055701));
#116778=CARTESIAN_POINT('Ctrl Pts',(4.07903658490318,2.26815682579272,-6.29476376356859));
#116779=CARTESIAN_POINT('Ctrl Pts',(3.98415774636946,2.25046493734972,-6.35524921920965));
#116780=CARTESIAN_POINT('Ctrl Pts',(3.88776522696987,2.23266407446841,-6.41367925170241));
#116781=CARTESIAN_POINT('Ctrl Pts',(4.223811072,2.36225522,-5.89253086800001));
#116782=CARTESIAN_POINT('Ctrl Pts',(4.032862577,2.323743665,-6.029404205));
#116783=CARTESIAN_POINT('Ctrl Pts',(3.833453187,2.285714286,-6.153627927));
#116784=CARTESIAN_POINT('Ctrl Pts',(3.69500769,2.259311335,-6.239873689));
#116785=CARTESIAN_POINT('Ctrl Pts',(3.552823492,2.232664075,-6.319805791));
#116786=CARTESIAN_POINT('Ctrl Pts',(3.549348952371,2.23201289883432,-6.32175908299683));
#116787=CARTESIAN_POINT('Ctrl Pts',(3.54587441274199,2.23136172266864,-6.32371237499365));
#116788=CARTESIAN_POINT('Ctrl Pts',(4.567021077,2.36225522,-5.949144349));
#116789=CARTESIAN_POINT('Ctrl Pts',(4.374238013,2.323743665,-6.097139466));
#116790=CARTESIAN_POINT('Ctrl Pts',(4.172277851,2.285714286,-6.232342861));
#116791=CARTESIAN_POINT('Ctrl Pts',(4.032061411,2.259311335,-6.326211565));
#116792=CARTESIAN_POINT('Ctrl Pts',(3.88776523,2.232664075,-6.41367925));
#116793=CARTESIAN_POINT('Ctrl Pts',(3.88423908007441,2.23201289883432,-6.41581668821089));
#116794=CARTESIAN_POINT('Ctrl Pts',(3.88071293014881,2.23136172266864,-6.41795412642177));
#116795=CARTESIAN_POINT('',(3.72029436861526,2.23266407357604,-6.36674251605016));
#116796=CARTESIAN_POINT('Ctrl Pts',(3.55964002860692,2.23138000478158,-6.31597371891253));
#116797=CARTESIAN_POINT('Ctrl Pts',(3.55623176030346,2.23202203989079,-6.31788975495627));
#116798=CARTESIAN_POINT('Ctrl Pts',(3.552823492,2.232664075,-6.319805791));
#116799=CARTESIAN_POINT('Ctrl Pts',(3.21062425,2.297126115,-6.512180928));
#116800=CARTESIAN_POINT('Ctrl Pts',(2.849653521,2.362252267,-6.666481441));
#116801=CARTESIAN_POINT('Ctrl Pts',(3.46612783746513,2.23138000478158,-6.65101670874053));
#116802=CARTESIAN_POINT('Ctrl Pts',(3.46253893523256,2.23202203989079,-6.65288211887026));
#116803=CARTESIAN_POINT('Ctrl Pts',(3.458950033,2.232664075,-6.654747529));
#116804=CARTESIAN_POINT('Ctrl Pts',(3.098614662,2.297126115,-6.842039689));
#116805=CARTESIAN_POINT('Ctrl Pts',(2.72016269,2.362252267,-6.989328647));
#116806=CARTESIAN_POINT('',(3.45895002652983,2.23266407419428,-6.65474752997787));
#116807=CARTESIAN_POINT('',(2.95078462496021,2.3223340536514,-6.89513379816407));
#116808=CARTESIAN_POINT('Origin',(-0.0613571587393019,2.41067416161038,
0.179383781189104));
#116809=CARTESIAN_POINT('Ctrl Pts',(2.853963409154,2.36147458188161,-6.66463748826855));
#116810=CARTESIAN_POINT('Ctrl Pts',(2.87011029019925,2.35461430857168,-6.7029813842314));
#116811=CARTESIAN_POINT('Ctrl Pts',(2.88626039459709,2.34792816125834,-6.74138361339339));
#116812=CARTESIAN_POINT('Ctrl Pts',(2.91852790927514,2.33489257365021,-6.81820344517192));
#116813=CARTESIAN_POINT('Ctrl Pts',(2.9346642473191,2.32853549264739,-6.85666611430339));
#116814=CARTESIAN_POINT('Ctrl Pts',(2.95078462656646,2.3223340536871,-6.89513379742501));
#116815=CARTESIAN_POINT('',(3.50588674961313,2.23266407264717,-6.48727666696439));
#116816=CARTESIAN_POINT('Origin',(2.83193607453214E-13,2.32340998499989,
-6.30138302648575E-13));
#116817=CARTESIAN_POINT('',(2.94886010308049,2.14301213124642,-6.89595708322331));
#116818=CARTESIAN_POINT('Origin',(-0.0548604496304522,2.0179410552179,0.1791610850029));
#116819=CARTESIAN_POINT('',(2.4181199873082,2.23266407449122,-7.09948559360941));
#116820=CARTESIAN_POINT('Origin',(-0.0316109121132391,2.41052400205891,
0.180522180259263));
#116821=CARTESIAN_POINT('Ctrl Pts',(2.95078462390421,2.32233405320707,-6.89513379868537));
#116822=CARTESIAN_POINT('Ctrl Pts',(2.87919440088891,2.31006874160469,-6.92577096014036));
#116823=CARTESIAN_POINT('Ctrl Pts',(2.80723510491418,2.29785936478813,-6.95524661337074));
#116824=CARTESIAN_POINT('Ctrl Pts',(2.73496282489214,2.28571428602063,-6.98355055384198));
#116825=CARTESIAN_POINT('Ctrl Pts',(2.63048283853519,2.26815682561336,-7.02446797583331));
#116826=CARTESIAN_POINT('Ctrl Pts',(2.52481962986214,2.25046493734972,-7.06314316892451));
#116827=CARTESIAN_POINT('Ctrl Pts',(2.41811998367477,2.23266407446841,-7.09948559701123));
#116828=CARTESIAN_POINT('Ctrl Pts',(2.858340762,2.36225522,-6.662761296));
#116829=CARTESIAN_POINT('Ctrl Pts',(2.642432815,2.323743665,-6.755386329));
#116830=CARTESIAN_POINT('Ctrl Pts',(2.420981077,2.285714286,-6.833838645));
#116831=CARTESIAN_POINT('Ctrl Pts',(2.26723207,2.259311335,-6.88830634));
#116832=CARTESIAN_POINT('Ctrl Pts',(2.11118902,2.232664075,-6.935804274));
#116833=CARTESIAN_POINT('Ctrl Pts',(2.10737581312693,2.23201289883432,-6.93696497579598));
#116834=CARTESIAN_POINT('Ctrl Pts',(2.10356260625386,2.23136172266864,-6.93812567759196));
#116835=CARTESIAN_POINT('Ctrl Pts',(3.181356483,2.36225522,-6.791831191));
#116836=CARTESIAN_POINT('Ctrl Pts',(2.961266004,2.323743665,-6.894923605));
#116837=CARTESIAN_POINT('Ctrl Pts',(2.734962825,2.285714286,-6.983550554));
#116838=CARTESIAN_POINT('Ctrl Pts',(2.577845571,2.259311335,-7.04508227100001));
#116839=CARTESIAN_POINT('Ctrl Pts',(2.418119987,2.232664075,-7.099485596));
#116840=CARTESIAN_POINT('Ctrl Pts',(2.41421679044806,2.23201289883432,-7.10081504407736));
#116841=CARTESIAN_POINT('Ctrl Pts',(2.41031359389613,2.23136172266864,-7.10214449215472));
#116842=CARTESIAN_POINT('',(2.2646545118938,2.23266407357604,-7.01764493229125));
#116843=CARTESIAN_POINT('Ctrl Pts',(2.11866997199718,2.23138000478158,-6.93352714751366));
#116844=CARTESIAN_POINT('Ctrl Pts',(2.11492949599859,2.23202203989079,-6.93466571075683));
#116845=CARTESIAN_POINT('Ctrl Pts',(2.11118902,2.232664075,-6.93580427400001));
#116846=CARTESIAN_POINT('Ctrl Pts',(1.735635238,2.297126115,-7.050119065));
#116847=CARTESIAN_POINT('Ctrl Pts',(1.349933756,2.362252267,-7.123214082));
#116848=CARTESIAN_POINT('Ctrl Pts',(1.95531970545204,2.23138000478158,-7.24063466103159));
#116849=CARTESIAN_POINT('Ctrl Pts',(1.95141370172602,2.23202203989079,-7.2416849510158));
#116850=CARTESIAN_POINT('Ctrl Pts',(1.947507698,2.232664075,-7.242735241));
#116851=CARTESIAN_POINT('Ctrl Pts',(1.55533449,2.297126115,-7.348187161));
#116852=CARTESIAN_POINT('Ctrl Pts',(1.154067742,2.362252267,-7.410676599));
#116853=CARTESIAN_POINT('',(1.94750769146921,2.23266407419429,-7.24273524056529));
#116854=CARTESIAN_POINT('',(1.39954697245937,2.32233405367958,-7.36826087172726));
#116855=CARTESIAN_POINT('Origin',(-0.0213604939950876,2.41067413430914,
0.188380002614758));
#116856=CARTESIAN_POINT('Ctrl Pts',(1.35453927669525,2.361474581882,-7.12233973837894));
#116857=CARTESIAN_POINT('Ctrl Pts',(1.36206584259948,2.35461431368943,-7.16325824691342));
#116858=CARTESIAN_POINT('Ctrl Pts',(1.36958301587436,2.34792817173249,-7.20423441295965));
#116859=CARTESIAN_POINT('Ctrl Pts',(1.3845821538606,2.33489257278914,-7.28619487280359));
#116860=CARTESIAN_POINT('Ctrl Pts',(1.39207289747177,2.32853549090866,-7.32722714788656));
#116861=CARTESIAN_POINT('Ctrl Pts',(1.39954697431476,2.32233405370702,-7.36826087139055));
#116862=CARTESIAN_POINT('',(2.02934834491728,2.23266407264717,-7.08926976153127));
#116863=CARTESIAN_POINT('Origin',(8.84166871661929E-14,2.32340998499967,
-5.66387214906428E-13));
#116864=CARTESIAN_POINT('',(1.3974904628466,2.14301213120873,-7.36865119339408));
#116865=CARTESIAN_POINT('Origin',(-0.0150634728038704,2.01794104739631,
0.186765608589459));
#116866=CARTESIAN_POINT('',(0.83540614281881,2.23266407449122,-7.45332788373253));
#116867=CARTESIAN_POINT('Origin',(0.00793508467594406,2.41052395448723,
0.183096902090448));
#116868=CARTESIAN_POINT('Ctrl Pts',(1.39954697122311,2.32233405322557,-7.36826087189618));
#116869=CARTESIAN_POINT('Ctrl Pts',(1.32304440380988,2.31006874162192,-7.38279197187679));
#116870=CARTESIAN_POINT('Ctrl Pts',(1.24643108191867,2.29785936479934,-7.3961093793232));
#116871=CARTESIAN_POINT('Ctrl Pts',(1.1697639772822,2.28571428612184,-7.40821518549939));
#116872=CARTESIAN_POINT('Ctrl Pts',(1.05893063938031,2.26815682586141,-7.42571587085398));
#116873=CARTESIAN_POINT('Ctrl Pts',(0.947423753831489,2.25046493734972,
-7.44077239346166));
#116874=CARTESIAN_POINT('Ctrl Pts',(0.835406138535195,2.23266407446841,
-7.45332788627282));
#116875=CARTESIAN_POINT('Ctrl Pts',(1.359217614,2.36225522,-7.121448411));
#116876=CARTESIAN_POINT('Ctrl Pts',(1.128445831,2.323743665,-7.16549409600001));
#116877=CARTESIAN_POINT('Ctrl Pts',(0.895306583,2.285714286,-7.194506663));
#116878=CARTESIAN_POINT('Ctrl Pts',(0.733443198,2.259311335,-7.214649441));
#116879=CARTESIAN_POINT('Ctrl Pts',(0.570837696,2.232664075,-7.227492257));
#116880=CARTESIAN_POINT('Ctrl Pts',(0.566864123208228,2.23201289883432,
-7.22780609548393));
#116881=CARTESIAN_POINT('Ctrl Pts',(0.562890550416455,2.23136172266864,
-7.22811993396787));
#116882=CARTESIAN_POINT('Ctrl Pts',(1.646935195,2.36225522,-7.316939556));
#116883=CARTESIAN_POINT('Ctrl Pts',(1.409828488,2.323743665,-7.370308779));
#116884=CARTESIAN_POINT('Ctrl Pts',(1.169763977,2.285714286,-7.408215186));
#116885=CARTESIAN_POINT('Ctrl Pts',(1.003092537,2.259311335,-7.434532759));
#116886=CARTESIAN_POINT('Ctrl Pts',(0.835406142,2.232664075,-7.453327886));
#116887=CARTESIAN_POINT('Ctrl Pts',(0.831308407984072,2.23201289883432,
-7.45378718045404));
#116888=CARTESIAN_POINT('Ctrl Pts',(0.827210673968144,2.23136172266864,
-7.45424647490808));
#116889=CARTESIAN_POINT('',(0.703121927779861,2.23266407357604,-7.340410070659));
#116890=CARTESIAN_POINT('Ctrl Pts',(0.57863326237553,2.23138000478158,-7.22687655198706));
#116891=CARTESIAN_POINT('Ctrl Pts',(0.574735479187765,2.23202203989079,
-7.22718440449353));
#116892=CARTESIAN_POINT('Ctrl Pts',(0.570837696,2.232664075,-7.227492257));
#116893=CARTESIAN_POINT('Ctrl Pts',(0.179489852,2.297126115,-7.258401471));
#116894=CARTESIAN_POINT('Ctrl Pts',(-0.212907412,2.362252267,-7.246873149));
#116895=CARTESIAN_POINT('Ctrl Pts',(0.35308299665963,2.23138000478158,-7.49168858409584));
#116896=CARTESIAN_POINT('Ctrl Pts',(0.349042531829815,2.23202203989079,
-7.49187464354792));
#116897=CARTESIAN_POINT('Ctrl Pts',(0.345002067,2.232664075,-7.492060703));
#116898=CARTESIAN_POINT('Ctrl Pts',(-0.060671395,2.297126115,-7.510741569));
#116899=CARTESIAN_POINT('Ctrl Pts',(-0.465990131,2.362252267,-7.485509548));
#116900=CARTESIAN_POINT('Ctrl Pts',(-0.208221607850005,2.36147458189157,
-7.24700929787493));
#116901=CARTESIAN_POINT('Ctrl Pts',(-0.209667279061951,2.35461431131095,
-7.2885891579842));
#116902=CARTESIAN_POINT('Ctrl Pts',(-0.211134518176119,2.34792816686656,
-7.33022331072456));
#116903=CARTESIAN_POINT('Ctrl Pts',(-0.214105126604883,2.33489257361319,
-7.41349191549236));
#116904=CARTESIAN_POINT('Ctrl Pts',(-0.21561023850716,2.32853549257574,
-7.4551751613142));
#116905=CARTESIAN_POINT('Ctrl Pts',(-0.217131939497084,2.32233405373809,
-7.49685625574536));
#116906=CARTESIAN_POINT('',(0.457919866879924,2.23266407264717,-7.35977648090965));
#116907=CARTESIAN_POINT('Ctrl Pts',(-0.203461038,2.36225522,-7.24714451400001));
#116908=CARTESIAN_POINT('Ctrl Pts',(-0.438306025,2.323743665,-7.240551323));
#116909=CARTESIAN_POINT('Ctrl Pts',(-0.672231452,2.285714286,-7.218767545));
#116910=CARTESIAN_POINT('Ctrl Pts',(-0.834640663,2.259311335,-7.203643554));
#116911=CARTESIAN_POINT('Ctrl Pts',(-0.996205363999999,2.232664075,-7.181230735));
#116912=CARTESIAN_POINT('Ctrl Pts',(-1.00015350285206,2.23201289883432,
-7.18068303540392));
#116913=CARTESIAN_POINT('Ctrl Pts',(-1.00410164170411,2.23136172266864,
-7.18013533580784));
#116914=CARTESIAN_POINT('Ctrl Pts',(0.035505048,2.36225522,-7.49991595900001));
#116915=CARTESIAN_POINT('Ctrl Pts',(-0.207531042,2.323743665,-7.501066506));
#116916=CARTESIAN_POINT('Ctrl Pts',(-0.450131734,2.285714286,-7.486479909));
#116917=CARTESIAN_POINT('Ctrl Pts',(-0.618563989,2.259311335,-7.476352759));
#116918=CARTESIAN_POINT('Ctrl Pts',(-0.786370366,2.232664075,-7.458660848));
#116919=CARTESIAN_POINT('Ctrl Pts',(-0.790471032002883,2.23201289883432,
-7.45822851271418));
#116920=CARTESIAN_POINT('Ctrl Pts',(-0.794571698005766,2.23136172266864,
-7.45779617742834));
#116921=CARTESIAN_POINT('',(-0.891287856244616,2.23266407357604,-7.31994579256607));
#116922=CARTESIAN_POINT('Ctrl Pts',(-0.988459695241115,2.23138000478158,
-7.18230524117258));
#116923=CARTESIAN_POINT('Ctrl Pts',(-0.992332529620557,2.23202203989079,
-7.18176798808629));
#116924=CARTESIAN_POINT('Ctrl Pts',(-0.996205364,2.232664075,-7.181230735));
#116925=CARTESIAN_POINT('Ctrl Pts',(-1.385048281,2.297126115,-7.12728909));
#116926=CARTESIAN_POINT('Ctrl Pts',(-1.765793266,2.362252267,-7.031676482));
#116927=CARTESIAN_POINT('Ctrl Pts',(-1.26566348041818,2.23138000478158,
-7.39243947503579));
#116928=CARTESIAN_POINT('Ctrl Pts',(-1.26964947870909,2.23202203989079,
-7.3917526040179));
#116929=CARTESIAN_POINT('Ctrl Pts',(-1.273635477,2.232664075,-7.391065733));
#116930=CARTESIAN_POINT('Ctrl Pts',(-1.673840353,2.297126115,-7.322102048));
#116931=CARTESIAN_POINT('Ctrl Pts',(-2.064258824,2.362252267,-7.210328391));
#116932=CARTESIAN_POINT('',(-1.27363548277204,2.23266407419429,-7.39106572986814));
#116933=CARTESIAN_POINT('',(-1.82365800664062,2.32233405365439,-7.27490697348646));
#116934=CARTESIAN_POINT('Origin',(0.0597124100100879,2.41067413317871,0.179937914551258));
#116935=CARTESIAN_POINT('Ctrl Pts',(-1.76124628115219,2.36147458186449,
-7.03281675718452));
#116936=CARTESIAN_POINT('Ctrl Pts',(-1.77159658621436,2.35461431668314,
-7.07311369487819));
#116937=CARTESIAN_POINT('Ctrl Pts',(-1.78197962485504,2.34792817786205,
-7.11345901463161));
#116938=CARTESIAN_POINT('Ctrl Pts',(-1.80278108757618,2.33489257408083,
-7.19414231772472));
#116939=CARTESIAN_POINT('Ctrl Pts',(-1.81321167554102,2.32853549357603,
-7.23452747417755));
#116940=CARTESIAN_POINT('Ctrl Pts',(-1.82365800496382,2.32233405369464,
-7.27490697382443));
#116941=CARTESIAN_POINT('',(-1.13492043497381,2.23266407264717,-7.28614823174549));
#116942=CARTESIAN_POINT('Origin',(2.73544208118093E-13,2.32340998500055,
1.10978934375616E-12));
#116943=CARTESIAN_POINT('',(-1.82568833581608,2.1430121312241,-7.27439771363291));
#116944=CARTESIAN_POINT('Origin',(0.06474963453826,2.01794105213501,0.175829002095066));
#116945=CARTESIAN_POINT('',(-2.37137706833043,2.23266407449123,-7.11523511726562));
#116946=CARTESIAN_POINT('Origin',(0.084081980906319,2.41052391280545,0.162842126679255));
#116947=CARTESIAN_POINT('Ctrl Pts',(-1.82365800778149,2.32233405321442,
-7.27490697333454));
#116948=CARTESIAN_POINT('Ctrl Pts',(-1.89919130811697,2.31006874160714,
-7.25597244811295));
#116949=CARTESIAN_POINT('Ctrl Pts',(-1.97431551001625,2.29785936478844,
-7.23588990102137));
#116950=CARTESIAN_POINT('Ctrl Pts',(-2.04897978584046,2.28571428607925,
-7.2146851515026));
#116951=CARTESIAN_POINT('Ctrl Pts',(-2.15691774703239,2.26815682575704,
-7.18403063233674));
#116952=CARTESIAN_POINT('Ctrl Pts',(-2.26444072465366,2.25046493734972,
-7.15087503667013));
#116953=CARTESIAN_POINT('Ctrl Pts',(-2.37137707325913,2.23266407446841,
-7.11523511779276));
#116954=CARTESIAN_POINT('Ctrl Pts',(-1.756626078,2.36225522,-7.033972194));
#116955=CARTESIAN_POINT('Ctrl Pts',(-1.984563179,2.323743665,-6.977048418));
#116956=CARTESIAN_POINT('Ctrl Pts',(-2.208336691,2.285714286,-6.905486881));
#116957=CARTESIAN_POINT('Ctrl Pts',(-2.363697654,2.259311335,-6.8558033));
#116958=CARTESIAN_POINT('Ctrl Pts',(-2.516666969,2.232664075,-6.79918284600001));
#116959=CARTESIAN_POINT('Ctrl Pts',(-2.52040506334849,2.23201289883432,
-6.7977992181848));
#116960=CARTESIAN_POINT('Ctrl Pts',(-2.52414315769698,2.23136172266864,
-6.79641559036959));
#116961=CARTESIAN_POINT('Ctrl Pts',(-1.577585275,2.36225522,-7.332204628));
#116962=CARTESIAN_POINT('Ctrl Pts',(-1.81518665,2.323743665,-7.2810827));
#116963=CARTESIAN_POINT('Ctrl Pts',(-2.048979786,2.285714286,-7.214685152));
#116964=CARTESIAN_POINT('Ctrl Pts',(-2.211297151,2.259311335,-7.16858681300001));
#116965=CARTESIAN_POINT('Ctrl Pts',(-2.37137707,2.232664075,-7.115235119));
#116966=CARTESIAN_POINT('Ctrl Pts',(-2.37528892539741,2.23201289883432,
-7.11393136951387));
#116967=CARTESIAN_POINT('Ctrl Pts',(-2.37920078079482,2.23136172266864,
-7.11262762002775));
#116968=CARTESIAN_POINT('',(-2.44402201117849,2.23266407357604,-6.9572089854233));
#116969=CARTESIAN_POINT('Ctrl Pts',(-2.5093333767475,2.23138000478158,-6.80189732065103));
#116970=CARTESIAN_POINT('Ctrl Pts',(-2.51300017287375,2.23202203989079,
-6.80054008332552));
#116971=CARTESIAN_POINT('Ctrl Pts',(-2.516666969,2.232664075,-6.799182846));
#116972=CARTESIAN_POINT('Ctrl Pts',(-2.884823095,2.297126115,-6.662912593));
#116973=CARTESIAN_POINT('Ctrl Pts',(-3.23611259,2.362252267,-6.487686437));
#116974=CARTESIAN_POINT('Ctrl Pts',(-2.82522894021175,2.23138000478158,
-6.94752811231027));
#116975=CARTESIAN_POINT('Ctrl Pts',(-2.82897409110587,2.23202203989079,
-6.94600042815513));
#116976=CARTESIAN_POINT('Ctrl Pts',(-2.832719242,2.232664075,-6.944472744));
#116977=CARTESIAN_POINT('Ctrl Pts',(-3.208742396,2.297126115,-6.791089174));
#116978=CARTESIAN_POINT('Ctrl Pts',(-3.566005068,2.362252267,-6.598000292));
#116979=CARTESIAN_POINT('',(-2.83271924697018,2.23266407419429,-6.94447273970029));
#116980=CARTESIAN_POINT('',(-3.34491185041081,2.32233405366361,-6.71279112679404));
#116981=CARTESIAN_POINT('Origin',(0.0969976335030265,2.4106740959476,0.162894538142772));
#116982=CARTESIAN_POINT('Ctrl Pts',(-3.23191703662375,2.36147458186189,
-6.48977752055159));
#116983=CARTESIAN_POINT('Ctrl Pts',(-3.25068803512464,2.354614306655,-6.52690738309182));
#116984=CARTESIAN_POINT('Ctrl Pts',(-3.26950140686306,2.34792815738699,
-6.56407746796472));
#116985=CARTESIAN_POINT('Ctrl Pts',(-3.30716101048175,2.33489257347995,
-6.63840262764445));
#116986=CARTESIAN_POINT('Ctrl Pts',(-3.32602935391116,2.32853549231932,
-6.67560133771195));
#116987=CARTESIAN_POINT('Ctrl Pts',(-3.34491184879149,2.32233405369777,
-6.71279112756188));
#116988=CARTESIAN_POINT('',(-2.67469311915078,2.23266407264717,-6.87182778968677));
#116989=CARTESIAN_POINT('Origin',(-1.81929124543068E-13,2.32340998499989,
-3.81205483845903E-13));
#116990=CARTESIAN_POINT('',(-3.34678523568675,2.14301213127624,-6.71185731238674));
#116991=CARTESIAN_POINT('Origin',(0.101033801869133,2.01794101580762,0.157798815744163));
#116992=CARTESIAN_POINT('',(-3.84550081497575,2.23266407449122,-6.43910890169064));
#116993=CARTESIAN_POINT('Origin',(0.117122493431832,2.4105239843923,0.140959894913686));
#116994=CARTESIAN_POINT('Ctrl Pts',(-3.34491185149413,2.32233405321711,
-6.71279112629689));
#116995=CARTESIAN_POINT('Ctrl Pts',(-3.41460886186971,2.31006874161239,
-6.67806185287211));
#116996=CARTESIAN_POINT('Ctrl Pts',(-3.48365954759103,2.29785936479251,
-6.64229934151317));
#116997=CARTESIAN_POINT('Ctrl Pts',(-3.55201981983207,2.28571428604147,
-6.60553973487858));
#116998=CARTESIAN_POINT('Ctrl Pts',(-3.65084443614975,2.26815682566445,
-6.5523984313499));
#116999=CARTESIAN_POINT('Ctrl Pts',(-3.74872611297771,2.25046493734972,
-6.49690373263539));
#117000=CARTESIAN_POINT('Ctrl Pts',(-3.84550081992341,2.23266407446841,
-6.43910890112039));
#117001=CARTESIAN_POINT('Ctrl Pts',(-3.227653236,2.36225522,-6.491899151));
#117002=CARTESIAN_POINT('Ctrl Pts',(-3.438024365,2.323743665,-6.387306483));
#117003=CARTESIAN_POINT('Ctrl Pts',(-3.641182561,2.285714286,-6.269313324));
#117004=CARTESIAN_POINT('Ctrl Pts',(-3.78223077,2.259311335,-6.187393303));
#117005=CARTESIAN_POINT('Ctrl Pts',(-3.919452023,2.232664075,-6.09921272300001));
#117006=CARTESIAN_POINT('Ctrl Pts',(-3.92280528368717,2.23201289883432,
-6.09705786385231));
#117007=CARTESIAN_POINT('Ctrl Pts',(-3.92615854437433,2.23136172266864,
-6.09490300470461));
#117008=CARTESIAN_POINT('Ctrl Pts',(-3.116909465,2.36225522,-6.821647557));
#117009=CARTESIAN_POINT('Ctrl Pts',(-3.337966148,2.323743665,-6.72064355999999));
#117010=CARTESIAN_POINT('Ctrl Pts',(-3.55201982,2.285714286,-6.605539735));
#117011=CARTESIAN_POINT('Ctrl Pts',(-3.700632515,2.259311335,-6.525625715));
#117012=CARTESIAN_POINT('Ctrl Pts',(-3.845500817,2.232664075,-6.439108903));
#117013=CARTESIAN_POINT('Ctrl Pts',(-3.84904094778363,2.23201289883432,
-6.43699470116816));
#117014=CARTESIAN_POINT('Ctrl Pts',(-3.85258107856726,2.23136172266864,
-6.43488049933635));
#117015=CARTESIAN_POINT('',(-3.88247641250146,2.23266407357604,-6.26916081764383));
#117016=CARTESIAN_POINT('Ctrl Pts',(-3.91287341787142,2.23138000478158,
-6.10344024028336));
#117017=CARTESIAN_POINT('Ctrl Pts',(-3.91616272043571,2.23202203989079,
-6.10132648164168));
#117018=CARTESIAN_POINT('Ctrl Pts',(-3.919452023,2.232664075,-6.09921272300001));
#117019=CARTESIAN_POINT('Ctrl Pts',(-4.249706787,2.297126115,-5.886985709));
#117020=CARTESIAN_POINT('Ctrl Pts',(-4.555114885,2.362252267,-5.640339386));
#117021=CARTESIAN_POINT('Ctrl Pts',(-4.25268983415697,2.23138000478158,
-6.17775805698345));
#117022=CARTESIAN_POINT('Ctrl Pts',(-4.25601901857848,2.23202203989079,
-6.17546099249173));
#117023=CARTESIAN_POINT('Ctrl Pts',(-4.259348203,2.232664075,-6.173163928));
#117024=CARTESIAN_POINT('Ctrl Pts',(-4.593607212,2.297126115,-5.942532517));
#117025=CARTESIAN_POINT('Ctrl Pts',(-4.901008879,2.362252267,-5.677157033));
#117026=CARTESIAN_POINT('',(-4.2593482069289,2.23266407419428,-6.17316392273257));
#117027=CARTESIAN_POINT('',(-4.70976133415161,2.32233405363239,-5.83679262770778));
#117028=CARTESIAN_POINT('Origin',(0.129747478483248,2.41067415754769,0.138234636497682));
#117029=CARTESIAN_POINT('Ctrl Pts',(-4.55146694246914,2.3614745818666,-5.64328350111219));
#117030=CARTESIAN_POINT('Ctrl Pts',(-4.57778088593664,2.3546143125077,-5.67551005075196));
#117031=CARTESIAN_POINT('Ctrl Pts',(-4.60414485515913,2.34792816933081,
-5.70776676917776));
#117032=CARTESIAN_POINT('Ctrl Pts',(-4.65690176272403,2.33489257255299,
-5.7722586097785));
#117033=CARTESIAN_POINT('Ctrl Pts',(-4.68332560212223,2.32853549046343,
-5.80453150350009));
#117034=CARTESIAN_POINT('Ctrl Pts',(-4.70976133268649,2.3223340536587,-5.83679262891339));
#117035=CARTESIAN_POINT('',(-4.08940012518944,2.23266407264717,-6.13618831737648));
#117036=CARTESIAN_POINT('Origin',(5.29090660172926E-14,2.32340998499989,
7.84962372879505E-14));
#117037=CARTESIAN_POINT('',(-4.71139017771449,2.14301213125108,-5.83547792273423));
#117038=CARTESIAN_POINT('Origin',(0.132593752782683,2.01794102669776,0.132390265305984));
#117039=CARTESIAN_POINT('',(-5.13981321874104,2.23266407449122,-5.46189711015753));
#117040=CARTESIAN_POINT('Origin',(0.144686138640672,2.41052395745531,0.112486115523932));
#117041=CARTESIAN_POINT('Ctrl Pts',(-4.70976133507838,2.32233405317635,
-5.83679262687341));
#117042=CARTESIAN_POINT('Ctrl Pts',(-4.77036310094747,2.31006874158962,
-5.78789250779538));
#117043=CARTESIAN_POINT('Ctrl Pts',(-4.83011153734743,2.29785936478343,
-5.73812224794854));
#117044=CARTESIAN_POINT('Ctrl Pts',(-4.88897135546675,2.28571428611673,
-5.68752662272347));
#117045=CARTESIAN_POINT('Ctrl Pts',(-4.97406169678273,2.2681568258489,-5.61438336118433));
#117046=CARTESIAN_POINT('Ctrl Pts',(-5.05772523537544,2.25046493734972,
-5.53914443058292));
#117047=CARTESIAN_POINT('Ctrl Pts',(-5.139813223451,2.23266407446841,-5.46189710853589));
#117048=CARTESIAN_POINT('Ctrl Pts',(-4.547758915,2.36225522,-5.64627212));
#117049=CARTESIAN_POINT('Ctrl Pts',(-4.730727352,2.323743665,-5.498901196));
#117050=CARTESIAN_POINT('Ctrl Pts',(-4.903770781,2.285714286,-5.339993645));
#117051=CARTESIAN_POINT('Ctrl Pts',(-5.023910978,2.259311335,-5.229667673));
#117052=CARTESIAN_POINT('Ctrl Pts',(-5.138967857,2.232664075,-5.114050192));
#117053=CARTESIAN_POINT('Ctrl Pts',(-5.14177948931427,2.23201289883432,
-5.11122486031624));
#117054=CARTESIAN_POINT('Ctrl Pts',(-5.14459112162854,2.23136172266864,
-5.10839952863248));
#117055=CARTESIAN_POINT('Ctrl Pts',(-4.510490432,2.36225522,-5.992117828));
#117056=CARTESIAN_POINT('Ctrl Pts',(-4.704666059,2.323743665,-5.845954596));
#117057=CARTESIAN_POINT('Ctrl Pts',(-4.888971356,2.285714286,-5.687526623));
#117058=CARTESIAN_POINT('Ctrl Pts',(-5.016930416,2.259311335,-5.577533611));
#117059=CARTESIAN_POINT('Ctrl Pts',(-5.139813221,2.232664075,-5.461897111));
#117060=CARTESIAN_POINT('Ctrl Pts',(-5.14281609460832,2.23201289883432,
-5.45907131455102));
#117061=CARTESIAN_POINT('Ctrl Pts',(-5.14581896821665,2.23136172266864,
-5.45624551810205));
#117062=CARTESIAN_POINT('',(-5.13939053267506,2.23266407357604,-5.28797365764722));
#117063=CARTESIAN_POINT('Ctrl Pts',(-5.13345184724536,2.23138000478158,
-5.11959307791208));
#117064=CARTESIAN_POINT('Ctrl Pts',(-5.13620985212268,2.23202203989079,
-5.11682163495604));
#117065=CARTESIAN_POINT('Ctrl Pts',(-5.138967857,2.232664075,-5.114050192));
#117066=CARTESIAN_POINT('Ctrl Pts',(-5.415878914,2.297126115,-4.835789916));
#117067=CARTESIAN_POINT('Ctrl Pts',(-5.66112507100001,2.362252267,-4.529256333));
#117068=CARTESIAN_POINT('Ctrl Pts',(-5.48129967805377,2.23138000478158,
-5.11912290128042));
#117069=CARTESIAN_POINT('Ctrl Pts',(-5.48405722702689,2.23202203989079,
-5.11616386464021));
#117070=CARTESIAN_POINT('Ctrl Pts',(-5.48681477600001,2.232664075,-5.113204828));
#117071=CARTESIAN_POINT('Ctrl Pts',(-5.763680059,2.297126115,-4.816109645));
#117072=CARTESIAN_POINT('Ctrl Pts',(-6.006846961,2.362252267,-4.49085622));
#117073=CARTESIAN_POINT('',(-5.48681477869489,2.23266407419428,-5.11320482201616));
#117074=CARTESIAN_POINT('',(-5.85438761178372,2.32233405365653,-4.68787219229255));
#117075=CARTESIAN_POINT('Origin',(0.156430345808302,2.41067413916276,0.107110851889194));
#117076=CARTESIAN_POINT('Ctrl Pts',(-5.65819531310717,2.36147458187234,
-4.5329158161281));
#117077=CARTESIAN_POINT('Ctrl Pts',(-5.6908218202369,2.35461430965226,-4.55873221783808));
#117078=CARTESIAN_POINT('Ctrl Pts',(-5.72350367110793,2.34792816349843,
-4.58456733051178));
#117079=CARTESIAN_POINT('Ctrl Pts',(-5.78889096359627,2.33489257215201,
-4.63621019074896));
#117080=CARTESIAN_POINT('Ctrl Pts',(-5.8216347488704,2.32853548963579,-4.66204821970733));
#117081=CARTESIAN_POINT('Ctrl Pts',(-5.85438761057469,2.3223340536835,-4.68787219383246));
#117082=CARTESIAN_POINT('',(-5.31289132665814,2.23266407264717,-5.11362749944603));
#117083=CARTESIAN_POINT('Origin',(-9.39786443110435E-13,2.32340998499933,
-5.47738937539677E-13));
#117084=CARTESIAN_POINT('',(-5.85569575168534,2.14301213125127,-4.68623807130231));
#117085=CARTESIAN_POINT('Origin',(0.157953816337484,2.01794102736107,0.100791350753756));
#117086=CARTESIAN_POINT('',(-6.19379366761472,2.23266407449123,-4.22929308165503));
#117087=CARTESIAN_POINT('Origin',(0.16548488433682,2.41052395892396,0.0787531823237286));
#117088=CARTESIAN_POINT('Ctrl Pts',(-5.85438761247407,2.32233405319692,
-4.68787219120225));
#117089=CARTESIAN_POINT('Ctrl Pts',(-5.90306046264052,2.31006874160582,
-4.62708774125359));
#117090=CARTESIAN_POINT('Ctrl Pts',(-5.95071287908218,2.29785936479246,
-4.56563693457481));
#117091=CARTESIAN_POINT('Ctrl Pts',(-5.99732002373333,2.28571428605796,
-4.50357108604458));
#117092=CARTESIAN_POINT('Ctrl Pts',(-6.06469736209479,2.26815682570485,
-4.41384596610625));
#117093=CARTESIAN_POINT('Ctrl Pts',(-6.130230746824,2.25046493734972,-4.32238089219941));
#117094=CARTESIAN_POINT('Ctrl Pts',(-6.19379367186398,2.23266407446841,
-4.22929307906654));
#117095=CARTESIAN_POINT('Ctrl Pts',(-5.655216442,2.36225522,-4.536631679));
#117096=CARTESIAN_POINT('Ctrl Pts',(-5.802226786,2.323743665,-4.3533734));
#117097=CARTESIAN_POINT('Ctrl Pts',(-5.93706413,2.285714286,-4.160981797));
#117098=CARTESIAN_POINT('Ctrl Pts',(-6.030678693,2.259311335,-4.027408594));
#117099=CARTESIAN_POINT('Ctrl Pts',(-6.118191265,2.232664075,-3.889760358));
#117100=CARTESIAN_POINT('Ctrl Pts',(-6.12032980010958,2.23201289883432,
-3.88639666317616));
#117101=CARTESIAN_POINT('Ctrl Pts',(-6.12246833521915,2.23136172266864,
-3.88303296835232));
#117102=CARTESIAN_POINT('Ctrl Pts',(-5.69316587900001,2.36225522,-4.88240333000001));
#117103=CARTESIAN_POINT('Ctrl Pts',(-5.851381014,2.323743665,-4.697915292));
#117104=CARTESIAN_POINT('Ctrl Pts',(-5.997320024,2.285714286,-4.503571086));
#117105=CARTESIAN_POINT('Ctrl Pts',(-6.09864222700001,2.259311335,-4.368642235));
#117106=CARTESIAN_POINT('Ctrl Pts',(-6.19379367,2.232664075,-4.229293082));
#117107=CARTESIAN_POINT('Ctrl Pts',(-6.19611887536115,2.23201289883432,
-4.22588782205426));
#117108=CARTESIAN_POINT('Ctrl Pts',(-6.1984440807223,2.23136172266864,-4.22248256210852));
#117109=CARTESIAN_POINT('',(-6.15599246264441,2.23266407357604,-4.05952672736318));
#117110=CARTESIAN_POINT('Ctrl Pts',(-6.11399577311955,2.23138000478158,
-3.89635943336084));
#117111=CARTESIAN_POINT('Ctrl Pts',(-6.11609351905978,2.23202203989079,
-3.89305989568042));
#117112=CARTESIAN_POINT('Ctrl Pts',(-6.118191265,2.232664075,-3.889760358));
#117113=CARTESIAN_POINT('Ctrl Pts',(-6.328810561,2.297126115,-3.558477961));
#117114=CARTESIAN_POINT('Ctrl Pts',(-6.50242734,2.362252267,-3.206390288));
#117115=CARTESIAN_POINT('Ctrl Pts',(-6.45361004080255,2.23138000478158,
-3.82112324805941));
#117116=CARTESIAN_POINT('Ctrl Pts',(-6.45566701440128,2.23202203989079,
-3.8176406005297));
#117117=CARTESIAN_POINT('Ctrl Pts',(-6.457723988,2.232664075,-3.814157953));
#117118=CARTESIAN_POINT('Ctrl Pts',(-6.664249632,2.297126115,-3.464490838));
#117119=CARTESIAN_POINT('Ctrl Pts',(-6.831811556,2.362252267,-3.094567962));
#117120=CARTESIAN_POINT('',(-6.45772398935623,2.23266407419428,-3.8141579465679));
#117121=CARTESIAN_POINT('',(-6.72526923157056,2.3223340536739,-3.31975206353202));
#117122=CARTESIAN_POINT('Origin',(0.175799019391143,2.41067416086851,0.0709788985909582));
#117123=CARTESIAN_POINT('Ctrl Pts',(-6.50035275888918,2.36147458185405,
-3.21059402588741));
#117124=CARTESIAN_POINT('Ctrl Pts',(-6.53776626144959,2.35461430567979,
-3.22879313047535));
#117125=CARTESIAN_POINT('Ctrl Pts',(-6.57523783952024,2.34792815538496,
-3.24699861286064));
#117126=CARTESIAN_POINT('Ctrl Pts',(-6.65019804501835,2.33489257396561,
-3.28337772900175));
#117127=CARTESIAN_POINT('Ctrl Pts',(-6.68773069966166,2.32853549328887,
-3.30157272760519));
#117128=CARTESIAN_POINT('Ctrl Pts',(-6.72526923074275,2.32233405371269,
-3.3197520650575));
#117129=CARTESIAN_POINT('',(-6.28795763415186,2.23266407264717,-3.85195914300908));
#117130=CARTESIAN_POINT('Origin',(-8.95550994473027E-13,2.32340998499911,
-4.43872369415566E-13));
#117131=CARTESIAN_POINT('',(-6.72619550060074,2.14301213124985,-3.31787493578972));
#117132=CARTESIAN_POINT('Origin',(0.175927995196032,2.01794103833251,0.064479450497496));
#117133=CARTESIAN_POINT('',(-6.95815920959667,2.23266407449123,-2.798932008156));
#117134=CARTESIAN_POINT('Origin',(0.178546055849216,2.41052401352776,0.0413378320593671));
#117135=CARTESIAN_POINT('Ctrl Pts',(-6.72526923217753,2.32233405323146,
-3.31975206253709));
#117136=CARTESIAN_POINT('Ctrl Pts',(-6.7597372782509,2.31006874161956,-3.24992549503813));
#117137=CARTESIAN_POINT('Ctrl Pts',(-6.79306550086175,2.29785936479525,
-3.1796675130989));
#117138=CARTESIAN_POINT('Ctrl Pts',(-6.82524067351545,2.28571428611621,
-3.10903357124698));
#117139=CARTESIAN_POINT('Ctrl Pts',(-6.87175451781382,2.26815682584759,
-3.00692203889695));
#117140=CARTESIAN_POINT('Ctrl Pts',(-6.91609348176508,2.25046493734972,
-2.90350762661701));
#117141=CARTESIAN_POINT('Ctrl Pts',(-6.95815921318946,2.23266407446841,
-2.79893200473371));
#117142=CARTESIAN_POINT('Ctrl Pts',(-6.498242333,2.36225522,-3.214863384));
#117143=CARTESIAN_POINT('Ctrl Pts',(-6.602420544,2.323743665,-3.004286703));
#117144=CARTESIAN_POINT('Ctrl Pts',(-6.692746959,2.285714286,-2.787407065));
#117145=CARTESIAN_POINT('Ctrl Pts',(-6.755458575,2.259311335,-2.636832366));
#117146=CARTESIAN_POINT('Ctrl Pts',(-6.81133485,2.232664075,-2.483589653));
#117147=CARTESIAN_POINT('Ctrl Pts',(-6.81270029239472,2.23201289883432,
-2.47984487765461));
#117148=CARTESIAN_POINT('Ctrl Pts',(-6.81406573478944,2.23136172266864,
-2.47610010230922));
#117149=CARTESIAN_POINT('Ctrl Pts',(-6.609635218,2.36225522,-3.544393078));
#117150=CARTESIAN_POINT('Ctrl Pts',(-6.724491896,2.323743665,-3.330206691));
#117151=CARTESIAN_POINT('Ctrl Pts',(-6.825240674,2.285714286,-3.109033571));
#117152=CARTESIAN_POINT('Ctrl Pts',(-6.895188305,2.259311335,-2.955478003));
#117153=CARTESIAN_POINT('Ctrl Pts',(-6.958159212,2.232664075,-2.798932008));
#117154=CARTESIAN_POINT('Ctrl Pts',(-6.95969802513763,2.23201289883432,
-2.79510651071521));
#117155=CARTESIAN_POINT('Ctrl Pts',(-6.96123683827525,2.23136172266864,
-2.79128101343042));
#117156=CARTESIAN_POINT('',(-6.88474702784079,2.23266407357604,-2.64126083873485));
#117157=CARTESIAN_POINT('Ctrl Pts',(-6.80865605252724,2.23138000478158,
-2.49093635239381));
#117158=CARTESIAN_POINT('Ctrl Pts',(-6.80999545126362,2.23202203989079,
-2.4872630026969));
#117159=CARTESIAN_POINT('Ctrl Pts',(-6.81133485,2.232664075,-2.483589653));
#117160=CARTESIAN_POINT('Ctrl Pts',(-6.945814061,2.297126115,-2.114775531));
#117161=CARTESIAN_POINT('Ctrl Pts',(-7.039683335,2.362252267,-1.733596997));
#117162=CARTESIAN_POINT('Ctrl Pts',(-7.12415677113848,2.23138000478158,
-2.3444521183563));
#117163=CARTESIAN_POINT('Ctrl Pts',(-7.12541698756924,2.23202203989079,
-2.34060870467815));
#117164=CARTESIAN_POINT('Ctrl Pts',(-7.126677204,2.232664075,-2.336765291));
#117165=CARTESIAN_POINT('Ctrl Pts',(-7.2532063,2.297126115,-1.950876291));
#117166=CARTESIAN_POINT('Ctrl Pts',(-7.337328235,2.362252267,-1.553581145));
#117167=CARTESIAN_POINT('',(-7.12667720394274,2.23266407419429,-2.33676528442554));
#117168=CARTESIAN_POINT('',(-7.28168473677128,2.32233405368831,-1.79640401797926));
#117169=CARTESIAN_POINT('Origin',(0.186947018560235,2.41067412192715,0.0315277854019649));
#117170=CARTESIAN_POINT('Ctrl Pts',(-7.03856093580355,2.36147458185582,
-1.73814842744207));
#117171=CARTESIAN_POINT('Ctrl Pts',(-7.07901198255375,2.35461430875897,
-1.74787924556015));
#117172=CARTESIAN_POINT('Ctrl Pts',(-7.11952111529154,2.34792816168966,
-1.75760380725075));
#117173=CARTESIAN_POINT('Ctrl Pts',(-7.2005492650654,2.3348925741771,-1.777018180687));
#117174=CARTESIAN_POINT('Ctrl Pts',(-7.24111581222357,2.32853549374325,
-1.78671937873909));
#117175=CARTESIAN_POINT('Ctrl Pts',(-7.28168473628263,2.32233405372934,
-1.79640401961946));
#117176=CARTESIAN_POINT('',(-6.96900603178777,2.23266407264717,-2.41017745815618));
#117177=CARTESIAN_POINT('Origin',(1.56515425620007E-12,2.32340998500011,
3.71989765379777E-13));
#117178=CARTESIAN_POINT('',(-7.28218582274825,2.14301213123374,-1.79437165622682));
#117179=CARTESIAN_POINT('Origin',(0.185675943570865,2.01794100957163,0.0251525977595751));
#117180=CARTESIAN_POINT('',(-7.39716895968944,2.23266407449122,-1.23769598468383));
#117181=CARTESIAN_POINT('Origin',(0.183257870512463,2.41052394691905,0.00198920916004167));
#117182=CARTESIAN_POINT('Ctrl Pts',(-7.28168473717622,2.32233405324734,
-1.79640401689558));
#117183=CARTESIAN_POINT('Ctrl Pts',(-7.30033629147207,2.3100687416291,-1.72080034473311));
#117184=CARTESIAN_POINT('Ctrl Pts',(-7.31778192934196,2.29785936479937,
-1.6450203727789));
#117185=CARTESIAN_POINT('Ctrl Pts',(-7.33402065462615,2.28571428606948,
-1.56912110203));
#117186=CARTESIAN_POINT('Ctrl Pts',(-7.35749606995706,2.26815682573308,
-1.45939777797517));
#117187=CARTESIAN_POINT('Ctrl Pts',(-7.3785673717505,2.25046493734972,-1.34886957116084));
#117188=CARTESIAN_POINT('Ctrl Pts',(-7.39716896245992,2.23266407446841,
-1.23769598055493));
#117189=CARTESIAN_POINT('Ctrl Pts',(-7.037417636,2.36225522,-1.742771649));
#117190=CARTESIAN_POINT('Ctrl Pts',(-7.09389245600001,2.323743665,-1.514722898));
#117191=CARTESIAN_POINT('Ctrl Pts',(-7.135484378,2.285714286,-1.283496277));
#117192=CARTESIAN_POINT('Ctrl Pts',(-7.164360722,2.259311335,-1.122960787));
#117193=CARTESIAN_POINT('Ctrl Pts',(-7.185987987,2.232664075,-0.961289056000001));
#117194=CARTESIAN_POINT('Ctrl Pts',(-7.18651649009927,2.23201289883432,
-0.957338301667589));
#117195=CARTESIAN_POINT('Ctrl Pts',(-7.18704499319853,2.23136172266864,
-0.953387547335178));
#117196=CARTESIAN_POINT('Ctrl Pts',(-7.21704536000001,2.36225522,-2.040650945));
#117197=CARTESIAN_POINT('Ctrl Pts',(-7.283173011,2.323743665,-1.806781326));
#117198=CARTESIAN_POINT('Ctrl Pts',(-7.334020655,2.285714286,-1.569121102));
#117199=CARTESIAN_POINT('Ctrl Pts',(-7.36932304100001,2.259311335,-1.404118904));
#117200=CARTESIAN_POINT('Ctrl Pts',(-7.397168962,2.232664075,-1.237695984));
#117201=CARTESIAN_POINT('Ctrl Pts',(-7.39784942971288,2.23201289883432,
-1.23362912538387));
#117202=CARTESIAN_POINT('Ctrl Pts',(-7.39852989742575,2.23136172266864,
-1.22956226676773));
#117203=CARTESIAN_POINT('',(-7.2915784731849,2.23266407357604,-1.09949252872145));
#117204=CARTESIAN_POINT('Ctrl Pts',(-7.18495114151865,2.23138000478158,
-0.969039855917186));
#117205=CARTESIAN_POINT('Ctrl Pts',(-7.18546956425932,2.23202203989079,
-0.965164455958594));
#117206=CARTESIAN_POINT('Ctrl Pts',(-7.18598798700001,2.232664075,-0.961289056));
#117207=CARTESIAN_POINT('Ctrl Pts',(-7.238039015,2.297126115,-0.572188548));
#117208=CARTESIAN_POINT('Ctrl Pts',(-7.24777156,2.362252267,-0.179742638));
#117209=CARTESIAN_POINT('Ctrl Pts',(-7.46158584913562,2.23138000478158,
-0.758157013164344));
#117210=CARTESIAN_POINT('Ctrl Pts',(-7.46199038206781,2.23202203989079,
-0.754132547082172));
#117211=CARTESIAN_POINT('Ctrl Pts',(-7.462394915,2.232664075,-0.750108081));
#117212=CARTESIAN_POINT('Ctrl Pts',(-7.503011102,2.297126115,-0.346040936));
#117213=CARTESIAN_POINT('Ctrl Pts',(-7.499759601,2.362252267,0.0600494));
#117214=CARTESIAN_POINT('',(-7.46239491352179,2.23266407419428,-0.750108074610252));
#117215=CARTESIAN_POINT('',(-7.4976167565496,2.32233405366971,-0.189058116750282));
#117216=CARTESIAN_POINT('Origin',(0.189354078892694,2.41067411514136,-0.00939739047842211));
#117217=CARTESIAN_POINT('Ctrl Pts',(-7.24765382489752,2.36147458195797,
-0.184428940551477));
#117218=CARTESIAN_POINT('Ctrl Pts',(-7.2892509864714,2.35461430889961,-0.185236478159344));
#117219=CARTESIAN_POINT('Ctrl Pts',(-7.33090353101137,2.34792816187836,
-0.18602541882174));
#117220=CARTESIAN_POINT('Ctrl Pts',(-7.41421080436065,2.3348925742867,-0.187567237801838));
#117221=CARTESIAN_POINT('Ctrl Pts',(-7.45591439820413,2.32853549395716,
-0.188321018621582));
#117222=CARTESIAN_POINT('Ctrl Pts',(-7.49761675641736,2.32233405371167,
-0.189058118439435));
#117223=CARTESIAN_POINT('',(-7.32419145269983,2.23266407264717,-0.855698553950613));
#117224=CARTESIAN_POINT('Origin',(1.34441069388203E-14,2.32340998499944,
7.28312809367138E-14));
#117225=CARTESIAN_POINT('',(-7.49766922989768,2.14301213117642,-0.186965551736699));
#117226=CARTESIAN_POINT('Origin',(0.186742279180522,2.01794106467577,-0.0153502760989665));
#117227=CARTESIAN_POINT('',(-7.49029531088826,2.23266407449123,0.381413326840851));
#117228=CARTESIAN_POINT('Origin',(0.179400584072913,2.41052393661623,-0.037452316932809));
#117229=CARTESIAN_POINT('Ctrl Pts',(-7.49761675672826,2.32233405323064,
-0.189058115616846));
#117230=CARTESIAN_POINT('Ctrl Pts',(-7.49957969341663,2.31006874161717,
-0.111212482487324));
#117231=CARTESIAN_POINT('Ctrl Pts',(-7.50032700817362,2.29785936479299,
-0.0334539078254175));
#117232=CARTESIAN_POINT('Ctrl Pts',(-7.49986998160248,2.28571428605214,
0.044161726036502));
#117233=CARTESIAN_POINT('Ctrl Pts',(-7.49920928364054,2.26815682569059,
0.156366300485565));
#117234=CARTESIAN_POINT('Ctrl Pts',(-7.49602765287769,2.25046493734972,
0.268840125821957));
#117235=CARTESIAN_POINT('Ctrl Pts',(-7.49029531270869,2.23266407446841,
0.381413331463295));
#117236=CARTESIAN_POINT('Ctrl Pts',(-7.247531111,2.36225522,-0.189189849));
#117237=CARTESIAN_POINT('Ctrl Pts',(-7.253661841,2.323743665,0.045667665));
#117238=CARTESIAN_POINT('Ctrl Pts',(-7.244574478,2.285714286,0.28042937));
#117239=CARTESIAN_POINT('Ctrl Pts',(-7.238265325,2.259311335,0.443419191));
#117240=CARTESIAN_POINT('Ctrl Pts',(-7.224632313,2.232664075,0.605960349000001));
#117241=CARTESIAN_POINT('Ctrl Pts',(-7.22429916458321,2.23201289883432,
0.609932349424512));
#117242=CARTESIAN_POINT('Ctrl Pts',(-7.22396601616642,2.23136172266864,
0.613904349849024));
#117243=CARTESIAN_POINT('Ctrl Pts',(-7.48699448200001,2.36225522,-0.441490242));
#117244=CARTESIAN_POINT('Ctrl Pts',(-7.50130105,2.323743665,-0.198872874));
#117245=CARTESIAN_POINT('Ctrl Pts',(-7.499869982,2.285714286,0.044161726));
#117246=CARTESIAN_POINT('Ctrl Pts',(-7.498876423,2.259311335,0.212895234));
#117247=CARTESIAN_POINT('Ctrl Pts',(-7.490295313,2.232664075,0.381413328));
#117248=CARTESIAN_POINT('Ctrl Pts',(-7.49008561735748,2.23201289883432,
0.385531386153037));
#117249=CARTESIAN_POINT('Ctrl Pts',(-7.48987592171496,2.23136172266864,
0.389649444306074));
#117250=CARTESIAN_POINT('',(-7.3574638135905,2.23266407357604,0.493686829699741));
#117251=CARTESIAN_POINT('Ctrl Pts',(-7.22528590126796,2.23138000478158,
0.598167867343195));
#117252=CARTESIAN_POINT('Ctrl Pts',(-7.22495910713398,2.23202203989079,
0.602064108171597));
#117253=CARTESIAN_POINT('Ctrl Pts',(-7.224632313,2.232664075,0.605960349000001));
#117254=CARTESIAN_POINT('Ctrl Pts',(-7.191821309,2.297126115,0.997153336));
#117255=CARTESIAN_POINT('Ctrl Pts',(-7.116962042,2.362252267,1.382516288));
#117256=CARTESIAN_POINT('Ctrl Pts',(-7.45011946511826,2.23138000478158,
0.86358867113768));
#117257=CARTESIAN_POINT('Ctrl Pts',(-7.44964939905913,2.23202203989079,
0.867606010068841));
#117258=CARTESIAN_POINT('Ctrl Pts',(-7.449179333,2.232664075,0.871623349000001));
#117259=CARTESIAN_POINT('Ctrl Pts',(-7.401983445,2.297126115,1.274974909));
#117260=CARTESIAN_POINT('Ctrl Pts',(-7.311510543,2.362252267,1.670872101));
#117261=CARTESIAN_POINT('',(-7.4491793301853,2.23266407419428,0.871623354933439));
#117262=CARTESIAN_POINT('',(-7.36296854853005,2.32233405328145,1.42712793824915));
#117263=CARTESIAN_POINT('Origin',(0.182906554548377,2.41067414117802,-0.0498831559296685));
#117264=CARTESIAN_POINT('Ctrl Pts',(-7.11785447610388,2.36147458187397,
1.37791423853736));
#117265=CARTESIAN_POINT('Ctrl Pts',(-7.15865271725039,2.35461430863267,
1.3860677412664));
#117266=CARTESIAN_POINT('Ctrl Pts',(-7.1995010489045,2.34792816140926,1.39425131177284));
#117267=CARTESIAN_POINT('Ctrl Pts',(-7.28119202925304,2.33489258355776,
1.41065412866113));
#117268=CARTESIAN_POINT('Ctrl Pts',(-7.32208259018484,2.32853551289289,
1.41888299719396));
#117269=CARTESIAN_POINT('Ctrl Pts',(-7.36296855028178,2.32233405367328,
1.42712792985716));
#117270=CARTESIAN_POINT('',(-7.3369058215324,2.23266407264717,0.738791863574644));
#117271=CARTESIAN_POINT('Ctrl Pts',(-7.118758086,2.36225522,1.373238257));
#117272=CARTESIAN_POINT('Ctrl Pts',(-7.07425806000001,2.323743665,1.60392286));
#117273=CARTESIAN_POINT('Ctrl Pts',(-7.014916327,2.285714286,1.831242452));
#117274=CARTESIAN_POINT('Ctrl Pts',(-6.973716685,2.259311335,1.98906538));
#117275=CARTESIAN_POINT('Ctrl Pts',(-6.925460861,2.232664075,2.144875721));
#117276=CARTESIAN_POINT('Ctrl Pts',(-6.92428163872934,2.23201289883432,
2.1486832411888));
#117277=CARTESIAN_POINT('Ctrl Pts',(-6.92310241645868,2.23136172266864,
2.15249076137759));
#117278=CARTESIAN_POINT('Ctrl Pts',(-7.406860063,2.36225522,1.178314054));
#117279=CARTESIAN_POINT('Ctrl Pts',(-7.368676589,2.323743665,1.418334652));
#117280=CARTESIAN_POINT('Ctrl Pts',(-7.315033724,2.285714286,1.655379601));
#117281=CARTESIAN_POINT('Ctrl Pts',(-7.277790677,2.259311335,1.819954627));
#117282=CARTESIAN_POINT('Ctrl Pts',(-7.23318378,2.232664075,1.982688177));
#117283=CARTESIAN_POINT('Ctrl Pts',(-7.23209372615764,2.23201289883432,
1.98666487888668));
#117284=CARTESIAN_POINT('Ctrl Pts',(-7.23100367231527,2.23136172266864,
1.99064158077337));
#117285=CARTESIAN_POINT('',(-7.23318377818739,2.23266407449123,1.98268817541319));
#117286=CARTESIAN_POINT('Ctrl Pts',(-7.36296854667059,2.3223340510831,1.42712794630432));
#117287=CARTESIAN_POINT('Ctrl Pts',(-7.34815108198387,2.31006874017642,
1.5035755606298));
#117288=CARTESIAN_POINT('Ctrl Pts',(-7.33216513098452,2.29785936406956,
1.57967682912431));
#117289=CARTESIAN_POINT('Ctrl Pts',(-7.31503372343977,2.28571428610238,
1.65537960077473));
#117290=CARTESIAN_POINT('Ctrl Pts',(-7.29026780498927,2.26815682581373,
1.76481886348275));
#117291=CARTESIAN_POINT('Ctrl Pts',(-7.26298201160635,2.25046493734972,
1.87397915710076));
#117292=CARTESIAN_POINT('Ctrl Pts',(-7.23318377897099,2.23266407446841,
1.9826881803197));
#117293=CARTESIAN_POINT('',(-7.07932232296849,2.23266407357604,2.06378194053243));
#117294=CARTESIAN_POINT('Origin',(-9.98333360424652E-13,2.323409985,1.0993810029003E-13));
#117295=CARTESIAN_POINT('',(-7.36256995669525,2.14301213123928,1.4291828538933));
#117296=CARTESIAN_POINT('Origin',(0.179076531732111,2.01794103526846,-0.0551354734157353));
#117297=CARTESIAN_POINT('Origin',(0.167155057818781,2.41052400122714,-0.075142510148061));
#117298=CARTESIAN_POINT('Ctrl Pts',(-6.92777432193795,2.23138000478158,
2.13740592539923));
#117299=CARTESIAN_POINT('Ctrl Pts',(-6.92661759146898,2.23202203989079,
2.14114082319961));
#117300=CARTESIAN_POINT('Ctrl Pts',(-6.925460861,2.232664075,2.144875721));
#117301=CARTESIAN_POINT('Ctrl Pts',(-6.809322032,2.297126115,2.519869437));
#117302=CARTESIAN_POINT('Ctrl Pts',(-6.65337129,2.362252267,2.880130289));
#117303=CARTESIAN_POINT('Ctrl Pts',(-7.0902937755932,2.23138000478158,2.44495390907349));
#117304=CARTESIAN_POINT('Ctrl Pts',(-7.0889710902966,2.23202203989079,2.44877627453674));
#117305=CARTESIAN_POINT('Ctrl Pts',(-7.08764840500001,2.232664075,2.45259864));
#117306=CARTESIAN_POINT('Ctrl Pts',(-6.95484726800001,2.297126115,2.836374343));
#117307=CARTESIAN_POINT('Ctrl Pts',(-6.781383379,2.362252267,3.20356668));
#117308=CARTESIAN_POINT('',(-7.08764840097537,2.23266407419428,2.45259864517374));
#117309=CARTESIAN_POINT('',(-7.0065546284336,2.23266407264717,2.29873719441841));
#117310=CARTESIAN_POINT('',(-6.88403611738364,2.32233405365637,2.97658306401144));
#117311=CARTESIAN_POINT('Origin',(0.167907100873431,2.41067411058327,-0.0880364936196407));
#117312=CARTESIAN_POINT('Ctrl Pts',(-6.65523216405864,2.36147458188244,
2.87582767986542));
#117313=CARTESIAN_POINT('Ctrl Pts',(-6.69332378753527,2.35461431140157,
2.89256096716532));
#117314=CARTESIAN_POINT('Ctrl Pts',(-6.73145786438581,2.34792816706396,
2.90933438625966));
#117315=CARTESIAN_POINT('Ctrl Pts',(-6.8077129334402,2.33489257223886,2.94291490396888));
#117316=CARTESIAN_POINT('Ctrl Pts',(-6.84587860805331,2.32853548981077,
2.95974168147538));
#117317=CARTESIAN_POINT('Ctrl Pts',(-6.88403611817317,2.32233405368326,
2.9765830622325));
#117318=CARTESIAN_POINT('Origin',(3.17454396103756E-13,2.323409985,-1.94289029309402E-13));
#117319=CARTESIAN_POINT('',(-6.63785661058304,2.23266407449122,3.4912547290495));
#117320=CARTESIAN_POINT('Ctrl Pts',(-6.88403611677099,2.32233405319557,
2.97658306513664));
#117321=CARTESIAN_POINT('Ctrl Pts',(-6.85313109707468,2.31006874160445,
3.0480580637289));
#117322=CARTESIAN_POINT('Ctrl Pts',(-6.82115936347794,2.29785936479146,
3.11894362395074));
#117323=CARTESIAN_POINT('Ctrl Pts',(-6.78815461857248,2.28571428603294,
3.189193764977));
#117324=CARTESIAN_POINT('Ctrl Pts',(-6.74044150717939,2.26815682564355,
3.29075045918057));
#117325=CARTESIAN_POINT('Ctrl Pts',(-6.69032740376249,2.25046493734972,
3.39149300637366));
#117326=CARTESIAN_POINT('Ctrl Pts',(-6.63785661028138,2.23266407446841,
3.4912547340209));
#117327=CARTESIAN_POINT('',(-6.88320509555524,2.14301213128533,2.97850425752067));
#117328=CARTESIAN_POINT('Origin',(0.163037348640993,2.01794103639389,-0.0923426108204922));
#117329=CARTESIAN_POINT('Origin',(0.147094092923629,2.41052394262412,-0.109319328977406));
#117330=CARTESIAN_POINT('Ctrl Pts',(-6.657119845,2.36225522,2.87145527));
#117331=CARTESIAN_POINT('Ctrl Pts',(-6.564069834,2.323743665,3.087180404));
#117332=CARTESIAN_POINT('Ctrl Pts',(-6.457248486,2.285714286,3.296428672));
#117333=CARTESIAN_POINT('Ctrl Pts',(-6.383084804,2.259311335,3.441705082));
#117334=CARTESIAN_POINT('Ctrl Pts',(-6.30246255700001,2.232664075,3.583499089));
#117335=CARTESIAN_POINT('Ctrl Pts',(-6.30049240000562,2.23201289883432,
3.58696409357439));
#117336=CARTESIAN_POINT('Ctrl Pts',(-6.29852224301123,2.23136172266863,
3.59042909814879));
#117337=CARTESIAN_POINT('Ctrl Pts',(-6.9803891,2.36225522,2.743021695));
#117338=CARTESIAN_POINT('Ctrl Pts',(-6.891501001,2.323743665,2.969222426));
#117339=CARTESIAN_POINT('Ctrl Pts',(-6.788154619,2.285714286,3.189193765));
#117340=CARTESIAN_POINT('Ctrl Pts',(-6.716403528,2.259311335,3.341914965));
#117341=CARTESIAN_POINT('Ctrl Pts',(-6.637856612,2.232664075,3.491254731));
#117342=CARTESIAN_POINT('Ctrl Pts',(-6.63593716964131,2.23201289883432,
3.49490413045825));
#117343=CARTESIAN_POINT('Ctrl Pts',(-6.63401772728261,2.23136172266864,
3.4985535299165));
#117344=CARTESIAN_POINT('',(-6.47015958873108,2.23266407357604,3.53737690226101));
#117345=CARTESIAN_POINT('Ctrl Pts',(-6.30632771577688,2.23138000478159,
3.5767012587878));
#117346=CARTESIAN_POINT('Ctrl Pts',(-6.30439513638845,2.23202203989079,
3.5801001738939));
#117347=CARTESIAN_POINT('Ctrl Pts',(-6.302462557,2.232664075,3.583499089));
#117348=CARTESIAN_POINT('Ctrl Pts',(-6.108426424,2.297126115,3.924759245));
#117349=CARTESIAN_POINT('Ctrl Pts',(-5.87867629,2.362252267,4.243072598));
#117350=CARTESIAN_POINT('Ctrl Pts',(-6.39893382949064,2.23138000478159,
3.91199581910429));
#117351=CARTESIAN_POINT('Ctrl Pts',(-6.39682037224532,2.23202203989079,
3.91544448155215));
#117352=CARTESIAN_POINT('Ctrl Pts',(-6.394706915,2.232664075,3.918893144));
#117353=CARTESIAN_POINT('Ctrl Pts',(-6.182510162,2.297126115,4.265148066));
#117354=CARTESIAN_POINT('Ctrl Pts',(-5.934166264,2.362252267,4.586466041));
#117355=CARTESIAN_POINT('',(-6.39470690994674,2.23266407419309,3.91889314820226));
#117356=CARTESIAN_POINT('',(-6.08321380637901,2.32233405369499,4.38685648066802));
#117357=CARTESIAN_POINT('Origin',(0.145056308722421,2.41067415180002,-0.12207334860511));
#117358=CARTESIAN_POINT('Ctrl Pts',(-5.88141859146556,2.361474581931,4.23927061465615));
#117359=CARTESIAN_POINT('Ctrl Pts',(-5.91502250640472,2.35461430846379,
4.26380127089592));
#117360=CARTESIAN_POINT('Ctrl Pts',(-5.94865925730689,2.34792816100449,
4.28838024850817));
#117361=CARTESIAN_POINT('Ctrl Pts',(-6.01591266561634,2.3348925741105,4.33756822829429));
#117362=CARTESIAN_POINT('Ctrl Pts',(-6.04956877750614,2.32853549356583,
4.36220608912047));
#117363=CARTESIAN_POINT('Ctrl Pts',(-6.08321380732606,2.32233405373527,
4.38685647922582));
#117364=CARTESIAN_POINT('',(-6.3485847285369,2.23266407264357,3.75119612913068));
#117365=CARTESIAN_POINT('Origin',(5.3256010712488E-13,2.32340998499967,
-3.86843335142828E-13));
#117366=CARTESIAN_POINT('',(-6.0819892141391,2.143012131239,4.38855411225098));
#117367=CARTESIAN_POINT('Origin',(0.139374592124883,2.01794105755577,-0.125231830788222));
#117368=CARTESIAN_POINT('',(-5.73215064603916,2.23266407449122,4.83657409078815));
#117369=CARTESIAN_POINT('Origin',(0.120154476291418,2.41052397133765,-0.138384219056065));
#117370=CARTESIAN_POINT('Ctrl Pts',(-6.08321380579988,2.32233405325243,
4.38685648167792));
#117371=CARTESIAN_POINT('Ctrl Pts',(-6.0376663161811,2.31006874163299,4.45001676899957));
#117372=CARTESIAN_POINT('Ctrl Pts',(-5.99120376380507,2.29785936480149,
4.51237208663772));
#117373=CARTESIAN_POINT('Ctrl Pts',(-5.94386894792437,2.28571428605536,
4.57388477374788));
#117374=CARTESIAN_POINT('Ctrl Pts',(-5.87543965642865,2.26815682569848,
4.66281021972723));
#117375=CARTESIAN_POINT('Ctrl Pts',(-5.8048405226744,2.25046493734972,4.75042441136098));
#117376=CARTESIAN_POINT('Ctrl Pts',(-5.73215064467174,2.23266407446841,
4.83657409558084));
#117377=CARTESIAN_POINT('Ctrl Pts',(-5.884202079,2.36225522,4.235406225));
#117378=CARTESIAN_POINT('Ctrl Pts',(-5.746952999,2.323743665,4.426084824));
#117379=CARTESIAN_POINT('Ctrl Pts',(-5.597646882,2.285714286,4.607477551));
#117380=CARTESIAN_POINT('Ctrl Pts',(-5.493986972,2.259311335,4.73341448));
#117381=CARTESIAN_POINT('Ctrl Pts',(-5.384768108,2.232664075,4.854562022));
#117382=CARTESIAN_POINT('Ctrl Pts',(-5.38209913861705,2.23201289883432,
4.857522491177));
#117383=CARTESIAN_POINT('Ctrl Pts',(-5.37943016923408,2.23136172266864,
4.860482960354));
#117384=CARTESIAN_POINT('Ctrl Pts',(-6.2275229,2.36225522,4.17946869));
#117385=CARTESIAN_POINT('Ctrl Pts',(-6.092086485,2.323743665,4.38127266));
#117386=CARTESIAN_POINT('Ctrl Pts',(-5.943868948,2.285714286,4.573884774));
#117387=CARTESIAN_POINT('Ctrl Pts',(-5.840964815,2.259311335,4.707611073));
#117388=CARTESIAN_POINT('Ctrl Pts',(-5.732150647,2.232664075,4.836574093));
#117389=CARTESIAN_POINT('Ctrl Pts',(-5.72949156712874,2.23201289883432,
4.83972554815443));
#117390=CARTESIAN_POINT('Ctrl Pts',(-5.72683248725748,2.23136172266864,
4.84287700330887));
#117391=CARTESIAN_POINT('',(-5.55845938329581,2.23266407357604,4.84556805085149));
#117392=CARTESIAN_POINT('Ctrl Pts',(-5.39000423404587,2.23138000478158,
4.8487540161696));
#117393=CARTESIAN_POINT('Ctrl Pts',(-5.38738617102294,2.23202203989079,
4.85165801908481));
#117394=CARTESIAN_POINT('Ctrl Pts',(-5.384768108,2.232664075,4.854562022));
#117395=CARTESIAN_POINT('Ctrl Pts',(-5.121907587,2.297126115,5.146131672));
#117396=CARTESIAN_POINT('Ctrl Pts',(-4.829100921,2.362252267,5.407613549));
#117397=CARTESIAN_POINT('Ctrl Pts',(-5.40836684853112,2.23138000478158,
5.19611715339498));
#117398=CARTESIAN_POINT('Ctrl Pts',(-5.40556144226556,2.23202203989079,
5.19903085719749));
#117399=CARTESIAN_POINT('Ctrl Pts',(-5.402756036,2.232664075,5.201944561));
#117400=CARTESIAN_POINT('Ctrl Pts',(-5.121085753,2.297126115,5.49448820600001));
#117401=CARTESIAN_POINT('Ctrl Pts',(-4.809474131,2.362252267,5.754907348));
#117402=CARTESIAN_POINT('',(-5.40275603017245,2.23266407419428,5.20194456401123));
#117403=CARTESIAN_POINT('',(-4.99794717941593,2.32233405365546,5.59200536389098));
#117404=CARTESIAN_POINT('Origin',(0.115422726916476,2.41067414184866,-0.150402059332356));
#117405=CARTESIAN_POINT('Ctrl Pts',(-4.83259642346235,2.3614745818336,5.40448996725973));
#117406=CARTESIAN_POINT('Ctrl Pts',(-4.86014132679959,2.35461430959202,
5.43567095312031));
#117407=CARTESIAN_POINT('Ctrl Pts',(-4.88770790993196,2.34792816341103,
5.46690618859985));
#117408=CARTESIAN_POINT('Ctrl Pts',(-4.94281497963354,2.3348925835358,5.52940164191918));
#117409=CARTESIAN_POINT('Ctrl Pts',(-4.97038777243001,2.32853551289827,
5.56069850005182));
#117410=CARTESIAN_POINT('Ctrl Pts',(-4.99794718101468,2.32233405368386,
5.59200536248922));
#117411=CARTESIAN_POINT('',(-5.39376206201143,2.23266407264716,5.02825330221466));
#117412=CARTESIAN_POINT('Origin',(8.38738800634786E-13,2.32340998500067,
-8.78637440582253E-13));
#117413=CARTESIAN_POINT('',(-4.99638627678617,2.14301213126216,5.59340005498915));
#117414=CARTESIAN_POINT('Origin',(0.109194973362047,2.01794105197273,-0.152265416766924));
#117415=CARTESIAN_POINT('',(-4.55841568752372,2.23266407449122,5.95574062463771));
#117416=CARTESIAN_POINT('Origin',(0.0875969833547863,2.41052397966279,-0.160978744647284));
#117417=CARTESIAN_POINT('Ctrl Pts',(-4.99794717819094,2.32233405317691,
5.59200536459627));
#117418=CARTESIAN_POINT('Ctrl Pts',(-4.93988696921939,2.31006874159968,
5.6438976355639));
#117419=CARTESIAN_POINT('Ctrl Pts',(-4.88110613546204,2.29785936479266,
5.69480704519649));
#117420=CARTESIAN_POINT('Ctrl Pts',(-4.82165457190422,2.28571428604934,
5.74470601375661));
#117421=CARTESIAN_POINT('Ctrl Pts',(-4.73570877678458,2.26815682568374,
5.81684215755424));
#117422=CARTESIAN_POINT('Ctrl Pts',(-4.64792575016144,2.25046493734972,
5.88723125139048));
#117423=CARTESIAN_POINT('Ctrl Pts',(-4.55841568517172,2.23266407446841,
5.95574062902004));
#117424=CARTESIAN_POINT('Ctrl Pts',(-4.836145564,2.36225522,5.40131429200001));
#117425=CARTESIAN_POINT('Ctrl Pts',(-4.661115028,2.323743665,5.558030436));
#117426=CARTESIAN_POINT('Ctrl Pts',(-4.476305531,2.285714286,5.703085901));
#117427=CARTESIAN_POINT('Ctrl Pts',(-4.347996415,2.259311335,5.803794678));
#117428=CARTESIAN_POINT('Ctrl Pts',(-4.215287887,2.232664075,5.89863103));
#117429=CARTESIAN_POINT('Ctrl Pts',(-4.21204490327798,2.23201289883432,
5.90094853551699));
#117430=CARTESIAN_POINT('Ctrl Pts',(-4.20880191955596,2.23136172266864,
5.90326604103399));
#117431=CARTESIAN_POINT('Ctrl Pts',(-5.183464651,2.36225522,5.420488373));
#117432=CARTESIAN_POINT('Ctrl Pts',(-5.007812776,2.323743665,5.588459453));
#117433=CARTESIAN_POINT('Ctrl Pts',(-4.821654572,2.285714286,5.744706014));
#117434=CARTESIAN_POINT('Ctrl Pts',(-4.692409079,2.259311335,5.85318452000001));
#117435=CARTESIAN_POINT('Ctrl Pts',(-4.558415688,2.232664075,5.955740627));
#117436=CARTESIAN_POINT('Ctrl Pts',(-4.55514130622198,2.23201289883432,
5.95824677932199));
#117437=CARTESIAN_POINT('Ctrl Pts',(-4.55186692444396,2.23136172266864,
5.96075293164397));
#117438=CARTESIAN_POINT('',(-4.38685179458954,2.23266407357604,5.92718582325286));
#117439=CARTESIAN_POINT('Ctrl Pts',(-4.2216501449166,2.23138000478158,5.89408442443341));
#117440=CARTESIAN_POINT('Ctrl Pts',(-4.2184690159583,2.23202203989079,5.8963577272167));
#117441=CARTESIAN_POINT('Ctrl Pts',(-4.215287887,2.232664075,5.89863103));
#117442=CARTESIAN_POINT('Ctrl Pts',(-3.895894042,2.297126115,6.126876702));
#117443=CARTESIAN_POINT('Ctrl Pts',(-3.55372216,2.362252267,6.3193005));
#117444=CARTESIAN_POINT('Ctrl Pts',(-4.16491064522116,2.23138000478158,
6.23727382379452));
#117445=CARTESIAN_POINT('Ctrl Pts',(-4.16154446761058,2.23202203989079,
6.23951632739726));
#117446=CARTESIAN_POINT('Ctrl Pts',(-4.15817829,2.232664075,6.241758831));
#117447=CARTESIAN_POINT('Ctrl Pts',(-3.820205066,2.297126115,6.466912183));
#117448=CARTESIAN_POINT('Ctrl Pts',(-3.459896332,2.362252267,6.654255583));
#117449=CARTESIAN_POINT('',(-4.15817828364985,2.2326640741942,6.24175883270281));
#117450=CARTESIAN_POINT('',(-3.67898209720619,2.32233405367819,6.53567829105955));
#117451=CARTESIAN_POINT('Origin',(0.0803922093623644,2.41067409671174,-0.171698205551547));
#117452=CARTESIAN_POINT('Ctrl Pts',(-3.55780741732799,2.36147458182567,
6.31700137554612));
#117453=CARTESIAN_POINT('Ctrl Pts',(-3.57800534560663,2.35461430959786,
6.35337470724872));
#117454=CARTESIAN_POINT('Ctrl Pts',(-3.59821278482228,2.34792816344734,
6.38980568064731));
#117455=CARTESIAN_POINT('Ctrl Pts',(-3.63859683118454,2.3348925756605,6.46268646034612));
#117456=CARTESIAN_POINT('Ctrl Pts',(-3.65879711607804,2.32853549679951,
6.49917900151715));
#117457=CARTESIAN_POINT('Ctrl Pts',(-3.67898209851557,2.32233405373059,
6.53567829016408));
#117458=CARTESIAN_POINT('',(-4.18673307644033,2.23266407264691,6.07019493881779));
#117459=CARTESIAN_POINT('Origin',(-2.31802424477401E-13,2.32340998500022,
4.01588484688631E-13));
#117460=CARTESIAN_POINT('',(-3.67715786974614,2.14301213125802,6.53670482748408));
#117461=CARTESIAN_POINT('Origin',(0.0739095778989851,2.01794107123741,-0.172179361219065));
#117462=CARTESIAN_POINT('',(-3.1715342780386,2.23266407449122,6.7964233455909));
#117463=CARTESIAN_POINT('Origin',(0.0509434473407411,2.41052397934557,-0.176046121056599));
#117464=CARTESIAN_POINT('Ctrl Pts',(-3.67898209636072,2.32233405324916,
6.53567829182381));
#117465=CARTESIAN_POINT('Ctrl Pts',(-3.61112399808775,2.3100687416221,6.57387612183453));
#117466=CARTESIAN_POINT('Ctrl Pts',(-3.54277340934683,2.29785936479204,
6.61095915618321));
#117467=CARTESIAN_POINT('Ctrl Pts',(-3.47398498685931,2.28571428605154,
6.64691118569604));
#117468=CARTESIAN_POINT('Ctrl Pts',(-3.37454141752927,2.26815682568914,
6.69888502086905));
#117469=CARTESIAN_POINT('Ctrl Pts',(-3.27367913498384,2.25046493734972,
6.7487577009611));
#117470=CARTESIAN_POINT('Ctrl Pts',(-3.17153427480362,2.23266407446842,
6.7964233493648));
#117471=CARTESIAN_POINT('Ctrl Pts',(-3.561956257,2.36225522,6.314662906));
#117472=CARTESIAN_POINT('Ctrl Pts',(-3.3573285,2.323743665,6.43008872300001));
#117473=CARTESIAN_POINT('Ctrl Pts',(-3.145657109,2.285714286,6.532024292));
#117474=CARTESIAN_POINT('Ctrl Pts',(-2.998698378,2.259311335,6.602795887));
#117475=CARTESIAN_POINT('Ctrl Pts',(-2.84870549,2.232664075,6.666886607));
#117476=CARTESIAN_POINT('Ctrl Pts',(-2.84504013027118,2.23201289883432,
6.66845278488491));
#117477=CARTESIAN_POINT('Ctrl Pts',(-2.84137477054235,2.23136172266864,
6.67001896276982));
#117478=CARTESIAN_POINT('Ctrl Pts',(-3.897033357,2.36225522,6.408052045));
#117479=CARTESIAN_POINT('Ctrl Pts',(-3.689379308,2.323743665,6.534336094));
#117480=CARTESIAN_POINT('Ctrl Pts',(-3.473984987,2.285714286,6.646911186));
#117481=CARTESIAN_POINT('Ctrl Pts',(-3.324441509,2.259311335,6.725069564));
#117482=CARTESIAN_POINT('Ctrl Pts',(-3.171534278,2.232664075,6.796423348));
#117483=CARTESIAN_POINT('Ctrl Pts',(-3.1677977007914,2.23201289883432,6.79816701258211));
#117484=CARTESIAN_POINT('Ctrl Pts',(-3.16406112358279,2.23136172266864,
6.7999106771642));
#117485=CARTESIAN_POINT('',(-3.01011989205181,2.23266407357603,6.73165497389956));
#117486=CARTESIAN_POINT('Ctrl Pts',(-2.85589638766259,2.23138000478158,
6.66381399592141));
#117487=CARTESIAN_POINT('Ctrl Pts',(-2.85230093883129,2.23202203989079,
6.6653503014607));
#117488=CARTESIAN_POINT('Ctrl Pts',(-2.84870549,2.232664075,6.666886607));
#117489=CARTESIAN_POINT('Ctrl Pts',(-2.487712823,2.297126115,6.821135787));
#117490=CARTESIAN_POINT('Ctrl Pts',(-2.112175301,2.362252267,6.935503983));
#117491=CARTESIAN_POINT('Ctrl Pts',(-2.72670784948992,2.23138000478158,
6.98678250313632));
#117492=CARTESIAN_POINT('Ctrl Pts',(-2.72293829924496,2.23202203989079,
6.98824894956816));
#117493=CARTESIAN_POINT('Ctrl Pts',(-2.719168749,2.232664075,6.989715396));
#117494=CARTESIAN_POINT('Ctrl Pts',(-2.340695835,2.297126115,7.136950535));
#117495=CARTESIAN_POINT('Ctrl Pts',(-1.948537627,2.362252267,7.242458223));
#117496=CARTESIAN_POINT('',(-2.71916874245356,2.23266407419428,6.98971539627998));
#117497=CARTESIAN_POINT('',(-2.18799190079208,2.32233405367884,7.17375016572119));
#117498=CARTESIAN_POINT('Origin',(0.0416026617872733,2.41067415701389,-0.18496603163382));
#117499=CARTESIAN_POINT('Ctrl Pts',(-2.11665929066327,2.36147458189896,
6.93413682048104));
#117500=CARTESIAN_POINT('Ctrl Pts',(-2.12856580561413,2.35461431306305,
6.97400170170876));
#117501=CARTESIAN_POINT('Ctrl Pts',(-2.14046921697517,2.34792817043707,
7.01392491861478));
#117502=CARTESIAN_POINT('Ctrl Pts',(-2.16424190922401,2.33489257395381,
7.0937832155994));
#117503=CARTESIAN_POINT('Ctrl Pts',(-2.17612510861286,2.32853549326735,
7.13376505783009));
#117504=CARTESIAN_POINT('Ctrl Pts',(-2.18799190243431,2.32233405371755,
7.17375016515142));
#117505=CARTESIAN_POINT('',(-2.78393710593565,2.23266407264716,6.82830100703027));
#117506=CARTESIAN_POINT('Origin',(1.87350135405495E-13,2.32340998500022,
-3.6125616387217E-13));
#117507=CARTESIAN_POINT('',(-2.18598964825113,2.14301213127997,7.17436054675462));
#117508=CARTESIAN_POINT('Origin',(0.0351680361798976,2.01794102414299,-0.184042014620551));
#117509=CARTESIAN_POINT('',(-1.63635545054791,2.23266407449123,7.31931286465458));
#117510=CARTESIAN_POINT('Origin',(0.0119076089986403,2.41052401647693,-0.182881204939523));
#117511=CARTESIAN_POINT('Ctrl Pts',(-2.18799189970922,2.32233405323606,
7.1737501661576));
#117512=CARTESIAN_POINT('Ctrl Pts',(-2.11350888185077,2.31006874162273,
7.1964674666809));
#117513=CARTESIAN_POINT('Ctrl Pts',(-2.03878453578529,2.29785936479673,
7.21799016405599));
#117514=CARTESIAN_POINT('Ctrl Pts',(-1.96387572496019,2.2857142860707,7.23831417758776));
#117515=CARTESIAN_POINT('Ctrl Pts',(-1.85558425318112,2.26815682573609,
7.26769546520652));
#117516=CARTESIAN_POINT('Ctrl Pts',(-1.74635892260611,2.25046493734973,
7.29471974078601));
#117517=CARTESIAN_POINT('Ctrl Pts',(-1.63635544658503,2.23266407446843,
7.31931286764579));
#117518=CARTESIAN_POINT('Ctrl Pts',(-2.121213834,2.36225522,6.932744901));
#117519=CARTESIAN_POINT('Ctrl Pts',(-1.896557022,2.323743665,7.001483207));
#117520=CARTESIAN_POINT('Ctrl Pts',(-1.667921256,2.285714286,7.055532488));
#117521=CARTESIAN_POINT('Ctrl Pts',(-1.509184538,2.259311335,7.093057699));
#117522=CARTESIAN_POINT('Ctrl Pts',(-1.34892079,2.232664075,7.123405976));
#117523=CARTESIAN_POINT('Ctrl Pts',(-1.34500444239351,2.23201289883432,
7.12414759351159));
#117524=CARTESIAN_POINT('Ctrl Pts',(-1.34108809478702,2.23136172266863,
7.12488921102318));
#117525=CARTESIAN_POINT('Ctrl Pts',(-2.428381113,2.36225522,7.095982326));
#117526=CARTESIAN_POINT('Ctrl Pts',(-2.198434563,2.323743665,7.174674441));
#117527=CARTESIAN_POINT('Ctrl Pts',(-1.963875725,2.285714286,7.238314178));
#117528=CARTESIAN_POINT('Ctrl Pts',(-1.80102675,2.259311335,7.282497829));
#117529=CARTESIAN_POINT('Ctrl Pts',(-1.63635545,2.232664075,7.319312867));
#117530=CARTESIAN_POINT('Ctrl Pts',(-1.63233139552941,2.23201289883432,
7.32021251203984));
#117531=CARTESIAN_POINT('Ctrl Pts',(-1.62830734105882,2.23136172266863,
7.32111215707968));
#117532=CARTESIAN_POINT('',(-1.49263812863751,2.23266407357604,7.22135941971465));
#117533=CARTESIAN_POINT('Ctrl Pts',(-1.35660408902388,2.23138000478158,
7.12195103128405));
#117534=CARTESIAN_POINT('Ctrl Pts',(-1.35276243951194,2.23202203989079,
7.12267850364202));
#117535=CARTESIAN_POINT('Ctrl Pts',(-1.34892079,2.232664075,7.123405976));
#117536=CARTESIAN_POINT('Ctrl Pts',(-0.963208917,2.297126115,7.196446144));
#117537=CARTESIAN_POINT('Ctrl Pts',(-0.571865472,2.362252267,7.227411008));
#117538=CARTESIAN_POINT('Ctrl Pts',(-1.16100722477529,2.23138000478158,
7.40959699727959));
#117539=CARTESIAN_POINT('Ctrl Pts',(-1.15701056188764,2.23202203989079,
7.4102188171398));
#117540=CARTESIAN_POINT('Ctrl Pts',(-1.153013899,2.232664075,7.410840637));
#117541=CARTESIAN_POINT('Ctrl Pts',(-0.751738269,2.297126115,7.473273012));
#117542=CARTESIAN_POINT('Ctrl Pts',(-0.346067467,2.362252267,7.492011566));
#117543=CARTESIAN_POINT('',(-1.15301389253179,2.23266407419428,7.41084063587417));
#117544=CARTESIAN_POINT('',(-0.594693634848295,2.32233405365367,7.47638545564975));
#117545=CARTESIAN_POINT('Origin',(0.000867775816465743,2.41067412545509,
-0.189584793094087));
#117546=CARTESIAN_POINT('Ctrl Pts',(-0.57653852750269,2.36147458197995,
7.22703973428062));
#117547=CARTESIAN_POINT('Ctrl Pts',(-0.579596905800721,2.35461430851645,
7.26853217341958));
#117548=CARTESIAN_POINT('Ctrl Pts',(-0.58263971288678,2.34792816106259,
7.31008092149065));
#117549=CARTESIAN_POINT('Ctrl Pts',(-0.588689435203046,2.33489257412025,
7.3931825410563));
#117550=CARTESIAN_POINT('Ctrl Pts',(-0.591699897721052,2.32853549358989,
7.43478416549529));
#117551=CARTESIAN_POINT('Ctrl Pts',(-0.594693636545425,2.32233405369389,
7.47638545543475));
#117552=CARTESIAN_POINT('',(-1.25096733006398,2.23266407264717,7.26712330898502));
#117553=CARTESIAN_POINT('Origin',(1.12435153418536E-14,2.32340998499911,
6.68735899989059E-13));
#117554=CARTESIAN_POINT('',(-0.592606979590432,2.14301213124966,7.47655114136116));
#117555=CARTESIAN_POINT('Origin',(-0.00521771807271636,2.01794103025283,
-0.18729966987722));
#117556=CARTESIAN_POINT('',(-0.0246624610398414,2.23266407449122,7.4999594488273));
#117557=CARTESIAN_POINT('Origin',(-0.0276848262311025,2.4105240391559,-0.181165925910276));
#117558=CARTESIAN_POINT('Ctrl Pts',(-0.594693633718621,2.32233405321371,
7.47638545586976));
#117559=CARTESIAN_POINT('Ctrl Pts',(-0.517068439203315,2.31006874160668,
7.4825599914261));
#117560=CARTESIAN_POINT('Ctrl Pts',(-0.439464362910036,2.29785936478825,
7.48751597444643));
#117561=CARTESIAN_POINT('Ctrl Pts',(-0.361937816336615,2.28571428609189,
7.49126164372934));
#117562=CARTESIAN_POINT('Ctrl Pts',(-0.2498620313125,2.268156825788,7.49667654805276));
#117563=CARTESIAN_POINT('Ctrl Pts',(-0.137380907420494,2.25046493734972,
7.4995887933537));
#117564=CARTESIAN_POINT('Ctrl Pts',(-0.0246624565258185,2.23266407446841,
7.49995945089641));
#117565=CARTESIAN_POINT('Ctrl Pts',(-0.58128581,2.36225522,7.22665945000001));
#117566=CARTESIAN_POINT('Ctrl Pts',(-0.347104645,2.323743665,7.245496119));
#117567=CARTESIAN_POINT('Ctrl Pts',(-0.112195259,2.285714286,7.249131826));
#117568=CARTESIAN_POINT('Ctrl Pts',(0.050897094,2.259311335,7.251656016));
#117569=CARTESIAN_POINT('Ctrl Pts',(0.213937947,2.232664075,7.246842799));
#117570=CARTESIAN_POINT('Ctrl Pts',(0.21792215841634,2.23201289883432,7.24672517894485));
#117571=CARTESIAN_POINT('Ctrl Pts',(0.221906369832681,2.23136172266864,
7.24660755888971));
#117572=CARTESIAN_POINT('Ctrl Pts',(-0.846180468000001,2.36225522,7.452112359));
#117573=CARTESIAN_POINT('Ctrl Pts',(-0.604693462,2.323743665,7.479532986));
#117574=CARTESIAN_POINT('Ctrl Pts',(-0.361937816,2.285714286,7.491261644));
#117575=CARTESIAN_POINT('Ctrl Pts',(-0.193397981,2.259311335,7.49940459));
#117576=CARTESIAN_POINT('Ctrl Pts',(-0.02466246,2.232664075,7.499959451));
#117577=CARTESIAN_POINT('Ctrl Pts',(-0.0205390886072463,2.23201289883432,
7.49997301007732));
#117578=CARTESIAN_POINT('Ctrl Pts',(-0.0164157172144926,2.23136172266864,
7.49998656915463));
#117579=CARTESIAN_POINT('',(0.0946377346806782,2.23266407357604,7.3734011251132));
#117580=CARTESIAN_POINT('Ctrl Pts',(-1.648995459,3.524895017,7.31647551600001));
#117581=CARTESIAN_POINT('Ctrl Pts',(-1.249180034,3.590632927,7.406586365));
#117582=CARTESIAN_POINT('Ctrl Pts',(-0.841926282,3.655724827,7.452594188));
#117583=CARTESIAN_POINT('Ctrl Pts',(-0.837869811072231,3.65637317805554,
7.45305245117261));
#117584=CARTESIAN_POINT('Ctrl Pts',(-0.833813340144462,3.65702152911109,
7.45351071434522));
#117585=CARTESIAN_POINT('Ctrl Pts',(-1.361222842,3.524895017,7.121065396));
#117586=CARTESIAN_POINT('Ctrl Pts',(-0.972085781,3.590632927,7.19545065));
#117587=CARTESIAN_POINT('Ctrl Pts',(-0.577160368,3.655724827,7.2269901));
#117588=CARTESIAN_POINT('Ctrl Pts',(-0.573226694096189,3.65637317805554,
7.22730425023526));
#117589=CARTESIAN_POINT('Ctrl Pts',(-0.569293020192376,3.65702152911109,
7.22761840047053));
#117590=CARTESIAN_POINT('',(-0.841926282128663,3.65572482719224,7.45259418698503));
#117591=CARTESIAN_POINT('',(-0.709543328283387,3.65572482753831,7.33979214368259));
#117592=CARTESIAN_POINT('',(-1.40345265024402,3.56509183363777,7.36751787445755));
#117593=CARTESIAN_POINT('Origin',(0.0485051084111301,3.48217865508547,-0.183541900715324));
#117594=CARTESIAN_POINT('Ctrl Pts',(-1.35657627490457,3.5256799153084,7.12195203649257));
#117595=CARTESIAN_POINT('Ctrl Pts',(-1.36441779022401,3.53257385732365,
7.16281259654519));
#117596=CARTESIAN_POINT('Ctrl Pts',(-1.37224786814811,3.53929993066044,
7.20372923721993));
#117597=CARTESIAN_POINT('Ctrl Pts',(-1.38786954498679,3.55242657232483,
7.28557141202438));
#117598=CARTESIAN_POINT('Ctrl Pts',(-1.3956699808557,3.55883456252376,7.32654325840034));
#117599=CARTESIAN_POINT('Ctrl Pts',(-1.40345265295455,3.5650918265975,7.36751787501784));
#117600=CARTESIAN_POINT('Ctrl Pts',(-1.98065117357706,3.66023518238734,
7.23433615161429));
#117601=CARTESIAN_POINT('Ctrl Pts',(-1.96707967046083,3.65798000469366,
7.23799719735335));
#117602=CARTESIAN_POINT('Ctrl Pts',(-1.95350816734467,3.655724827,7.24165824309244));
#117603=CARTESIAN_POINT('Ctrl Pts',(-1.55924996584151,3.590210912,7.34801325007673));
#117604=CARTESIAN_POINT('Ctrl Pts',(-1.15577569402086,3.524902621,7.41093724298845));
#117605=CARTESIAN_POINT('Ctrl Pts',(-2.14324560227677,3.66023518238734,
6.92601882209799));
#117606=CARTESIAN_POINT('Ctrl Pts',(-2.13025076263838,3.65798000469366,
6.92998674554904));
#117607=CARTESIAN_POINT('Ctrl Pts',(-2.117255923,3.655724827,6.933954669));
#117608=CARTESIAN_POINT('Ctrl Pts',(-1.739750052,3.590210912,7.04922461000001));
#117609=CARTESIAN_POINT('Ctrl Pts',(-1.351961251,3.524902621,7.122829548));
#117610=CARTESIAN_POINT('',(-1.9538431656242,3.65572482796969,7.24102876003761));
#117611=CARTESIAN_POINT('Origin',(0.0455076985269759,3.62500080274065,-0.187575497393542));
#117612=CARTESIAN_POINT('',(-2.03554954552453,3.65572482783621,7.08749169292897));
#117613=CARTESIAN_POINT('Origin',(1.77700736070374E-13,3.74685310400044,
-5.76795555762288E-13));
#117614=CARTESIAN_POINT('',(-1.3977596385386,3.74576903896356,7.36860013775438));
#117615=CARTESIAN_POINT('Origin',(0.0166322859562379,3.6250069064723,-0.191260385052409));
#117616=CARTESIAN_POINT('Origin',(0.0739319513853717,3.48232180518702,-0.168097046009336));
#117617=CARTESIAN_POINT('Ctrl Pts',(-3.183268824,3.524895017,6.79093510500001));
#117618=CARTESIAN_POINT('Ctrl Pts',(-2.812172031,3.590632927,6.96488771));
#117619=CARTESIAN_POINT('Ctrl Pts',(-2.424329967,3.655724827,7.097367414));
#117620=CARTESIAN_POINT('Ctrl Pts',(-2.42046684714056,3.65637317805554,
7.09868698457524));
#117621=CARTESIAN_POINT('Ctrl Pts',(-2.41660372728112,3.65702152911109,
7.10000655515048));
#117622=CARTESIAN_POINT('Ctrl Pts',(-2.860216771,3.524895017,6.661956171));
#117623=CARTESIAN_POINT('Ctrl Pts',(-2.496168149,3.590632927,6.818255304));
#117624=CARTESIAN_POINT('Ctrl Pts',(-2.117255923,3.655724827,6.933954669));
#117625=CARTESIAN_POINT('Ctrl Pts',(-2.11348174922899,3.65637317805554,
6.9351070981874));
#117626=CARTESIAN_POINT('Ctrl Pts',(-2.10970757545797,3.65702152911109,
6.93625952737481));
#117627=CARTESIAN_POINT('',(-2.42432996689638,3.65572482719223,7.0973674129809));
#117628=CARTESIAN_POINT('',(-2.27079294813839,3.65572482753831,7.01566104048418));
#117629=CARTESIAN_POINT('',(-2.95443926801662,3.56509183364827,6.89356856695547));
#117630=CARTESIAN_POINT('Origin',(0.0868271680473698,3.48217862574191,-0.168823614740856));
#117631=CARTESIAN_POINT('Ctrl Pts',(-2.8558694398306,3.52567991525912,6.66382095678268));
#117632=CARTESIAN_POINT('Ctrl Pts',(-2.87231143739544,3.53257385729302,
6.70204052566982));
#117633=CARTESIAN_POINT('Ctrl Pts',(-2.88875432070427,3.5392999306393,6.74031732272066));
#117634=CARTESIAN_POINT('Ctrl Pts',(-2.9216044198429,3.5524265723222,6.81688787423154));
#117635=CARTESIAN_POINT('Ctrl Pts',(-2.93803022178784,3.55883456252969,
6.85522495849874));
#117636=CARTESIAN_POINT('Ctrl Pts',(-2.9544392707911,3.56509182660857,6.89356856691695));
#117637=CARTESIAN_POINT('Ctrl Pts',(-3.4895130783971,3.66023518275518,6.63941993631662));
#117638=CARTESIAN_POINT('Ctrl Pts',(-3.47704588511778,3.65798000487759,
6.64591286140526));
#117639=CARTESIAN_POINT('Ctrl Pts',(-3.46457869183844,3.655724827,6.65240578649394));
#117640=CARTESIAN_POINT('Ctrl Pts',(-3.10240121177959,3.590210912,6.84102813268988));
#117641=CARTESIAN_POINT('Ctrl Pts',(-2.72188674166561,3.524902621,6.98921603906657));
#117642=CARTESIAN_POINT('Ctrl Pts',(-3.58202702740848,3.66023518275517,
6.30335789998202));
#117643=CARTESIAN_POINT('Ctrl Pts',(-3.57018898520421,3.65798000487759,
6.310026562491));
#117644=CARTESIAN_POINT('Ctrl Pts',(-3.558350943,3.655724827,6.316695225));
#117645=CARTESIAN_POINT('Ctrl Pts',(-3.21445058,3.590210912,6.510422821));
#117646=CARTESIAN_POINT('Ctrl Pts',(-2.851550952,3.524902621,6.665670046));
#117647=CARTESIAN_POINT('',(-3.46477053722386,3.65572482796921,6.65171900613451));
#117648=CARTESIAN_POINT('Origin',(0.0847667939926843,3.62500083493656,-0.173406924032474));
#117649=CARTESIAN_POINT('',(-3.51156073694809,3.6557248278362,6.48420709396512));
#117650=CARTESIAN_POINT('Origin',(3.52365706057789E-13,3.74685310400033,
-7.35522753814166E-13));
#117651=CARTESIAN_POINT('',(-2.94911201028439,3.74576903892179,6.89584935664121));
#117652=CARTESIAN_POINT('Origin',(0.0573589000497271,3.62500690824354,-0.183213729323725));
#117653=CARTESIAN_POINT('Origin',(0.108339344283563,3.48232178954017,-0.148273784597132));
#117654=CARTESIAN_POINT('Ctrl Pts',(-4.568696076,3.524895017,5.947858115));
#117655=CARTESIAN_POINT('Ctrl Pts',(-4.243669988,3.590632927,6.197518646));
#117656=CARTESIAN_POINT('Ctrl Pts',(-3.893374677,3.655724827,6.410275628));
#117657=CARTESIAN_POINT('Ctrl Pts',(-3.88988554341135,3.65637317805554,
6.41239480433152));
#117658=CARTESIAN_POINT('Ctrl Pts',(-3.88639640982271,3.65702152911109,
6.41451398066305));
#117659=CARTESIAN_POINT('Ctrl Pts',(-4.225470143,3.524895017,5.891341279));
#117660=CARTESIAN_POINT('Ctrl Pts',(-3.903532469,3.590632927,6.122245918));
#117661=CARTESIAN_POINT('Ctrl Pts',(-3.558350943,3.655724827,6.316695225));
#117662=CARTESIAN_POINT('Ctrl Pts',(-3.55491274551712,3.65637317805554,
6.31863204683871));
#117663=CARTESIAN_POINT('Ctrl Pts',(-3.55147454803423,3.65702152911109,
6.32056886867742));
#117664=CARTESIAN_POINT('',(-3.89337467666367,3.65572482719222,6.41027562703023));
#117665=CARTESIAN_POINT('',(-3.72586281284665,3.65572482753831,6.36348542483327));
#117666=CARTESIAN_POINT('',(-4.36727958874213,3.56509183365971,6.09728365434218));
#117667=CARTESIAN_POINT('Origin',(0.121089349492222,3.48217863436218,-0.146211419860039));
#117668=CARTESIAN_POINT('Ctrl Pts',(-4.22162532422951,3.52567991517959,
5.89409701454771));
#117669=CARTESIAN_POINT('Ctrl Pts',(-4.24589899453622,3.53257385725303,
5.92788848789027));
#117670=CARTESIAN_POINT('Ctrl Pts',(-4.27018583224941,3.53929993064236,
5.9617356610522));
#117671=CARTESIAN_POINT('Ctrl Pts',(-4.31872831917925,3.5524265723403,6.02945423542216));
#117672=CARTESIAN_POINT('Ctrl Pts',(-4.34301143468863,3.55883456254377,
6.06336395806092));
#117673=CARTESIAN_POINT('Ctrl Pts',(-4.36727959145042,3.56509182661936,
6.09728365370327));
#117674=CARTESIAN_POINT('Ctrl Pts',(-4.83520922754559,3.66023518254056,
5.734051826069));
#117675=CARTESIAN_POINT('Ctrl Pts',(-4.82442929775634,3.65798000477028,
5.74307302777226));
#117676=CARTESIAN_POINT('Ctrl Pts',(-4.81364936796707,3.655724827,5.75209422947556));
#117677=CARTESIAN_POINT('Ctrl Pts',(-4.50048762381256,3.590210912,6.01416414226722));
#117678=CARTESIAN_POINT('Ctrl Pts',(-4.16072539051528,3.524902621,6.24068686043289));
#117679=CARTESIAN_POINT('Ctrl Pts',(-4.85331684811587,3.66023518254055,
5.38595896879557));
#117680=CARTESIAN_POINT('Ctrl Pts',(-4.8431891385579,3.65798000477028,5.39501655039777));
#117681=CARTESIAN_POINT('Ctrl Pts',(-4.83306142900001,3.655724827,5.404074132));
#117682=CARTESIAN_POINT('Ctrl Pts',(-4.538846972,3.590210912,5.667200897));
#117683=CARTESIAN_POINT('Ctrl Pts',(-4.2178053,3.524902621,5.896831221));
#117684=CARTESIAN_POINT('',(-4.81368909063475,3.65572482796923,5.75138226461583));
#117685=CARTESIAN_POINT('Origin',(0.120062423877048,3.62500079669572,-0.151130525073971));
#117686=CARTESIAN_POINT('',(-4.8233752520844,3.65572482783621,5.57772817788604));
#117687=CARTESIAN_POINT('Origin',(-1.32272665043232E-14,3.74685310399945,
-1.3834419720915E-13));
#117688=CARTESIAN_POINT('',(-4.36256718226609,3.74576903900012,6.10065632338557));
#117689=CARTESIAN_POINT('Origin',(0.0954033633209156,3.62500690501871,-0.166599734340824));
#117690=CARTESIAN_POINT('Origin',(0.137680597554032,3.48232182391876,-0.12151708137942));
#117691=CARTESIAN_POINT('Ctrl Pts',(-5.740496178,3.524895017,4.826665891));
#117692=CARTESIAN_POINT('Ctrl Pts',(-5.476738654,3.590632927,5.140360499));
#117693=CARTESIAN_POINT('Ctrl Pts',(-5.180369514,3.655724827,5.423446478));
#117694=CARTESIAN_POINT('Ctrl Pts',(-5.17741751467674,3.65637317805554,
5.42626616974804));
#117695=CARTESIAN_POINT('Ctrl Pts',(-5.17446551535348,3.65702152911109,
5.42908586149607));
#117696=CARTESIAN_POINT('Ctrl Pts',(-5.393145228,3.524895017,4.845253817));
#117697=CARTESIAN_POINT('Ctrl Pts',(-5.128371949,3.590632927,5.139967117));
#117698=CARTESIAN_POINT('Ctrl Pts',(-4.833061429,3.655724827,5.404074132));
#117699=CARTESIAN_POINT('Ctrl Pts',(-4.83011997411306,3.65637317805554,
5.40670478284829));
#117700=CARTESIAN_POINT('Ctrl Pts',(-4.82717851922612,3.65702152911109,
5.40933543369657));
#117701=CARTESIAN_POINT('',(-5.18036951346671,3.65572482719222,5.42344647712341));
#117702=CARTESIAN_POINT('',(-5.0067154739218,3.65572482753831,5.41376030276029));
#117703=CARTESIAN_POINT('',(-5.57591077020258,3.56509183361144,5.01589653507367));
#117704=CARTESIAN_POINT('Origin',(0.149689339756273,3.48217862564796,-0.11676230994226));
#117705=CARTESIAN_POINT('Ctrl Pts',(-5.38998270015482,3.52567991529733,
4.84877164788896));
#117706=CARTESIAN_POINT('Ctrl Pts',(-5.4209530333726,3.53257385731543,4.87655497351864));
#117707=CARTESIAN_POINT('Ctrl Pts',(-5.45194819991669,3.53929993065206,
4.9043898661806));
#117708=CARTESIAN_POINT('Ctrl Pts',(-5.51391328222832,3.55242657230943,
4.96009001803131));
#117709=CARTESIAN_POINT('Ctrl Pts',(-5.54491826003029,3.5588345625054,4.98798679819863));
#117710=CARTESIAN_POINT('Ctrl Pts',(-5.57591077268672,3.56509182657088,
5.01589653389362));
#117711=CARTESIAN_POINT('Ctrl Pts',(-5.95481636838717,3.66023518243299,
4.56056582557203));
#117712=CARTESIAN_POINT('Ctrl Pts',(-5.9462277592515,3.6579800047165,4.57169348256676));
#117713=CARTESIAN_POINT('Ctrl Pts',(-5.93763915011584,3.655724827,4.58282113956136));
#117714=CARTESIAN_POINT('Ctrl Pts',(-5.68813623743456,3.590210912,4.90608452105027));
#117715=CARTESIAN_POINT('Ctrl Pts',(-5.405013144833,3.524902621,5.20035010028962));
#117716=CARTESIAN_POINT('Ctrl Pts',(-5.89767096768627,3.66023518243299,
4.21671858239213));
#117717=CARTESIAN_POINT('Ctrl Pts',(-5.88972715084314,3.6579800047165,4.22774156069603));
#117718=CARTESIAN_POINT('Ctrl Pts',(-5.881783334,3.655724827,4.238764539));
#117719=CARTESIAN_POINT('Ctrl Pts',(-5.651011924,3.590210912,4.558986958));
#117720=CARTESIAN_POINT('Ctrl Pts',(-5.386839759,3.524902621,4.852263122));
#117721=CARTESIAN_POINT('',(-5.93752489301315,3.65572482796969,4.58211728013338));
#117722=CARTESIAN_POINT('Origin',(0.149744069363979,3.62500078453731,-0.121787357599193));
#117723=CARTESIAN_POINT('',(-5.90965410140387,3.6557248278362,4.41044089164858));
#117724=CARTESIAN_POINT('Origin',(-5.31692745386891E-13,3.74685310399945,
5.28656979303932E-13));
#117725=CARTESIAN_POINT('',(-5.57203356115642,3.74576903893306,5.0202033813573));
#117726=CARTESIAN_POINT('Origin',(0.128986941211358,3.62500691642831,-0.1421958581512));
#117727=CARTESIAN_POINT('Origin',(0.160584885775001,3.48232175534712,-0.0890793231381287));
#117728=CARTESIAN_POINT('Ctrl Pts',(-6.643877059,3.524895017,3.479784134));
#117729=CARTESIAN_POINT('Ctrl Pts',(-6.45372110700001,3.590632927,3.842844807));
#117730=CARTESIAN_POINT('Ctrl Pts',(-6.225136031,3.655724827,4.183022998));
#117731=CARTESIAN_POINT('Ctrl Pts',(-6.22285919816356,3.65637317805554,
4.18641135951976));
#117732=CARTESIAN_POINT('Ctrl Pts',(-6.22058236532713,3.65702152911109,
4.18979972103951));
#117733=CARTESIAN_POINT('Ctrl Pts',(-6.308642835,3.524895017,3.572607672));
#117734=CARTESIAN_POINT('Ctrl Pts',(-6.113414457,3.590632927,3.917349167));
#117735=CARTESIAN_POINT('Ctrl Pts',(-5.881783334,3.655724827,4.238764539));
#117736=CARTESIAN_POINT('Ctrl Pts',(-5.87947616086335,3.65637317805554,
4.24196601254285));
#117737=CARTESIAN_POINT('Ctrl Pts',(-5.87716898772669,3.65702152911109,
4.24516748608571));
#117738=CARTESIAN_POINT('',(-6.2251360300065,3.65572482719341,4.18302299766136));
#117739=CARTESIAN_POINT('',(-6.05345968438371,3.65572482753831,4.21089376579204));
#117740=CARTESIAN_POINT('',(-6.52381856146396,3.56509183365653,3.69997166835753));
#117741=CARTESIAN_POINT('Origin',(0.171290316374076,3.48217861527856,-0.0818537976551986));
#117742=CARTESIAN_POINT('Ctrl Pts',(-6.30631047561056,3.52567991521273,
3.57672310740658));
#117743=CARTESIAN_POINT('Ctrl Pts',(-6.3425293335264,3.53257385729465,3.59719916832424));
#117744=CARTESIAN_POINT('Ctrl Pts',(-6.37878352962734,3.53929993068875,
3.61772025216271));
#117745=CARTESIAN_POINT('Ctrl Pts',(-6.45127378889825,3.55242657236831,
3.65879750424727));
#117746=CARTESIAN_POINT('Ctrl Pts',(-6.48755087059545,3.55883456255701,
3.67937691930957));
#117747=CARTESIAN_POINT('Ctrl Pts',(-6.52381856365252,3.56509182661619,
3.69997166664249));
#117748=CARTESIAN_POINT('Ctrl Pts',(-6.79598291391073,3.66023518252636,
3.17383283411095));
#117749=CARTESIAN_POINT('Ctrl Pts',(-6.78998721890074,3.65798000476318,
3.18654663001993));
#117750=CARTESIAN_POINT('Ctrl Pts',(-6.78399152389072,3.655724827,3.19926042592882));
#117751=CARTESIAN_POINT('Ctrl Pts',(-6.60981392261041,3.590210912,3.56860184020761));
#117752=CARTESIAN_POINT('Ctrl Pts',(-6.39656849161497,3.524902621,3.91685074986811));
#117753=CARTESIAN_POINT('Ctrl Pts',(-6.66625654791415,3.66023518252636,
2.85030912050949));
#117754=CARTESIAN_POINT('Ctrl Pts',(-6.66086806745706,3.65798000476318,
2.86278207375473));
#117755=CARTESIAN_POINT('Ctrl Pts',(-6.655479587,3.655724827,2.875255027));
#117756=CARTESIAN_POINT('Ctrl Pts',(-6.49894183800001,3.590210912,3.237599855));
#117757=CARTESIAN_POINT('Ctrl Pts',(-6.303991579,3.524902621,3.580808593));
#117758=CARTESIAN_POINT('',(-6.78372862907646,3.65572482796968,3.19859758423855));
#117759=CARTESIAN_POINT('Origin',(0.172423757110239,3.62500079678153,-0.0867494472170341));
#117760=CARTESIAN_POINT('',(-6.71960409236808,3.6557248278362,3.03692629071717));
#117761=CARTESIAN_POINT('Origin',(-4.58400678526871E-13,3.74685310399922,
2.42210765333262E-13));
#117762=CARTESIAN_POINT('',(-6.52095784402233,3.74576903896765,3.70501130866201));
#117763=CARTESIAN_POINT('Origin',(0.1565391361659,3.62500690036652,-0.111142978870203));
#117764=CARTESIAN_POINT('Origin',(0.175979677428308,3.48232175808432,-0.0524755584305797));
#117765=CARTESIAN_POINT('Ctrl Pts',(-7.236597633,3.524895017,1.970191539));
#117766=CARTESIAN_POINT('Ctrl Pts',(-7.128934734,3.590632927,2.365641964));
#117767=CARTESIAN_POINT('Ctrl Pts',(-6.978822105,3.655724827,2.747006012));
#117768=CARTESIAN_POINT('Ctrl Pts',(-6.97732690081234,3.65637317805554,
2.75080460726404));
#117769=CARTESIAN_POINT('Ctrl Pts',(-6.97583169662468,3.65702152911109,
2.75460320252807));
#117770=CARTESIAN_POINT('Ctrl Pts',(-6.929155316,3.524895017,2.132910362));
#117771=CARTESIAN_POINT('Ctrl Pts',(-6.812600499,3.590632927,2.511560324));
#117772=CARTESIAN_POINT('Ctrl Pts',(-6.655479587,3.655724827,2.875255027));
#117773=CARTESIAN_POINT('Ctrl Pts',(-6.65391457646654,3.65637317805554,
2.87887762588843));
#117774=CARTESIAN_POINT('Ctrl Pts',(-6.65234956593308,3.65702152911109,
2.88250022477685));
#117775=CARTESIAN_POINT('',(-6.97882210397194,3.65572482719341,2.74700601187689));
#117776=CARTESIAN_POINT('',(-6.81715084725753,3.65572482753831,2.81113051645041));
#117777=CARTESIAN_POINT('',(-7.16667984697849,3.56509183358835,2.21104023908412));
#117778=CARTESIAN_POINT('Origin',(0.184881715215719,3.48217862292307,-0.0431177229222868));
#117779=CARTESIAN_POINT('Ctrl Pts',(-6.92776218226152,3.52567991532782,
2.13743097000641));
#117780=CARTESIAN_POINT('Ctrl Pts',(-6.96753601101609,3.53257385732146,
2.14964232807016));
#117781=CARTESIAN_POINT('Ctrl Pts',(-7.00735403030485,3.53929993063986,
2.16189005980139));
#117782=CARTESIAN_POINT('Ctrl Pts',(-7.0869799025562,3.5524265722855,2.18642368566547));
#117783=CARTESIAN_POINT('Ctrl Pts',(-7.12683281221999,3.55883456247887,
2.19872346528053));
#117784=CARTESIAN_POINT('Ctrl Pts',(-7.16667984873252,3.56509182654799,
2.21104023698621));
#117785=CARTESIAN_POINT('Ctrl Pts',(-7.31937685100235,3.66023518245291,
1.63869494790891));
#117786=CARTESIAN_POINT('Ctrl Pts',(-7.31625442236225,3.65798000472645,
1.65240039930247));
#117787=CARTESIAN_POINT('Ctrl Pts',(-7.31313199372215,3.655724827,1.66610585069603));
#117788=CARTESIAN_POINT('Ctrl Pts',(-7.22242405433387,3.590210912,2.06425530344297));
#117789=CARTESIAN_POINT('Ctrl Pts',(-7.08902740513761,3.524902621,2.4502038113659));
#117790=CARTESIAN_POINT('Ctrl Pts',(-7.12313537988812,3.6602351824529,1.35062237334953));
#117791=CARTESIAN_POINT('Ctrl Pts',(-7.12055419544399,3.65798000472645,
1.36396207967477));
#117792=CARTESIAN_POINT('Ctrl Pts',(-7.117973011,3.655724827,1.377301786));
#117793=CARTESIAN_POINT('Ctrl Pts',(-7.042988456,3.590210912,1.764826182));
#117794=CARTESIAN_POINT('Ctrl Pts',(-6.926375758,3.524902621,2.141919433));
#117795=CARTESIAN_POINT('',(-7.31273275387848,3.65572482796968,1.66551502051135));
#117796=CARTESIAN_POINT('Origin',(0.187041280494084,3.62500079681395,-0.0476553129920807));
#117797=CARTESIAN_POINT('',(-7.21535286393197,3.6557248278362,1.52140839206518));
#117798=CARTESIAN_POINT('Origin',(3.19622800448727E-13,3.74685310400067,
-1.90602741922952E-13));
#117799=CARTESIAN_POINT('',(-7.16496938536899,3.74576903896349,2.21657702469344));
#117800=CARTESIAN_POINT('Origin',(0.176771704888491,3.62500695122242,-0.0748931927977434));
#117801=CARTESIAN_POINT('Origin',(0.183145646297144,3.48232178901916,-0.0134181692116192));
#117802=CARTESIAN_POINT('Ctrl Pts',(-7.490942944,3.524895017,0.368474977));
#117803=CARTESIAN_POINT('Ctrl Pts',(-7.470807296,3.590632927,0.777824331000001));
#117804=CARTESIAN_POINT('Ctrl Pts',(-7.406186214,3.655724827,1.182542078));
#117805=CARTESIAN_POINT('Ctrl Pts',(-7.40554255255019,3.65637317805554,
1.18657328892585));
#117806=CARTESIAN_POINT('Ctrl Pts',(-7.40489889110037,3.65702152911109,
1.19060449985171));
#117807=CARTESIAN_POINT('Ctrl Pts',(-7.225668194,3.524895017,0.593480535));
#117808=CARTESIAN_POINT('Ctrl Pts',(-7.19323691400001,3.590632927,0.988333711));
#117809=CARTESIAN_POINT('Ctrl Pts',(-7.117973011,3.655724827,1.377301786));
#117810=CARTESIAN_POINT('Ctrl Pts',(-7.11722334121076,3.65637317805554,
1.38117612154711));
#117811=CARTESIAN_POINT('Ctrl Pts',(-7.11647367142152,3.65702152911109,
1.38505045709422));
#117812=CARTESIAN_POINT('',(-7.40618621304264,3.65572482719222,1.18254207762938));
#117813=CARTESIAN_POINT('',(-7.26207961307256,3.65572482753831,1.27992192875138));
#117814=CARTESIAN_POINT('',(-7.47443514863315,3.56509183364457,0.618723025311942));
#117815=CARTESIAN_POINT('Origin',(0.189828274593485,3.48217859273075,-0.002365545620195));
#117816=CARTESIAN_POINT('Ctrl Pts',(-7.22527942811084,3.5256799152277,0.59819493566734));
#117817=CARTESIAN_POINT('Ctrl Pts',(-7.26674844813655,3.53257385726692,
0.601570601551338));
#117818=CARTESIAN_POINT('Ctrl Pts',(-7.30826844481787,3.53929993062775,
0.604972290989346));
#117819=CARTESIAN_POINT('Ctrl Pts',(-7.39130671308658,3.55242657231642,
0.611815125443492));
#117820=CARTESIAN_POINT('Ctrl Pts',(-7.43287197300667,3.55883456252145,
0.615260145453034));
#117821=CARTESIAN_POINT('Ctrl Pts',(-7.4744351498985,3.56509182660472,0.61872302284527));
#117822=CARTESIAN_POINT('Ctrl Pts',(-7.50052486205555,3.66023518270933,
0.0269335060383855));
#117823=CARTESIAN_POINT('Ctrl Pts',(-7.5004217009998,3.65798000485466,0.0409897622297917));
#117824=CARTESIAN_POINT('Ctrl Pts',(-7.5003185399441,3.655724827,0.0550460184211978));
#117825=CARTESIAN_POINT('Ctrl Pts',(-7.49732166560829,3.590210912,0.463386483204042));
#117826=CARTESIAN_POINT('Ctrl Pts',(-7.4500112758201,3.524902621,0.868988066263494));
#117827=CARTESIAN_POINT('Ctrl Pts',(-7.24694431946642,3.66023518270933,
-0.212217977081353));
#117828=CARTESIAN_POINT('Ctrl Pts',(-7.24729112423315,3.65798000485466,
-0.198635266540677));
#117829=CARTESIAN_POINT('Ctrl Pts',(-7.24763792900001,3.655724827,-0.185052556));
#117830=CARTESIAN_POINT('Ctrl Pts',(-7.257712761,3.590210912,0.209531198));
#117831=CARTESIAN_POINT('Ctrl Pts',(-7.224890305,3.524902621,0.602876501));
#117832=CARTESIAN_POINT('',(-7.49980162322622,3.65572482796921,0.0545548269909637));
#117833=CARTESIAN_POINT('Origin',(0.192912584456805,3.62500082539466,-0.00633279149226233));
#117834=CARTESIAN_POINT('',(-7.3737197555458,3.65572482783619,-0.0652488718236939));
#117835=CARTESIAN_POINT('Origin',(1.24249568966839E-12,3.746853104,-1.76270944455409E-13));
#117836=CARTESIAN_POINT('',(-7.47395492125183,3.7457690389483,0.62449806318162));
#117837=CARTESIAN_POINT('Origin',(0.188738899842835,3.62500689805883,-0.0351415693773142));
#117838=CARTESIAN_POINT('Origin',(0.181748235893762,3.4823217650145,0.0262664429100363));
#117839=CARTESIAN_POINT('Ctrl Pts',(-7.39502008900001,3.524895017,-1.250471066));
#117840=CARTESIAN_POINT('Ctrl Pts',(-7.463353212,3.590632927,-0.846363502));
#117841=CARTESIAN_POINT('Ctrl Pts',(-7.487245287,3.655724827,-0.437216209));
#117842=CARTESIAN_POINT('Ctrl Pts',(-7.48748326518231,3.65637317805554,
-0.433140877364431));
#117843=CARTESIAN_POINT('Ctrl Pts',(-7.48772124336463,3.65702152911109,
-0.429065545728861));
#117844=CARTESIAN_POINT('Ctrl Pts',(-7.184316859,3.524895017,-0.973699783));
#117845=CARTESIAN_POINT('Ctrl Pts',(-7.237525565,3.590632927,-0.581106288000001));
#117846=CARTESIAN_POINT('Ctrl Pts',(-7.24763792900001,3.655724827,-0.185052556));
#117847=CARTESIAN_POINT('Ctrl Pts',(-7.24773865369652,3.65637317805554,
-0.181107643419569));
#117848=CARTESIAN_POINT('Ctrl Pts',(-7.24783937839304,3.65702152911109,
-0.177162730839138));
#117849=CARTESIAN_POINT('',(-7.48724528598708,3.65572482719222,-0.437216209161948));
#117850=CARTESIAN_POINT('',(-7.36744160786082,3.6557248275383,-0.311134385795709));
#117851=CARTESIAN_POINT('',(-7.43269416944146,3.56509183362407,-1.00252498910139));
#117852=CARTESIAN_POINT('Origin',(0.185898731912409,3.48217863734023,0.0384972227116154));
#117853=CARTESIAN_POINT('Ctrl Pts',(-7.18495063902355,3.52567991522723,
-0.969012029225632));
#117854=CARTESIAN_POINT('Ctrl Pts',(-7.22617580481923,3.53257385729222,
-0.974629897902441));
#117855=CARTESIAN_POINT('Ctrl Pts',(-7.26745634979461,3.53929993067353,
-0.980233309912086));
#117856=CARTESIAN_POINT('Ctrl Pts',(-7.35002423646398,3.55242657234091,
-0.991401229939742));
#117857=CARTESIAN_POINT('Ctrl Pts',(-7.39135830107595,3.55883456252679,
-0.996972054680568));
#117858=CARTESIAN_POINT('Ctrl Pts',(-7.43269417014898,3.56509182658403,
-1.00252499176763));
#117859=CARTESIAN_POINT('Ctrl Pts',(-7.33095666743836,3.66023518241854,
-1.58608731454857));
#117860=CARTESIAN_POINT('Ctrl Pts',(-7.3338775975828,3.65798000470928,-1.57233751009812));
#117861=CARTESIAN_POINT('Ctrl Pts',(-7.33679852772727,3.655724827,-1.55858770564767));
#117862=CARTESIAN_POINT('Ctrl Pts',(-7.42165284693166,3.590210912,-1.15914977384803));
#117863=CARTESIAN_POINT('Ctrl Pts',(-7.46264089952596,3.524902621,-0.752860595137903));
#117864=CARTESIAN_POINT('Ctrl Pts',(-7.03189419658587,3.66023518241855,
-1.76513524738259));
#117865=CARTESIAN_POINT('Ctrl Pts',(-7.03515277429293,3.65798000470927,
-1.75194464669127));
#117866=CARTESIAN_POINT('Ctrl Pts',(-7.038411352,3.655724827,-1.738754046));
#117867=CARTESIAN_POINT('Ctrl Pts',(-7.13307448300001,3.590210912,-1.355561232));
#117868=CARTESIAN_POINT('Ctrl Pts',(-7.185577012,3.524902621,-0.964356266));
#117869=CARTESIAN_POINT('',(-7.33618810462917,3.65572482796923,-1.55895629147011));
#117870=CARTESIAN_POINT('Origin',(0.18976414911995,3.62500081621431,0.0352858245829443));
#117871=CARTESIAN_POINT('',(-7.18729970665748,3.65572482783619,-1.64885517145456));
#117872=CARTESIAN_POINT('Origin',(1.38647773817446E-12,3.74685310399989,
1.68756068147369E-13));
#117873=CARTESIAN_POINT('',(-7.43346663204992,3.74576903894809,-0.99678173471832));
#117874=CARTESIAN_POINT('Origin',(0.191880327280147,3.62500693360438,0.00625327433957518));
#117875=CARTESIAN_POINT('Origin',(0.171852892384567,3.48232180857018,0.064722890966695));
#117876=CARTESIAN_POINT('Ctrl Pts',(-6.953314313,3.524895017,-2.810946471));
#117877=CARTESIAN_POINT('Ctrl Pts',(-7.106921026,3.590632927,-2.430976319));
#117878=CARTESIAN_POINT('Ctrl Pts',(-7.21820909200001,3.655724827,-2.036530753));
#117879=CARTESIAN_POINT('Ctrl Pts',(-7.21931758222782,3.65637317805554,
-2.03260185863572));
#117880=CARTESIAN_POINT('Ctrl Pts',(-7.22042607245565,3.65702152911109,
-2.02867296427143));
#117881=CARTESIAN_POINT('Ctrl Pts',(-6.807034852,3.524895017,-2.495350981));
#117882=CARTESIAN_POINT('Ctrl Pts',(-6.943395564,3.590632927,-2.123374403));
#117883=CARTESIAN_POINT('Ctrl Pts',(-7.038411352,3.655724827,-1.738754046));
#117884=CARTESIAN_POINT('Ctrl Pts',(-7.03935776140644,3.65637317805554,
-1.7349230161108));
#117885=CARTESIAN_POINT('Ctrl Pts',(-7.04030417081289,3.65702152911109,
-1.73109198622161));
#117886=CARTESIAN_POINT('',(-7.21820909110468,3.65572482719347,-2.03653075247278));
#117887=CARTESIAN_POINT('',(-7.12831022115529,3.65572482753849,-1.88764240268987));
#117888=CARTESIAN_POINT('',(-7.04340867175693,3.5650918336432,-2.5768960497187));
#117889=CARTESIAN_POINT('Origin',(0.173276962231453,3.48217863691368,0.0775599817067715));
#117890=CARTESIAN_POINT('Ctrl Pts',(-6.80866154308647,3.52567991522762,
-2.49090906827572));
#117891=CARTESIAN_POINT('Ctrl Pts',(-6.84771521166626,3.53257385728763,
-2.50525778638665));
#117892=CARTESIAN_POINT('Ctrl Pts',(-6.88682607244739,3.5392999306626,-2.51960429069231));
#117893=CARTESIAN_POINT('Ctrl Pts',(-6.96506279516603,3.55242657233973,
-2.54826076596736));
#117894=CARTESIAN_POINT('Ctrl Pts',(-7.00423292972117,3.55883456253521,
-2.56258695001126));
#117895=CARTESIAN_POINT('Ctrl Pts',(-7.04340867186995,3.56509182660347,
-2.57689605248768));
#117896=CARTESIAN_POINT('Ctrl Pts',(-6.81860108506758,3.66023518271245,
-3.12494445771658));
#117897=CARTESIAN_POINT('Ctrl Pts',(-6.82440952740602,3.65798000485622,
-3.1121440288865));
#117898=CARTESIAN_POINT('Ctrl Pts',(-6.83021796974439,3.655724827,-3.09934360005647));
#117899=CARTESIAN_POINT('Ctrl Pts',(-6.99895579083881,3.590210912,-2.72748547630777));
#117900=CARTESIAN_POINT('Ctrl Pts',(-7.12632572833151,3.524902621,-2.33950633195554));
#117901=CARTESIAN_POINT('Ctrl Pts',(-6.48804051683436,3.66023518271245,
-3.23551675937307));
#117902=CARTESIAN_POINT('Ctrl Pts',(-6.49405850041722,3.65798000485622,
-3.22333504468654));
#117903=CARTESIAN_POINT('Ctrl Pts',(-6.500076484,3.655724827,-3.21115333));
#117904=CARTESIAN_POINT('Ctrl Pts',(-6.674901571,3.590210912,-2.857269126));
#117905=CARTESIAN_POINT('Ctrl Pts',(-6.810274123,3.524902621,-2.486496806));
#117906=CARTESIAN_POINT('',(-6.8295425829065,3.65572482796921,-3.0995723456306));
#117907=CARTESIAN_POINT('Origin',(0.177741842606053,3.62500083374336,0.0752544236285414));
#117908=CARTESIAN_POINT('',(-6.66480951171505,3.65572482783619,-3.15536283582134));
#117909=CARTESIAN_POINT('Origin',(-1.01915004213637E-12,3.74685310399945,
-3.9942008034366E-13));
#117910=CARTESIAN_POINT('',(-7.04539770494289,3.74576903893068,-2.57145312554884));
#117911=CARTESIAN_POINT('Origin',(0.186050156975672,3.62500693608475,0.0473557262033941));
#117912=CARTESIAN_POINT('Origin',(0.153921800927286,3.48232180130307,0.10015310657206));
#117913=CARTESIAN_POINT('Ctrl Pts',(-6.186479288,3.524895017,-4.239985143));
#117914=CARTESIAN_POINT('Ctrl Pts',(-6.418177113,3.590632927,-3.901919385));
#117915=CARTESIAN_POINT('Ctrl Pts',(-6.611657462,3.655724827,-3.540619381));
#117916=CARTESIAN_POINT('Ctrl Pts',(-6.61358463248514,3.65637317805554,
-3.53702063462816));
#117917=CARTESIAN_POINT('Ctrl Pts',(-6.61551180297026,3.65702152911109,
-3.53342188825632));
#117918=CARTESIAN_POINT('Ctrl Pts',(-6.111463461,3.524895017,-3.90032234));
#117919=CARTESIAN_POINT('Ctrl Pts',(-6.324600105,3.590632927,-3.56635589));
#117920=CARTESIAN_POINT('Ctrl Pts',(-6.500076484,3.655724827,-3.21115333));
#117921=CARTESIAN_POINT('Ctrl Pts',(-6.50182432506083,3.65637317805554,
-3.20761531751753));
#117922=CARTESIAN_POINT('Ctrl Pts',(-6.50357216612167,3.65702152911109,
-3.20407730503506));
#117923=CARTESIAN_POINT('',(-6.61165746100982,3.65572482719223,-3.54061938074149));
#117924=CARTESIAN_POINT('',(-6.55586697148985,3.6557248275383,-3.37588635843267));
#117925=CARTESIAN_POINT('',(-6.32478121320232,3.56509183364413,-4.03077431486429));
#117926=CARTESIAN_POINT('Origin',(0.152552477801926,3.48217864579776,0.112995930087421));
#117927=CARTESIAN_POINT('Ctrl Pts',(-6.11400700101208,3.52567991521301,
-3.89633396802979));
#117928=CARTESIAN_POINT('Ctrl Pts',(-6.14906306633873,3.53257385726894,
-3.91874260539261));
#117929=CARTESIAN_POINT('Ctrl Pts',(-6.18417546266473,3.53929993065058,
-3.94116137533083));
#117930=CARTESIAN_POINT('Ctrl Pts',(-6.25442275923254,3.55242657233169,
-3.98596646072884));
#117931=CARTESIAN_POINT('Ctrl Pts',(-6.28959741171118,3.5588345625289,-4.00837812752732));
#117932=CARTESIAN_POINT('Ctrl Pts',(-6.32478121271705,3.56509182660387,
-4.03077431759362));
#117933=CARTESIAN_POINT('Ctrl Pts',(-5.98741529591276,3.6602351824927,-4.51768266859114));
#117934=CARTESIAN_POINT('Ctrl Pts',(-5.99583965351217,3.65798000474635,
-4.50643015061259));
#117935=CARTESIAN_POINT('Ctrl Pts',(-6.00426401111169,3.655724827,-4.49517763263396));
#117936=CARTESIAN_POINT('Ctrl Pts',(-6.24899534042545,3.590210912,-4.16828698839096));
#117937=CARTESIAN_POINT('Ctrl Pts',(-6.45679148737917,3.524902621,-3.81675935347235));
#117938=CARTESIAN_POINT('Ctrl Pts',(-5.64081327373058,3.6602351824927,-4.55460910073637));
#117939=CARTESIAN_POINT('Ctrl Pts',(-5.64930926836524,3.65798000474635,
-4.5440058768682));
#117940=CARTESIAN_POINT('Ctrl Pts',(-5.657805263,3.655724827,-4.533402653));
#117941=CARTESIAN_POINT('Ctrl Pts',(-5.90461768,3.590210912,-4.225374291));
#117942=CARTESIAN_POINT('Ctrl Pts',(-6.11653038600001,3.524902621,-3.892371519));
#117943=CARTESIAN_POINT('',(-6.00355524095616,3.65572482796921,-4.49525584204769));
#117944=CARTESIAN_POINT('Origin',(0.157409015298306,3.62500080212542,0.111704365062237));
#117945=CARTESIAN_POINT('',(-5.83068023116903,3.65572482783619,-4.5143292409069));
#117946=CARTESIAN_POINT('Origin',(8.11416905888152E-13,3.746853104,4.95046711956881E-13));
#117947=CARTESIAN_POINT('',(-6.32789381133044,3.74576903895181,-4.02588622646399));
#117948=CARTESIAN_POINT('Origin',(0.171520220307716,3.62500688869145,0.0862437827618023));
#117949=CARTESIAN_POINT('Origin',(0.128792829381679,3.48232179096176,0.130899938843843));
#117950=CARTESIAN_POINT('Ctrl Pts',(-5.130371368,3.524895017,-5.470766823));
#117951=CARTESIAN_POINT('Ctrl Pts',(-5.42932637000001,3.590632927,-5.190413038));
#117952=CARTESIAN_POINT('Ctrl Pts',(-5.695952078,3.655724827,-4.87915258300001));
#117953=CARTESIAN_POINT('Ctrl Pts',(-5.69860781641318,3.65637317805554,
-4.87605225800491));
#117954=CARTESIAN_POINT('Ctrl Pts',(-5.70126355482636,3.65702152911109,
-4.87295193300981));
#117955=CARTESIAN_POINT('Ctrl Pts',(-5.130126831,3.524895017,-5.122918962));
#117956=CARTESIAN_POINT('Ctrl Pts',(-5.410073373,3.590632927,-4.84257854));
#117957=CARTESIAN_POINT('Ctrl Pts',(-5.657805263,3.655724827,-4.533402653));
#117958=CARTESIAN_POINT('Ctrl Pts',(-5.66027280861432,3.65637317805554,
-4.53032309144649));
#117959=CARTESIAN_POINT('Ctrl Pts',(-5.66274035422865,3.65702152911109,
-4.52724352989298));
#117960=CARTESIAN_POINT('',(-5.69595207709824,3.65572482719222,-4.87915258250859));
#117961=CARTESIAN_POINT('',(-5.67687866839472,3.6557248275383,-4.70627762053947));
#117962=CARTESIAN_POINT('',(-5.31041401431081,3.56509183366011,-5.29617805336075));
#117963=CARTESIAN_POINT('Origin',(0.124695323616197,3.48217858686857,0.143148643923253));
#117964=CARTESIAN_POINT('Ctrl Pts',(-5.13346828674902,3.52567991526401,
-5.11957062121533));
#117965=CARTESIAN_POINT('Ctrl Pts',(-5.16288756611796,3.53257385730878,
-5.14899137500095));
#117966=CARTESIAN_POINT('Ctrl Pts',(-5.19235968126349,3.53929993068155,
-5.17843413396552));
#117967=CARTESIAN_POINT('Ctrl Pts',(-5.25133286608943,3.55242657235264,
-5.23729279388202));
#117968=CARTESIAN_POINT('Ctrl Pts',(-5.28086730881873,3.55883456254548,
-5.26674199901425));
#117969=CARTESIAN_POINT('Ctrl Pts',(-5.31041401324188,3.56509182661964,
-5.2961780559303));
#117970=CARTESIAN_POINT('Ctrl Pts',(-4.87626462183353,3.6602351825012,-5.69917906100448));
#117971=CARTESIAN_POINT('Ctrl Pts',(-4.88691098140035,3.65798000475061,
-5.69000060847828));
#117972=CARTESIAN_POINT('Ctrl Pts',(-4.89755734096719,3.655724827,-5.68082215595224));
#117973=CARTESIAN_POINT('Ctrl Pts',(-5.20683881358382,3.590210912,-5.4141840346501));
#117974=CARTESIAN_POINT('Ctrl Pts',(-5.4853448518014,3.524902621,-5.11554494931966));
#117975=CARTESIAN_POINT('Ctrl Pts',(-4.52982787051219,3.66023518250122,
-5.6607329833822));
#117976=CARTESIAN_POINT('Ctrl Pts',(-4.54040461325608,3.65798000475061,
-5.65220404469116));
#117977=CARTESIAN_POINT('Ctrl Pts',(-4.550981356,3.655724827,-5.643675106));
#117978=CARTESIAN_POINT('Ctrl Pts',(-4.858240429,3.590210912,-5.39590565));
#117979=CARTESIAN_POINT('Ctrl Pts',(-5.136784486,3.524902621,-5.116243265));
#117980=CARTESIAN_POINT('',(-4.89684832804113,3.65572482796969,-5.68074617259837));
#117981=CARTESIAN_POINT('Origin',(0.129715678256187,3.62500078845805,0.14293098103293));
#117982=CARTESIAN_POINT('',(-4.72391482347484,3.65572482783619,-5.66221062818384));
#117983=CARTESIAN_POINT('Origin',(1.27415439310496E-12,3.74685310400078,
1.28065960613988E-12));
#117984=CARTESIAN_POINT('',(-5.31450463647661,3.74576903894741,-5.29207336199999));
#117985=CARTESIAN_POINT('Origin',(0.148970427180682,3.62500693028495,0.121099350128863));
#117986=CARTESIAN_POINT('Origin',(0.0976423688931122,3.48232175760876,0.155526501769297));
#117987=CARTESIAN_POINT('Ctrl Pts',(-3.834372984,3.524895017,-6.445741526));
#117988=CARTESIAN_POINT('Ctrl Pts',(-4.186606361,3.590632927,-6.236208745));
#117989=CARTESIAN_POINT('Ctrl Pts',(-4.513910305,3.655724827,-5.989542033));
#117990=CARTESIAN_POINT('Ctrl Pts',(-4.51717043195245,3.65637317805554,
-5.98708509714327));
#117991=CARTESIAN_POINT('Ctrl Pts',(-4.52043055890489,3.65702152911109,
-5.98462816128654));
#117992=CARTESIAN_POINT('Ctrl Pts',(-3.908911172,3.524895017,-6.105973587));
#117993=CARTESIAN_POINT('Ctrl Pts',(-4.242577624,3.590632927,-5.892367599));
#117994=CARTESIAN_POINT('Ctrl Pts',(-4.550981356,3.655724827,-5.643675106));
#117995=CARTESIAN_POINT('Ctrl Pts',(-4.55405322646585,3.65637317805554,
-5.64119799225248));
#117996=CARTESIAN_POINT('Ctrl Pts',(-4.5571250969317,3.65702152911109,-5.63872087850496));
#117997=CARTESIAN_POINT('',(-4.51391030460831,3.65572482719341,-5.98954203202406));
#117998=CARTESIAN_POINT('',(-4.53244582789803,3.6557248275383,-5.81660857152752));
#117999=CARTESIAN_POINT('',(-4.04773775792123,3.5650918336188,-6.31393839137917));
#118000=CARTESIAN_POINT('Origin',(0.0910073196940303,3.48217860516275,0.16660777581755));
#118001=CARTESIAN_POINT('Ctrl Pts',(-3.91289430058519,3.52567991523439,
-6.10342184256814));
#118002=CARTESIAN_POINT('Ctrl Pts',(-3.93530118122091,3.53257385728072,
-6.13847903075732));
#118003=CARTESIAN_POINT('Ctrl Pts',(-3.95775493185482,3.53929993065187,
-6.17356906780972));
#118004=CARTESIAN_POINT('Ctrl Pts',(-4.00269648435988,3.55242657232069,
-6.24372913625754));
#118005=CARTESIAN_POINT('Ctrl Pts',(-4.02520971961444,3.5588345625106,-6.27883886740677));
#118006=CARTESIAN_POINT('Ctrl Pts',(-4.04773775635048,3.56509182657902,
-6.31393839364233));
#118007=CARTESIAN_POINT('Ctrl Pts',(-3.53710523200821,3.66023518267594,
-6.61418817373702));
#118008=CARTESIAN_POINT('Ctrl Pts',(-3.54947578204589,3.65798000483796,
-6.60751296069411));
#118009=CARTESIAN_POINT('Ctrl Pts',(-3.56184633208361,3.655724827,-6.60083774765122));
#118010=CARTESIAN_POINT('Ctrl Pts',(-3.92121628953467,3.590210912,-6.40691985233655));
#118011=CARTESIAN_POINT('Ctrl Pts',(-4.25740958765534,3.524902621,-6.17513334797329));
#118012=CARTESIAN_POINT('Ctrl Pts',(-3.20703274994005,3.66023518267593,
-6.50216728302699));
#118013=CARTESIAN_POINT('Ctrl Pts',(-3.21919568447,3.65798000483796,-6.49611143301358));
#118014=CARTESIAN_POINT('Ctrl Pts',(-3.231358619,3.655724827,-6.490055583));
#118015=CARTESIAN_POINT('Ctrl Pts',(-3.584697254,3.590210912,-6.314130458));
#118016=CARTESIAN_POINT('Ctrl Pts',(-3.916848252,3.524902621,-6.10088516300001));
#118017=CARTESIAN_POINT('',(-3.56117022965222,3.65572482796966,-6.60061112390672));
#118018=CARTESIAN_POINT('Origin',(0.095957020842885,3.62500083064261,0.167474319064722));
#118019=CARTESIAN_POINT('',(-3.39626440859483,3.6557248278362,-6.54533333861582));
#118020=CARTESIAN_POINT('Origin',(7.66530935947252E-13,3.74685310400089,
1.24769986009632E-12));
#118021=CARTESIAN_POINT('',(-4.05261513061144,3.74576903895328,-6.31080902873435));
#118022=CARTESIAN_POINT('Origin',(0.119454723690957,3.62500693046372,0.150292257934594));
#118023=CARTESIAN_POINT('Origin',(0.0619259432285724,3.48232178816845,0.17288060055575));
#118024=CARTESIAN_POINT('Ctrl Pts',(-2.359083581,3.524895017,-7.11932051900001));
#118025=CARTESIAN_POINT('Ctrl Pts',(-2.748125292,3.590632927,-6.99040626299999));
#118026=CARTESIAN_POINT('Ctrl Pts',(-3.120803103,3.655724827,-6.81986715399999));
#118027=CARTESIAN_POINT('Ctrl Pts',(-3.12451517857529,3.65637317805554,
-6.81816849085863));
#118028=CARTESIAN_POINT('Ctrl Pts',(-3.12822725415059,3.65702152911109,
-6.81646982771726));
#118029=CARTESIAN_POINT('Ctrl Pts',(-2.504919172,3.524895017,-6.803519673));
#118030=CARTESIAN_POINT('Ctrl Pts',(-2.87670366,3.590632927,-6.66663609900001));
#118031=CARTESIAN_POINT('Ctrl Pts',(-3.231358619,3.655724827,-6.490055583));
#118032=CARTESIAN_POINT('Ctrl Pts',(-3.23489117707591,3.65637317805554,
-6.48829674412854));
#118033=CARTESIAN_POINT('Ctrl Pts',(-3.23842373515182,3.65702152911109,
-6.48653790525709));
#118034=CARTESIAN_POINT('',(-3.12080310282607,3.65572482719341,-6.81986715296628));
#118035=CARTESIAN_POINT('',(-3.17608085802301,3.6557248275383,-6.65496136992077));
#118036=CARTESIAN_POINT('',(-2.59579378301225,3.56509183361683,-7.03646598849934));
#118037=CARTESIAN_POINT('Origin',(0.0530637683764096,3.48217861931808,0.182276192629589));
#118038=CARTESIAN_POINT('Ctrl Pts',(-2.50935772659468,3.52567991518581,
-6.80188384193689));
#118039=CARTESIAN_POINT('Ctrl Pts',(-2.52370448737854,3.53257385723308,
-6.84093822952236));
#118040=CARTESIAN_POINT('Ctrl Pts',(-2.53808996089894,3.53929993059772,
-6.88003477361846));
#118041=CARTESIAN_POINT('Ctrl Pts',(-2.56689846389596,3.55242657228965,
-6.9582156441211));
#118042=CARTESIAN_POINT('Ctrl Pts',(-2.5813377978392,3.55883456249658,-6.99734420948112));
#118043=CARTESIAN_POINT('Ctrl Pts',(-2.59579378099291,3.56509182657663,
-7.03646599037154));
#118044=CARTESIAN_POINT('Ctrl Pts',(-2.0325547345735,3.66023518250409,-7.21992519859157));
#118045=CARTESIAN_POINT('Ctrl Pts',(-2.04607104101206,3.65798000475204,
-7.21606535104289));
#118046=CARTESIAN_POINT('Ctrl Pts',(-2.05958734745061,3.655724827,-7.21220550349425));
#118047=CARTESIAN_POINT('Ctrl Pts',(-2.45224205075605,3.590210912,-7.10007521842663));
#118048=CARTESIAN_POINT('Ctrl Pts',(-2.83040258307706,3.524902621,-6.94597937575816));
#118049=CARTESIAN_POINT('Ctrl Pts',(-1.73428034373308,3.66023518250408,
-7.03956746721845));
#118050=CARTESIAN_POINT('Ctrl Pts',(-1.74746074386651,3.65798000475204,
-7.03626787110924));
#118051=CARTESIAN_POINT('Ctrl Pts',(-1.760641144,3.655724827,-7.032968275));
#118052=CARTESIAN_POINT('Ctrl Pts',(-2.14353762,3.590210912,-6.937113543));
#118053=CARTESIAN_POINT('Ctrl Pts',(-2.513764547,3.524902621,-6.800256451));
#118054=CARTESIAN_POINT('',(-2.05897576934496,3.65572482796967,-7.21183883606633));
#118055=CARTESIAN_POINT('Origin',(0.0577116199150312,3.62500080581228,0.184186927122787));
#118056=CARTESIAN_POINT('',(-1.90980844449988,3.65572482783619,-7.12240353765932));
#118057=CARTESIAN_POINT('Origin',(1.07986536379556E-13,3.74685310400033,
2.95336671785051E-13));
#118058=CARTESIAN_POINT('',(-2.60122984621702,3.74576903893663,-7.03445827951591));
#118059=CARTESIAN_POINT('Origin',(0.0843535976532561,3.62500687597838,0.172457830982561));
#118060=CARTESIAN_POINT('Origin',(0.0233139335965546,3.48232177458421,0.182151020955458));
#118061=CARTESIAN_POINT('Ctrl Pts',(-0.773486052000001,3.524895017,-7.460007998));
#118062=CARTESIAN_POINT('Ctrl Pts',(-1.181144938,3.590632927,-7.417740153));
#118063=CARTESIAN_POINT('Ctrl Pts',(-1.581770616,3.655724827,-7.33130286600001));
#118064=CARTESIAN_POINT('Ctrl Pts',(-1.58576106767231,3.65637317805554,
-7.3304419031726));
#118065=CARTESIAN_POINT('Ctrl Pts',(-1.58975151934463,3.65702152911109,
-7.3295809403452));
#118066=CARTESIAN_POINT('Ctrl Pts',(-0.983799934,3.524895017,-7.182940741));
#118067=CARTESIAN_POINT('Ctrl Pts',(-1.37631823,3.590632927,-7.129180104));
#118068=CARTESIAN_POINT('Ctrl Pts',(-1.760641144,3.655724827,-7.032968275));
#118069=CARTESIAN_POINT('Ctrl Pts',(-1.76446921119364,3.65637317805554,
-7.03200995236865));
#118070=CARTESIAN_POINT('Ctrl Pts',(-1.76829727838728,3.65702152911109,
-7.03105162973729));
#118071=CARTESIAN_POINT('',(-1.58177061555191,3.65572482719222,-7.33130286508043));
#118072=CARTESIAN_POINT('',(-1.67120587678719,3.6557248275383,-7.18213557124759));
#118073=CARTESIAN_POINT('',(-1.02247337587459,3.56509183364358,-7.42997625638912));
#118074=CARTESIAN_POINT('Origin',(0.0126391814059199,3.48217861389325,0.189421790792401));
#118075=CARTESIAN_POINT('Ctrl Pts',(-0.988486372994223,3.52567991519632,
-7.18229731285625));
#118076=CARTESIAN_POINT('Ctrl Pts',(-0.994102175902777,3.53257385726828,
-7.22352276015149));
#118077=CARTESIAN_POINT('Ctrl Pts',(-0.999746723952424,3.53929993065635,
-7.26479770048792));
#118078=CARTESIAN_POINT('Ctrl Pts',(-1.0110751242192,3.55242657234039,-7.3473437222239));
#118079=CARTESIAN_POINT('Ctrl Pts',(-1.01676538966102,3.55883456253443,
-7.38866151338171));
#118080=CARTESIAN_POINT('Ctrl Pts',(-1.02247337348076,3.56509182660379,
-7.42997625778604));
#118081=CARTESIAN_POINT('Ctrl Pts',(-0.432964236225081,3.66023518261545,
-7.48806654611535));
#118082=CARTESIAN_POINT('Ctrl Pts',(-0.446994292381468,3.65798000480772,
-7.48720254598314));
#118083=CARTESIAN_POINT('Ctrl Pts',(-0.461024348537847,3.655724827,-7.48633854585082));
#118084=CARTESIAN_POINT('Ctrl Pts',(-0.868603699188754,3.590210912,-7.4612389590092));
#118085=CARTESIAN_POINT('Ctrl Pts',(-1.27104909975372,3.524902621,-7.39203912715354));
#118086=CARTESIAN_POINT('Ctrl Pts',(-0.180434915674636,3.66023518261545,
-7.24780530097854));
#118087=CARTESIAN_POINT('Ctrl Pts',(-0.194016481337319,3.65798000480772,
-7.24741624398922));
#118088=CARTESIAN_POINT('Ctrl Pts',(-0.207598047,3.655724827,-7.247027187));
#118089=CARTESIAN_POINT('Ctrl Pts',(-0.60214855,3.590210912,-7.23572490900001));
#118090=CARTESIAN_POINT('Ctrl Pts',(-0.993140006000001,3.524902621,-7.181655306));
#118091=CARTESIAN_POINT('',(-0.460505891419481,3.65572482796966,-7.48584897967103));
#118092=CARTESIAN_POINT('Origin',(0.0167675994576022,3.62500082997759,0.192286946163568));
#118093=CARTESIAN_POINT('',(-0.334051961171194,3.65572482783619,-7.3664380632655));
#118094=CARTESIAN_POINT('Origin',(1.43006266550838E-13,3.74685310400067,
5.2952434104192E-13));
#118095=CARTESIAN_POINT('',(-1.02821394480032,3.74576903896483,-7.42918407892651));
#118096=CARTESIAN_POINT('Origin',(0.0453081133289925,3.62500687504689,0.186559308707741));
#118097=CARTESIAN_POINT('Origin',(-0.0163882141384704,3.48232176110686,
0.182904204562684));
#118098=CARTESIAN_POINT('Ctrl Pts',(0.848278826,3.524895017,-7.451873793));
#118099=CARTESIAN_POINT('Ctrl Pts',(0.44106444,3.590632927,-7.49822875700001));
#118100=CARTESIAN_POINT('Ctrl Pts',(0.031223706,3.655724827,-7.499935005));
#118101=CARTESIAN_POINT('Ctrl Pts',(0.027141467311413,3.65637317805554,
-7.49995200016671));
#118102=CARTESIAN_POINT('Ctrl Pts',(0.0230592286228261,3.65702152911109,
-7.49996899533341));
#118103=CARTESIAN_POINT('Ctrl Pts',(0.583320695,3.524895017,-7.226495483));
#118104=CARTESIAN_POINT('Ctrl Pts',(0.188422311,3.590632927,-7.25837157));
#118105=CARTESIAN_POINT('Ctrl Pts',(-0.207598047,3.655724827,-7.247027187));
#118106=CARTESIAN_POINT('Ctrl Pts',(-0.21154262715707,3.65637317805554,
-7.24691419071793));
#118107=CARTESIAN_POINT('Ctrl Pts',(-0.215487207314141,3.65702152911109,
-7.24680119443587));
#118108=CARTESIAN_POINT('',(0.0312237062235909,3.65572482719222,-7.49993500399947));
#118109=CARTESIAN_POINT('',(-0.0881871672015895,3.6557248275383,-7.37348109603945));
#118110=CARTESIAN_POINT('',(0.59865674998268,3.56509183372456,-7.47606909195671));
#118111=CARTESIAN_POINT('Origin',(-0.0283764114982865,3.48217863417679,
0.187710425900819));
#118112=CARTESIAN_POINT('Ctrl Pts',(0.578605504166122,3.52567991521001,
-7.22687454364312));
#118113=CARTESIAN_POINT('Ctrl Pts',(0.581983248302078,3.53257385729805,
-7.26834339445086));
#118114=CARTESIAN_POINT('Ctrl Pts',(0.585343558783091,3.53929993070054,
-7.30986676056336));
#118115=CARTESIAN_POINT('Ctrl Pts',(0.592024964821285,3.55242657240916,
-7.3929181733487));
#118116=CARTESIAN_POINT('Ctrl Pts',(0.595349838307345,3.55883456261099,
-7.43449321637042));
#118117=CARTESIAN_POINT('Ctrl Pts',(0.598656752679924,3.56509182668411,
-7.47606909280178));
#118118=CARTESIAN_POINT('Ctrl Pts',(1.18687118926983,3.66023518255067,-7.4060742236875));
#118119=CARTESIAN_POINT('Ctrl Pts',(1.17298341369048,3.65798000477534,-7.40824647072547));
#118120=CARTESIAN_POINT('Ctrl Pts',(1.15909563811114,3.655724827,-7.41041871776356));
#118121=CARTESIAN_POINT('Ctrl Pts',(0.755649595500152,3.590210912,-7.47352345804971));
#118122=CARTESIAN_POINT('Ctrl Pts',(0.3477372264216,3.524902621,-7.49245534442631));
#118123=CARTESIAN_POINT('Ctrl Pts',(1.38184744851904,3.66023518255067,-7.11714381383192));
#118124=CARTESIAN_POINT('Ctrl Pts',(1.36849977675952,3.65798000477534,-7.11968348791595));
#118125=CARTESIAN_POINT('Ctrl Pts',(1.355152105,3.655724827,-7.122223162));
#118126=CARTESIAN_POINT('Ctrl Pts',(0.967396318,3.590210912,-7.196001821));
#118127=CARTESIAN_POINT('Ctrl Pts',(0.573922658000001,3.524902621,-7.22724794000001));
#118128=CARTESIAN_POINT('',(1.15949673172118,3.65572482796968,-7.40982914442963));
#118129=CARTESIAN_POINT('Origin',(-0.0249604152249596,3.62500078965105,
0.191395883719061));
#118130=CARTESIAN_POINT('',(1.25732442189929,3.65572482783619,-7.26602613188263));
#118131=CARTESIAN_POINT('Origin',(-3.67934171628323E-14,3.74685310399933,
-1.82145964977565E-13));
#118132=CARTESIAN_POINT('',(0.59288009775944,3.74576903896458,-7.47652948820546));
#118133=CARTESIAN_POINT('Origin',(0.0041440898913598,3.62500689541319,0.191937658093946));
#118134=CARTESIAN_POINT('Origin',(-0.0553240300614782,3.48232179305368,
0.175104735946446));
#118135=CARTESIAN_POINT('Ctrl Pts',(2.430379128,3.524895017,-7.095298253));
#118136=CARTESIAN_POINT('Ctrl Pts',(2.042650135,3.590632927,-7.228108519));
#118137=CARTESIAN_POINT('Ctrl Pts',(1.642758043,3.655724827,-7.31787851900001));
#118138=CARTESIAN_POINT('Ctrl Pts',(1.63877489824694,3.65637317805554,-7.31877267747834));
#118139=CARTESIAN_POINT('Ctrl Pts',(1.63479175349388,3.65702152911109,-7.31966683595668));
#118140=CARTESIAN_POINT('Ctrl Pts',(2.123165896,3.524895017,-6.932147328));
#118141=CARTESIAN_POINT('Ctrl Pts',(1.744352434,3.590632927,-7.048169649));
#118142=CARTESIAN_POINT('Ctrl Pts',(1.355152105,3.655724827,-7.122223162));
#118143=CARTESIAN_POINT('Ctrl Pts',(1.35127545607555,3.65637317805554,-7.12296077564041));
#118144=CARTESIAN_POINT('Ctrl Pts',(1.34739880715111,3.65702152911109,-7.12369838928082));
#118145=CARTESIAN_POINT('',(1.64275804250961,3.65572482719341,-7.31787851806958));
#118146=CARTESIAN_POINT('',(1.49895507722978,3.6557248275383,-7.22005083982947));
#118147=CARTESIAN_POINT('',(2.19179435121699,3.56509183362882,-7.17258924590931));
#118148=CARTESIAN_POINT('Origin',(-0.0680652196647022,3.48217863853533,
0.177221885982551));
#118149=CARTESIAN_POINT('Ctrl Pts',(2.11864243056491,3.52567991520743,-6.93353115305763));
#118150=CARTESIAN_POINT('Ctrl Pts',(2.13085578201956,3.53257385728076,-6.97330436997477));
#118151=CARTESIAN_POINT('Ctrl Pts',(2.14306382660055,3.5392999306645,-7.0131345753751));
#118152=CARTESIAN_POINT('Ctrl Pts',(2.16744262385646,3.55242657234158,-7.09280798740711));
#118153=CARTESIAN_POINT('Ctrl Pts',(2.17962716896065,3.55883456253058,-7.13269627949745));
#118154=CARTESIAN_POINT('Ctrl Pts',(2.19179435396591,3.56509182658866,-7.17258924617516));
#118155=CARTESIAN_POINT('Ctrl Pts',(2.7512098358553,3.66023518259726,-6.97778210206156));
#118156=CARTESIAN_POINT('Ctrl Pts',(2.73811371755116,3.65798000479863,-6.98288902444044));
#118157=CARTESIAN_POINT('Ctrl Pts',(2.725017599247,3.655724827,-6.98799594681922));
#118158=CARTESIAN_POINT('Ctrl Pts',(2.34456955567036,3.590210912,-7.13635430634087));
#118159=CARTESIAN_POINT('Ctrl Pts',(1.95026374733726,3.524902621,-7.24253267697325));
#118160=CARTESIAN_POINT('Ctrl Pts',(2.87951616181174,3.66023518259726,-6.65369259232325));
#118161=CARTESIAN_POINT('Ctrl Pts',(2.86702650590587,3.65798000479863,-6.65904224516163));
#118162=CARTESIAN_POINT('Ctrl Pts',(2.85453685,3.655724827,-6.664391898));
#118163=CARTESIAN_POINT('Ctrl Pts',(2.491706808,3.590210912,-6.819801685));
#118164=CARTESIAN_POINT('Ctrl Pts',(2.114149336,3.524902621,-6.934902493));
#118165=CARTESIAN_POINT('',(2.7252825740502,3.65572482796922,-6.9873339345461));
#118166=CARTESIAN_POINT('Origin',(-0.065521295201377,3.62500080738625,0.181555350276441));
#118167=CARTESIAN_POINT('',(2.78990971120828,3.65572482783619,-6.8258628944585));
#118168=CARTESIAN_POINT('Origin',(-3.50630982581812E-13,3.746853104,9.64506252643105E-13));
#118169=CARTESIAN_POINT('',(2.18625172566659,3.74576903899511,-7.17428068773578));
#118170=CARTESIAN_POINT('Origin',(-0.0372137556890989,3.62500689313507,
0.188341216217426));
#118171=CARTESIAN_POINT('Origin',(-0.0916730539911931,3.48232175921621,
0.159118208518176));
#118172=CARTESIAN_POINT('Ctrl Pts',(3.898837603,3.524895017,-6.40695445200001));
#118173=CARTESIAN_POINT('Ctrl Pts',(3.54872378,3.590632927,-6.62000996));
#118174=CARTESIAN_POINT('Ctrl Pts',(3.177478839,3.655724827,-6.793646166));
#118175=CARTESIAN_POINT('Ctrl Pts',(3.17378103559647,3.65637317805554,-6.7953756779276));
#118176=CARTESIAN_POINT('Ctrl Pts',(3.17008323219293,3.65702152911109,-6.79710518985521));
#118177=CARTESIAN_POINT('Ctrl Pts',(3.56373422,3.524895017,-6.313659668));
#118178=CARTESIAN_POINT('Ctrl Pts',(3.218718575,3.590632927,-6.508403149));
#118179=CARTESIAN_POINT('Ctrl Pts',(2.85453685,3.655724827,-6.664391898));
#118180=CARTESIAN_POINT('Ctrl Pts',(2.85090940010511,3.65637317805554,-6.66594563156849));
#118181=CARTESIAN_POINT('Ctrl Pts',(2.84728195021021,3.65702152911109,-6.66749936513699));
#118182=CARTESIAN_POINT('',(3.17747883877563,3.65572482719221,-6.7936461649991));
#118183=CARTESIAN_POINT('',(3.01600784751012,3.6557248275383,-6.72901903065084));
#118184=CARTESIAN_POINT('',(3.68244608528429,3.5650918335834,-6.53372709883351));
#118185=CARTESIAN_POINT('Origin',(-0.104571314098206,3.4821786308546,0.158446455861564));
#118186=CARTESIAN_POINT('Ctrl Pts',(3.55961399212263,3.52567991522661,-6.31598355143909));
#118187=CARTESIAN_POINT('Ctrl Pts',(3.58009186818585,3.53257385728007,-6.35220138326043));
#118188=CARTESIAN_POINT('Ctrl Pts',(3.60057681230707,3.53929993065276,-6.38847601200459));
#118189=CARTESIAN_POINT('Ctrl Pts',(3.64151307537039,3.55242657230514,-6.46104598330199));
#118190=CARTESIAN_POINT('Ctrl Pts',(3.66198755634127,3.55883456248648,-6.49738239230802));
#118191=CARTESIAN_POINT('Ctrl Pts',(3.68244608799738,3.56509182654294,-6.53372709851843));
#118192=CARTESIAN_POINT('Ctrl Pts',(4.18690496959621,3.66023518258216,-6.22321664433177));
#118193=CARTESIAN_POINT('Ctrl Pts',(4.17521286864247,3.65798000479108,-6.23101944800773));
#118194=CARTESIAN_POINT('Ctrl Pts',(4.16352076768874,3.655724827,-6.2388222516838));
#118195=CARTESIAN_POINT('Ctrl Pts',(3.82386004954764,3.590210912,-6.46549715900866));
#118196=CARTESIAN_POINT('Ctrl Pts',(3.46159810317059,3.524902621,-6.65395723145168));
#118197=CARTESIAN_POINT('Ctrl Pts',(4.24254189986292,3.66023518258215,-5.87912210056792));
#118198=CARTESIAN_POINT('Ctrl Pts',(4.23149426243145,3.65798000479108,-5.887031588284));
#118199=CARTESIAN_POINT('Ctrl Pts',(4.220446625,3.655724827,-5.894941076));
#118200=CARTESIAN_POINT('Ctrl Pts',(3.899507858,3.590210912,-6.124715202));
#118201=CARTESIAN_POINT('Ctrl Pts',(3.555520741,3.524902621,-6.318288713));
#118202=CARTESIAN_POINT('',(4.1636372344602,3.65572482796924,-6.23811875514344));
#118203=CARTESIAN_POINT('Origin',(-0.103018465060341,3.62500078945646,0.16322552726801));
#118204=CARTESIAN_POINT('',(4.19204192424133,3.65572482783619,-6.06652989444278));
#118205=CARTESIAN_POINT('Origin',(1.70219741080224E-13,3.74685310400067,
-4.30645102911242E-13));
#118206=CARTESIAN_POINT('',(3.67739665309663,3.74576903894327,-6.53657049634743));
#118207=CARTESIAN_POINT('Origin',(-0.0768314298786682,3.62500687472217,
0.175937908449575));
#118208=CARTESIAN_POINT('Origin',(-0.123735352695494,3.48232183506359,0.135690896681645));
#118209=CARTESIAN_POINT('Ctrl Pts',(5.184990765,3.524895017,-5.419028581));
#118210=CARTESIAN_POINT('Ctrl Pts',(4.888863046,3.590632927,-5.702367093));
#118211=CARTESIAN_POINT('Ctrl Pts',(4.56362425700001,3.655724827,-5.951750469));
#118212=CARTESIAN_POINT('Ctrl Pts',(4.56038470012501,3.65637317805554,-5.95423446432146));
#118213=CARTESIAN_POINT('Ctrl Pts',(4.55714514325,3.65702152911109,-5.95671845964291));
#118214=CARTESIAN_POINT('Ctrl Pts',(4.837666293,3.524895017,-5.3999523));
#118215=CARTESIAN_POINT('Ctrl Pts',(4.542581014,3.590632927,-5.664310951));
#118216=CARTESIAN_POINT('Ctrl Pts',(4.220446625,3.655724827,-5.894941076));
#118217=CARTESIAN_POINT('Ctrl Pts',(4.21723798965313,3.65637317805554,-5.89723827864709));
#118218=CARTESIAN_POINT('Ctrl Pts',(4.21402935430626,3.65702152911109,-5.89953548129418));
#118219=CARTESIAN_POINT('',(4.56362425617658,3.65572482719341,-5.95175046836352));
#118220=CARTESIAN_POINT('',(4.39203544364972,3.6557248275383,-5.92334577053529));
#118221=CARTESIAN_POINT('',(5.00091073256986,3.56509183364167,-5.5893551342245));
#118222=CARTESIAN_POINT('Origin',(-0.136187625454915,3.48217863687975,0.13226210935372));
#118223=CARTESIAN_POINT('Ctrl Pts',(4.83414195973404,3.52567991526989,-5.40310757969719));
#118224=CARTESIAN_POINT('Ctrl Pts',(4.86192683761031,3.53257385730368,-5.43407652037869));
#118225=CARTESIAN_POINT('Ctrl Pts',(4.88973082787118,3.53929993065564,-5.46509941075241));
#118226=CARTESIAN_POINT('Ctrl Pts',(4.94531042240983,3.55242657232849,-5.52717264983697));
#118227=CARTESIAN_POINT('Ctrl Pts',(4.97311747519163,3.55883456253002,-5.5582581256464));
#118228=CARTESIAN_POINT('Ctrl Pts',(5.00091073518349,3.56509182660111,-5.58935513330523));
#118229=CARTESIAN_POINT('Ctrl Pts',(5.42682507887805,3.66023518234146,-5.17766049455861));
#118230=CARTESIAN_POINT('Ctrl Pts',(5.41708370537352,3.65798000467073,-5.18779432855361));
#118231=CARTESIAN_POINT('Ctrl Pts',(5.40734233186913,3.655724827,-5.19792816254849));
#118232=CARTESIAN_POINT('Ctrl Pts',(5.1243510961745,3.590210912,-5.49232055015615));
#118233=CARTESIAN_POINT('Ctrl Pts',(4.8110719779955,3.524902621,-5.75425014158161));
#118234=CARTESIAN_POINT('Ctrl Pts',(5.40719109246663,3.66023518234146,-4.82965039351245));
#118235=CARTESIAN_POINT('Ctrl Pts',(5.3981020492333,3.65798000467073,-4.83974987675623));
#118236=CARTESIAN_POINT('Ctrl Pts',(5.389013006,3.655724827,-4.84984936));
#118237=CARTESIAN_POINT('Ctrl Pts',(5.124972255,3.590210912,-5.143243843));
#118238=CARTESIAN_POINT('Ctrl Pts',(4.830639948,3.524902621,-5.406238775));
#118239=CARTESIAN_POINT('',(5.40730484475352,3.65572482796924,-5.1972160764868));
#118240=CARTESIAN_POINT('Origin',(-0.135698834732586,3.62500078415649,0.137263720372715));
#118241=CARTESIAN_POINT('',(5.39815891547351,3.65572482783619,-5.02353269878948));
#118242=CARTESIAN_POINT('Origin',(-6.48352899146332E-13,3.74685310400033,
7.49834222490975E-13));
#118243=CARTESIAN_POINT('',(4.99659059976157,3.7457690389762,-5.59321753308891));
#118244=CARTESIAN_POINT('Origin',(-0.112856569653407,3.62500690610598,0.155308033448146));
#118245=CARTESIAN_POINT('Origin',(-0.150011969543891,3.48232183530511,0.105919035512763));
#118246=CARTESIAN_POINT('Ctrl Pts',(6.228699522,3.524895017,-4.177714957));
#118247=CARTESIAN_POINT('Ctrl Pts',(6.000404509,3.590632927,-4.518087878));
#118248=CARTESIAN_POINT('Ctrl Pts',(5.736379676,3.655724827,-4.831557535));
#118249=CARTESIAN_POINT('Ctrl Pts',(5.73374984372955,3.65637317805554,-4.83467986485974));
#118250=CARTESIAN_POINT('Ctrl Pts',(5.73112001145909,3.65702152911109,-4.83780219471947));
#118251=CARTESIAN_POINT('Ctrl Pts',(5.885394466,3.524895017,-4.233749163));
#118252=CARTESIAN_POINT('Ctrl Pts',(5.654037413,3.590632927,-4.555361869));
#118253=CARTESIAN_POINT('Ctrl Pts',(5.389013006,3.655724827,-4.84984936));
#118254=CARTESIAN_POINT('Ctrl Pts',(5.3863732174238,3.65637317805554,-4.8527826170663));
#118255=CARTESIAN_POINT('Ctrl Pts',(5.38373342884759,3.65702152911109,-4.85571587413261));
#118256=CARTESIAN_POINT('',(5.73637967537562,3.65572482719222,-4.83155753418609));
#118257=CARTESIAN_POINT('',(5.56269634316541,3.6557248275383,-4.84070344501162));
#118258=CARTESIAN_POINT('',(6.08553835246286,3.56509183360283,-4.38363113539836));
#118259=CARTESIAN_POINT('Origin',(-0.161436092508902,3.48217862844388,0.099893592570503));
#118260=CARTESIAN_POINT('Ctrl Pts',(5.88263082197757,3.52567991525343,-4.23758830135811));
#118261=CARTESIAN_POINT('Ctrl Pts',(5.91642351169788,3.53257385731059,-4.26186027829801));
#118262=CARTESIAN_POINT('Ctrl Pts',(5.95024646463923,3.5392999306834,-4.28618083490518));
#118263=CARTESIAN_POINT('Ctrl Pts',(6.0178705506578,3.55242657233255,-4.33485486628895));
#118264=CARTESIAN_POINT('Ctrl Pts',(6.05170994837978,3.5588345625107,-4.35923588648579));
#118265=CARTESIAN_POINT('Ctrl Pts',(6.08553835480099,3.56509182656289,-4.38363113396183));
#118266=CARTESIAN_POINT('Ctrl Pts',(6.41299288018051,3.66023518264005,-3.89000269152138));
#118267=CARTESIAN_POINT('Ctrl Pts',(6.40565772889045,3.65798000482003,-3.90199371024413));
#118268=CARTESIAN_POINT('Ctrl Pts',(6.39832257760057,3.655724827,-3.91398472896682));
#118269=CARTESIAN_POINT('Ctrl Pts',(6.18523318223122,3.590210912,-4.26232913639525));
#118270=CARTESIAN_POINT('Ctrl Pts',(5.93558547476414,3.524902621,-4.58548070971702));
#118271=CARTESIAN_POINT('Ctrl Pts',(6.31900604215917,3.66023518264005,-3.55434960027559));
#118272=CARTESIAN_POINT('Ctrl Pts',(6.31230058557958,3.65798000482002,-3.56616683963779));
#118273=CARTESIAN_POINT('Ctrl Pts',(6.305595129,3.655724827,-3.577984079));
#118274=CARTESIAN_POINT('Ctrl Pts',(6.11079864400001,3.590210912,-3.921280119));
#118275=CARTESIAN_POINT('Ctrl Pts',(5.8798838,3.524902621,-4.241399121));
#118276=CARTESIAN_POINT('',(6.39813288944175,3.65572482796921,-3.91329734966681));
#118277=CARTESIAN_POINT('Origin',(-0.162033723642388,3.625000821317,0.104883187102724));
#118278=CARTESIAN_POINT('',(6.35186399537058,3.65572482783619,-3.74564069745897));
#118279=CARTESIAN_POINT('Origin',(-1.09504419421036E-12,3.74685310400022,
8.21391565875018E-13));
#118280=CARTESIAN_POINT('',(6.08214952370044,3.74576903895158,-4.38833193457553));
#118281=CARTESIAN_POINT('Origin',(-0.143604888526815,3.62500691428628,0.127416356990091));
#118282=CARTESIAN_POINT('Origin',(-0.169274007653364,3.48232181604004,0.0711943981419716));
#118283=CARTESIAN_POINT('Ctrl Pts',(6.981161212,3.524895017,-2.741056025));
#118284=CARTESIAN_POINT('Ctrl Pts',(6.831373726,3.590632927,-3.122547895));
#118285=CARTESIAN_POINT('Ctrl Pts',(6.640908357,3.655724827,-3.485446341));
#118286=CARTESIAN_POINT('Ctrl Pts',(6.63901121737071,3.65637317805554,-3.48906100873161));
#118287=CARTESIAN_POINT('Ctrl Pts',(6.63711407774142,3.65702152911109,-3.49267567646322));
#118288=CARTESIAN_POINT('Ctrl Pts',(6.657928135,3.524895017,-2.869580621));
#118289=CARTESIAN_POINT('Ctrl Pts',(6.501117306,3.590632927,-3.233409128));
#118290=CARTESIAN_POINT('Ctrl Pts',(6.305595129,3.655724827,-3.577984079));
#118291=CARTESIAN_POINT('Ctrl Pts',(6.30364762078715,3.65637317805554,-3.58141623466291));
#118292=CARTESIAN_POINT('Ctrl Pts',(6.3017001125743,3.65702152911109,-3.58484839032582));
#118293=CARTESIAN_POINT('',(6.64090835621227,3.65572482719221,-3.48544634034164));
#118294=CARTESIAN_POINT('',(6.47325174457986,3.6557248275383,-3.5317152071043));
#118295=CARTESIAN_POINT('',(6.88561296283959,3.56509183365582,-2.9729334170755));
#118296=CARTESIAN_POINT('Origin',(-0.179136108976734,3.48217859046664,0.0628542098480828));
#118297=CARTESIAN_POINT('Ctrl Pts',(6.65605440467583,3.52567991529962,-2.8739241044273));
#118298=CARTESIAN_POINT('Ctrl Pts',(6.6942747977918,3.532573857343,-2.89036418659647));
#118299=CARTESIAN_POINT('Ctrl Pts',(6.73253518976221,3.53929993071124,-2.90684520700562));
#118300=CARTESIAN_POINT('Ctrl Pts',(6.80904174042197,3.55242657236825,-2.93984408706979));
#118301=CARTESIAN_POINT('Ctrl Pts',(6.84733119056229,3.55883456255224,-2.95638062236419));
#118302=CARTESIAN_POINT('Ctrl Pts',(6.88561296482973,3.56509182661546,-2.97293341513429));
#118303=CARTESIAN_POINT('Ctrl Pts',(7.09929626144607,3.66023518257403,-2.42045268846277));
#118304=CARTESIAN_POINT('Ctrl Pts',(7.09471031655864,3.65798000478701,-2.43374020435282));
#118305=CARTESIAN_POINT('Ctrl Pts',(7.09012437167135,3.655724827,-2.44702772024295));
#118306=CARTESIAN_POINT('Ctrl Pts',(6.95690063859252,3.590210912,-2.83303595054817));
#118307=CARTESIAN_POINT('Ctrl Pts',(6.7825575919012,3.524902621,-3.20229929665602));
#118308=CARTESIAN_POINT('Ctrl Pts',(6.93535129000859,3.66023518257402,-2.11285137176261));
#118309=CARTESIAN_POINT('Ctrl Pts',(6.93134296050429,3.65798000478701,-2.12583380538133));
#118310=CARTESIAN_POINT('Ctrl Pts',(6.927334631,3.655724827,-2.138816239));
#118311=CARTESIAN_POINT('Ctrl Pts',(6.810890881,3.590210912,-2.515961694));
#118312=CARTESIAN_POINT('Ctrl Pts',(6.65419082,3.524902621,-2.878236358));
#118313=CARTESIAN_POINT('',(7.0897913521598,3.65572482796968,-2.44639718807978));
#118314=CARTESIAN_POINT('Origin',(-0.180792207890397,3.62500079491804,0.067598601871706));
#118315=CARTESIAN_POINT('',(7.0085629743906,3.65572482783619,-2.29260670041997));
#118316=CARTESIAN_POINT('Origin',(-1.05904868208384E-12,3.74685310399967,
4.43005007677577E-13));
#118317=CARTESIAN_POINT('',(6.88331389544986,3.74576903895486,-2.97825281201177));
#118318=CARTESIAN_POINT('Origin',(-0.167638058101914,3.62500693769422,0.0935665359519333));
#118319=CARTESIAN_POINT('Origin',(-0.180621310204258,3.48232174501777,0.03314105327856));
#118320=CARTESIAN_POINT('Ctrl Pts',(7.407191563,3.524895017,-1.176228359));
#118321=CARTESIAN_POINT('Ctrl Pts',(7.3429155,3.590632927,-1.581001044));
#118322=CARTESIAN_POINT('Ctrl Pts',(7.23491554400001,3.655724827,-1.976359549));
#118323=CARTESIAN_POINT('Ctrl Pts',(7.23383980515275,3.65637317805554,-1.98029753673787));
#118324=CARTESIAN_POINT('Ctrl Pts',(7.2327640663055,3.65702152911109,-1.98423552447575));
#118325=CARTESIAN_POINT('Ctrl Pts',(7.119144485,3.524895017,-1.371233679));
#118326=CARTESIAN_POINT('Ctrl Pts',(7.04421218,3.590632927,-1.76026577));
#118327=CARTESIAN_POINT('Ctrl Pts',(6.927334631,3.655724827,-2.138816239));
#118328=CARTESIAN_POINT('Ctrl Pts',(6.9261704664532,3.65637317805554,-2.14258680947271));
#118329=CARTESIAN_POINT('Ctrl Pts',(6.92500630190641,3.65702152911109,-2.14635737994542));
#118330=CARTESIAN_POINT('',(7.23491554310333,3.65572482719222,-1.97635954850634));
#118331=CARTESIAN_POINT('',(7.08112508842043,3.6557248275383,-2.05758789083237));
#118332=CARTESIAN_POINT('',(7.36372396347785,3.5650918336313,-1.42322463610039));
#118333=CARTESIAN_POINT('Origin',(-0.18845974150441,3.48217865323327,0.0228757456814541));
#118334=CARTESIAN_POINT('Ctrl Pts',(7.11824828163573,3.52567991527641,-1.37587841094358));
#118335=CARTESIAN_POINT('Ctrl Pts',(7.15910923468992,3.53257385730954,-1.38371787822706));
#118336=CARTESIAN_POINT('Ctrl Pts',(7.20001805195165,3.53929993065615,-1.39158872810488));
#118337=CARTESIAN_POINT('Ctrl Pts',(7.28182970571336,3.55242657232356,-1.40736946568701));
#118338=CARTESIAN_POINT('Ctrl Pts',(7.32277883614221,3.5588345625215,-1.41528828600276));
#118339=CARTESIAN_POINT('Ctrl Pts',(7.36372396500073,3.56509182659103,-1.42322463379433));
#118340=CARTESIAN_POINT('Ctrl Pts',(7.45364443950742,3.6602351826602,-0.837725005818015));
#118341=CARTESIAN_POINT('Ctrl Pts',(7.45202213458921,3.6579800048301,-0.851687709842381));
#118342=CARTESIAN_POINT('Ctrl Pts',(7.45039982967101,3.655724827,-0.865650413866756));
#118343=CARTESIAN_POINT('Ctrl Pts',(7.40327115312175,3.590210912,-1.27127315120231));
#118344=CARTESIAN_POINT('Ctrl Pts',(7.31238485399817,3.524902621,-1.66938192753812));
#118345=CARTESIAN_POINT('Ctrl Pts',(7.22740722112359,3.6602351826602,-0.572558560699135));
#118346=CARTESIAN_POINT('Ctrl Pts',(7.22628344356181,3.6579800048301,-0.586099144849566));
#118347=CARTESIAN_POINT('Ctrl Pts',(7.225159666,3.655724827,-0.599639729));
#118348=CARTESIAN_POINT('Ctrl Pts',(7.19251343,3.590210912,-0.992999697));
#118349=CARTESIAN_POINT('Ctrl Pts',(7.11735527300001,3.524902621,-1.380490461));
#118350=CARTESIAN_POINT('',(7.44993905018901,3.65572482796966,-0.865106212554298));
#118351=CARTESIAN_POINT('Origin',(-0.1910970176312,3.62500080004091,0.0271531853036942));
#118352=CARTESIAN_POINT('',(7.33754933848588,3.65572482783619,-0.732372961650914));
#118353=CARTESIAN_POINT('Origin',(5.8113236445223E-14,3.74685310400044,
-2.49908600757909E-14));
#118354=CARTESIAN_POINT('',(7.36262215976636,3.74576903890217,-1.42891389836548));
#118355=CARTESIAN_POINT('Origin',(-0.18383269441779,3.62500689138061,0.0553417618585858));
#118356=CARTESIAN_POINT('Origin',(-0.18352264207554,3.48232177509209,-0.00646204176435239));
#118357=CARTESIAN_POINT('Ctrl Pts',(7.486869868,3.524895017,0.443598437));
#118358=CARTESIAN_POINT('Ctrl Pts',(7.511110706,3.590632927,0.03447166));
#118359=CARTESIAN_POINT('Ctrl Pts',(7.490626122,3.655724827,-0.374860382));
#118360=CARTESIAN_POINT('Ctrl Pts',(7.49042208429856,3.65637317805554,-0.378937553837026));
#118361=CARTESIAN_POINT('Ctrl Pts',(7.49021804659711,3.65702152911109,-0.383014725674051));
#118362=CARTESIAN_POINT('Ctrl Pts',(7.24747755100001,3.524895017,0.191230626));
#118363=CARTESIAN_POINT('Ctrl Pts',(7.257927521,3.590632927,-0.204814342));
#118364=CARTESIAN_POINT('Ctrl Pts',(7.225159666,3.655724827,-0.599639729));
#118365=CARTESIAN_POINT('Ctrl Pts',(7.22483328017661,3.65637317805554,-0.603572406589943));
#118366=CARTESIAN_POINT('Ctrl Pts',(7.22450689435324,3.65702152911109,-0.607505084179886));
#118367=CARTESIAN_POINT('',(7.35789289421796,3.6557248275383,-0.487250052208563));
#118368=CARTESIAN_POINT('Ctrl Pts',(7.24760078043643,3.52567991527447,0.186501828081928));
#118369=CARTESIAN_POINT('Ctrl Pts',(7.28919168065719,3.53257385729426,0.187629540275512));
#118370=CARTESIAN_POINT('Ctrl Pts',(7.33083607233944,3.53929993063177,0.188736892956231));
#118371=CARTESIAN_POINT('Ctrl Pts',(7.41412740695866,3.55242657232097,0.190912187476825));
#118372=CARTESIAN_POINT('Ctrl Pts',(7.45582148165056,3.55883456253418,0.19198135736837));
#118373=CARTESIAN_POINT('Ctrl Pts',(7.49751541623966,3.56509182662043,0.193032549343876));
#118374=CARTESIAN_POINT('Ctrl Pts',(7.45946848896609,3.66023518245835,0.784173763584061));
#118375=CARTESIAN_POINT('Ctrl Pts',(7.46088568114384,3.65798000472918,0.770188752851863));
#118376=CARTESIAN_POINT('Ctrl Pts',(7.46230287332171,3.655724827,0.756203742119653));
#118377=CARTESIAN_POINT('Ctrl Pts',(7.50347293574159,3.590210912,0.349932966859502));
#118378=CARTESIAN_POINT('Ctrl Pts',(7.50029312680127,3.524902621,-0.0584061149389999));
#118379=CARTESIAN_POINT('Ctrl Pts',(7.18151762197959,3.66023518245835,0.99450645132611));
#118380=CARTESIAN_POINT('Ctrl Pts',(7.18333094298972,3.65798000472918,0.981040860163056));
#118381=CARTESIAN_POINT('Ctrl Pts',(7.18514426400001,3.655724827,0.967575269));
#118382=CARTESIAN_POINT('Ctrl Pts',(7.237822045,3.590210912,0.576393863));
#118383=CARTESIAN_POINT('Ctrl Pts',(7.247720104,3.524902621,0.181805635));
#118384=CARTESIAN_POINT('',(7.32344005060519,3.65572482783619,0.862105722358991));
#118385=CARTESIAN_POINT('Ctrl Pts',(7.21647046,3.524895017,2.042683064));
#118386=CARTESIAN_POINT('Ctrl Pts',(7.328094724,3.590632927,1.648332506));
#118387=CARTESIAN_POINT('Ctrl Pts',(7.396083347,3.655724827,1.24416684));
#118388=CARTESIAN_POINT('Ctrl Pts',(7.39676055100675,3.65637317805554,1.24014112810397));
#118389=CARTESIAN_POINT('Ctrl Pts',(7.39743775501351,3.65702152911109,1.23611541620793));
#118390=CARTESIAN_POINT('Ctrl Pts',(7.036926621,3.524895017,1.7447532));
#118391=CARTESIAN_POINT('Ctrl Pts',(7.132270238,3.590632927,1.360213978));
#118392=CARTESIAN_POINT('Ctrl Pts',(7.18514426400001,3.655724827,0.967575269));
#118393=CARTESIAN_POINT('Ctrl Pts',(7.18567091832362,3.65637317805554,0.963664371923291));
#118394=CARTESIAN_POINT('Ctrl Pts',(7.18619757264725,3.65702152911109,0.959753474846583));
#118395=CARTESIAN_POINT('',(7.39608334597518,3.65572482719222,1.24416684004987));
#118396=CARTESIAN_POINT('',(7.29061380500531,3.6557248275383,1.10587105776134));
#118397=CARTESIAN_POINT('',(7.28073138003579,3.56509183364385,1.80026374265344));
#118398=CARTESIAN_POINT('Origin',(-0.180646895504575,3.48217863662677,-0.0583707780274595));
#118399=CARTESIAN_POINT('Ctrl Pts',(7.03806352124642,3.52567991521218,1.7401614500682));
#118400=CARTESIAN_POINT('Ctrl Pts',(7.07843962488291,3.53257385728293,1.7502036110421));
#118401=CARTESIAN_POINT('Ctrl Pts',(7.11887234611513,3.53929993067132,1.76023738760649));
#118402=CARTESIAN_POINT('Ctrl Pts',(7.19974875170204,3.55242657234967,1.78026699959728));
#118403=CARTESIAN_POINT('Ctrl Pts',(7.24023820213086,3.55883456254047,1.79027416635503));
#118404=CARTESIAN_POINT('Ctrl Pts',(7.28073138044745,3.56509182660367,1.80026374539461));
#118405=CARTESIAN_POINT('Ctrl Pts',(7.11649608109494,3.66023518243807,2.36940544160283));
#118406=CARTESIAN_POINT('Ctrl Pts',(7.12088650402253,3.65798000471904,2.35605204714253));
#118407=CARTESIAN_POINT('Ctrl Pts',(7.12527692695003,3.655724827,2.34269865268223));
#118408=CARTESIAN_POINT('Ctrl Pts',(7.25282066421712,3.590210912,1.95477660900104));
#118409=CARTESIAN_POINT('Ctrl Pts',(7.33749603053574,3.524902621,1.55530070319499));
#118410=CARTESIAN_POINT('Ctrl Pts',(6.79982824183194,3.66023518243808,2.51506944727944));
#118411=CARTESIAN_POINT('Ctrl Pts',(6.8044938724159,3.65798000471904,2.50230848463969));
#118412=CARTESIAN_POINT('Ctrl Pts',(6.809159503,3.655724827,2.489547522));
#118413=CARTESIAN_POINT('Ctrl Pts',(6.944698145,3.590210912,2.118835886));
#118414=CARTESIAN_POINT('Ctrl Pts',(7.039189599,3.524902621,1.735600702));
#118415=CARTESIAN_POINT('',(7.1246302310521,3.65572482796922,2.34299907947824));
#118416=CARTESIAN_POINT('Origin',(-0.184836620676564,3.62500080738618,-0.0555960842180652));
#118417=CARTESIAN_POINT('',(6.96689484519621,3.65572482783619,2.41627330110929));
#118418=CARTESIAN_POINT('Origin',(5.73759789679329E-13,3.74685310399911,
1.59052458703624E-13));
#118419=CARTESIAN_POINT('',(7.2821202696205,3.74576903894091,1.79463767308797));
#118420=CARTESIAN_POINT('Origin',(-0.190079571027402,3.6250068814924,-0.0269625511958518));
#118421=CARTESIAN_POINT('Origin',(-0.163847624695173,3.48232176305973,-0.0829240434496378));
#118422=CARTESIAN_POINT('Ctrl Pts',(6.608636913,3.524895017,3.546254101));
#118423=CARTESIAN_POINT('Ctrl Pts',(6.802425177,3.590632927,3.185119157));
#118424=CARTESIAN_POINT('Ctrl Pts',(6.955707935,3.655724827,2.805018204));
#118425=CARTESIAN_POINT('Ctrl Pts',(6.95723471541271,3.65637317805554,2.80123218985553));
#118426=CARTESIAN_POINT('Ctrl Pts',(6.95876149582542,3.65702152911109,2.79744617571105));
#118427=CARTESIAN_POINT('Ctrl Pts',(6.497336824,3.524895017,3.216693053));
#118428=CARTESIAN_POINT('Ctrl Pts',(6.673115926,3.590632927,2.861640204));
#118429=CARTESIAN_POINT('Ctrl Pts',(6.809159503,3.655724827,2.489547522));
#118430=CARTESIAN_POINT('Ctrl Pts',(6.81051457170667,3.65637317805554,2.48584127463075));
#118431=CARTESIAN_POINT('Ctrl Pts',(6.81186964041335,3.65702152911109,2.48213502726149));
#118432=CARTESIAN_POINT('',(6.95570793398814,3.65572482719221,2.8050182038267));
#118433=CARTESIAN_POINT('',(6.88243371781578,3.6557248275383,2.64728286607875));
#118434=CARTESIAN_POINT('',(6.72350843674559,3.56509183364709,3.32331660677712));
#118435=CARTESIAN_POINT('Origin',(-0.163875473105116,3.48217864288177,-0.0958398440449543));
#118436=CARTESIAN_POINT('Ctrl Pts',(6.49943423469484,3.52567991526485,3.21245305500109));
#118437=CARTESIAN_POINT('Ctrl Pts',(6.53670759947093,3.53257385731295,3.23094010477315));
#118438=CARTESIAN_POINT('Ctrl Pts',(6.5740380605636,3.53929993067782,3.24943113723722));
#118439=CARTESIAN_POINT('Ctrl Pts',(6.64871784602487,3.55242657234897,3.28637850488452));
#118440=CARTESIAN_POINT('Ctrl Pts',(6.68610943050522,3.55883456254205,3.30485574479466));
#118441=CARTESIAN_POINT('Ctrl Pts',(6.72350843655732,3.56509182660701,3.32331660954475));
#118442=CARTESIAN_POINT('Ctrl Pts',(6.44076422642631,3.660235182589,3.84384635591007));
#118443=CARTESIAN_POINT('Ctrl Pts',(6.44792258902591,3.6579800047945,3.83174896713056));
#118444=CARTESIAN_POINT('Ctrl Pts',(6.45508095162562,3.655724827,3.81965157835112));
#118445=CARTESIAN_POINT('Ctrl Pts',(6.663034559558,3.590210912,3.46821706966159));
#118446=CARTESIAN_POINT('Ctrl Pts',(6.83160577317824,3.524902621,3.09628338849629));
#118447=CARTESIAN_POINT('Ctrl Pts',(6.1001864494939,3.660235182589,3.91803059333484));
#118448=CARTESIAN_POINT('Ctrl Pts',(6.10748623024694,3.6579800047945,3.90657094716742));
#118449=CARTESIAN_POINT('Ctrl Pts',(6.114786011,3.655724827,3.895111301));
#118450=CARTESIAN_POINT('Ctrl Pts',(6.326847879,3.590210912,3.562203498));
#118451=CARTESIAN_POINT('Ctrl Pts',(6.501514411,3.524902621,3.208241008));
#118452=CARTESIAN_POINT('',(6.45438479219936,3.65572482796923,3.81980596085165));
#118453=CARTESIAN_POINT('Origin',(-0.168563572421865,3.62500081258431,-0.0940305921459722));
#118454=CARTESIAN_POINT('',(6.28458538020791,3.65572482783619,3.85745862658826));
#118455=CARTESIAN_POINT('Origin',(-1.34441069388203E-12,3.74685310400044,
-6.36426675248991E-13));
#118456=CARTESIAN_POINT('',(6.72607429379896,3.74576903896969,3.31812064153517));
#118457=CARTESIAN_POINT('Origin',(-0.179839597766256,3.62500689088592,-0.0671937332775935));
#118458=CARTESIAN_POINT('Origin',(-0.142191017882454,3.48232181496895,-0.116207852334306));
#118459=CARTESIAN_POINT('Ctrl Pts',(5.69179085,3.524895017,4.884006237));
#118460=CARTESIAN_POINT('Ctrl Pts',(5.958681789,3.590632927,4.572973176));
#118461=CARTESIAN_POINT('Ctrl Pts',(6.190091351,3.655724827,4.234710034));
#118462=CARTESIAN_POINT('Ctrl Pts',(6.19239631726747,3.65637317805554,4.23134074741953));
#118463=CARTESIAN_POINT('Ctrl Pts',(6.19470128353494,3.65702152911109,4.22797146083906));
#118464=CARTESIAN_POINT('Ctrl Pts',(5.653938778,3.524895017,4.538223914));
#118465=CARTESIAN_POINT('Ctrl Pts',(5.90193413,3.590632927,4.229259314));
#118466=CARTESIAN_POINT('Ctrl Pts',(6.114786011,3.655724827,3.895111301));
#118467=CARTESIAN_POINT('Ctrl Pts',(6.11690613257765,3.65637317805554,3.89178300336333));
#118468=CARTESIAN_POINT('Ctrl Pts',(6.11902625415531,3.65702152911109,3.88845470572666));
#118469=CARTESIAN_POINT('',(6.19009135031808,3.65572482719341,4.23471003320417));
#118470=CARTESIAN_POINT('',(6.15243867918163,3.6557248275383,4.06491067025219));
#118471=CARTESIAN_POINT('',(5.85190171216796,3.56509183364086,4.69097487982885));
#118472=CARTESIAN_POINT('Origin',(-0.139441555156309,3.48217860768295,-0.128827649737256));
#118473=CARTESIAN_POINT('Ctrl Pts',(5.65689862657596,3.52567991524778,4.53453392617591));
#118474=CARTESIAN_POINT('Ctrl Pts',(5.68932639171087,3.53257385728754,4.56060143058841));
#118475=CARTESIAN_POINT('Ctrl Pts',(5.72180906204669,3.53929993064708,4.58668509863778));
#118476=CARTESIAN_POINT('Ctrl Pts',(5.78680028387411,3.5524265723281,4.63882260382768));
#118477=CARTESIAN_POINT('Ctrl Pts',(5.81934561351409,3.55883456252675,4.66490594159134));
#118478=CARTESIAN_POINT('Ctrl Pts',(5.85190171139198,3.56509182660114,4.69097488248765));
#118479=CARTESIAN_POINT('Ctrl Pts',(5.46386939543312,3.66023518256184,5.13855328504425));
#118480=CARTESIAN_POINT('Ctrl Pts',(5.47346098040717,3.65798000478092,5.12827756291872));
#118481=CARTESIAN_POINT('Ctrl Pts',(5.48305256538124,3.655724827,5.11800184079321));
#118482=CARTESIAN_POINT('Ctrl Pts',(5.76169236399178,3.590210912,4.81948755442943));
#118483=CARTESIAN_POINT('Ctrl Pts',(6.00627722401707,3.524902621,4.4924873040965));
#118484=CARTESIAN_POINT('Ctrl Pts',(5.11530671890459,3.66023518256184,5.13778898070581));
#118485=CARTESIAN_POINT('Ctrl Pts',(5.12489931995231,3.65798000478092,5.1281664918529));
#118486=CARTESIAN_POINT('Ctrl Pts',(5.134491921,3.655724827,5.118544003));
#118487=CARTESIAN_POINT('Ctrl Pts',(5.413161237,3.590210912,4.839006433));
#118488=CARTESIAN_POINT('Ctrl Pts',(5.659835635,3.524902621,4.530867531));
#118489=CARTESIAN_POINT('',(5.48233949409281,3.65572482796922,5.11800296022109));
#118490=CARTESIAN_POINT('Origin',(-0.144408942952712,3.6250008350005,-0.128068477123946));
#118491=CARTESIAN_POINT('',(5.308415687593,3.65572482783619,5.11827347277353));
#118492=CARTESIAN_POINT('Origin',(2.91867224833098E-13,3.74685310399922,
2.51968584885631E-13));
#118493=CARTESIAN_POINT('',(5.85552455969037,3.74576903894377,4.68645197666851));
#118494=CARTESIAN_POINT('Origin',(-0.16119026828776,3.62500687370807,-0.104282894806315));
#118495=CARTESIAN_POINT('Origin',(-0.113885433031731,3.48232172951026,-0.144057869348729));
#118496=CARTESIAN_POINT('Ctrl Pts',(4.508802972,3.524895017,5.99338767));
#118497=CARTESIAN_POINT('Ctrl Pts',(4.836317064,3.590632927,5.747000052));
#118498=CARTESIAN_POINT('Ctrl Pts',(5.135032975,3.655724827,5.466391529));
#118499=CARTESIAN_POINT('Ctrl Pts',(5.13800834945065,3.65637317805554,5.46359651407369));
#118500=CARTESIAN_POINT('Ctrl Pts',(5.14098372390131,3.65702152911109,5.46080149914739));
#118501=CARTESIAN_POINT('Ctrl Pts',(4.546168838,3.524895017,5.647552469));
#118502=CARTESIAN_POINT('Ctrl Pts',(4.854784453,3.590632927,5.39912296));
#118503=CARTESIAN_POINT('Ctrl Pts',(5.134491921,3.655724827,5.118544003));
#118504=CARTESIAN_POINT('Ctrl Pts',(5.13727796092388,3.65637317805554,5.11574928256728));
#118505=CARTESIAN_POINT('Ctrl Pts',(5.14006400084776,3.65702152911109,5.11295456213456));
#118506=CARTESIAN_POINT('',(5.13503297415595,3.65572482719221,5.46639152841513));
#118507=CARTESIAN_POINT('',(5.1347624456325,3.6557248275383,5.29246776829695));
#118508=CARTESIAN_POINT('',(4.70666656738194,3.56509183363972,5.83928838101205));
#118509=CARTESIAN_POINT('Origin',(-0.108487181196059,3.48217862674873,-0.155791336103154));
#118510=CARTESIAN_POINT('Ctrl Pts',(4.54985272534518,3.5256799152631,5.64458503093839));
#118511=CARTESIAN_POINT('Ctrl Pts',(4.57591860460814,3.53257385730365,5.67701410253778));
#118512=CARTESIAN_POINT('Ctrl Pts',(4.60203463073502,3.5392999306659,5.70947076287906));
#118513=CARTESIAN_POINT('Ctrl Pts',(4.6542983717518,3.55242657233496,5.77436051365568));
#118514=CARTESIAN_POINT('Ctrl Pts',(4.68047566321139,3.5588345625283,5.80683032126513));
#118515=CARTESIAN_POINT('Ctrl Pts',(4.70666656605314,3.56509182659974,5.83928838344145));
#118516=CARTESIAN_POINT('Ctrl Pts',(4.23149010313324,3.66023518260803,6.1929871736484));
#118517=CARTESIAN_POINT('Ctrl Pts',(4.24306641882883,3.65798000480402,6.18501359937273));
#118518=CARTESIAN_POINT('Ctrl Pts',(4.25464273452441,3.655724827,6.17704002509703));
#118519=CARTESIAN_POINT('Ctrl Pts',(4.59093983763609,3.590210912,5.94540415744501));
#118520=CARTESIAN_POINT('Ctrl Pts',(4.90010182696033,3.524902621,5.67862750629276));
#118521=CARTESIAN_POINT('Ctrl Pts',(3.89124093061716,3.66023518260803,6.11731006767163));
#118522=CARTESIAN_POINT('Ctrl Pts',(3.90267781280862,3.65798000480402,6.10997467283589));
#118523=CARTESIAN_POINT('Ctrl Pts',(3.914114695,3.655724827,6.102639278));
#118524=CARTESIAN_POINT('Ctrl Pts',(4.246361193,3.590210912,5.889542806));
#118525=CARTESIAN_POINT('Ctrl Pts',(4.553509235,3.524902621,5.641635724));
#118526=CARTESIAN_POINT('',(4.25394609309613,3.65572482796967,6.17688782937028));
#118527=CARTESIAN_POINT('Origin',(-0.113501710319515,3.62500081890866,-0.156117841935746));
#118528=CARTESIAN_POINT('',(4.08403037681007,3.65572482783619,6.13976354063303));
#118529=CARTESIAN_POINT('Origin',(2.14238349283136E-13,3.74685310400067,
3.43908929112402E-13));
#118530=CARTESIAN_POINT('',(4.71117700472489,3.74576903895635,5.83565002592714));
#118531=CARTESIAN_POINT('Origin',(-0.135004131882551,3.62500692857403,-0.136496139368398));
#118532=CARTESIAN_POINT('Origin',(-0.0802545157818219,3.48232179160699,
-0.165171658052808));
#118533=CARTESIAN_POINT('Ctrl Pts',(3.114988478,3.524895017,6.822524956));
#118534=CARTESIAN_POINT('Ctrl Pts',(3.487811527,3.590632927,6.652303593));
#118535=CARTESIAN_POINT('Ctrl Pts',(3.839866164,3.655724827,6.442470632));
#118536=CARTESIAN_POINT('Ctrl Pts',(3.84337282144137,3.65637317805554,6.44038058052275));
#118537=CARTESIAN_POINT('Ctrl Pts',(3.84687947888274,3.65702152911109,6.4382905290455));
#118538=CARTESIAN_POINT('Ctrl Pts',(3.225825097,3.524895017,6.492807747));
#118539=CARTESIAN_POINT('Ctrl Pts',(3.580630451,3.590632927,6.316529616));
#118540=CARTESIAN_POINT('Ctrl Pts',(3.914114695,3.655724827,6.102639278));
#118541=CARTESIAN_POINT('Ctrl Pts',(3.91743638113306,3.65637317805554,6.10050881282057));
#118542=CARTESIAN_POINT('Ctrl Pts',(3.92075806726612,3.65702152911109,6.09837834764114));
#118543=CARTESIAN_POINT('',(3.83986616329884,3.65572482719222,6.44247063125054));
#118544=CARTESIAN_POINT('',(3.87699042669408,3.6557248275383,6.27255495673431));
#118545=CARTESIAN_POINT('',(3.34135292461231,3.56509183369146,6.71456324749908));
#118546=CARTESIAN_POINT('Origin',(-0.0724602166674065,3.48217860567644,
-0.175470452308175));
#118547=CARTESIAN_POINT('Ctrl Pts',(3.230060768144,3.5256799151844,6.49070161308116));
#118548=CARTESIAN_POINT('Ctrl Pts',(3.24854594976219,3.53257385725448,6.52797590452752));
#118549=CARTESIAN_POINT('Ctrl Pts',(3.26707417510236,3.53929993064325,6.56528791979451));
#118550=CARTESIAN_POINT('Ctrl Pts',(3.30416664053201,3.55242657235513,6.63989574360624));
#118551=CARTESIAN_POINT('Ctrl Pts',(3.32275187260552,3.55883456256649,6.67723376899636));
#118552=CARTESIAN_POINT('Ctrl Pts',(3.3413529227585,3.56509182665127,6.71456324960291));
#118553=CARTESIAN_POINT('Ctrl Pts',(2.80125103830434,3.66023518240983,6.95784386525036));
#118554=CARTESIAN_POINT('Ctrl Pts',(2.81427078837048,3.65798000470493,6.95254527459315));
#118555=CARTESIAN_POINT('Ctrl Pts',(2.82729053843668,3.655724827,6.94724668393587));
#118556=CARTESIAN_POINT('Ctrl Pts',(3.20552006655533,3.590210912,6.79332026954184));
#118557=CARTESIAN_POINT('Ctrl Pts',(3.56480311451474,3.524902621,6.59924139770641));
#118558=CARTESIAN_POINT('Ctrl Pts',(2.48522504358556,3.66023518240984,6.81079253315187));
#118559=CARTESIAN_POINT('Ctrl Pts',(2.49797143029281,3.65798000470493,6.80608722757588));
#118560=CARTESIAN_POINT('Ctrl Pts',(2.510717817,3.655724827,6.801381922));
#118561=CARTESIAN_POINT('Ctrl Pts',(2.881006018,3.590210912,6.664690703));
#118562=CARTESIAN_POINT('Ctrl Pts',(3.234265804,3.524902621,6.488607301));
#118563=CARTESIAN_POINT('',(2.82664290169905,3.65572482796968,6.94694828916187));
#118564=CARTESIAN_POINT('Origin',(-0.0772874867209844,3.6250008063393,-0.176867614939211));
#118565=CARTESIAN_POINT('',(2.66868034532562,3.65572482783619,6.87416508912661));
#118566=CARTESIAN_POINT('Origin',(4.88758339356465E-13,3.74685310399989,
9.87925019568792E-13));
#118567=CARTESIAN_POINT('',(3.34654004947767,3.74576903895837,6.71197956588787));
#118568=CARTESIAN_POINT('Origin',(-0.102505000056622,3.62500693001679,-0.162326509812541));
#118569=CARTESIAN_POINT('Origin',(-0.0428713111393131,3.48232180333034,
-0.178562645459894));
#118570=CARTESIAN_POINT('Ctrl Pts',(1.575520586,3.524895017,7.332648559));
#118571=CARTESIAN_POINT('Ctrl Pts',(1.9762198,3.590632927,7.246552811));
#118572=CARTESIAN_POINT('Ctrl Pts',(2.365151479,3.655724827,7.11730696800001));
#118573=CARTESIAN_POINT('Ctrl Pts',(2.36902545202297,3.65637317805554,7.11601960845552));
#118574=CARTESIAN_POINT('Ctrl Pts',(2.37289942504594,3.65702152911109,7.11473224891103));
#118575=CARTESIAN_POINT('Ctrl Pts',(1.754645359,3.524895017,7.03446655100001));
#118576=CARTESIAN_POINT('Ctrl Pts',(2.139050148,3.590632927,6.938582368));
#118577=CARTESIAN_POINT('Ctrl Pts',(2.510717817,3.655724827,6.801381922));
#118578=CARTESIAN_POINT('Ctrl Pts',(2.51441983100647,3.65637317805554,6.80001533024304));
#118579=CARTESIAN_POINT('Ctrl Pts',(2.51812184501293,3.65702152911109,6.79864873848607));
#118580=CARTESIAN_POINT('',(2.36515147845739,3.65572482719223,7.11730696713216));
#118581=CARTESIAN_POINT('',(2.43793464488681,3.65572482753831,6.95934444609059));
#118582=CARTESIAN_POINT('',(1.81980133343817,3.5650918336497,7.27587259882722));
#118583=CARTESIAN_POINT('Origin',(-0.0330452042788285,3.48217859242297,
-0.186944949984029));
#118584=CARTESIAN_POINT('Ctrl Pts',(1.75923475895739,3.52567991519402,7.03332020162641));
#118585=CARTESIAN_POINT('Ctrl Pts',(1.76927489669448,3.53257385725999,7.07369680843662));
#118586=CARTESIAN_POINT('Ctrl Pts',(1.77934896227731,3.53929993064844,7.11411951025837));
#118587=CARTESIAN_POINT('Ctrl Pts',(1.79953575004537,3.55242657233731,7.1949568280426));
#118588=CARTESIAN_POINT('Ctrl Pts',(1.80965989807368,3.55883456253557,7.2354171865551));
#118589=CARTESIAN_POINT('Ctrl Pts',(1.81980133120497,3.56509182660936,7.27587260047597));
#118590=CARTESIAN_POINT('Ctrl Pts',(1.24002858623345,3.66023518253582,7.39735951019233));
#118591=CARTESIAN_POINT('Ctrl Pts',(1.25388298254613,3.65798000476791,7.39498365900624));
#118592=CARTESIAN_POINT('Ctrl Pts',(1.26773737885882,3.655724827,7.39260780782015));
#118593=CARTESIAN_POINT('Ctrl Pts',(1.67021374028811,3.590210912,7.32358827646765));
#118594=CARTESIAN_POINT('Ctrl Pts',(2.06281817067519,3.524902621,7.21128209545936));
#118595=CARTESIAN_POINT('Ctrl Pts',(0.963002793498291,3.66023518253582,
7.1858099096259));
#118596=CARTESIAN_POINT('Ctrl Pts',(0.976462678749152,3.65798000476791,
7.18395470781295));
#118597=CARTESIAN_POINT('Ctrl Pts',(0.989922564,3.655724827,7.182099506));
#118598=CARTESIAN_POINT('Ctrl Pts',(1.380938204,3.590210912,7.12820507));
#118599=CARTESIAN_POINT('Ctrl Pts',(1.763791699,3.524902621,7.032178812));
#118600=CARTESIAN_POINT('',(1.26716903033796,3.65572482796929,7.39217716664284));
#118601=CARTESIAN_POINT('Origin',(-0.037459188035332,3.62500079716236,-0.189346868690627));
#118602=CARTESIAN_POINT('',(1.12854578661594,3.65572482783626,7.28713831720771));
#118603=CARTESIAN_POINT('Origin',(3.20490162186715E-13,3.74685310399967,
1.17700987845026E-12));
#118604=CARTESIAN_POINT('',(1.82542260129696,3.7457690389737,7.274464401048));
#118605=CARTESIAN_POINT('Origin',(-0.0652131106448975,3.62500690827945,
-0.180566992370154));
#118606=CARTESIAN_POINT('Origin',(-0.00348321090670733,3.48232174858048,
-0.183603634743864));
#118607=CARTESIAN_POINT('Ctrl Pts',(-0.037616899,3.524895017,7.49990566400001));
#118608=CARTESIAN_POINT('Ctrl Pts',(0.372222232,3.590632927,7.501961273));
#118609=CARTESIAN_POINT('Ctrl Pts',(0.77984494,3.655724827,7.459345941));
#118610=CARTESIAN_POINT('Ctrl Pts',(0.783905085932064,3.65637317805554,
7.45892146890003));
#118611=CARTESIAN_POINT('Ctrl Pts',(0.787965231864128,3.65702152911109,
7.45849699680004));
#118612=CARTESIAN_POINT('Ctrl Pts',(0.201420355,3.524895017,7.247201518));
#118613=CARTESIAN_POINT('Ctrl Pts',(0.597450238,3.590632927,7.23619472));
#118614=CARTESIAN_POINT('Ctrl Pts',(0.989922563999999,3.655724827,7.182099506));
#118615=CARTESIAN_POINT('Ctrl Pts',(0.993831803810694,3.65637317805554,
7.18156068797354));
#118616=CARTESIAN_POINT('Ctrl Pts',(0.997741043621388,3.65702152911109,
7.18102186994708));
#118617=CARTESIAN_POINT('',(0.779844939665669,3.65572482719222,7.45934594003148));
#118618=CARTESIAN_POINT('',(0.88488374872519,3.6557248275383,7.32072272389584));
#118619=CARTESIAN_POINT('',(0.213157853479665,3.56509183362931,7.49697023446842));
#118620=CARTESIAN_POINT('Origin',(0.00791499949564178,3.48217862741154,
-0.189678175733404));
#118621=CARTESIAN_POINT('Ctrl Pts',(0.206148889001752,3.52567991523746,
7.24706855475945));
#118622=CARTESIAN_POINT('Ctrl Pts',(0.207274516531135,3.5325738572827,7.28865951157601));
#118623=CARTESIAN_POINT('Ctrl Pts',(0.208423369727975,3.5392999306431,7.33030277919583));
#118624=CARTESIAN_POINT('Ctrl Pts',(0.210760567333695,3.55242657232236,
7.4135897279966));
#118625=CARTESIAN_POINT('Ctrl Pts',(0.211950237156683,3.55883456252139,
7.45528053840675));
#118626=CARTESIAN_POINT('Ctrl Pts',(0.213157850959172,3.56509182658913,
7.4969702355981));
#118627=CARTESIAN_POINT('Ctrl Pts',(-0.379176222983314,3.66023518244822,
7.49098284762322));
#118628=CARTESIAN_POINT('Ctrl Pts',(-0.365134997269743,3.65798000472411,
7.49164082814761));
#118629=CARTESIAN_POINT('Ctrl Pts',(-0.351093771556175,3.655724827,7.49229880867192));
#118630=CARTESIAN_POINT('Ctrl Pts',(0.0568100748054015,3.590210912,7.51141343528446));
#118631=CARTESIAN_POINT('Ctrl Pts',(0.464378140806264,3.524902621,7.48613125750417));
#118632=CARTESIAN_POINT('Ctrl Pts',(-0.60424839578379,3.66023518244822,
7.22482680159335));
#118633=CARTESIAN_POINT('Ctrl Pts',(-0.590704381891892,3.65798000472411,
7.22590845079669));
#118634=CARTESIAN_POINT('Ctrl Pts',(-0.577160368,3.655724827,7.2269901));
#118635=CARTESIAN_POINT('Ctrl Pts',(-0.183700746,3.590210912,7.25841249));
#118636=CARTESIAN_POINT('Ctrl Pts',(0.210844655,3.524902621,7.24693345700001));
#118637=CARTESIAN_POINT('',(-0.351556258027216,3.65572482796968,7.4917560572968));
#118638=CARTESIAN_POINT('Origin',(0.00412055726725919,3.62500080754839,
-0.192972789225312));
#118639=CARTESIAN_POINT('',(-0.464358318833719,3.6557248278362,7.35937305782598));
#118640=CARTESIAN_POINT('Origin',(4.42896587460329E-14,3.74685310400067,
5.41233724504764E-13));
#118641=CARTESIAN_POINT('',(0.218950420586282,3.74576903894199,7.49680336605748));
#118642=CARTESIAN_POINT('Origin',(-0.0248718918509416,3.62500691765216,
-0.190364284633733));
#118643=CARTESIAN_POINT('Origin',(0.0360675772053069,3.48232171708846,-0.180060425093342));
#118644=CARTESIAN_POINT('Ctrl Pts',(0.467054599,2.232664075,7.485443207));
#118645=CARTESIAN_POINT('Ctrl Pts',(0.87318754,2.168401865,7.460102522));
#118646=CARTESIAN_POINT('Ctrl Pts',(1.274194673,2.103255924,7.39096935));
#118647=CARTESIAN_POINT('Ctrl Pts',(0.213937947,2.232664075,7.246842799));
#118648=CARTESIAN_POINT('Ctrl Pts',(0.607125298,2.168401865,7.235235304));
#118649=CARTESIAN_POINT('Ctrl Pts',(0.996748685,2.103255924,7.181155343));
#118650=CARTESIAN_POINT('',(0.992091960527736,2.10403448620838,7.18180016027124));
#118651=CARTESIAN_POINT('Origin',(-0.0408077731901307,2.01791740531367,
-0.190716934482191));
#118652=CARTESIAN_POINT('Ctrl Pts',(1.02848533315001,2.14301213123373,7.42914651317701));
#118653=CARTESIAN_POINT('Ctrl Pts',(1.02259958178598,2.1370611205462,7.38936730565107));
#118654=CARTESIAN_POINT('Ctrl Pts',(1.01650022449132,2.13073653553286,7.34805528870324));
#118655=CARTESIAN_POINT('Ctrl Pts',(1.00415932290291,2.11752971609119,7.26418729613499));
#118656=CARTESIAN_POINT('Ctrl Pts',(0.998112042998285,2.11086974920619,
7.22296771414384));
#118657=CARTESIAN_POINT('Ctrl Pts',(0.992091959548518,2.10403448636993,
7.18180016038761));
#118658=CARTESIAN_POINT('Ctrl Pts',(0.777222552,2.103262031,7.459619635));
#118659=CARTESIAN_POINT('Ctrl Pts',(0.902618358,2.123129682,7.446554566));
#118660=CARTESIAN_POINT('Ctrl Pts',(1.027504195,2.142857143,7.429282275));
#118661=CARTESIAN_POINT('Ctrl Pts',(1.309731339,2.187438859,7.390248953));
#118662=CARTESIAN_POINT('Ctrl Pts',(1.588183719,2.232664075,7.329916267));
#118663=CARTESIAN_POINT('Ctrl Pts',(0.98739763,2.103262031,7.182447071));
#118664=CARTESIAN_POINT('Ctrl Pts',(1.10813418,2.123129682,7.165848969));
#118665=CARTESIAN_POINT('Ctrl Pts',(1.228244647,2.142857143,7.145202243));
#118666=CARTESIAN_POINT('Ctrl Pts',(1.499680022,2.187438859,7.098543095));
#118667=CARTESIAN_POINT('Ctrl Pts',(1.766793184,2.232664075,7.031425307));
#118668=CARTESIAN_POINT('Ctrl Pts',(1.76679317507296,2.23266407348855,7.03142530924311));
#118669=CARTESIAN_POINT('Ctrl Pts',(1.62253262275256,2.20823916463419,7.06767380049264));
#118670=CARTESIAN_POINT('Ctrl Pts',(1.47748684829027,2.183982876726,7.09939539754149));
#118671=CARTESIAN_POINT('Ctrl Pts',(1.33207819674674,2.15996092288709,7.126574751153));
#118672=CARTESIAN_POINT('Ctrl Pts',(1.29748568338354,2.15424613390885,7.13304068108929));
#118673=CARTESIAN_POINT('Ctrl Pts',(1.2628726178915,2.14854459021232,7.13924977054086));
#118674=CARTESIAN_POINT('Ctrl Pts',(1.22824464580779,2.14285714281195,7.14520224326374));
#118675=CARTESIAN_POINT('Ctrl Pts',(1.14987371677628,2.12998516349532,7.15867403410597));
#118676=CARTESIAN_POINT('Ctrl Pts',(1.07113569834775,2.11704095619703,7.1708810795655));
#118677=CARTESIAN_POINT('Ctrl Pts',(0.992091965201322,2.1040344873685,7.18180016009835));
#118678=CARTESIAN_POINT('Ctrl Pts',(2.065284143,2.232664075,7.210034772));
#118679=CARTESIAN_POINT('Ctrl Pts',(2.456474424,2.168401865,7.097979961));
#118680=CARTESIAN_POINT('Ctrl Pts',(2.833244645,2.103255924,6.944258404));
#118681=CARTESIAN_POINT('Ctrl Pts',(1.766793184,2.232664075,7.031425307));
#118682=CARTESIAN_POINT('Ctrl Pts',(2.148292764,2.168401865,6.93556553));
#118683=CARTESIAN_POINT('Ctrl Pts',(2.51718138,2.103255924,6.798992418));
#118684=CARTESIAN_POINT('',(2.51277214473806,2.10403448615021,6.80062321801409));
#118685=CARTESIAN_POINT('Origin',(-0.0808521565263137,2.01791771072404,
-0.177485649792515));
#118686=CARTESIAN_POINT('Ctrl Pts',(2.6014868140917,2.14301213126478,7.03436325144443));
#118687=CARTESIAN_POINT('Ctrl Pts',(2.58718731604052,2.13706112120453,6.99677932611909));
#118688=CARTESIAN_POINT('Ctrl Pts',(2.57234969575751,2.13073653613662,6.9577443421695));
#118689=CARTESIAN_POINT('Ctrl Pts',(2.54226833099551,2.11752978378426,6.8784904682225));
#118690=CARTESIAN_POINT('Ctrl Pts',(2.52750135875876,2.11086978246806,6.83953434665737));
#118691=CARTESIAN_POINT('Ctrl Pts',(2.51277214242083,2.10403448654085,6.80062321882262));
#118692=CARTESIAN_POINT('Ctrl Pts',(2.362649238,2.103262031,7.118138));
#118693=CARTESIAN_POINT('Ctrl Pts',(2.482304756,2.123129682,7.078421992));
#118694=CARTESIAN_POINT('Ctrl Pts',(2.600557799,2.142857143,7.034706755));
#118695=CARTESIAN_POINT('Ctrl Pts',(2.867795619,2.187438859,6.935915516));
#118696=CARTESIAN_POINT('Ctrl Pts',(3.126768193,2.232664075,6.817134344));
#118697=CARTESIAN_POINT('Ctrl Pts',(2.50832663,2.103262031,6.802264146));
#118698=CARTESIAN_POINT('Ctrl Pts',(2.622672326,2.123129682,6.76009931));
#118699=CARTESIAN_POINT('Ctrl Pts',(2.735536241,2.142857143,6.714115092));
#118700=CARTESIAN_POINT('Ctrl Pts',(2.99059527,2.187438859,6.610196228));
#118701=CARTESIAN_POINT('Ctrl Pts',(3.237035134,2.232664075,6.487226182));
#118702=CARTESIAN_POINT('Ctrl Pts',(3.23703512624068,2.23266407357605,6.48722618587179));
#118703=CARTESIAN_POINT('Ctrl Pts',(3.10393962719884,2.20823915874926,6.55363897853008));
#118704=CARTESIAN_POINT('Ctrl Pts',(2.969104115023,2.18398286498676,6.61579951009992));
#118705=CARTESIAN_POINT('Ctrl Pts',(2.83293776111239,2.1599609054766,6.67360199905533));
#118706=CARTESIAN_POINT('Ctrl Pts',(2.80054401808973,2.15424612233873,6.68735311245094));
#118707=CARTESIAN_POINT('Ctrl Pts',(2.76807499048703,2.14854458445958,6.70085780874828));
#118708=CARTESIAN_POINT('Ctrl Pts',(2.7355362399328,2.14285714285121,6.71411509285976));
#118709=CARTESIAN_POINT('Ctrl Pts',(2.6618936167638,2.12998516357859,6.74411935469137));
#118710=CARTESIAN_POINT('Ctrl Pts',(2.58762060356933,2.11704095629822,6.77296735215525));
#118711=CARTESIAN_POINT('Ctrl Pts',(2.51277214949572,2.10403448774872,6.80062321598498));
#118712=CARTESIAN_POINT('Ctrl Pts',(3.566943297,2.232664075,6.597493124));
#118713=CARTESIAN_POINT('Ctrl Pts',(3.924899294,2.168401865,6.403963745));
#118714=CARTESIAN_POINT('Ctrl Pts',(4.259815245,2.103255924,6.172841653));
#118715=CARTESIAN_POINT('Ctrl Pts',(3.237035134,2.232664075,6.487226182));
#118716=CARTESIAN_POINT('Ctrl Pts',(3.589008448,2.168401865,6.311596421));
#118717=CARTESIAN_POINT('Ctrl Pts',(3.919913471,2.103255924,6.098916164));
#118718=CARTESIAN_POINT('',(3.91595789500394,2.10403448615343,6.10145669215797));
#118719=CARTESIAN_POINT('Origin',(-0.117115990262643,2.01791771245111,-0.155955219364138));
#118720=CARTESIAN_POINT('Ctrl Pts',(4.05284566323258,2.14301213126278,6.31066098193969));
#118721=CARTESIAN_POINT('Ctrl Pts',(4.03080108980658,2.13706113288446,6.27702978339675));
#118722=CARTESIAN_POINT('Ctrl Pts',(4.00791888512396,2.1307365166235,6.24209689464461));
#118723=CARTESIAN_POINT('Ctrl Pts',(3.96150363406452,2.1175297837628,6.1711626411393));
#118724=CARTESIAN_POINT('Ctrl Pts',(3.9387074907344,2.11086978244736,6.13629175453385));
#118725=CARTESIAN_POINT('Ctrl Pts',(3.91595789307703,2.10403448653057,6.10145669334236));
#118726=CARTESIAN_POINT('Ctrl Pts',(3.837601071,2.103262031,6.443820142));
#118727=CARTESIAN_POINT('Ctrl Pts',(3.945921342,2.123129682,6.379310274));
#118728=CARTESIAN_POINT('Ctrl Pts',(4.052012211,2.142857143,6.311196166));
#118729=CARTESIAN_POINT('Ctrl Pts',(4.291764963,2.187438859,6.157266379));
#118730=CARTESIAN_POINT('Ctrl Pts',(4.519148461,2.232664075,5.985590797));
#118731=CARTESIAN_POINT('Ctrl Pts',(3.911969065,2.103262031,6.104014911));
#118732=CARTESIAN_POINT('Ctrl Pts',(4.014577229,2.123129682,6.03825492));
#118733=CARTESIAN_POINT('Ctrl Pts',(4.114917201,2.142857143,5.969083383));
#118734=CARTESIAN_POINT('Ctrl Pts',(4.341673608,2.187438859,5.812763932));
#118735=CARTESIAN_POINT('Ctrl Pts',(4.55591692,2.232664075,5.639691571));
#118736=CARTESIAN_POINT('Ctrl Pts',(4.55591691329171,2.23266407358393,5.63969157641916));
#118737=CARTESIAN_POINT('Ctrl Pts',(4.44020990789959,2.20823916035437,5.73316326695541));
#118738=CARTESIAN_POINT('Ctrl Pts',(4.32188945961225,2.18398286813883,5.82285616395298));
#118739=CARTESIAN_POINT('Ctrl Pts',(4.20133243362317,2.15996091009865,5.90857899901553));
#118740=CARTESIAN_POINT('Ctrl Pts',(4.17265211345323,2.15424612539781,5.92897232188741));
#118741=CARTESIAN_POINT('Ctrl Pts',(4.14384529634021,2.14854458596021,5.94914117258918));
#118742=CARTESIAN_POINT('Ctrl Pts',(4.11491719997479,2.14285714279844,5.96908338370675));
#118743=CARTESIAN_POINT('Ctrl Pts',(4.04944632956831,2.12998516349913,6.01421714887343));
#118744=CARTESIAN_POINT('Ctrl Pts',(3.98311124483373,2.11704095625173,6.05835719870953));
#118745=CARTESIAN_POINT('Ctrl Pts',(3.91595789925707,2.10403448771939,6.10145668921002));
#118746=CARTESIAN_POINT('Ctrl Pts',(4.901816146,2.232664075,5.67646003));
#118747=CARTESIAN_POINT('Ctrl Pts',(5.209800235,2.168401865,5.410505303));
#118748=CARTESIAN_POINT('Ctrl Pts',(5.48720162,2.103255924,5.112789687));
#118749=CARTESIAN_POINT('Ctrl Pts',(4.55591692,2.232664075,5.639691571));
#118750=CARTESIAN_POINT('Ctrl Pts',(4.861906086,2.168401865,5.392504079));
#118751=CARTESIAN_POINT('Ctrl Pts',(5.139354765,2.103255924,5.113661369));
#118752=CARTESIAN_POINT('',(5.13603780693689,2.10403448615971,5.11699283304007));
#118753=CARTESIAN_POINT('Origin',(-0.147903519018688,2.01791776476396,-0.127132470961947));
#118754=CARTESIAN_POINT('Ctrl Pts',(5.3146979529777,2.14301213129116,5.29187921908646));
#118755=CARTESIAN_POINT('Ctrl Pts',(5.28593899785615,2.13706112090324,5.26377317422809));
#118756=CARTESIAN_POINT('Ctrl Pts',(5.25608237635443,2.13073653635175,5.23457613979777));
#118757=CARTESIAN_POINT('Ctrl Pts',(5.19550343018011,2.11752978375768,5.17527810805184));
#118758=CARTESIAN_POINT('Ctrl Pts',(5.16574403856045,2.1108697824829,5.14612298051484));
#118759=CARTESIAN_POINT('Ctrl Pts',(5.13603780536316,2.10403448654035,5.11699283455561));
#118760=CARTESIAN_POINT('Ctrl Pts',(5.133110943,2.103262031,5.468196417));
#118761=CARTESIAN_POINT('Ctrl Pts',(5.22503103100001,2.123129682,5.381909097));
#118762=CARTESIAN_POINT('Ctrl Pts',(5.313999035,2.142857143,5.292581058));
#118763=CARTESIAN_POINT('Ctrl Pts',(5.51505614700001,2.187438859,5.09071031));
#118764=CARTESIAN_POINT('Ctrl Pts',(5.70021837,2.232664075,4.874167676));
#118765=CARTESIAN_POINT('Ctrl Pts',(5.132692175,2.103262031,5.120348722));
#118766=CARTESIAN_POINT('Ctrl Pts',(5.218764963,2.123129682,5.03406844200001));
#118767=CARTESIAN_POINT('Ctrl Pts',(5.301889206,2.142857143,4.944943968));
#118768=CARTESIAN_POINT('Ctrl Pts',(5.489740113,2.187438859,4.743533254));
#118769=CARTESIAN_POINT('Ctrl Pts',(5.661769094,2.232664075,4.52845125));
#118770=CARTESIAN_POINT('Ctrl Pts',(5.66176908835685,2.23266407351645,4.52845125705543));
#118771=CARTESIAN_POINT('Ctrl Pts',(5.56886090028387,2.20823916067901,4.64461121517142));
#118772=CARTESIAN_POINT('Ctrl Pts',(5.47258804156651,2.18398286888765,4.75764253910149));
#118773=CARTESIAN_POINT('Ctrl Pts',(5.3732774492891,2.15996091126762,4.86727741707001));
#118774=CARTESIAN_POINT('Ctrl Pts',(5.3496516190285,2.15424612616522,4.89335937830019));
#118775=CARTESIAN_POINT('Ctrl Pts',(5.32585399435101,2.14854458632816,4.91924930846668));
#118776=CARTESIAN_POINT('Ctrl Pts',(5.30188920503029,2.14285714276879,4.94494396917447));
#118777=CARTESIAN_POINT('Ctrl Pts',(5.24765143282067,2.12998516346269,5.0030968345205));
#118778=CARTESIAN_POINT('Ctrl Pts',(5.19235603125489,2.11704095613966,5.06046499702258));
#118779=CARTESIAN_POINT('Ctrl Pts',(5.13603781027864,2.10403448767572,5.11699282926966));
#118780=CARTESIAN_POINT('Ctrl Pts',(6.00748552,2.232664075,4.490001975));
#118781=CARTESIAN_POINT('Ctrl Pts',(6.251096707,2.168401865,4.164057646));
#118782=CARTESIAN_POINT('Ctrl Pts',(6.458012545,2.103255924,3.813669358));
#118783=CARTESIAN_POINT('Ctrl Pts',(5.661769094,2.232664075,4.52845125000001));
#118784=CARTESIAN_POINT('Ctrl Pts',(5.907466399,2.168401865,4.221264238));
#118785=CARTESIAN_POINT('Ctrl Pts',(6.11848554200001,2.103255924,3.889297452));
#118786=CARTESIAN_POINT('',(6.11596229886022,2.10403448614595,3.89326407593993));
#118787=CARTESIAN_POINT('Origin',(-0.171775416579336,2.01791771392519,-0.0923653430460797));
#118788=CARTESIAN_POINT('Ctrl Pts',(6.32804087377597,2.14301213122732,4.02565506515197));
#118789=CARTESIAN_POINT('Ctrl Pts',(6.2939123810826,2.13706113181295,4.00438848838436));
#118790=CARTESIAN_POINT('Ctrl Pts',(6.2584771297729,2.13073651823195,3.98229225490456));
#118791=CARTESIAN_POINT('Ctrl Pts',(6.18656726015707,2.11752978376512,3.93740332255265));
#118792=CARTESIAN_POINT('Ctrl Pts',(6.15123613580716,2.11086978246197,3.91532721515228));
#118793=CARTESIAN_POINT('Ctrl Pts',(6.11596229761108,2.10403448649821,3.89326407782788));
#118794=CARTESIAN_POINT('Ctrl Pts',(6.188602252,2.103262031,4.236885904));
#118795=CARTESIAN_POINT('Ctrl Pts',(6.259824077,2.123129682,4.132855832));
#118796=CARTESIAN_POINT('Ctrl Pts',(6.327509171,2.142857143,4.026490742));
#118797=CARTESIAN_POINT('Ctrl Pts',(6.480469435,2.187438859,3.786118284));
#118798=CARTESIAN_POINT('Ctrl Pts',(6.614752403,2.232664075,3.534833892));
#118799=CARTESIAN_POINT('Ctrl Pts',(6.113416303,2.103262031,3.897260718));
#118800=CARTESIAN_POINT('Ctrl Pts',(6.178929047,2.123129682,3.794494518));
#118801=CARTESIAN_POINT('Ctrl Pts',(6.240950764,2.142857143,3.68958447));
#118802=CARTESIAN_POINT('Ctrl Pts',(6.381112471,2.187438859,3.452500234));
#118803=CARTESIAN_POINT('Ctrl Pts',(6.502883238,2.232664075,3.205465582));
#118804=CARTESIAN_POINT('Ctrl Pts',(6.50288323411111,2.23266407355568,3.20546558988933));
#118805=CARTESIAN_POINT('Ctrl Pts',(6.43711819122571,2.20823917803144,3.33888221223235));
#118806=CARTESIAN_POINT('Ctrl Pts',(6.36739458367594,2.18398290322023,3.46996665495728));
#118807=CARTESIAN_POINT('Ctrl Pts',(6.29397413275033,2.159960962177,3.59838708563228));
#118808=CARTESIAN_POINT('Ctrl Pts',(6.2765074614521,2.15424616006317,3.62893821167822));
#118809=CARTESIAN_POINT('Ctrl Pts',(6.25883172995105,2.14854460328905,3.65933872608122));
#118810=CARTESIAN_POINT('Ctrl Pts',(6.24095076365543,2.14285714287543,3.68958447084559));
#118811=CARTESIAN_POINT('Ctrl Pts',(6.20048218741084,2.12998516355731,3.75803727196376));
#118812=CARTESIAN_POINT('Ctrl Pts',(6.15881202082062,2.1170409562234,3.8259510754514));
#118813=CARTESIAN_POINT('Ctrl Pts',(6.11596230129555,2.10403448764277,3.89326407151601));
#118814=CARTESIAN_POINT('Ctrl Pts',(6.832251548,2.232664075,3.093596417));
#118815=CARTESIAN_POINT('Ctrl Pts',(7.000098845,2.168401865,2.722903281));
#118816=CARTESIAN_POINT('Ctrl Pts',(7.126853981,2.103255924,2.336226088));
#118817=CARTESIAN_POINT('Ctrl Pts',(6.502883238,2.232664075,3.205465582));
#118818=CARTESIAN_POINT('Ctrl Pts',(6.676800149,2.168401865,2.852642774));
#118819=CARTESIAN_POINT('Ctrl Pts',(6.811522736,2.103255924,2.483074308));
#118820=CARTESIAN_POINT('',(6.80991119082281,2.10403448614523,2.48749061760122));
#118821=CARTESIAN_POINT('Origin',(-0.18761523090055,2.01791774112694,-0.0532792561436141));
#118822=CARTESIAN_POINT('Ctrl Pts',(7.04549163606581,2.14301213123522,2.57119575439931));
#118823=CARTESIAN_POINT('Ctrl Pts',(7.0075893623576,2.13706113168265,2.55776299520579));
#118824=CARTESIAN_POINT('Ctrl Pts',(6.96823253200764,2.13073651834497,2.54380089153319));
#118825=CARTESIAN_POINT('Ctrl Pts',(6.88835362328561,2.11752970809174,2.51541977092132));
#118826=CARTESIAN_POINT('Ctrl Pts',(6.84910305541128,2.11086974536017,2.50145502478111));
#118827=CARTESIAN_POINT('Ctrl Pts',(6.80991119013385,2.10403448647952,2.48749061958345));
#118828=CARTESIAN_POINT('Ctrl Pts',(6.954721399,2.103262031,2.807463316));
#118829=CARTESIAN_POINT('Ctrl Pts',(7.001914706,2.123129682,2.690554822));
#118830=CARTESIAN_POINT('Ctrl Pts',(7.04515201,2.142857143,2.572126194));
#118831=CARTESIAN_POINT('Ctrl Pts',(7.142863175,2.187438859,2.304491575));
#118832=CARTESIAN_POINT('Ctrl Pts',(7.219987966,2.232664075,2.030215204));
#118833=CARTESIAN_POINT('Ctrl Pts',(6.808283879,2.103262031,2.491941134));
#118834=CARTESIAN_POINT('Ctrl Pts',(6.850173276,2.123129682,2.377494247));
#118835=CARTESIAN_POINT('Ctrl Pts',(6.888192401,2.142857143,2.261704102));
#118836=CARTESIAN_POINT('Ctrl Pts',(6.974111103,2.187438859,2.00003214));
#118837=CARTESIAN_POINT('Ctrl Pts',(7.039929788,2.232664075,1.732595906));
#118838=CARTESIAN_POINT('Ctrl Pts',(7.03992978592764,2.23266407357604,1.73259591442046));
#118839=CARTESIAN_POINT('Ctrl Pts',(7.0043828991772,2.2082391610559,1.87703097072648));
#118840=CARTESIAN_POINT('Ctrl Pts',(6.96446864068666,2.18398286961989,2.02003934379038));
#118841=CARTESIAN_POINT('Ctrl Pts',(6.92037127959601,2.15996091242376,2.16124069710796));
#118842=CARTESIAN_POINT('Ctrl Pts',(6.90988058740402,2.15424612694543,2.19483227488293));
#118843=CARTESIAN_POINT('Ctrl Pts',(6.89915334705155,2.14854458673851,2.2283217045661));
#118844=CARTESIAN_POINT('Ctrl Pts',(6.88819240064526,2.14285714281593,2.26170410308038));
#118845=CARTESIAN_POINT('Ctrl Pts',(6.86338528583572,2.12998516352363,2.33725606329273));
#118846=CARTESIAN_POINT('Ctrl Pts',(6.83728880486597,2.11704095620497,2.41253993402923));
#118847=CARTESIAN_POINT('Ctrl Pts',(6.80991119222406,2.10403448758666,2.48749061268677));
#118848=CARTESIAN_POINT('Ctrl Pts',(7.337549087,2.232664075,1.552537729));
#118849=CARTESIAN_POINT('Ctrl Pts',(7.421784141,2.168401865,1.154428985));
#118850=CARTESIAN_POINT('Ctrl Pts',(7.462451646,2.103255924,0.749543483));
#118851=CARTESIAN_POINT('Ctrl Pts',(7.039929788,2.232664075,1.732595906));
#118852=CARTESIAN_POINT('Ctrl Pts',(7.133934145,2.168401865,1.350634904));
#118853=CARTESIAN_POINT('Ctrl Pts',(7.186060697,2.103255924,0.960745369));
#118854=CARTESIAN_POINT('',(7.18543620485501,2.10403448618026,0.965404863172399));
#118855=CARTESIAN_POINT('Origin',(-0.194682222779703,2.01791775279427,-0.0117018739600151));
#118856=CARTESIAN_POINT('Ctrl Pts',(7.43350303989041,2.14301213123168,0.9965101881476));
#118857=CARTESIAN_POINT('Ctrl Pts',(7.39359918050729,2.13706112069452,0.991539338668986));
#118858=CARTESIAN_POINT('Ctrl Pts',(7.35216123765767,2.13073653596577,0.986364239354941));
#118859=CARTESIAN_POINT('Ctrl Pts',(7.26804866643051,2.11752971237787,0.97581824705879));
#118860=CARTESIAN_POINT('Ctrl Pts',(7.22671373277042,2.11086974748737,0.970617699025719));
#118861=CARTESIAN_POINT('Ctrl Pts',(7.18543620457699,2.10403448656051,0.965404864875282));
#118862=CARTESIAN_POINT('Ctrl Pts',(7.395645502,2.103262031,1.246766863));
#118863=CARTESIAN_POINT('Ctrl Pts',(7.416603586,2.123129682,1.122446458));
#118864=CARTESIAN_POINT('Ctrl Pts',(7.433371371,2.142857143,0.997491884));
#118865=CARTESIAN_POINT('Ctrl Pts',(7.471264572,2.187438859,0.715109402));
#118866=CARTESIAN_POINT('Ctrl Pts',(7.487624915,2.232664075,0.43066591));
#118867=CARTESIAN_POINT('Ctrl Pts',(7.184803668,2.103262031,0.970101153));
#118868=CARTESIAN_POINT('Ctrl Pts',(7.201111017,2.123129682,0.849324988));
#118869=CARTESIAN_POINT('Ctrl Pts',(7.213349817,2.142857143,0.728068964));
#118870=CARTESIAN_POINT('Ctrl Pts',(7.241008051,2.187438859,0.454044767));
#118871=CARTESIAN_POINT('Ctrl Pts',(7.247797047,2.232664075,0.178711971));
#118872=CARTESIAN_POINT('Ctrl Pts',(7.24779704678624,2.23266407357604,0.178711979669084));
#118873=CARTESIAN_POINT('Ctrl Pts',(7.2441304941737,2.20823916217468,0.327411748160941));
#118874=CARTESIAN_POINT('Ctrl Pts',(7.23589198219421,2.18398287173784,0.475657044536055));
#118875=CARTESIAN_POINT('Ctrl Pts',(7.22317971082102,2.15996091544561,0.623036812005189));
#118876=CARTESIAN_POINT('Ctrl Pts',(7.22015548100198,2.15424612896897,0.658098232141686));
#118877=CARTESIAN_POINT('Ctrl Pts',(7.21687827448317,2.14854458776399,0.693110743211409));
#118878=CARTESIAN_POINT('Ctrl Pts',(7.21334981720885,2.14285714284448,0.728068965329833));
#118879=CARTESIAN_POINT('Ctrl Pts',(7.20536411757946,2.12998516353824,0.80718735947546));
#118880=CARTESIAN_POINT('Ctrl Pts',(7.19606156435664,2.11704095622061,0.886321106970012));
#118881=CARTESIAN_POINT('Ctrl Pts',(7.18543620520422,2.10403448763058,0.965404858045334));
#118882=CARTESIAN_POINT('Ctrl Pts',(7.499750986,2.232664075,-0.061115898));
#118883=CARTESIAN_POINT('Ctrl Pts',(7.496435059,2.168401865,-0.468025127));
#118884=CARTESIAN_POINT('Ctrl Pts',(7.449113366,2.103255924,-0.872186943));
#118885=CARTESIAN_POINT('Ctrl Pts',(7.247797047,2.232664075,0.178711971));
#118886=CARTESIAN_POINT('Ctrl Pts',(7.257493309,2.168401865,-0.214527153));
#118887=CARTESIAN_POINT('Ctrl Pts',(7.224586446,2.103255924,-0.606506955));
#118888=CARTESIAN_POINT('',(7.22497820779803,2.10403448615812,-0.60182215072398));
#118889=CARTESIAN_POINT('Origin',(-0.19264630124107,2.01791774916566,0.0304226431543164));
#118890=CARTESIAN_POINT('Ctrl Pts',(7.47393210366752,2.14301213123845,-0.624771087536083));
#118891=CARTESIAN_POINT('Ctrl Pts',(7.43389266566128,2.1370611321497,-0.621047578195944));
#118892=CARTESIAN_POINT('Ctrl Pts',(7.39231082795438,2.13073651714187,-0.617193735242821));
#118893=CARTESIAN_POINT('Ctrl Pts',(7.30789826191783,2.11752978375747,-0.609411504752216));
#118894=CARTESIAN_POINT('Ctrl Pts',(7.26641150752387,2.11086978240992,-0.605604655337827));
#118895=CARTESIAN_POINT('Ctrl Pts',(7.22497820791532,2.10403448648335,-0.601822148851471));
#118896=CARTESIAN_POINT('Ctrl Pts',(7.49075744100001,2.103262031,-0.372227023));
#118897=CARTESIAN_POINT('Ctrl Pts',(7.484500325,2.123129682,-0.498146254));
#118898=CARTESIAN_POINT('Ctrl Pts',(7.474014549,2.142857143,-0.623784038));
#118899=CARTESIAN_POINT('Ctrl Pts',(7.45031794100001,2.187438859,-0.907710493));
#118900=CARTESIAN_POINT('Ctrl Pts',(7.405148846,2.232664075,-1.189020844));
#118901=CARTESIAN_POINT('Ctrl Pts',(7.225370023,2.103262031,-0.597099681));
#118902=CARTESIAN_POINT('Ctrl Pts',(7.21533281000001,2.123129682,-0.718557763));
#118903=CARTESIAN_POINT('Ctrl Pts',(7.201219013,2.142857143,-0.839609869));
#118904=CARTESIAN_POINT('Ctrl Pts',(7.16932351,2.187438859,-1.113173236));
#118905=CARTESIAN_POINT('Ctrl Pts',(7.116765371,2.232664075,-1.383528337));
#118906=CARTESIAN_POINT('Ctrl Pts',(7.11676537265484,2.23266407357604,-1.38352832848763));
#118907=CARTESIAN_POINT('Ctrl Pts',(7.14515060543227,2.20823915451187,-1.23751683208644));
#118908=CARTESIAN_POINT('Ctrl Pts',(7.16897306784405,2.18398285663643,-1.09096634643821));
#118909=CARTESIAN_POINT('Ctrl Pts',(7.18824029892274,2.15996089312086,-0.944299428321259));
#118910=CARTESIAN_POINT('Ctrl Pts',(7.1928239362316,2.15424611408736,-0.909407649886073));
#118911=CARTESIAN_POINT('Ctrl Pts',(7.19714999795818,2.14854458029521,-0.874509254573029));
#118912=CARTESIAN_POINT('Ctrl Pts',(7.201219013176,2.14285714275399,-0.839609867490446));
#118913=CARTESIAN_POINT('Ctrl Pts',(7.21042813048085,2.12998516345522,-0.760624528096376));
#118914=CARTESIAN_POINT('Ctrl Pts',(7.21835448240667,2.11704095613337,-0.681341109868308));
#118915=CARTESIAN_POINT('Ctrl Pts',(7.2249782070012,2.10403448753746,-0.601822155615398));
#118916=CARTESIAN_POINT('Ctrl Pts',(7.311272864,2.232664075,-1.671911813));
#118917=CARTESIAN_POINT('Ctrl Pts',(7.22056100600001,2.168401865,-2.068594904));
#118918=CARTESIAN_POINT('Ctrl Pts',(7.087462824,2.103255924,-2.453134876));
#118919=CARTESIAN_POINT('Ctrl Pts',(7.11676537100001,2.232664075,-1.383528337));
#118920=CARTESIAN_POINT('Ctrl Pts',(7.041700152,2.168401865,-1.769658159));
#118921=CARTESIAN_POINT('Ctrl Pts',(6.925298563,2.103255924,-2.145399688));
#118922=CARTESIAN_POINT('',(6.9266882593708,2.10403448615338,-2.14090862880051));
#118923=CARTESIAN_POINT('Origin',(-0.181602426183516,2.01791772037682,0.0711246562100257));
#118924=CARTESIAN_POINT('Ctrl Pts',(7.16488840885302,2.1430121312558,-2.21683876058331));
#118925=CARTESIAN_POINT('Ctrl Pts',(7.12658551329033,2.13706113188681,-2.20459500866285));
#118926=CARTESIAN_POINT('Ctrl Pts',(7.0868043014371,2.13073651737911,-2.19189240173367));
#118927=CARTESIAN_POINT('Ctrl Pts',(7.00603766334665,2.11752969561696,-2.16614573670162));
#118928=CARTESIAN_POINT('Ctrl Pts',(6.96633949502101,2.11086973926319,-2.15350955562722));
#118929=CARTESIAN_POINT('Ctrl Pts',(6.92668826047007,2.10403448652366,-2.14090862668333));
#118930=CARTESIAN_POINT('Ctrl Pts',(7.235609888,2.103262031,-1.973815986));
#118931=CARTESIAN_POINT('Ctrl Pts',(7.202430147,2.123129682,-2.095446201));
#118932=CARTESIAN_POINT('Ctrl Pts',(7.165181113,2.142857143,-2.215892511));
#118933=CARTESIAN_POINT('Ctrl Pts',(7.081002724,2.187438859,-2.488086853));
#118934=CARTESIAN_POINT('Ctrl Pts',(6.976416247,2.232664075,-2.753110305));
#118935=CARTESIAN_POINT('Ctrl Pts',(6.928086106,2.103262031,-2.136380796));
#118936=CARTESIAN_POINT('Ctrl Pts',(6.892173659,2.123129682,-2.252841553));
#118937=CARTESIAN_POINT('Ctrl Pts',(6.852367211,2.142857143,-2.368029478));
#118938=CARTESIAN_POINT('Ctrl Pts',(6.76240936900001,2.187438859,-2.628340495));
#118939=CARTESIAN_POINT('Ctrl Pts',(6.652961655,2.232664075,-2.881076398));
#118940=CARTESIAN_POINT('Ctrl Pts',(6.65296165844605,2.23266407357604,-2.88107639004239));
#118941=CARTESIAN_POINT('Ctrl Pts',(6.71207139004059,2.20823916520409,-2.74458060686293));
#118942=CARTESIAN_POINT('Ctrl Pts',(6.7668408976219,2.18398287772463,-2.60657757543584));
#118943=CARTESIAN_POINT('Ctrl Pts',(6.81718670611509,2.15996092424679,-2.46748159380732));
#118944=CARTESIAN_POINT('Ctrl Pts',(6.82916390418536,2.15424613480453,-2.43439085253997));
#118945=CARTESIAN_POINT('Ctrl Pts',(6.84089097018248,2.14854459064272,-2.40123827769394));
#118946=CARTESIAN_POINT('Ctrl Pts',(6.85236721156548,2.14285714277589,-2.36802947663634));
#118947=CARTESIAN_POINT('Ctrl Pts',(6.87834053749264,2.12998516342169,-2.29287045888821));
#118948=CARTESIAN_POINT('Ctrl Pts',(6.90312516711685,2.11704095609726,-2.21714457406265));
#118949=CARTESIAN_POINT('Ctrl Pts',(6.92668825783225,2.10403448760368,-2.14090863337329));
#118950=CARTESIAN_POINT('Ctrl Pts',(6.780927749,2.232664075,-3.20453099));
#118951=CARTESIAN_POINT('Ctrl Pts',(6.60706154500001,2.168401865,-3.572439483));
#118952=CARTESIAN_POINT('Ctrl Pts',(6.39441039699999,2.103255924,-3.919376949));
#118953=CARTESIAN_POINT('Ctrl Pts',(6.65296165500001,2.232664075,-2.881076398));
#118954=CARTESIAN_POINT('Ctrl Pts',(6.496644922,2.168401865,-3.242041916));
#118955=CARTESIAN_POINT('Ctrl Pts',(6.302191415,2.103255924,-3.583975916));
#118956=CARTESIAN_POINT('',(6.30451406692602,2.10403448613635,-3.57988859897104));
#118957=CARTESIAN_POINT('Origin',(-0.162066820169903,2.01791775098821,0.108500875694056));
#118958=CARTESIAN_POINT('Ctrl Pts',(6.52082249472584,2.1430121312108,-3.70524951776582));
#118959=CARTESIAN_POINT('Ctrl Pts',(6.48604707792739,2.13706112048613,-3.68505798914409));
#118960=CARTESIAN_POINT('Ctrl Pts',(6.44992678160988,2.13073653562651,-3.6641006748843));
#118961=CARTESIAN_POINT('Ctrl Pts',(6.37658358245868,2.11752978372462,-3.62159373779538));
#118962=CARTESIAN_POINT('Ctrl Pts',(6.34052967847826,2.11086978237466,-3.60071889880975));
#118963=CARTESIAN_POINT('Ctrl Pts',(6.3045140674439,2.1040344864438,-3.57988859797476));
#118964=CARTESIAN_POINT('Ctrl Pts',(6.642133258,2.103262031,-3.483111508));
#118965=CARTESIAN_POINT('Ctrl Pts',(6.58358234,2.123129682,-3.594765413));
#118966=CARTESIAN_POINT('Ctrl Pts',(6.521311771,2.142857143,-3.704388314));
#118967=CARTESIAN_POINT('Ctrl Pts',(6.380587689,2.187438859,-3.952123038));
#118968=CARTESIAN_POINT('Ctrl Pts',(6.221474178,2.232664075,-4.188467387));
#118969=CARTESIAN_POINT('Ctrl Pts',(6.306852583,2.103262031,-3.575767121));
#118970=CARTESIAN_POINT('Ctrl Pts',(6.246744129,2.123129682,-3.681784975));
#118971=CARTESIAN_POINT('Ctrl Pts',(6.183106334,2.142857143,-3.785722661));
#118972=CARTESIAN_POINT('Ctrl Pts',(6.039292483,2.187438859,-4.020609474));
#118973=CARTESIAN_POINT('Ctrl Pts',(5.878072847,2.232664075,-4.243908529));
#118974=CARTESIAN_POINT('Ctrl Pts',(5.87807285211789,2.23266407356433,-4.24390852191141));
#118975=CARTESIAN_POINT('Ctrl Pts',(5.96514322424147,2.20823915554531,-4.12331073155852));
#118976=CARTESIAN_POINT('Ctrl Pts',(6.04829885431209,2.18398285863974,-4.00030791039458));
#118977=CARTESIAN_POINT('Ctrl Pts',(6.12736915752677,2.15996089602006,-3.87528672607273));
#118978=CARTESIAN_POINT('Ctrl Pts',(6.14617983486012,2.15424611601566,-3.84554442001723));
#118979=CARTESIAN_POINT('Ctrl Pts',(6.16475952120855,2.14854458125394,-3.81568795542351));
#118980=CARTESIAN_POINT('Ctrl Pts',(6.18310633482256,2.14285714274501,-3.78572265965654));
#118981=CARTESIAN_POINT('Ctrl Pts',(6.22462938632703,2.1299851634521,-3.71790431536696));
#118982=CARTESIAN_POINT('Ctrl Pts',(6.26511339219194,2.11704095609181,-3.64927682231));
#118983=CARTESIAN_POINT('Ctrl Pts',(6.30451406510162,2.1040344874241,-3.57988860303163));
#118984=CARTESIAN_POINT('Ctrl Pts',(5.933513989,2.232664075,-4.587309859));
#118985=CARTESIAN_POINT('Ctrl Pts',(5.684623229,2.168401865,-4.909240762));
#118986=CARTESIAN_POINT('Ctrl Pts',(5.402362448,2.103255924,-5.202353312));
#118987=CARTESIAN_POINT('Ctrl Pts',(5.878072847,2.232664075,-4.243908529));
#118988=CARTESIAN_POINT('Ctrl Pts',(5.647813796,2.168401865,-4.562831397));
#118989=CARTESIAN_POINT('Ctrl Pts',(5.384400802,2.103255924,-4.854969413));
#118990=CARTESIAN_POINT('',(5.38754780319582,2.10403448614009,-4.85147695721227));
#118991=CARTESIAN_POINT('Origin',(-0.134953223403402,2.01791771288928,0.140803705752561));
#118992=CARTESIAN_POINT('Ctrl Pts',(5.57185016888731,2.14301213123745,-5.02040692549819));
#118993=CARTESIAN_POINT('Ctrl Pts',(5.54222842210557,2.13706113221689,-4.99321183034187));
#118994=CARTESIAN_POINT('Ctrl Pts',(5.51145765309236,2.13073651663086,-4.96497955430377));
#118995=CARTESIAN_POINT('Ctrl Pts',(5.44896662714916,2.11752970447619,-4.90769952435097));
#118996=CARTESIAN_POINT('Ctrl Pts',(5.41824331752903,2.11086974357807,-4.8795623880085));
#118997=CARTESIAN_POINT('Ctrl Pts',(5.38754780472493,2.10403448646141,-4.85147695546285));
#118998=CARTESIAN_POINT('Ctrl Pts',(5.73807786,2.103262031,-4.829540607));
#118999=CARTESIAN_POINT('Ctrl Pts',(5.656893541,2.123129682,-4.92599738900001));
#119000=CARTESIAN_POINT('Ctrl Pts',(5.57251314,2.142857143,-5.019671036));
#119001=CARTESIAN_POINT('Ctrl Pts',(5.38182346500001,2.187438859,-5.231362342));
#119002=CARTESIAN_POINT('Ctrl Pts',(5.17562289100001,2.232664075,-5.42797639));
#119003=CARTESIAN_POINT('Ctrl Pts',(5.39071764200001,2.103262031,-4.847954548));
#119004=CARTESIAN_POINT('Ctrl Pts',(5.309223786,2.123129682,-4.93857222300001));
#119005=CARTESIAN_POINT('Ctrl Pts',(5.224730277,2.142857143,-5.026399659));
#119006=CARTESIAN_POINT('Ctrl Pts',(5.033784992,2.187438859,-5.224879222));
#119007=CARTESIAN_POINT('Ctrl Pts',(4.828331886,2.232664075,-5.40830021300001));
#119008=CARTESIAN_POINT('Ctrl Pts',(4.82833189246886,2.23266407357604,-5.40830020722484));
#119009=CARTESIAN_POINT('Ctrl Pts',(4.93929153811201,2.20823916200544,-5.30923950860549));
#119010=CARTESIAN_POINT('Ctrl Pts',(5.04694497896374,2.18398287142066,-5.20698845514794));
#119011=CARTESIAN_POINT('Ctrl Pts',(5.15104249613844,2.15996091496511,-5.10188800353165));
#119012=CARTESIAN_POINT('Ctrl Pts',(5.17580713464865,2.1542461286371,-5.07688476846726));
#119013=CARTESIAN_POINT('Ctrl Pts',(5.20037072289607,2.14854458757901,-5.05172038722873));
#119014=CARTESIAN_POINT('Ctrl Pts',(5.22473027788515,2.14285714280411,-5.026399658127));
#119015=CARTESIAN_POINT('Ctrl Pts',(5.2798614829953,2.12998516349225,-4.96909309752418));
#119016=CARTESIAN_POINT('Ctrl Pts',(5.33415187731937,2.11704095622504,-4.91077294193982));
#119017=CARTESIAN_POINT('Ctrl Pts',(5.3875477996425,2.10403448764827,-4.85147696088472));
#119018=CARTESIAN_POINT('Ctrl Pts',(4.808655709,2.232664075,-5.755591218));
#119019=CARTESIAN_POINT('Ctrl Pts',(4.49637825,2.168401865,-6.016491399));
#119020=CARTESIAN_POINT('Ctrl Pts',(4.157706034,2.103255924,-6.242073416));
#119021=CARTESIAN_POINT('Ctrl Pts',(4.828331886,2.232664075,-5.408300213));
#119022=CARTESIAN_POINT('Ctrl Pts',(4.534897174,2.168401865,-5.670267952));
#119023=CARTESIAN_POINT('Ctrl Pts',(4.214841591,2.103255924,-5.89894993700001));
#119024=CARTESIAN_POINT('',(4.21866579235029,2.10403448613268,-5.89621564507842));
#119025=CARTESIAN_POINT('Origin',(-0.10152958199823,2.0179177372351,0.16652289096133));
#119026=CARTESIAN_POINT('Ctrl Pts',(4.36234432157512,2.14301213124375,-6.10081568470611));
#119027=CARTESIAN_POINT('Ctrl Pts',(4.33926125518818,2.13706113194744,-6.06788859432327));
#119028=CARTESIAN_POINT('Ctrl Pts',(4.31527899933983,2.13073651770443,-6.03370157478219));
#119029=CARTESIAN_POINT('Ctrl Pts',(4.26656278041319,2.11752978376772,-5.96432740782818));
#119030=CARTESIAN_POINT('Ctrl Pts',(4.24260626070986,2.11086978241002,-5.93024327565625));
#119031=CARTESIAN_POINT('Ctrl Pts',(4.21866579364788,2.10403448646565,-5.8962156440986));
#119032=CARTESIAN_POINT('Ctrl Pts',(4.56571631700001,2.103262031,-5.950145755));
#119033=CARTESIAN_POINT('Ctrl Pts',(4.465694686,2.123129682,-6.026895202));
#119034=CARTESIAN_POINT('Ctrl Pts',(4.363149987,2.142857143,-6.100239519));
#119035=CARTESIAN_POINT('Ctrl Pts',(4.131411158,2.187438859,-6.265988957));
#119036=CARTESIAN_POINT('Ctrl Pts',(3.88776523,2.232664075,-6.41367925));
#119037=CARTESIAN_POINT('Ctrl Pts',(4.222518736,2.103262031,-5.89345701));
#119038=CARTESIAN_POINT('Ctrl Pts',(4.123450039,2.123129682,-5.964437323));
#119039=CARTESIAN_POINT('Ctrl Pts',(4.022051639,2.142857143,-6.032047796));
#119040=CARTESIAN_POINT('Ctrl Pts',(3.79290331,2.187438859,-6.184839426));
#119041=CARTESIAN_POINT('Ctrl Pts',(3.552823492,2.232664075,-6.319805791));
#119042=CARTESIAN_POINT('Ctrl Pts',(3.55282349975592,2.23266407353897,-6.31980578663983));
#119043=CARTESIAN_POINT('Ctrl Pts',(3.68248410597432,2.20823915946357,-6.24691410877597));
#119044=CARTESIAN_POINT('Ctrl Pts',(3.80960163581233,2.18398286641657,-6.17019592741199));
#119045=CARTESIAN_POINT('Ctrl Pts',(3.93385891325753,2.15996090757301,-6.08993054588538));
#119046=CARTESIAN_POINT('Ctrl Pts',(3.96341951185059,2.15424612371975,-6.07083554579355));
#119047=CARTESIAN_POINT('Ctrl Pts',(3.99281840242606,2.14854458512651,-6.05153994733617));
#119048=CARTESIAN_POINT('Ctrl Pts',(4.02205164024343,2.14285714280556,-6.03204779538241));
#119049=CARTESIAN_POINT('Ctrl Pts',(4.08821312487487,2.12998516350552,-5.98793260951333));
#119050=CARTESIAN_POINT('Ctrl Pts',(4.15377134973306,2.11704095621315,-5.94264677680663));
#119051=CARTESIAN_POINT('Ctrl Pts',(4.21866578869385,2.10403448753419,-5.89621564797567));
#119052=CARTESIAN_POINT('Ctrl Pts',(3.458950033,2.232664075,-6.65474752900001));
#119053=CARTESIAN_POINT('Ctrl Pts',(3.09788762,2.168401865,-6.842417585));
#119054=CARTESIAN_POINT('Ctrl Pts',(2.718639907,2.103255924,-6.989921105));
#119055=CARTESIAN_POINT('Ctrl Pts',(3.552823492,2.232664075,-6.319805791));
#119056=CARTESIAN_POINT('Ctrl Pts',(3.2099338,2.168401865,-6.51256908));
#119057=CARTESIAN_POINT('Ctrl Pts',(2.848201072,2.103255924,-6.667102118));
#119058=CARTESIAN_POINT('',(2.85252365806424,2.10403448616781,-6.66525384222965));
#119059=CARTESIAN_POINT('Origin',(-0.0633584653971375,2.01791772718142,
0.184455723869529));
#119060=CARTESIAN_POINT('Ctrl Pts',(2.94886010157405,2.14301213123103,-6.89595708377018));
#119061=CARTESIAN_POINT('Ctrl Pts',(2.93339505702871,2.13706113248801,-6.85883763699611));
#119062=CARTESIAN_POINT('Ctrl Pts',(2.91732268763611,2.13073651658488,-6.82029440453739));
#119063=CARTESIAN_POINT('Ctrl Pts',(2.88465882512707,2.11752978380204,-6.74206962658952));
#119064=CARTESIAN_POINT('Ctrl Pts',(2.86858947662357,2.11086978246595,-6.70363241887223));
#119065=CARTESIAN_POINT('Ctrl Pts',(2.85252365959982,2.10403448655234,-6.66525384151835));
#119066=CARTESIAN_POINT('Ctrl Pts',(3.179866955,2.103262031,-6.792528701));
#119067=CARTESIAN_POINT('Ctrl Pts',(3.065684911,2.123129682,-6.845982094));
#119068=CARTESIAN_POINT('Ctrl Pts',(2.94977079,2.142857143,-6.895567583));
#119069=CARTESIAN_POINT('Ctrl Pts',(2.687818656,2.187438859,-7.007624892));
#119070=CARTESIAN_POINT('Ctrl Pts',(2.418119987,2.232664075,-7.099485596));
#119071=CARTESIAN_POINT('Ctrl Pts',(2.856879547,2.103262031,-6.663387971));
#119072=CARTESIAN_POINT('Ctrl Pts',(2.744868352,2.123129682,-6.711411963));
#119073=CARTESIAN_POINT('Ctrl Pts',(2.631306337,2.142857143,-6.755644082));
#119074=CARTESIAN_POINT('Ctrl Pts',(2.374669684,2.187438859,-6.855603411));
#119075=CARTESIAN_POINT('Ctrl Pts',(2.11118902,2.232664075,-6.93580427400001));
#119076=CARTESIAN_POINT('Ctrl Pts',(2.11118902852914,2.23266407353601,-6.93580427140382));
#119077=CARTESIAN_POINT('Ctrl Pts',(2.25348776161027,2.20823916567505,-6.89248996866132));
#119078=CARTESIAN_POINT('Ctrl Pts',(2.3941254605974,2.18398287874681,-6.84489194029667));
#119079=CARTESIAN_POINT('Ctrl Pts',(2.53273232253612,2.15996092583572,-6.79321477552511));
#119080=CARTESIAN_POINT('Ctrl Pts',(2.56570670678256,2.15424613585664,-6.78092084819633));
#119081=CARTESIAN_POINT('Ctrl Pts',(2.59856628612993,2.148544591162,-6.76839624943633));
#119082=CARTESIAN_POINT('Ctrl Pts',(2.63130633851113,2.1428571427663,-6.75564408154887));
#119083=CARTESIAN_POINT('Ctrl Pts',(2.70540446514762,2.12998516346204,-6.7267830475775));
#119084=CARTESIAN_POINT('Ctrl Pts',(2.77916509043874,2.11704095622701,-6.69664905294933));
#119085=CARTESIAN_POINT('Ctrl Pts',(2.85252365304596,2.10403448768073,-6.66525384416611));
#119086=CARTESIAN_POINT('Ctrl Pts',(1.947507698,2.232664075,-7.242735241));
#119087=CARTESIAN_POINT('Ctrl Pts',(1.554543209,2.168401865,-7.34839993));
#119088=CARTESIAN_POINT('Ctrl Pts',(1.1524532,2.103255924,-7.410927852));
#119089=CARTESIAN_POINT('Ctrl Pts',(2.11118902,2.232664075,-6.935804274));
#119090=CARTESIAN_POINT('Ctrl Pts',(1.73487749,2.168401865,-7.050349716));
#119091=CARTESIAN_POINT('Ctrl Pts',(1.348381837,2.103255924,-7.123508014));
#119092=CARTESIAN_POINT('',(1.35300068745991,2.10403448615076,-7.12263217777289));
#119093=CARTESIAN_POINT('Origin',(-0.0222246460937434,2.01791773180016,
0.193763435003071));
#119094=CARTESIAN_POINT('Ctrl Pts',(1.39749046141378,2.14301213120456,-7.36865119365262));
#119095=CARTESIAN_POINT('Ctrl Pts',(1.3903665633665,2.13706113123047,-7.32907504328819));
#119096=CARTESIAN_POINT('Ctrl Pts',(1.38295561590674,2.13073651802702,-7.28797786324355));
#119097=CARTESIAN_POINT('Ctrl Pts',(1.36787133931593,2.11752970466789,-7.20455966330647));
#119098=CARTESIAN_POINT('Ctrl Pts',(1.36044059487456,2.11086974367532,-7.16356692879696));
#119099=CARTESIAN_POINT('Ctrl Pts',(1.35300068947363,2.10403448647302,-7.12263217749919));
#119100=CARTESIAN_POINT('Ctrl Pts',(1.645330548,2.103262031,-7.317300553));
#119101=CARTESIAN_POINT('Ctrl Pts',(1.522327117,2.123129682,-7.344958472));
#119102=CARTESIAN_POINT('Ctrl Pts',(1.398463589,2.142857143,-7.36846657));
#119103=CARTESIAN_POINT('Ctrl Pts',(1.118546742,2.187438859,-7.421592076));
#119104=CARTESIAN_POINT('Ctrl Pts',(0.835406142,2.232664075,-7.45332788600001));
#119105=CARTESIAN_POINT('Ctrl Pts',(1.357655845,2.103262031,-7.121746317));
#119106=CARTESIAN_POINT('Ctrl Pts',(1.237939671,2.123129682,-7.14456843900001));
#119107=CARTESIAN_POINT('Ctrl Pts',(1.117524075,2.142857143,-7.163353959));
#119108=CARTESIAN_POINT('Ctrl Pts',(0.845399144,2.187438859,-7.205807));
#119109=CARTESIAN_POINT('Ctrl Pts',(0.570837696,2.232664075,-7.227492257));
#119110=CARTESIAN_POINT('Ctrl Pts',(0.570837704799485,2.23266407355057,
-7.22749225630501));
#119111=CARTESIAN_POINT('Ctrl Pts',(0.719120844582198,2.20823916949319,
-7.21578064104272));
#119112=CARTESIAN_POINT('Ctrl Pts',(0.866702658605281,2.18398288628028,
-7.19952837926755));
#119113=CARTESIAN_POINT('Ctrl Pts',(1.01317800933121,2.15996093704372,-7.17885578073409));
#119114=CARTESIAN_POINT('Ctrl Pts',(1.04802432438135,2.15424614334589,-7.17393779366096));
#119115=CARTESIAN_POINT('Ctrl Pts',(1.08280810605537,2.14854459495148,-7.16876984815762));
#119116=CARTESIAN_POINT('Ctrl Pts',(1.11752407577372,2.14285714287763,-7.16335395890305));
#119117=CARTESIAN_POINT('Ctrl Pts',(1.19609409852967,2.12998516356796,-7.15109658704414));
#119118=CARTESIAN_POINT('Ctrl Pts',(1.2746081595671,2.11704095627861,-7.13752346249769));
#119119=CARTESIAN_POINT('Ctrl Pts',(1.35300068233045,2.10403448759796,-7.12263217854009));
#119120=CARTESIAN_POINT('Ctrl Pts',(0.345002067,2.232664075,-7.492060703));
#119121=CARTESIAN_POINT('Ctrl Pts',(-0.061489915,2.168401865,-7.510779261));
#119122=CARTESIAN_POINT('Ctrl Pts',(-0.467620938,2.103255924,-7.485407848));
#119123=CARTESIAN_POINT('Ctrl Pts',(0.570837696,2.232664075,-7.227492257));
#119124=CARTESIAN_POINT('Ctrl Pts',(0.178700236,2.168401865,-7.258463836));
#119125=CARTESIAN_POINT('Ctrl Pts',(-0.214486235,2.103255924,-7.246826592));
#119126=CARTESIAN_POINT('',(-0.209787091421739,2.10403448613548,-7.24696414904864));
#119127=CARTESIAN_POINT('Origin',(0.0199483692145396,2.01791774013504,0.19401068436918));
#119128=CARTESIAN_POINT('Ctrl Pts',(-0.219224279818263,2.14301213120524,
-7.49679536283724));
#119129=CARTESIAN_POINT('Ctrl Pts',(-0.217673919736163,2.13706111995674,
-7.45661297729562));
#119130=CARTESIAN_POINT('Ctrl Pts',(-0.216076931763984,2.13073653540574,
-7.41488367955731));
#119131=CARTESIAN_POINT('Ctrl Pts',(-0.212876114293857,2.11752978377184,
-7.3301734731909));
#119132=CARTESIAN_POINT('Ctrl Pts',(-0.211320895472153,2.11086978240037,
-7.28854146381932));
#119133=CARTESIAN_POINT('Ctrl Pts',(-0.209787090011732,2.10403448647094,
-7.2469641490455));
#119134=CARTESIAN_POINT('Ctrl Pts',(0.033860313,2.103262031,-7.499923565));
#119135=CARTESIAN_POINT('Ctrl Pts',(-0.092213001,2.123129682,-7.500492755));
#119136=CARTESIAN_POINT('Ctrl Pts',(-0.218234215,2.142857143,-7.496824249));
#119137=CARTESIAN_POINT('Ctrl Pts',(-0.503027175,2.187438859,-7.488533863));
#119138=CARTESIAN_POINT('Ctrl Pts',(-0.786370366,2.232664075,-7.458660848));
#119139=CARTESIAN_POINT('Ctrl Pts',(-0.205050335,2.103262031,-7.247099721));
#119140=CARTESIAN_POINT('Ctrl Pts',(-0.326873693,2.123129682,-7.243652835));
#119141=CARTESIAN_POINT('Ctrl Pts',(-0.448512371,2.142857143,-7.236113367));
#119142=CARTESIAN_POINT('Ctrl Pts',(-0.723401321,2.187438859,-7.21907506300001));
#119143=CARTESIAN_POINT('Ctrl Pts',(-0.996205364,2.232664075,-7.181230735));
#119144=CARTESIAN_POINT('Ctrl Pts',(-0.996205355809929,2.23266407364226,
-7.18123073613615));
#119145=CARTESIAN_POINT('Ctrl Pts',(-0.848871309784289,2.20823916417171,
-7.20166942852254));
#119146=CARTESIAN_POINT('Ctrl Pts',(-0.701246087786972,2.18398287560745,
-7.21752286603136));
#119147=CARTESIAN_POINT('Ctrl Pts',(-0.553751218670259,2.15996092105231,
-7.22882145264826));
#119148=CARTESIAN_POINT('Ctrl Pts',(-0.518662401800881,2.15424613267169,
-7.23150937012673));
#119149=CARTESIAN_POINT('Ctrl Pts',(-0.483580922611584,2.14854458956584,
-7.23393973070297));
#119150=CARTESIAN_POINT('Ctrl Pts',(-0.448512369351866,2.14285714274861,
-7.23611336720714));
#119151=CARTESIAN_POINT('Ctrl Pts',(-0.369144296888193,2.12998516335947,
-7.2410327977486));
#119152=CARTESIAN_POINT('Ctrl Pts',(-0.289548030983509,2.11704095615912,
-7.24465520746409));
#119153=CARTESIAN_POINT('Ctrl Pts',(-0.209787096109261,2.10403448751812,
-7.24696414920313));
#119154=CARTESIAN_POINT('Ctrl Pts',(-1.273635477,2.232664075,-7.391065733));
#119155=CARTESIAN_POINT('Ctrl Pts',(-1.674647839,2.168401865,-7.321962901));
#119156=CARTESIAN_POINT('Ctrl Pts',(-2.065829641,2.103255924,-7.209878494));
#119157=CARTESIAN_POINT('Ctrl Pts',(-0.996205363999999,2.232664075,-7.181230735));
#119158=CARTESIAN_POINT('Ctrl Pts',(-1.385832842,2.168401865,-7.127180253));
#119159=CARTESIAN_POINT('Ctrl Pts',(-1.767325168,2.103255924,-7.031291613));
#119160=CARTESIAN_POINT('',(-1.76276545949674,2.10403448615187,-7.03243613115166));
#119161=CARTESIAN_POINT('Origin',(0.0611885772422269,2.01791773077624,0.185186671872305));
#119162=CARTESIAN_POINT('Ctrl Pts',(-1.82568833719172,2.14301213121992,
-7.27439771327462));
#119163=CARTESIAN_POINT('Ctrl Pts',(-1.81553619967466,2.13706112066952,
-7.23548805575916));
#119164=CARTESIAN_POINT('Ctrl Pts',(-1.80500598344183,2.13073653646983,
-7.19507767308385));
#119165=CARTESIAN_POINT('Ctrl Pts',(-1.78366980731394,2.11752978372427,
-7.11303601874195));
#119166=CARTESIAN_POINT('Ctrl Pts',(-1.77320129741869,2.11086978243029,
-7.07271166924485));
#119167=CARTESIAN_POINT('Ctrl Pts',(-1.76276545739217,2.10403448650513,
-7.03243613163703));
#119168=CARTESIAN_POINT('Ctrl Pts',(-1.579193193,2.103262031,-7.331858486));
#119169=CARTESIAN_POINT('Ctrl Pts',(-1.702441341,2.123129682,-7.305312333));
#119170=CARTESIAN_POINT('Ctrl Pts',(-1.824727629,2.142857143,-7.274638759));
#119171=CARTESIAN_POINT('Ctrl Pts',(-2.1010801,2.187438859,-7.20532013));
#119172=CARTESIAN_POINT('Ctrl Pts',(-2.37137707,2.232664075,-7.115235119));
#119173=CARTESIAN_POINT('Ctrl Pts',(-1.758168589,2.103262031,-7.03358679600001));
#119174=CARTESIAN_POINT('Ctrl Pts',(-1.876402807,2.123129682,-7.004032076));
#119175=CARTESIAN_POINT('Ctrl Pts',(-1.993576877,2.142857143,-6.970520155));
#119176=CARTESIAN_POINT('Ctrl Pts',(-2.258376345,2.187438859,-6.894787199));
#119177=CARTESIAN_POINT('Ctrl Pts',(-2.516666969,2.232664075,-6.799182846));
#119178=CARTESIAN_POINT('Ctrl Pts',(-2.51666696086751,2.23266407357605,
-6.79918284901019));
#119179=CARTESIAN_POINT('Ctrl Pts',(-2.37717117474474,2.20823915657027,
-6.85081617631785));
#119180=CARTESIAN_POINT('Ctrl Pts',(-2.23640532564656,2.18398286067009,
-6.89803404054907));
#119181=CARTESIAN_POINT('Ctrl Pts',(-2.09478762344738,2.15996089904969,
-6.94077551930649));
#119182=CARTESIAN_POINT('Ctrl Pts',(-2.06109702949982,2.15424611804273,
-6.95094363941559));
#119183=CARTESIAN_POINT('Ctrl Pts',(-2.02735823470697,2.14854458228384,
-6.96085864743894));
#119184=CARTESIAN_POINT('Ctrl Pts',(-1.99357687567617,2.14285714278373,
-6.97052015543815));
#119185=CARTESIAN_POINT('Ctrl Pts',(-1.91712191750664,2.12998516346973,
-6.99238636286277));
#119186=CARTESIAN_POINT('Ctrl Pts',(-1.8401652780448,2.11704095609638,-7.01303492728226));
#119187=CARTESIAN_POINT('Ctrl Pts',(-1.76276546417599,2.10403448765243,
-7.0324361299985));
#119188=CARTESIAN_POINT('Ctrl Pts',(-2.832719242,2.232664075,-6.94447274400001));
#119189=CARTESIAN_POINT('Ctrl Pts',(-3.209501092,2.168401865,-6.790779694));
#119190=CARTESIAN_POINT('Ctrl Pts',(-3.567442445,2.103255924,-6.597223234));
#119191=CARTESIAN_POINT('Ctrl Pts',(-2.516666969,2.232664075,-6.79918284600001));
#119192=CARTESIAN_POINT('Ctrl Pts',(-2.885565917,2.168401865,-6.662637643));
#119193=CARTESIAN_POINT('Ctrl Pts',(-3.237525941,2.103255924,-6.486981253));
#119194=CARTESIAN_POINT('',(-3.23331887357527,2.10403448611767,-6.48907921541247));
#119195=CARTESIAN_POINT('Origin',(0.0995677333265954,2.01791771040135,0.167703467424962));
#119196=CARTESIAN_POINT('Ctrl Pts',(-3.34678523697546,2.14301213127202,
-6.71185731172976));
#119197=CARTESIAN_POINT('Ctrl Pts',(-3.32850605734533,2.13706113135863,
-6.67603981394334));
#119198=CARTESIAN_POINT('Ctrl Pts',(-3.30953490584366,2.13073651740591,
-6.63883771552103));
#119199=CARTESIAN_POINT('Ctrl Pts',(-3.2710610826908,2.11752978374566,-6.56330090580391));
#119200=CARTESIAN_POINT('Ctrl Pts',(-3.25216877742398,2.11086978240132,
-6.52616973707515));
#119201=CARTESIAN_POINT('Ctrl Pts',(-3.23331887183686,2.10403448644393,
-6.48907921623583));
#119202=CARTESIAN_POINT('Ctrl Pts',(-3.11840538,2.103262031,-6.820963853));
#119203=CARTESIAN_POINT('Ctrl Pts',(-3.233065417,2.123129682,-6.768543626));
#119204=CARTESIAN_POINT('Ctrl Pts',(-3.345898807,2.142857143,-6.712299246));
#119205=CARTESIAN_POINT('Ctrl Pts',(-3.600888855,2.187438859,-6.585193635));
#119206=CARTESIAN_POINT('Ctrl Pts',(-3.845500817,2.232664075,-6.439108903));
#119207=CARTESIAN_POINT('Ctrl Pts',(-3.229076835,2.103262031,-6.491191169));
#119208=CARTESIAN_POINT('Ctrl Pts',(-3.33819341,2.123129682,-6.436910561));
#119209=CARTESIAN_POINT('Ctrl Pts',(-3.445423944,2.142857143,-6.378993169));
#119210=CARTESIAN_POINT('Ctrl Pts',(-3.6877522,2.187438859,-6.248106749));
#119211=CARTESIAN_POINT('Ctrl Pts',(-3.919452023,2.232664075,-6.09921272300001));
#119212=CARTESIAN_POINT('Ctrl Pts',(-3.91945201577089,2.23266407358896,
-6.09921272764555));
#119213=CARTESIAN_POINT('Ctrl Pts',(-3.79431723693095,2.20823916327371,
-6.17962634524914));
#119214=CARTESIAN_POINT('Ctrl Pts',(-3.66699289525697,2.18398287387826,
-6.25600075962498));
#119215=CARTESIAN_POINT('Ctrl Pts',(-3.53787432629011,2.15996091850635,
-6.32818656929695));
#119216=CARTESIAN_POINT('Ctrl Pts',(-3.50715721036665,2.15424613097601,
-6.34535946628199));
#119217=CARTESIAN_POINT('Ctrl Pts',(-3.47633860863562,2.14854458871641,
-6.36229553001448));
#119218=CARTESIAN_POINT('Ctrl Pts',(-3.44542394254845,2.14285714274096,
-6.37899316990622));
#119219=CARTESIAN_POINT('Ctrl Pts',(-3.37545704587549,2.12998516332753,
-6.41678371346767));
#119220=CARTESIAN_POINT('Ctrl Pts',(-3.3047384418402,2.11704095611477,-6.45349292782825));
#119221=CARTESIAN_POINT('Ctrl Pts',(-3.23331887791259,2.1040344875398,-6.48907921306364));
#119222=CARTESIAN_POINT('Ctrl Pts',(-4.259348203,2.232664075,-6.173163928));
#119223=CARTESIAN_POINT('Ctrl Pts',(-4.59428164,2.168401865,-5.942067176));
#119224=CARTESIAN_POINT('Ctrl Pts',(-4.902245606,2.103255924,-5.676089148));
#119225=CARTESIAN_POINT('Ctrl Pts',(-3.919452023,2.232664075,-6.09921272300001));
#119226=CARTESIAN_POINT('Ctrl Pts',(-4.250373136,2.168401865,-5.886557502));
#119227=CARTESIAN_POINT('Ctrl Pts',(-4.5563436,2.103255924,-5.639346859));
#119228=CARTESIAN_POINT('',(-4.55268589075539,2.10403448616461,-5.64230016800444));
#119229=CARTESIAN_POINT('Origin',(0.133291235478736,2.017917758889,0.142378628454944));
#119230=CARTESIAN_POINT('Ctrl Pts',(-4.71139017880313,2.14301213124691,
-5.8354779218392));
#119231=CARTESIAN_POINT('Ctrl Pts',(-4.68583860689175,2.13706112064235,
-5.80442724467249));
#119232=CARTESIAN_POINT('Ctrl Pts',(-4.65931375765888,2.13073653525099,
-5.77217329178188));
#119233=CARTESIAN_POINT('Ctrl Pts',(-4.60550117740287,2.11752978380513,
-5.70667313699972));
#119234=CARTESIAN_POINT('Ctrl Pts',(-4.57906846021973,2.11086978249623,
-5.67447136160385));
#119235=CARTESIAN_POINT('Ctrl Pts',(-4.55268588945731,2.1040344865579,-5.6423001689854));
#119236=CARTESIAN_POINT('Ctrl Pts',(-4.511804397,2.103262031,-5.99112853100001));
#119237=CARTESIAN_POINT('Ctrl Pts',(-4.612514947,2.123129682,-5.915285341));
#119238=CARTESIAN_POINT('Ctrl Pts',(-4.710619476,2.142857143,-5.83610008));
#119239=CARTESIAN_POINT('Ctrl Pts',(-4.93232405,2.187438859,-5.657150805));
#119240=CARTESIAN_POINT('Ctrl Pts',(-5.139813221,2.232664075,-5.461897111));
#119241=CARTESIAN_POINT('Ctrl Pts',(-4.548997036,2.103262031,-5.64527465800001));
#119242=CARTESIAN_POINT('Ctrl Pts',(-4.6438938,2.123129682,-5.568806262));
#119243=CARTESIAN_POINT('Ctrl Pts',(-4.736166816,2.142857143,-5.489191552));
#119244=CARTESIAN_POINT('Ctrl Pts',(-4.944692861,2.187438859,-5.309271772));
#119245=CARTESIAN_POINT('Ctrl Pts',(-5.138967857,2.232664075,-5.114050192));
#119246=CARTESIAN_POINT('Ctrl Pts',(-5.13896785074891,2.23266407354481,
-5.11405019828154));
#119247=CARTESIAN_POINT('Ctrl Pts',(-5.03404520691936,2.20823916389876,
-5.21948406613815));
#119248=CARTESIAN_POINT('Ctrl Pts',(-4.92611588207458,2.18398287519858,
-5.32144385596657));
#119249=CARTESIAN_POINT('Ctrl Pts',(-4.81553385235499,2.15996092059238,
-5.41969867423203));
#119250=CARTESIAN_POINT('Ctrl Pts',(-4.7892265476722,2.15424613238941,-5.4430733531669));
#119251=CARTESIAN_POINT('Ctrl Pts',(-4.76276921770239,2.14854458946511,
-5.46623855226876));
#119252=CARTESIAN_POINT('Ctrl Pts',(-4.73616681522128,2.14285714283382,
-5.48919155269031));
#119253=CARTESIAN_POINT('Ctrl Pts',(-4.67595955624502,2.12998516351878,
-5.54113938823304));
#119254=CARTESIAN_POINT('Ctrl Pts',(-4.61478570966966,2.11704095624726,
-5.59219277144713));
#119255=CARTESIAN_POINT('Ctrl Pts',(-4.55268589439775,2.10403448758647,
-5.6423001647471));
#119256=CARTESIAN_POINT('Ctrl Pts',(-5.486814776,2.232664075,-5.11320482800001));
#119257=CARTESIAN_POINT('Ctrl Pts',(-5.764238685,2.168401865,-4.815510201));
#119258=CARTESIAN_POINT('Ctrl Pts',(-6.007825211,2.103255924,-4.489547442));
#119259=CARTESIAN_POINT('Ctrl Pts',(-5.138967857,2.232664075,-5.114050192));
#119260=CARTESIAN_POINT('Ctrl Pts',(-5.416437632,2.168401865,-4.835228475));
#119261=CARTESIAN_POINT('Ctrl Pts',(-5.662111695,2.103255924,-4.528022874));
#119262=CARTESIAN_POINT('',(-5.65917437505436,2.10403448616662,-4.53169343530542));
#119263=CARTESIAN_POINT('Origin',(0.160781923469345,2.01791774637,0.110395999616852));
#119264=CARTESIAN_POINT('Ctrl Pts',(-5.85569575257519,2.14301213124708,
-4.68623807016988));
#119265=CARTESIAN_POINT('Ctrl Pts',(-5.82406658291385,2.13706112033571,
-4.66140617195806));
#119266=CARTESIAN_POINT('Ctrl Pts',(-5.79122822973611,2.1307365362573,-4.63560836239601));
#119267=CARTESIAN_POINT('Ctrl Pts',(-5.72459315521941,2.11752978376544,
-4.5832076747887));
#119268=CARTESIAN_POINT('Ctrl Pts',(-5.69185599037294,2.11086978245082,
-4.5574410118544));
#119269=CARTESIAN_POINT('Ctrl Pts',(-5.65917437376922,2.10403448653929,
-4.53169343683771));
#119270=CARTESIAN_POINT('Ctrl Pts',(-5.694236456,2.103262031,-4.881154698));
#119271=CARTESIAN_POINT('Ctrl Pts',(-5.776288404,2.123129682,-4.785434889));
#119272=CARTESIAN_POINT('Ctrl Pts',(-5.855076814,2.142857143,-4.687011361));
#119273=CARTESIAN_POINT('Ctrl Pts',(-6.033129253,2.187438859,-4.464585891));
#119274=CARTESIAN_POINT('Ctrl Pts',(-6.19379367,2.232664075,-4.229293082));
#119275=CARTESIAN_POINT('Ctrl Pts',(-5.656211191,2.103262031,-4.535391379));
#119276=CARTESIAN_POINT('Ctrl Pts',(-5.732450877,2.123129682,-4.440310772));
#119277=CARTESIAN_POINT('Ctrl Pts',(-5.805451792,2.142857143,-4.342721438));
#119278=CARTESIAN_POINT('Ctrl Pts',(-5.97042518,2.187438859,-4.122181147));
#119279=CARTESIAN_POINT('Ctrl Pts',(-6.118191265,2.232664075,-3.889760358));
#119280=CARTESIAN_POINT('Ctrl Pts',(-6.11819126023038,2.23266407354021,
-3.88976036550212));
#119281=CARTESIAN_POINT('Ctrl Pts',(-6.038386802732,2.20823916020164,-4.01528453383383));
#119282=CARTESIAN_POINT('Ctrl Pts',(-5.95489913341043,2.18398286787429,
-4.13806219287367));
#119283=CARTESIAN_POINT('Ctrl Pts',(-5.86802431742651,2.15996090971641,
-4.25779175283678));
#119284=CARTESIAN_POINT('Ctrl Pts',(-5.84735694074199,2.15424612514592,
-4.28627521939729));
#119285=CARTESIAN_POINT('Ctrl Pts',(-5.82649801453941,2.14854458583761,
-4.31458635487229));
#119286=CARTESIAN_POINT('Ctrl Pts',(-5.80545179132039,2.14285714280396,
-4.34272143928787));
#119287=CARTESIAN_POINT('Ctrl Pts',(-5.75781939364538,2.12998516349468,
-4.40639754486088));
#119288=CARTESIAN_POINT('Ctrl Pts',(-5.70905072577705,2.11704095625527,
-4.469407896851));
#119289=CARTESIAN_POINT('Ctrl Pts',(-5.65917437799496,2.10403448764214,
-4.53169343152591));
#119290=CARTESIAN_POINT('Ctrl Pts',(-6.45772398800001,2.232664075,-3.814157953));
#119291=CARTESIAN_POINT('Ctrl Pts',(-6.664666336,2.168401865,-3.463785321));
#119292=CARTESIAN_POINT('Ctrl Pts',(-6.832485586,2.103255924,-3.093079487));
#119293=CARTESIAN_POINT('Ctrl Pts',(-6.118191265,2.232664075,-3.889760358));
#119294=CARTESIAN_POINT('Ctrl Pts',(-6.329235524,2.168401865,-3.557809538));
#119295=CARTESIAN_POINT('Ctrl Pts',(-6.503125741,2.103255924,-3.204973572));
#119296=CARTESIAN_POINT('',(-6.50104615573101,2.10403448617462,-3.20918975457166));
#119297=CARTESIAN_POINT('Origin',(0.180754841449393,2.01791773564785,0.0732516632395214));
#119298=CARTESIAN_POINT('Ctrl Pts',(-6.72619550123132,2.14301213123526,
-3.31787493432136));
#119299=CARTESIAN_POINT('Ctrl Pts',(-6.68996775205999,2.13706113217375,
-3.30042296334979));
#119300=CARTESIAN_POINT('Ctrl Pts',(-6.65235119062877,2.1307365168745,-3.28228747872196));
#119301=CARTESIAN_POINT('Ctrl Pts',(-6.57600906312516,2.11752970468666,
-3.24543629492975));
#119302=CARTESIAN_POINT('Ctrl Pts',(-6.53849844888826,2.11086974369859,
-3.22730968301239));
#119303=CARTESIAN_POINT('Ctrl Pts',(-6.50104615485299,2.10403448649296,
-3.20918975626637));
#119304=CARTESIAN_POINT('Ctrl Pts',(-6.61041234600001,2.103262031,-3.542943496));
#119305=CARTESIAN_POINT('Ctrl Pts',(-6.669969036,2.123129682,-3.431822819));
#119306=CARTESIAN_POINT('Ctrl Pts',(-6.725757268,2.142857143,-3.3187632));
#119307=CARTESIAN_POINT('Ctrl Pts',(-6.851832038,2.187438859,-3.063261902));
#119308=CARTESIAN_POINT('Ctrl Pts',(-6.95815921200001,2.232664075,-2.798932008));
#119309=CARTESIAN_POINT('Ctrl Pts',(-6.49894719800001,2.103262031,-3.213438239));
#119310=CARTESIAN_POINT('Ctrl Pts',(-6.552964923,2.123129682,-3.104191285));
#119311=CARTESIAN_POINT('Ctrl Pts',(-6.603280295,2.142857143,-2.993190497));
#119312=CARTESIAN_POINT('Ctrl Pts',(-6.716987053,2.187438859,-2.742341913));
#119313=CARTESIAN_POINT('Ctrl Pts',(-6.81133485,2.232664075,-2.483589653));
#119314=CARTESIAN_POINT('Ctrl Pts',(-6.81133484702938,2.23266407357604,
-2.48358966114703));
#119315=CARTESIAN_POINT('Ctrl Pts',(-6.76038013566595,2.20823914906342,
-2.62333480722537));
#119316=CARTESIAN_POINT('Ctrl Pts',(-6.7052379020462,2.1839828457863,-2.7611894355538));
#119317=CARTESIAN_POINT('Ctrl Pts',(-6.64613245686244,2.15996087693181,
-2.89679536201218));
#119318=CARTESIAN_POINT('Ctrl Pts',(-6.63207140127089,2.15424610330256,
-2.92905571407529));
#119319=CARTESIAN_POINT('Ctrl Pts',(-6.61778622926372,2.14854457488727,
-2.96118894202542));
#119320=CARTESIAN_POINT('Ctrl Pts',(-6.60328029421641,2.14285714269277,
-2.99319049872867));
#119321=CARTESIAN_POINT('Ctrl Pts',(-6.57044999596232,2.12998516336823,
-3.06561744956076));
#119322=CARTESIAN_POINT('Ctrl Pts',(-6.5363668754193,2.11704095610237,-3.13763847664814));
#119323=CARTESIAN_POINT('Ctrl Pts',(-6.50104615793019,2.10403448763485,
-3.20918974991449));
#119324=CARTESIAN_POINT('Ctrl Pts',(-7.126677204,2.232664075,-2.336765291));
#119325=CARTESIAN_POINT('Ctrl Pts',(-7.253461596,2.168401865,-1.950097689));
#119326=CARTESIAN_POINT('Ctrl Pts',(-7.337666529,2.103255924,-1.551982574));
#119327=CARTESIAN_POINT('Ctrl Pts',(-6.81133485,2.232664075,-2.483589653));
#119328=CARTESIAN_POINT('Ctrl Pts',(-6.946085397,2.168401865,-2.114031381));
#119329=CARTESIAN_POINT('Ctrl Pts',(-7.040060855,2.103255924,-1.732063268));
#119330=CARTESIAN_POINT('',(-7.03893624373328,2.10403448613602,-1.73662792757353));
#119331=CARTESIAN_POINT('Origin',(0.19227601318856,2.01791769717493,0.032682179817278));
#119332=CARTESIAN_POINT('Ctrl Pts',(-7.28218582306869,2.14301213122963,
-1.7943716548747));
#119333=CARTESIAN_POINT('Ctrl Pts',(-7.24305332634239,2.13706112086173,
-1.7851155788767));
#119334=CARTESIAN_POINT('Ctrl Pts',(-7.20241782122318,2.13073653615391,
-1.77549058655946));
#119335=CARTESIAN_POINT('Ctrl Pts',(-7.11993850864511,2.11752970689892,
-1.7559122383386));
#119336=CARTESIAN_POINT('Ctrl Pts',(-7.07940817845469,2.11086974474719,
-1.74627308796845));
#119337=CARTESIAN_POINT('Ctrl Pts',(-7.03893624340029,2.10403448644561,
-1.7366279295276));
#119338=CARTESIAN_POINT('Ctrl Pts',(-7.217492702,2.103262031,-2.039068194));
#119339=CARTESIAN_POINT('Ctrl Pts',(-7.251769329,2.123129682,-1.917742529));
#119340=CARTESIAN_POINT('Ctrl Pts',(-7.281948786,2.142857143,-1.79533336));
#119341=CARTESIAN_POINT('Ctrl Pts',(-7.350150772,2.187438859,-1.518703192));
#119342=CARTESIAN_POINT('Ctrl Pts',(-7.397168962,2.232664075,-1.237695984));
#119343=CARTESIAN_POINT('Ctrl Pts',(-7.03779965700001,2.103262031,-1.741228298));
#119344=CARTESIAN_POINT('Ctrl Pts',(-7.067069611,2.123129682,-1.622923263));
#119345=CARTESIAN_POINT('Ctrl Pts',(-7.09234675,2.142857143,-1.503701295));
#119346=CARTESIAN_POINT('Ctrl Pts',(-7.149470077,2.187438859,-1.234273819));
#119347=CARTESIAN_POINT('Ctrl Pts',(-7.18598798700001,2.232664075,-0.961289056));
#119348=CARTESIAN_POINT('Ctrl Pts',(-7.18598798581391,2.23266407353109,
-0.961289064866521));
#119349=CARTESIAN_POINT('Ctrl Pts',(-7.16626565124671,2.20823915894989,
-1.1087207436533));
#119350=CARTESIAN_POINT('Ctrl Pts',(-7.14204729433149,2.18398286543511,
-1.25520629864654));
#119351=CARTESIAN_POINT('Ctrl Pts',(-7.1134749823763,2.15996090615119,-1.40034769983849));
#119352=CARTESIAN_POINT('Ctrl Pts',(-7.10667767780776,2.15424612276782,
-1.43487659308848));
#119353=CARTESIAN_POINT('Ctrl Pts',(-7.09963416776281,2.14854458464336,
-1.46932951247662));
#119354=CARTESIAN_POINT('Ctrl Pts',(-7.09234674973051,2.14285714278968,
-1.50370129627107));
#119355=CARTESIAN_POINT('Ctrl Pts',(-7.07585365867762,2.12998516347851,
-1.58149248822485));
#119356=CARTESIAN_POINT('Ctrl Pts',(-7.05804977456917,2.11704095615068,
-1.65915656746971));
#119357=CARTESIAN_POINT('Ctrl Pts',(-7.03893624466465,2.10403448753363,
-1.73662792249327));
#119358=CARTESIAN_POINT('Ctrl Pts',(-7.462394915,2.232664075,-0.750108081));
#119359=CARTESIAN_POINT('Ctrl Pts',(-7.503093053,2.168401865,-0.345225657));
#119360=CARTESIAN_POINT('Ctrl Pts',(-7.49974634,2.103255924,0.0616833200000001));
#119361=CARTESIAN_POINT('Ctrl Pts',(-7.185987987,2.232664075,-0.961289056000001));
#119362=CARTESIAN_POINT('Ctrl Pts',(-7.238144037,2.168401865,-0.571403467));
#119363=CARTESIAN_POINT('Ctrl Pts',(-7.247810547,2.103255924,-0.17816361));
#119364=CARTESIAN_POINT('',(-7.24769349611018,2.10403448614893,-0.182863309005228));
#119365=CARTESIAN_POINT('Origin',(0.194806409965016,2.01791775247604,-0.00941555982621519));
#119366=CARTESIAN_POINT('Ctrl Pts',(-7.49766922992161,2.14301213117218,
-0.186965550243363));
#119367=CARTESIAN_POINT('Ctrl Pts',(-7.45746192152156,2.1370611319295,-0.186338207433853));
#119368=CARTESIAN_POINT('Ctrl Pts',(-7.41570717295776,2.13073651822537,
-0.185673671629014));
#119369=CARTESIAN_POINT('Ctrl Pts',(-7.33094802269037,2.11752978372598,
-0.18428367832303));
#119370=CARTESIAN_POINT('Ctrl Pts',(-7.28929287292505,2.11086978243035,
-0.183582704619183));
#119371=CARTESIAN_POINT('Ctrl Pts',(-7.24769349602953,2.10403448649871,
-0.182863310345257));
#119372=CARTESIAN_POINT('Ctrl Pts',(-7.487091121,2.103262031,-0.43984833));
#119373=CARTESIAN_POINT('Ctrl Pts',(-7.494484947,2.123129682,-0.313990729));
#119374=CARTESIAN_POINT('Ctrl Pts',(-7.497644473,2.142857143,-0.187955727));
#119375=CARTESIAN_POINT('Ctrl Pts',(-7.504784626,2.187438859,0.0968683920000001));
#119376=CARTESIAN_POINT('Ctrl Pts',(-7.490295313,2.232664075,0.381413328));
#119377=CARTESIAN_POINT('Ctrl Pts',(-7.247572426,2.103262031,-0.187600458));
#119378=CARTESIAN_POINT('Ctrl Pts',(-7.25072598,2.123129682,-0.065769154));
#119379=CARTESIAN_POINT('Ctrl Pts',(-7.249782953,2.142857143,0.056099309));
#119380=CARTESIAN_POINT('Ctrl Pts',(-7.247651826,2.187438859,0.331507546));
#119381=CARTESIAN_POINT('Ctrl Pts',(-7.224632313,2.232664075,0.605960349000001));
#119382=CARTESIAN_POINT('Ctrl Pts',(-7.22463231372479,2.23266407357604,
0.605960340358616));
#119383=CARTESIAN_POINT('Ctrl Pts',(-7.23706452836554,2.20823916065962,
0.457735822982831));
#119384=CARTESIAN_POINT('Ctrl Pts',(-7.2449024470062,2.18398286877176,0.309468797995694));
#119385=CARTESIAN_POINT('Ctrl Pts',(-7.24819925090731,2.15996091108634,
0.161578529878988));
#119386=CARTESIAN_POINT('Ctrl Pts',(-7.24898355524294,2.15424612606176,
0.126395673403131));
#119387=CARTESIAN_POINT('Ctrl Pts',(-7.24951107796628,2.14854458630384,
0.0912340876929665));
#119388=CARTESIAN_POINT('Ctrl Pts',(-7.24978295323504,2.14285714282549,
0.056099307698734));
#119389=CARTESIAN_POINT('Ctrl Pts',(-7.25039826940105,2.12998516354546,
-0.0234186967996028));
#119390=CARTESIAN_POINT('Ctrl Pts',(-7.2497061112786,2.11704095613262,-0.103094342054953));
#119391=CARTESIAN_POINT('Ctrl Pts',(-7.2476934961534,2.10403448751907,-0.182863304051553));
#119392=CARTESIAN_POINT('Ctrl Pts',(-7.449179333,2.232664075,0.871623349000001));
#119393=CARTESIAN_POINT('Ctrl Pts',(-7.401888218,2.168401865,1.275788744));
#119394=CARTESIAN_POINT('Ctrl Pts',(-7.311146348,2.103255924,1.672464971));
#119395=CARTESIAN_POINT('Ctrl Pts',(-7.224632313,2.232664075,0.605960349000001));
#119396=CARTESIAN_POINT('Ctrl Pts',(-7.191755107,2.168401865,0.997942639));
#119397=CARTESIAN_POINT('Ctrl Pts',(-7.116660674,2.103255924,1.38406678));
#119398=CARTESIAN_POINT('',(-7.11755665582389,2.10403448616646,1.37945179518342));
#119399=CARTESIAN_POINT('Origin',(0.188227755794577,2.01791772706583,-0.0510730378310159));
#119400=CARTESIAN_POINT('Ctrl Pts',(-7.36256995640569,2.14301213123507,
1.42918285531713));
#119401=CARTESIAN_POINT('Ctrl Pts',(-7.32316781099792,2.13706113177995,
1.42115214801647));
#119402=CARTESIAN_POINT('Ctrl Pts',(-7.28224641026556,2.13073651812043,
1.41282511087366));
#119403=CARTESIAN_POINT('Ctrl Pts',(-7.19917007545252,2.11752978377754,
1.39596189507937));
#119404=CARTESIAN_POINT('Ctrl Pts',(-7.15833811113647,2.11086978244974,
1.38769185434603));
#119405=CARTESIAN_POINT('Ctrl Pts',(-7.11755665617418,2.1040344865323,1.37945179314629));
#119406=CARTESIAN_POINT('Ctrl Pts',(-7.40660148,2.103262031,1.179938354));
#119407=CARTESIAN_POINT('Ctrl Pts',(-7.386766779,2.123129682,1.304442928));
#119408=CARTESIAN_POINT('Ctrl Pts',(-7.362758637,2.142857143,1.428210506));
#119409=CARTESIAN_POINT('Ctrl Pts',(-7.308503091,2.187438859,1.707910518));
#119410=CARTESIAN_POINT('Ctrl Pts',(-7.23318378,2.232664075,1.982688177));
#119411=CARTESIAN_POINT('Ctrl Pts',(-7.118456763,2.103262031,1.374799371));
#119412=CARTESIAN_POINT('Ctrl Pts',(-7.095346459,2.123129682,1.494460248));
#119413=CARTESIAN_POINT('Ctrl Pts',(-7.068227363,2.142857143,1.613276771));
#119414=CARTESIAN_POINT('Ctrl Pts',(-7.00694143000001,2.187438859,1.881787987));
#119415=CARTESIAN_POINT('Ctrl Pts',(-6.925460861,2.232664075,2.144875721));
#119416=CARTESIAN_POINT('Ctrl Pts',(-6.92546086356549,2.23266407357604,
2.14487571271646));
#119417=CARTESIAN_POINT('Ctrl Pts',(-6.96946627562099,2.20823917943093,
2.00278927011421));
#119418=CARTESIAN_POINT('Ctrl Pts',(-7.00899394941072,2.18398290596486,
1.85967367665201));
#119419=CARTESIAN_POINT('Ctrl Pts',(-7.04400569229374,2.15996096621933,
1.71594982672751));
#119420=CARTESIAN_POINT('Ctrl Pts',(-7.05233496260397,2.1542461627551,1.68175801856626));
#119421=CARTESIAN_POINT('Ctrl Pts',(-7.06040888047637,2.14854460463559,
1.64753178316994));
#119422=CARTESIAN_POINT('Ctrl Pts',(-7.06822736368688,2.14285714288217,
1.61327676996052));
#119423=CARTESIAN_POINT('Ctrl Pts',(-7.08592231393104,2.12998516356634,
1.53575012699934));
#119424=CARTESIAN_POINT('Ctrl Pts',(-7.10237424704962,2.1170409562774,1.45778846079541));
#119425=CARTESIAN_POINT('Ctrl Pts',(-7.11755665457197,2.10403448768129,
1.37945180024277));
#119426=CARTESIAN_POINT('Ctrl Pts',(-7.087648405,2.232664075,2.45259864));
#119427=CARTESIAN_POINT('Ctrl Pts',(-6.954579317,2.168401865,2.837148681));
#119428=CARTESIAN_POINT('Ctrl Pts',(-6.780685278,2.103255924,3.205044018));
#119429=CARTESIAN_POINT('Ctrl Pts',(-6.925460861,2.232664075,2.144875721));
#119430=CARTESIAN_POINT('Ctrl Pts',(-6.809087701,2.168401865,2.520626056));
#119431=CARTESIAN_POINT('Ctrl Pts',(-6.652743657,2.103255924,2.881579746));
#119432=CARTESIAN_POINT('',(-6.65461077679171,2.10403448616333,2.8772652662477));
#119433=CARTESIAN_POINT('Origin',(0.172847689192316,2.01791773293874,-0.0903423007010168));
#119434=CARTESIAN_POINT('Ctrl Pts',(-6.8832050949221,2.1430121312801,2.97850425893303));
#119435=CARTESIAN_POINT('Ctrl Pts',(-6.84645051598016,2.13706113205809,
2.96219100944993));
#119436=CARTESIAN_POINT('Ctrl Pts',(-6.80827589352981,2.13073651702508,
2.94526175870189));
#119437=CARTESIAN_POINT('Ctrl Pts',(-6.73076693640448,2.11752978374688,
2.91093384222074));
#119438=CARTESIAN_POINT('Ctrl Pts',(-6.69266741499653,2.11086978242154,
2.89407948519025));
#119439=CARTESIAN_POINT('Ctrl Pts',(-6.65461077734004,2.1040344865073,2.8772652648668));
#119440=CARTESIAN_POINT('Ctrl Pts',(-6.979787386,2.103262031,2.744552431));
#119441=CARTESIAN_POINT('Ctrl Pts',(-6.933651607,2.123129682,2.861882283));
#119442=CARTESIAN_POINT('Ctrl Pts',(-6.883598391,2.142857143,2.977595203));
#119443=CARTESIAN_POINT('Ctrl Pts',(-6.770484074,2.187438859,3.239092645));
#119444=CARTESIAN_POINT('Ctrl Pts',(-6.63785661200001,2.232664075,3.491254731));
#119445=CARTESIAN_POINT('Ctrl Pts',(-6.656489974,2.103262031,2.87291511));
#119446=CARTESIAN_POINT('Ctrl Pts',(-6.608196425,2.123129682,2.98481035));
#119447=CARTESIAN_POINT('Ctrl Pts',(-6.556169318,2.142857143,3.095019205));
#119448=CARTESIAN_POINT('Ctrl Pts',(-6.438594242,2.187438859,3.344078114));
#119449=CARTESIAN_POINT('Ctrl Pts',(-6.302462557,2.232664075,3.583499089));
#119450=CARTESIAN_POINT('Ctrl Pts',(-6.30246256128625,2.23266407357604,
3.58349908146159));
#119451=CARTESIAN_POINT('Ctrl Pts',(-6.37598361868775,2.20823915216313,
3.45419425947911));
#119452=CARTESIAN_POINT('Ctrl Pts',(-6.44535285159381,2.18398285191355,
3.32292176254641));
#119453=CARTESIAN_POINT('Ctrl Pts',(-6.51044248130645,2.15996088600698,
3.19008443517309));
#119454=CARTESIAN_POINT('Ctrl Pts',(-6.5259271713798,2.15424610934197,3.15848270608615));
#119455=CARTESIAN_POINT('Ctrl Pts',(-6.54116988211619,2.14854457790376,
3.12679246227866));
#119456=CARTESIAN_POINT('Ctrl Pts',(-6.55616931878926,2.14285714270073,
3.09501920332812));
#119457=CARTESIAN_POINT('Ctrl Pts',(-6.59011650761173,2.12998516340818,
3.02310898135356));
#119458=CARTESIAN_POINT('Ctrl Pts',(-6.62294325708969,2.11704095609677,
2.95050669476758));
#119459=CARTESIAN_POINT('Ctrl Pts',(-6.65461077492281,2.10403448753761,
2.87726527063246));
#119460=CARTESIAN_POINT('Ctrl Pts',(-6.39470691500001,2.232664075,3.918893144));
#119461=CARTESIAN_POINT('Ctrl Pts',(-6.182082017,2.168401865,4.265846698));
#119462=CARTESIAN_POINT('Ctrl Pts',(-5.933166901,2.103255924,4.58775876899999));
#119463=CARTESIAN_POINT('Ctrl Pts',(-6.302462557,2.232664075,3.583499089));
#119464=CARTESIAN_POINT('Ctrl Pts',(-6.108034921,2.168401865,3.9254478));
#119465=CARTESIAN_POINT('Ctrl Pts',(-5.877751741,2.103255924,4.244353245));
#119466=CARTESIAN_POINT('',(-5.88050269387236,2.10403448615122,4.24054101112135));
#119467=CARTESIAN_POINT('Origin',(0.149385849193904,2.01791769792684,-0.125387414436151));
#119468=CARTESIAN_POINT('Ctrl Pts',(-6.08198921328939,2.14301213123481,
4.38855411340676));
#119469=CARTESIAN_POINT('Ctrl Pts',(-6.04960074080206,2.13706112071591,
4.36472106532138));
#119470=CARTESIAN_POINT('Ctrl Pts',(-6.01595806662983,2.13073653570991,
4.33998131233119));
#119471=CARTESIAN_POINT('Ctrl Pts',(-5.94764061628231,2.1175297837157,4.28979375773196));
#119472=CARTESIAN_POINT('Ctrl Pts',(-5.91405502901557,2.11086978238005,
4.26514317521297));
#119473=CARTESIAN_POINT('Ctrl Pts',(-5.88050269485777,2.10403448647498,
4.2405410096875));
#119474=CARTESIAN_POINT('Ctrl Pts',(-6.226606191,2.103262031,4.180834288));
#119475=CARTESIAN_POINT('Ctrl Pts',(-6.156326591,2.123129682,4.285503204));
#119476=CARTESIAN_POINT('Ctrl Pts',(-6.082568734,2.142857143,4.387750858));
#119477=CARTESIAN_POINT('Ctrl Pts',(-5.915884747,2.187438859,4.618818401));
#119478=CARTESIAN_POINT('Ctrl Pts',(-5.732150647,2.232664075,4.836574093));
#119479=CARTESIAN_POINT('Ctrl Pts',(-5.883273111,2.103262031,4.236696531));
#119480=CARTESIAN_POINT('Ctrl Pts',(-5.81205447,2.123129682,4.335594037));
#119481=CARTESIAN_POINT('Ctrl Pts',(-5.737552082,2.142857143,4.43204198));
#119482=CARTESIAN_POINT('Ctrl Pts',(-5.569185542,2.187438859,4.650002864));
#119483=CARTESIAN_POINT('Ctrl Pts',(-5.384768108,2.232664075,4.854562022));
#119484=CARTESIAN_POINT('Ctrl Pts',(-5.38476811398704,2.23266407353178,
4.85456201535907));
#119485=CARTESIAN_POINT('Ctrl Pts',(-5.48436695112432,2.20823916515672,
4.74408518097743));
#119486=CARTESIAN_POINT('Ctrl Pts',(-5.58033402759021,2.18398287769443,
4.6307941581107));
#119487=CARTESIAN_POINT('Ctrl Pts',(-5.67245795214641,2.15996092427026,
4.51505490397573));
#119488=CARTESIAN_POINT('Ctrl Pts',(-5.69437410617214,2.15424613483007,
4.4875206957593));
#119489=CARTESIAN_POINT('Ctrl Pts',(-5.71607296529475,2.14854459067243,
4.45984802322099));
#119490=CARTESIAN_POINT('Ctrl Pts',(-5.73755208278728,2.14285714281209,
4.43204197907132));
#119491=CARTESIAN_POINT('Ctrl Pts',(-5.78616417716126,2.12998516349167,
4.36911062020453));
#119492=CARTESIAN_POINT('Ctrl Pts',(-5.83383080093272,2.11704095618126,
4.30526251552709));
#119493=CARTESIAN_POINT('Ctrl Pts',(-5.88050269069905,2.10403448751903,
4.24054101494961));
#119494=CARTESIAN_POINT('Ctrl Pts',(-5.402756036,2.232664075,5.201944561));
#119495=CARTESIAN_POINT('Ctrl Pts',(-5.120517432,2.168401865,5.49507846600001));
#119496=CARTESIAN_POINT('Ctrl Pts',(-4.808220234,2.103255924,5.755955019));
#119497=CARTESIAN_POINT('Ctrl Pts',(-5.38476810800001,2.232664075,4.854562022));
#119498=CARTESIAN_POINT('Ctrl Pts',(-5.121377218,2.168401865,5.14671996700001));
#119499=CARTESIAN_POINT('Ctrl Pts',(-4.827922686,2.103255924,5.408665504));
#119500=CARTESIAN_POINT('',(-4.83142884100588,2.10403448617778,5.40553377166433));
#119501=CARTESIAN_POINT('Origin',(0.118938734844523,2.01791776995071,-0.154569479146689));
#119502=CARTESIAN_POINT('Ctrl Pts',(-4.99638627563914,2.14301213125791,
5.5934000559955));
#119503=CARTESIAN_POINT('Ctrl Pts',(-4.96987847844244,2.13706113193449,
5.56316170396712));
#119504=CARTESIAN_POINT('Ctrl Pts',(-4.94234053791621,2.13073651703642,
5.53176802477778));
#119505=CARTESIAN_POINT('Ctrl Pts',(-4.88640923164154,2.11752978377236,
5.46806768500414));
#119506=CARTESIAN_POINT('Ctrl Pts',(-4.85890800332318,2.11086978245107,
5.43677351095245));
#119507=CARTESIAN_POINT('Ctrl Pts',(-4.83142884221226,2.10403448652669,
5.40553377052683));
#119508=CARTESIAN_POINT('Ctrl Pts',(-5.182275811,2.103262031,5.421624979));
#119509=CARTESIAN_POINT('Ctrl Pts',(-5.091138586,2.123129682,5.508738758));
#119510=CARTESIAN_POINT('Ctrl Pts',(-4.997124924,2.142857143,5.59274016));
#119511=CARTESIAN_POINT('Ctrl Pts',(-4.784665224,2.187438859,5.782573342));
#119512=CARTESIAN_POINT('Ctrl Pts',(-4.558415688,2.232664075,5.955740627));
#119513=CARTESIAN_POINT('Ctrl Pts',(-4.834960937,2.103262031,5.402374731));
#119514=CARTESIAN_POINT('Ctrl Pts',(-4.744147307,2.123129682,5.483650165));
#119515=CARTESIAN_POINT('Ctrl Pts',(-4.650653287,2.142857143,5.561827398));
#119516=CARTESIAN_POINT('Ctrl Pts',(-4.439367916,2.187438859,5.738498649));
#119517=CARTESIAN_POINT('Ctrl Pts',(-4.215287887,2.232664075,5.89863103));
#119518=CARTESIAN_POINT('Ctrl Pts',(-4.21528789435224,2.23266407351613,
5.89863102474593));
#119519=CARTESIAN_POINT('Ctrl Pts',(-4.3363073888234,2.20823917136867,5.81214790559146));
#119520=CARTESIAN_POINT('Ctrl Pts',(-4.45438500029938,2.18398289002927,
5.72213567242712));
#119521=CARTESIAN_POINT('Ctrl Pts',(-4.56923560956039,2.15996094257694,
5.62890628343251));
#119522=CARTESIAN_POINT('Ctrl Pts',(-4.59655844647514,2.15424614701044,
5.6067271116584));
#119523=CARTESIAN_POINT('Ctrl Pts',(-4.62369883406465,2.14854459675296,
5.58436600038853));
#119524=CARTESIAN_POINT('Ctrl Pts',(-4.65065328800589,2.142857142822,5.56182739730908));
#119525=CARTESIAN_POINT('Ctrl Pts',(-4.71165724029445,2.12998516349101,
5.51081750162112));
#119526=CARTESIAN_POINT('Ctrl Pts',(-4.77193490002844,2.11704095622126,
5.45870904546891));
#119527=CARTESIAN_POINT('Ctrl Pts',(-4.83142883691819,2.10403448756895,
5.40553377475842));
#119528=CARTESIAN_POINT('Ctrl Pts',(-4.15817829,2.232664075,6.24175883100001));
#119529=CARTESIAN_POINT('Ctrl Pts',(-3.819523143,2.168401865,6.467366471));
#119530=CARTESIAN_POINT('Ctrl Pts',(-3.458446532,2.103255924,6.65500921));
#119531=CARTESIAN_POINT('Ctrl Pts',(-4.215287887,2.232664075,5.89863103));
#119532=CARTESIAN_POINT('Ctrl Pts',(-3.895249607,2.168401865,6.127337229));
#119533=CARTESIAN_POINT('Ctrl Pts',(-3.552345332,2.103255924,6.320074576));
#119534=CARTESIAN_POINT('',(-3.55644274485985,2.10403448617125,6.31776978103635));
#119535=CARTESIAN_POINT('Origin',(0.082930208574552,2.01791772973768,-0.176524146984284));
#119536=CARTESIAN_POINT('Ctrl Pts',(-3.67715786822644,2.14301213123246,
6.53670482815667));
#119537=CARTESIAN_POINT('Ctrl Pts',(-3.65777016219678,2.1370611324582,6.50147504250649));
#119538=CARTESIAN_POINT('Ctrl Pts',(-3.63762475105466,2.13073651583364,
6.46489547691489));
#119539=CARTESIAN_POINT('Ctrl Pts',(-3.59669478159521,2.11752978378474,
6.39066084503437));
#119540=CARTESIAN_POINT('Ctrl Pts',(-3.57656383913306,2.1108697824456,6.35418636013881));
#119541=CARTESIAN_POINT('Ctrl Pts',(-3.55644274658363,2.10403448654469,
6.31776978008171));
#119542=CARTESIAN_POINT('Ctrl Pts',(-3.895627974,2.103262031,6.408906513));
#119543=CARTESIAN_POINT('Ctrl Pts',(-3.787894599,2.123129682,6.47439181));
#119544=CARTESIAN_POINT('Ctrl Pts',(-3.678021106,2.142857143,6.536219148));
#119545=CARTESIAN_POINT('Ctrl Pts',(-3.429720073,2.187438859,6.67594158));
#119546=CARTESIAN_POINT('Ctrl Pts',(-3.171534278,2.232664075,6.796423348));
#119547=CARTESIAN_POINT('Ctrl Pts',(-3.560571363,2.103262031,6.315443893));
#119548=CARTESIAN_POINT('Ctrl Pts',(-3.45440909,2.123129682,6.375296907));
#119549=CARTESIAN_POINT('Ctrl Pts',(-3.346295113,2.142857143,6.431547949));
#119550=CARTESIAN_POINT('Ctrl Pts',(-3.101970381,2.187438859,6.558668615));
#119551=CARTESIAN_POINT('Ctrl Pts',(-2.84870549,2.232664075,6.666886607));
#119552=CARTESIAN_POINT('Ctrl Pts',(-2.84870549797434,2.23266407357603,
6.66688660359263));
#119553=CARTESIAN_POINT('Ctrl Pts',(-2.98548704572222,2.20823915222455,
6.60844097999876));
#119554=CARTESIAN_POINT('Ctrl Pts',(-3.12015414092708,2.18398285202096,
6.54591632681462));
#119555=CARTESIAN_POINT('Ctrl Pts',(-3.25236126881296,2.15996088615698,
6.47955601744561));
#119556=CARTESIAN_POINT('Ctrl Pts',(-3.28381307499604,2.1542461094534,6.46376903514065));
#119557=CARTESIAN_POINT('Ctrl Pts',(-3.31512580993533,2.14854457797663,
6.44776514722032));
#119558=CARTESIAN_POINT('Ctrl Pts',(-3.34629511470663,2.14285714273527,
6.43154794832585));
#119559=CARTESIAN_POINT('Ctrl Pts',(-3.41683844901538,2.12998516343135,
6.39484468235121));
#119560=CARTESIAN_POINT('Ctrl Pts',(-3.48690862792303,2.11704095624996,
6.35691240809715));
#119561=CARTESIAN_POINT('Ctrl Pts',(-3.55644274019248,2.10403448765571,
6.317769783299));
#119562=CARTESIAN_POINT('Ctrl Pts',(-2.719168749,2.232664075,6.989715396));
#119563=CARTESIAN_POINT('Ctrl Pts',(-2.339932197,2.168401865,7.137247609));
#119564=CARTESIAN_POINT('Ctrl Pts',(-1.946959715,2.103255924,7.242882566));
#119565=CARTESIAN_POINT('Ctrl Pts',(-2.84870549,2.232664075,6.666886607));
#119566=CARTESIAN_POINT('Ctrl Pts',(-2.486984455,2.168401865,6.821447013));
#119567=CARTESIAN_POINT('Ctrl Pts',(-2.110664259,2.103255924,6.935963984));
#119568=CARTESIAN_POINT('',(-2.11516133921097,2.10403448613605,6.93459389680005));
#119569=CARTESIAN_POINT('Origin',(0.0430438123248453,2.01791774548237,-0.190224481398423));
#119570=CARTESIAN_POINT('Ctrl Pts',(-2.18598964688697,2.14301213127581,
7.17436054715705));
#119571=CARTESIAN_POINT('Ctrl Pts',(-2.17462855492618,2.13706112079029,
7.13578655461992));
#119572=CARTESIAN_POINT('Ctrl Pts',(-2.16281771494847,2.13073653523302,
7.09573172665891));
#119573=CARTESIAN_POINT('Ctrl Pts',(-2.13880288145904,2.11752978374283,
7.01443380632184));
#119574=CARTESIAN_POINT('Ctrl Pts',(-2.12698352521162,2.11086978238224,
6.97448451705866));
#119575=CARTESIAN_POINT('Ctrl Pts',(-2.11516134064851,2.10403448644958,
6.93459389632029));
#119576=CARTESIAN_POINT('Ctrl Pts',(-2.426824903,2.103262031,7.0965147));
#119577=CARTESIAN_POINT('Ctrl Pts',(-2.307532871,2.123129682,7.137309497));
#119578=CARTESIAN_POINT('Ctrl Pts',(-2.186937109,2.142857143,7.174071792));
#119579=CARTESIAN_POINT('Ctrl Pts',(-1.914405023,2.187438859,7.25715021));
#119580=CARTESIAN_POINT('Ctrl Pts',(-1.63635545,2.232664075,7.319312867));
#119581=CARTESIAN_POINT('Ctrl Pts',(-2.119693429,2.103262031,6.933209918));
#119582=CARTESIAN_POINT('Ctrl Pts',(-2.003146542,2.123129682,6.968841851));
#119583=CARTESIAN_POINT('Ctrl Pts',(-1.885467899,2.142857143,7.000536465));
#119584=CARTESIAN_POINT('Ctrl Pts',(-1.619528158,2.187438859,7.072162525));
#119585=CARTESIAN_POINT('Ctrl Pts',(-1.34892079,2.232664075,7.12340597600001));
#119586=CARTESIAN_POINT('Ctrl Pts',(-1.34892079852034,2.23266407357604,
7.12340597438655));
#119587=CARTESIAN_POINT('Ctrl Pts',(-1.49506844498092,2.20823916996667,
7.09573078629201));
#119588=CARTESIAN_POINT('Ctrl Pts',(-1.64002794687247,2.18398288716985,
7.06361739593309));
#119589=CARTESIAN_POINT('Ctrl Pts',(-1.78340954923378,2.15996093828879,
7.0272292105977));
#119590=CARTESIAN_POINT('Ctrl Pts',(-1.81751986821592,2.15424614416311,
7.01857250298299));
#119591=CARTESIAN_POINT('Ctrl Pts',(-1.85154099512468,2.1485445953398,7.00967406320081));
#119592=CARTESIAN_POINT('Ctrl Pts',(-1.88546790014525,2.1428571428359,7.00053646483213));
#119593=CARTESIAN_POINT('Ctrl Pts',(-1.96225208760458,2.12998516346518,
6.97985603268479));
#119594=CARTESIAN_POINT('Ctrl Pts',(-2.03883838298836,2.11704095611587,
6.95787361101836));
#119595=CARTESIAN_POINT('Ctrl Pts',(-2.11516133429163,2.10403448747751,
6.93459389798712));
#119596=CARTESIAN_POINT('Ctrl Pts',(-1.153013899,2.232664075,7.410840637));
#119597=CARTESIAN_POINT('Ctrl Pts',(-0.750928622,2.168401865,7.47339898));
#119598=CARTESIAN_POINT('Ctrl Pts',(-0.344435225,2.103255924,7.492086784));
#119599=CARTESIAN_POINT('Ctrl Pts',(-1.34892079,2.232664075,7.123405976));
#119600=CARTESIAN_POINT('Ctrl Pts',(-0.962430673,2.168401865,7.19659351500001));
#119601=CARTESIAN_POINT('Ctrl Pts',(-0.57029087,2.103255924,7.227535425));
#119602=CARTESIAN_POINT('',(-0.574977339844184,2.10403448631433,7.22716410899259));
#119603=CARTESIAN_POINT('Origin',(0.00114484907014038,2.01791774551872,
-0.195030425692181));
#119604=CARTESIAN_POINT('Ctrl Pts',(-0.592606977972668,2.14301213123161,
7.47655114138138));
#119605=CARTESIAN_POINT('Ctrl Pts',(-0.58980377572683,2.13706113256072,
7.43643676802673));
#119606=CARTESIAN_POINT('Ctrl Pts',(-0.58687965707151,2.13073651668701,
7.3947792195583));
#119607=CARTESIAN_POINT('Ctrl Pts',(-0.580902935316097,2.11752978377134,
7.31021963858121));
#119608=CARTESIAN_POINT('Ctrl Pts',(-0.577947825397008,2.11086978246525,
7.26866352942372));
#119609=CARTESIAN_POINT('Ctrl Pts',(-0.574977341364854,2.10403448656429,
7.22716410884257));
#119610=CARTESIAN_POINT('Ctrl Pts',(-0.844546196,2.103262031,7.452297748));
#119611=CARTESIAN_POINT('Ctrl Pts',(-0.71927347,2.123129682,7.46649452400001));
#119612=CARTESIAN_POINT('Ctrl Pts',(-0.593594363,2.142857143,7.476472814));
#119613=CARTESIAN_POINT('Ctrl Pts',(-0.309574522,2.187438859,7.499022561));
#119614=CARTESIAN_POINT('Ctrl Pts',(-0.02466246,2.232664075,7.499959451));
#119615=CARTESIAN_POINT('Ctrl Pts',(-0.579700987,2.103262031,7.226786752));
#119616=CARTESIAN_POINT('Ctrl Pts',(-0.458219089,2.123129682,7.236531495));
#119617=CARTESIAN_POINT('Ctrl Pts',(-0.336478302,2.142857143,7.242187677));
#119618=CARTESIAN_POINT('Ctrl Pts',(-0.061358598,2.187438859,7.254969977));
#119619=CARTESIAN_POINT('Ctrl Pts',(0.213937947,2.232664075,7.24684279900001));
#119620=CARTESIAN_POINT('Ctrl Pts',(0.213937946177155,2.232664075,7.24684279987291));
#119621=CARTESIAN_POINT('Ctrl Pts',(0.0652582714129358,2.2082392481818,
7.25123205215457));
#119622=CARTESIAN_POINT('Ctrl Pts',(-0.0832151217912876,2.18398304100009,
7.25103147792061));
#119623=CARTESIAN_POINT('Ctrl Pts',(-0.231066464265715,2.15996116639334,
7.24631687763066));
#119624=CARTESIAN_POINT('Ctrl Pts',(-0.266240708327531,2.15424629586123,
7.2451952611578));
#119625=CARTESIAN_POINT('Ctrl Pts',(-0.301379809906624,2.1485446709918,
7.24381838362196));
#119626=CARTESIAN_POINT('Ctrl Pts',(-0.336478303285617,2.14285714284189,
7.24218767723706));
#119627=CARTESIAN_POINT('Ctrl Pts',(-0.415913000634215,2.12998516353286,
7.23849707277838));
#119628=CARTESIAN_POINT('Ctrl Pts',(-0.49543432170632,2.11704095620001,
7.23349237724681));
#119629=CARTESIAN_POINT('Ctrl Pts',(-0.574977334691461,2.10403448761162,
7.22716410912341));
#119630=CARTESIAN_POINT('Ctrl Pts',(-1.353927101,3.785444214,7.122456136));
#119631=CARTESIAN_POINT('Ctrl Pts',(-0.968373059999999,3.720864611,7.195747154));
#119632=CARTESIAN_POINT('Ctrl Pts',(-0.577160368,3.655724827,7.2269901));
#119633=CARTESIAN_POINT('Ctrl Pts',(-1.641499383,3.785444214,7.318160956));
#119634=CARTESIAN_POINT('Ctrl Pts',(-1.245351414,3.720864611,7.407018888));
#119635=CARTESIAN_POINT('Ctrl Pts',(-0.841926282,3.655724827,7.452594188));
#119636=CARTESIAN_POINT('',(-1.34934427538633,3.78467661253199,7.12332577179078));
#119637=CARTESIAN_POINT('Origin',(0.0106253979274054,3.6250144669058,-0.197552907747238));
#119638=CARTESIAN_POINT('Ctrl Pts',(-1.39775963841221,3.74576903859142,
7.3686001377517));
#119639=CARTESIAN_POINT('Ctrl Pts',(-1.39215392831734,3.75001846750314,
7.34045544110582));
#119640=CARTESIAN_POINT('Ctrl Pts',(-1.38653968409124,3.75433282935595,
7.31232213507245));
#119641=CARTESIAN_POINT('Ctrl Pts',(-1.38096227129015,3.75872286883793,
7.28419340331767));
#119642=CARTESIAN_POINT('Ctrl Pts',(-1.37564367939182,3.76290918770205,
7.25736999071461));
#119643=CARTESIAN_POINT('Ctrl Pts',(-1.37034856584378,3.76716275954374,
7.23055231415295));
#119644=CARTESIAN_POINT('Ctrl Pts',(-1.36507845944258,3.77148708937521,
7.20374123248363));
#119645=CARTESIAN_POINT('Ctrl Pts',(-1.35980819818422,3.77581154627309,
7.17692936299568));
#119646=CARTESIAN_POINT('Ctrl Pts',(-1.35456290478237,3.78020679563467,
7.15012388873262));
#119647=CARTESIAN_POINT('Ctrl Pts',(-1.34934427553073,3.78467661261598,
7.12332577112288));
#119648=CARTESIAN_POINT('Ctrl Pts',(-2.117255923,3.655724827,6.933954669));
#119649=CARTESIAN_POINT('Ctrl Pts',(-1.84081698,3.703213228,7.018364219));
#119650=CARTESIAN_POINT('Ctrl Pts',(-1.558535692,3.75,7.080499029));
#119651=CARTESIAN_POINT('Ctrl Pts',(-1.451936835,3.76766825,7.103963212));
#119652=CARTESIAN_POINT('Ctrl Pts',(-1.344679932,3.785449891,7.124207737));
#119653=CARTESIAN_POINT('Ctrl Pts',(-1.953843178,3.655724827,7.241028714));
#119654=CARTESIAN_POINT('Ctrl Pts',(-1.665161983,3.703213228,7.318923417));
#119655=CARTESIAN_POINT('Ctrl Pts',(-1.371195932,3.75,7.373589473));
#119656=CARTESIAN_POINT('Ctrl Pts',(-1.260184519,3.76766825,7.39423320399999));
#119657=CARTESIAN_POINT('Ctrl Pts',(-1.148601964,3.785449891,7.411525722));
#119658=CARTESIAN_POINT('Ctrl Pts',(-2.11725591807228,3.65572482784652,
6.93395467050466));
#119659=CARTESIAN_POINT('Ctrl Pts',(-1.9749657670162,3.68016831499129,6.97740241147478));
#119660=CARTESIAN_POINT('Ctrl Pts',(-1.83165561670273,3.70444732820564,
7.01636901394677));
#119661=CARTESIAN_POINT('Ctrl Pts',(-1.68774656448177,3.72849594166796,
7.05081637380165));
#119662=CARTESIAN_POINT('Ctrl Pts',(-1.64472605968218,3.73568508977861,
7.06111414720158));
#119663=CARTESIAN_POINT('Ctrl Pts',(-1.6016520313209,3.74285367318542,7.07100840506992));
#119664=CARTESIAN_POINT('Ctrl Pts',(-1.55853569152624,3.75000000007635,
7.08049902912192));
#119665=CARTESIAN_POINT('Ctrl Pts',(-1.48913063931403,3.76150355506906,
7.09577623651641));
#119666=CARTESIAN_POINT('Ctrl Pts',(-1.41938586396231,3.77306479256719,
7.11005806111148));
#119667=CARTESIAN_POINT('Ctrl Pts',(-1.34934427541734,3.7846766123156,7.12332577109486));
#119668=CARTESIAN_POINT('Ctrl Pts',(-2.853390569,3.785444214,6.664882764));
#119669=CARTESIAN_POINT('Ctrl Pts',(-2.492605969,3.720864611,6.819343002));
#119670=CARTESIAN_POINT('Ctrl Pts',(-2.117255923,3.655724827,6.933954669));
#119671=CARTESIAN_POINT('Ctrl Pts',(-3.176310322,3.785444214,6.794192575));
#119672=CARTESIAN_POINT('Ctrl Pts',(-2.808525901,3.720864611,6.96613316000001));
#119673=CARTESIAN_POINT('Ctrl Pts',(-2.424329967,3.655724827,7.097367414));
#119674=CARTESIAN_POINT('',(-2.84910183335486,3.7846766124451,6.6667172411859));
#119675=CARTESIAN_POINT('Origin',(0.0528447207396793,3.62501418821225,-0.190649488831013));
#119676=CARTESIAN_POINT('Ctrl Pts',(-2.94911201019669,3.74576903853266,
6.89584935663054));
#119677=CARTESIAN_POINT('Ctrl Pts',(-2.93758708077133,3.75001846748317,
6.86956772922826));
#119678=CARTESIAN_POINT('Ctrl Pts',(-2.92605626518708,3.75433282933,6.84329906083679));
#119679=CARTESIAN_POINT('Ctrl Pts',(-2.91456240336134,3.75872286881353,
6.81702694207654));
#119680=CARTESIAN_POINT('Ctrl Pts',(-2.90360191637789,3.76290918768055,
6.79197398598008));
#119681=CARTESIAN_POINT('Ctrl Pts',(-2.89266559197175,3.76716275952688,
6.76692158464856));
#119682=CARTESIAN_POINT('Ctrl Pts',(-2.88175510775647,3.77148708936756,
6.74187024814746));
#119683=CARTESIAN_POINT('Ctrl Pts',(-2.87084430300772,3.77581154625049,
6.71681817567609));
#119684=CARTESIAN_POINT('Ctrl Pts',(-2.85995925715714,3.78020679560255,
6.69176698148066));
#119685=CARTESIAN_POINT('Ctrl Pts',(-2.84910183346196,3.78467661243857,
6.66671724045537));
#119686=CARTESIAN_POINT('Ctrl Pts',(-3.558350943,3.655724827,6.316695225));
#119687=CARTESIAN_POINT('Ctrl Pts',(-3.306520548,3.703213228,6.458557527));
#119688=CARTESIAN_POINT('Ctrl Pts',(-3.044195986,3.75,6.579921793));
#119689=CARTESIAN_POINT('Ctrl Pts',(-2.945133458,3.76766825,6.625752999));
#119690=CARTESIAN_POINT('Ctrl Pts',(-2.844736136,3.785449891,6.668581282));
#119691=CARTESIAN_POINT('Ctrl Pts',(-3.46477054,3.655724827,6.651718958));
#119692=CARTESIAN_POINT('Ctrl Pts',(-3.19958361,3.703213228,6.78985045));
#119693=CARTESIAN_POINT('Ctrl Pts',(-2.924241908,3.75,6.906432456));
#119694=CARTESIAN_POINT('Ctrl Pts',(-2.820263672,3.76766825,6.95045772));
#119695=CARTESIAN_POINT('Ctrl Pts',(-2.715007236,3.785449891,6.991332899));
#119696=CARTESIAN_POINT('Ctrl Pts',(-3.55835093856568,3.65572482783619,
6.31669522749796));
#119697=CARTESIAN_POINT('Ctrl Pts',(-3.42872747054081,3.68016830784389,
6.38971533905775));
#119698=CARTESIAN_POINT('Ctrl Pts',(-3.29714453855422,3.70444731404074,
6.45857835112766));
#119699=CARTESIAN_POINT('Ctrl Pts',(-3.16400520355533,3.72849592062057,
6.52315652692829));
#119700=CARTESIAN_POINT('Ctrl Pts',(-3.12420417265987,3.73568507575255,
6.54246170049126));
#119701=CARTESIAN_POINT('Ctrl Pts',(-3.08426412533397,3.74285366614081,
6.56138429775543));
#119702=CARTESIAN_POINT('Ctrl Pts',(-3.04419598618343,3.74999999996728,
6.57992179291514));
#119703=CARTESIAN_POINT('Ctrl Pts',(-2.97969773445506,3.76150355493518,
6.60976186182413));
#119704=CARTESIAN_POINT('Ctrl Pts',(-2.91465372285346,3.77306479257878,
6.63870285047732));
#119705=CARTESIAN_POINT('Ctrl Pts',(-2.84910183331928,3.78467661222203,
6.66671724047858));
#119706=CARTESIAN_POINT('Ctrl Pts',(-4.219432665,3.785444214,5.895666882));
#119707=CARTESIAN_POINT('Ctrl Pts',(-3.900287394,3.720864611,6.124073949));
#119708=CARTESIAN_POINT('Ctrl Pts',(-3.558350943,3.655724827,6.316695225));
#119709=CARTESIAN_POINT('Ctrl Pts',(-4.56260052,3.785444214,5.9525353));
#119710=CARTESIAN_POINT('Ctrl Pts',(-4.240376838,3.720864611,6.199518789));
#119711=CARTESIAN_POINT('Ctrl Pts',(-3.893374677,3.655724827,6.41027562800001));
#119712=CARTESIAN_POINT('',(-4.21563855624423,3.78467661244694,5.89838042167661));
#119713=CARTESIAN_POINT('Origin',(0.0925935034102404,3.6250141983369,-0.174832560614677));
#119714=CARTESIAN_POINT('Ctrl Pts',(-4.36256718214553,3.74576903864837,
6.10065632342285));
#119715=CARTESIAN_POINT('Ctrl Pts',(-4.34566192601587,3.75001846755915,
6.07746666510329));
#119716=CARTESIAN_POINT('Ctrl Pts',(-4.32875370718208,3.75433282938854,
6.05429092807439));
#119717=CARTESIAN_POINT('Ctrl Pts',(-4.31188083645845,3.75872286886535,
6.03110387735168));
#119718=CARTESIAN_POINT('Ctrl Pts',(-4.29579095460153,3.76290918770143,
6.00899282625375));
#119719=CARTESIAN_POINT('Ctrl Pts',(-4.27972478969674,3.76716275952398,
5.98687712269222));
#119720=CARTESIAN_POINT('Ctrl Pts',(-4.2636840897836,3.7714870893529,5.96475690416098));
#119721=CARTESIAN_POINT('Ctrl Pts',(-4.24764291863144,3.77581154622073,
5.94263603578839));
#119722=CARTESIAN_POINT('Ctrl Pts',(-4.23162709297523,3.78020679556982,
5.92051048772824));
#119723=CARTESIAN_POINT('Ctrl Pts',(-4.21563855622686,3.78467661242271,
5.89838042089163));
#119724=CARTESIAN_POINT('Ctrl Pts',(-4.833061429,3.655724827,5.404074132));
#119725=CARTESIAN_POINT('Ctrl Pts',(-4.61761489,3.703213228,5.596755863));
#119726=CARTESIAN_POINT('Ctrl Pts',(-4.38751306,3.75,5.771674726));
#119727=CARTESIAN_POINT('Ctrl Pts',(-4.300618913,3.76766825,5.83772994));
#119728=CARTESIAN_POINT('Ctrl Pts',(-4.21177564,3.785449891,5.901139378));
#119729=CARTESIAN_POINT('Ctrl Pts',(-4.813689083,3.655724827,5.751382217));
#119730=CARTESIAN_POINT('Ctrl Pts',(-4.584396264,3.703213228,5.943291623));
#119731=CARTESIAN_POINT('Ctrl Pts',(-4.340553583,3.75,6.116338332));
#119732=CARTESIAN_POINT('Ctrl Pts',(-4.24847043,3.76766825,6.181686558));
#119733=CARTESIAN_POINT('Ctrl Pts',(-4.154461786,3.785449891,6.244233121));
#119734=CARTESIAN_POINT('Ctrl Pts',(-4.83306142520631,3.6557248278362,5.40407413539284));
#119735=CARTESIAN_POINT('Ctrl Pts',(-4.72216563184353,3.68016831124059,
5.50325230504341));
#119736=CARTESIAN_POINT('Ctrl Pts',(-4.60846253156385,3.70444732075457,
5.59879179157711));
#119737=CARTESIAN_POINT('Ctrl Pts',(-4.4923183023693,3.72849593057745,5.69048119835488));
#119738=CARTESIAN_POINT('Ctrl Pts',(-4.45759785485245,3.73568508238464,
5.71789105985171));
#119739=CARTESIAN_POINT('Ctrl Pts',(-4.42265939864353,3.74285366946605,
5.74495717419604));
#119740=CARTESIAN_POINT('Ctrl Pts',(-4.38751305994637,3.75000000000682,
5.77167472617292));
#119741=CARTESIAN_POINT('Ctrl Pts',(-4.33093747394232,3.7615035549861,5.81468236902783));
#119742=CARTESIAN_POINT('Ctrl Pts',(-4.27363561251273,3.77306479258905,
5.85692927332391));
#119743=CARTESIAN_POINT('Ctrl Pts',(-4.2156385560841,3.78467661217519,5.89838042094478));
#119744=CARTESIAN_POINT('Ctrl Pts',(-5.388178779,3.785444214,4.85077617));
#119745=CARTESIAN_POINT('Ctrl Pts',(-5.125595715,3.720864611,5.142450006));
#119746=CARTESIAN_POINT('Ctrl Pts',(-4.83306142900001,3.655724827,5.404074132));
#119747=CARTESIAN_POINT('Ctrl Pts',(-5.735548589,3.785444214,4.83254409));
#119748=CARTESIAN_POINT('Ctrl Pts',(-5.473952467,3.720864611,5.143021809));
#119749=CARTESIAN_POINT('Ctrl Pts',(-5.180369514,3.655724827,5.423446478));
#119750=CARTESIAN_POINT('',(-5.38505670423473,3.78467661256409,4.85424188857806));
#119751=CARTESIAN_POINT('Origin',(0.128012373723314,3.62501421072075,-0.15084001019758));
#119752=CARTESIAN_POINT('Ctrl Pts',(-5.57203356107251,3.74576903855143,
5.02020338136684));
#119753=CARTESIAN_POINT('Ctrl Pts',(-5.55053844964326,3.7500184675163,5.00119001457086));
#119754=CARTESIAN_POINT('Ctrl Pts',(-5.52904343725189,3.75433282935624,
4.98219088070486));
#119755=CARTESIAN_POINT('Ctrl Pts',(-5.50758051440555,3.75872286883733,
4.96317309889155));
#119756=CARTESIAN_POINT('Ctrl Pts',(-5.48711358252958,3.76290918771084,
4.94503784081921));
#119757=CARTESIAN_POINT('Ctrl Pts',(-5.46666881295276,3.76716275956891,
4.92689294063437));
#119758=CARTESIAN_POINT('Ctrl Pts',(-5.44624794248302,3.77148708941655,
4.90873815689551));
#119759=CARTESIAN_POINT('Ctrl Pts',(-5.42582647195078,3.77581154633361,
4.89058283968258));
#119760=CARTESIAN_POINT('Ctrl Pts',(-5.40542874841309,3.78020679571413,
4.87241750373948));
#119761=CARTESIAN_POINT('Ctrl Pts',(-5.38505670397224,3.78467661270115,
4.85424188794923));
#119762=CARTESIAN_POINT('Ctrl Pts',(-5.881783334,3.655724827,4.238764539));
#119763=CARTESIAN_POINT('Ctrl Pts',(-5.712794691,3.703213228,4.473256116));
#119764=CARTESIAN_POINT('Ctrl Pts',(-5.5256749,3.75,4.693550565));
#119765=CARTESIAN_POINT('Ctrl Pts',(-5.455012208,3.76766825,4.776741117));
#119766=CARTESIAN_POINT('Ctrl Pts',(-5.381877196,3.785449891,4.857766756));
#119767=CARTESIAN_POINT('Ctrl Pts',(-5.937524875,3.655724827,4.582117236));
#119768=CARTESIAN_POINT('Ctrl Pts',(-5.75484764300001,3.703213228,4.818831084));
#119769=CARTESIAN_POINT('Ctrl Pts',(-5.553905796,3.75,5.040251027));
#119770=CARTESIAN_POINT('Ctrl Pts',(-5.478023433,3.76766825,5.123866603));
#119771=CARTESIAN_POINT('Ctrl Pts',(-5.399658321,3.785449891,5.205159941));
#119772=CARTESIAN_POINT('Ctrl Pts',(-5.88178333102439,3.65572482783619,
4.23876454312901));
#119773=CARTESIAN_POINT('Ctrl Pts',(-5.79480058251351,3.68016831447287,
4.35946331600408));
#119774=CARTESIAN_POINT('Ctrl Pts',(-5.70429395042422,3.7044473271979,4.47721196332595));
#119775=CARTESIAN_POINT('Ctrl Pts',(-5.61057560779318,3.72849594018888,
4.59172531338442));
#119776=CARTESIAN_POINT('Ctrl Pts',(-5.58255922733452,3.73568508878181,
4.62595820198196));
#119777=CARTESIAN_POINT('Ctrl Pts',(-5.55425603991417,3.74285367266895,
4.65990224573283));
#119778=CARTESIAN_POINT('Ctrl Pts',(-5.52567489984892,3.75000000003778,
4.69355056517787));
#119779=CARTESIAN_POINT('Ctrl Pts',(-5.47966739129328,3.76150355502565,
4.74771479136725));
#119780=CARTESIAN_POINT('Ctrl Pts',(-5.43278705104974,3.77306479261622,
4.80129219296576));
#119781=CARTESIAN_POINT('Ctrl Pts',(-5.38505670388047,3.78467661243118,
4.8542418879857));
#119782=CARTESIAN_POINT('Ctrl Pts',(-6.304979642,3.785444214,3.579068554));
#119783=CARTESIAN_POINT('Ctrl Pts',(-6.11123687700001,3.720864611,3.920370815));
#119784=CARTESIAN_POINT('Ctrl Pts',(-5.881783334,3.655724827,4.238764539));
#119785=CARTESIAN_POINT('Ctrl Pts',(-6.640308781,3.785444214,3.48658849));
#119786=CARTESIAN_POINT('Ctrl Pts',(-6.451572163,3.720864611,3.846042846));
#119787=CARTESIAN_POINT('Ctrl Pts',(-6.22513603100001,3.655724827,4.183022998));
#119788=CARTESIAN_POINT('',(-6.30267558725977,3.78467661246027,3.58312440082087));
#119789=CARTESIAN_POINT('Origin',(0.15744564959693,3.62501421946758,-0.119794573750415));
#119790=CARTESIAN_POINT('Ctrl Pts',(-6.52095784396231,3.7457690385946,3.70501130873339));
#119791=CARTESIAN_POINT('Ctrl Pts',(-6.49587796423671,3.75001846753171,
3.6910632775486));
#119792=CARTESIAN_POINT('Ctrl Pts',(-6.47080124111466,3.75433282936697,
3.67712912506813));
#119793=CARTESIAN_POINT('Ctrl Pts',(-6.44575184852869,3.75872286883072,
3.66316986236309));
#119794=CARTESIAN_POINT('Ctrl Pts',(-6.42186487777182,3.76290918767787,
3.64985838189991));
#119795=CARTESIAN_POINT('Ctrl Pts',(-6.3979974783993,3.76716275950069,3.63653272053864));
#119796=CARTESIAN_POINT('Ctrl Pts',(-6.37415129467673,3.77148708931986,
3.62319226906006));
#119797=CARTESIAN_POINT('Ctrl Pts',(-6.35030441032532,3.77581154619291,
3.60985142562337));
#119798=CARTESIAN_POINT('Ctrl Pts',(-6.32647856400905,3.78020679553667,
3.59649569275204));
#119799=CARTESIAN_POINT('Ctrl Pts',(-6.30267558683402,3.78467661244032,
3.58312440024228));
#119800=CARTESIAN_POINT('Ctrl Pts',(-6.655479587,3.655724827,2.875255027));
#119801=CARTESIAN_POINT('Ctrl Pts',(-6.540850562,3.703213228,3.140591884));
#119802=CARTESIAN_POINT('Ctrl Pts',(-6.405462322,3.75,3.395961195));
#119803=CARTESIAN_POINT('Ctrl Pts',(-6.354335194,3.76766825,3.492397189));
#119804=CARTESIAN_POINT('Ctrl Pts',(-6.300328155,3.785449891,3.587250358));
#119805=CARTESIAN_POINT('Ctrl Pts',(-6.783728602,3.655724827,3.198597545));
#119806=CARTESIAN_POINT('Ctrl Pts',(-6.656208743,3.703213228,3.46904736));
#119807=CARTESIAN_POINT('Ctrl Pts',(-6.507563547,3.75,3.728487185));
#119808=CARTESIAN_POINT('Ctrl Pts',(-6.451430149,3.76766825,3.82646034));
#119809=CARTESIAN_POINT('Ctrl Pts',(-6.392372834,3.785449891,3.922699268));
#119810=CARTESIAN_POINT('Ctrl Pts',(-6.65547958491555,3.65572482786355,
2.87525503182498));
#119811=CARTESIAN_POINT('Ctrl Pts',(-6.59647713513738,3.68016830533402,
3.01183060287484));
#119812=CARTESIAN_POINT('Ctrl Pts',(-6.53339900144488,3.70444730902973,
3.14628255331846));
#119813=CARTESIAN_POINT('Ctrl Pts',(-6.46648875464711,3.72849591317344,
3.27826527057431));
#119814=CARTESIAN_POINT('Ctrl Pts',(-6.44648641654104,3.73568507080001,
3.3177205567383));
#119815=CARTESIAN_POINT('Ctrl Pts',(-6.42614188288712,3.7428536636702,3.35695540555018));
#119816=CARTESIAN_POINT('Ctrl Pts',(-6.40546232214056,3.74999999996442,
3.39596119492824));
#119817=CARTESIAN_POINT('Ctrl Pts',(-6.37217415113294,3.76150355492965,
3.45874934637612));
#119818=CARTESIAN_POINT('Ctrl Pts',(-6.33790740515646,3.77306479242226,
3.5211520252893));
#119819=CARTESIAN_POINT('Ctrl Pts',(-6.3026755867305,3.78467661218534,3.58312440034133));
#119820=CARTESIAN_POINT('Ctrl Pts',(-6.926966664,3.785444214,2.140007671));
#119821=CARTESIAN_POINT('Ctrl Pts',(-6.811123395,3.720864611,2.514979442));
#119822=CARTESIAN_POINT('Ctrl Pts',(-6.655479587,3.655724827,2.875255027));
#119823=CARTESIAN_POINT('Ctrl Pts',(-7.234575514,3.785444214,1.977603887));
#119824=CARTESIAN_POINT('Ctrl Pts',(-7.127523515,3.720864611,2.369227193));
#119825=CARTESIAN_POINT('Ctrl Pts',(-6.978822105,3.655724827,2.747006012));
#119826=CARTESIAN_POINT('',(-6.92558836415996,3.78467661244452,2.1444639974593));
#119827=CARTESIAN_POINT('Origin',(0.179517066360537,3.62501419796814,-0.083147728267117));
#119828=CARTESIAN_POINT('Ctrl Pts',(-7.16496938531577,3.74576903859088,
2.21657702476992));
#119829=CARTESIAN_POINT('Ctrl Pts',(-7.13747744483996,3.75001846753709,
2.20834652356073));
#119830=CARTESIAN_POINT('Ctrl Pts',(-7.10999157065178,3.75433282938089,
2.20012889801899));
#119831=CARTESIAN_POINT('Ctrl Pts',(-7.08252699007823,3.75872286885859,
2.19188087402488));
#119832=CARTESIAN_POINT('Ctrl Pts',(-7.05633690862041,3.76290918771448,
2.18401560116213));
#119833=CARTESIAN_POINT('Ctrl Pts',(-7.03016289250742,3.76716275954892,
2.17613227165504));
#119834=CARTESIAN_POINT('Ctrl Pts',(-7.00400641660713,3.77148708937527,
2.16822993708759));
#119835=CARTESIAN_POINT('Ctrl Pts',(-6.97784917217286,3.7758115462598,2.16032737033241));
#119836=CARTESIAN_POINT('Ctrl Pts',(-6.95170927313872,3.78020679561047,
2.15240573970377));
#119837=CARTESIAN_POINT('Ctrl Pts',(-6.92558836364052,3.78467661253422,
2.14446399698953));
#119838=CARTESIAN_POINT('Ctrl Pts',(-7.117973011,3.655724827,1.377301786));
#119839=CARTESIAN_POINT('Ctrl Pts',(-7.063063531,3.703213228,1.661077066));
#119840=CARTESIAN_POINT('Ctrl Pts',(-6.985737446,3.75,1.939580454));
#119841=CARTESIAN_POINT('Ctrl Pts',(-6.95653653,3.76766825,2.044752649));
#119842=CARTESIAN_POINT('Ctrl Pts',(-6.924182773,3.785449891,2.148998121));
#119843=CARTESIAN_POINT('Ctrl Pts',(-7.312732719,3.655724827,1.665514988));
#119844=CARTESIAN_POINT('Ctrl Pts',(-7.24633292000001,3.703213228,1.957054837));
#119845=CARTESIAN_POINT('Ctrl Pts',(-7.156934859,3.75,2.242383426));
#119846=CARTESIAN_POINT('Ctrl Pts',(-7.123175161,3.76766825,2.350133045));
#119847=CARTESIAN_POINT('Ctrl Pts',(-7.086187098,3.785449891,2.456817537));
#119848=CARTESIAN_POINT('Ctrl Pts',(-7.11797301003313,3.65572482783619,
1.37730179099681));
#119849=CARTESIAN_POINT('Ctrl Pts',(-7.08970970895861,3.68016831136589,
1.52336811954265));
#119850=CARTESIAN_POINT('Ctrl Pts',(-7.05700949318934,3.70444732101029,
1.66823662756823));
#119851=CARTESIAN_POINT('Ctrl Pts',(-7.02003594244959,3.72849593099671,
1.81151742205105));
#119852=CARTESIAN_POINT('Ctrl Pts',(-7.00898297661549,3.73568508267999,
1.85435014150631));
#119853=CARTESIAN_POINT('Ctrl Pts',(-6.99754842866315,3.74285366964143,
1.89704113948066));
#119854=CARTESIAN_POINT('Ctrl Pts',(-6.98573744594291,3.75000000006696,
1.93958045449333));
#119855=CARTESIAN_POINT('Ctrl Pts',(-6.96672513038322,3.76150355507051,
2.00805662662846));
#119856=CARTESIAN_POINT('Ctrl Pts',(-6.94667425285339,3.77306479261547,
2.07636670287174));
#119857=CARTESIAN_POINT('Ctrl Pts',(-6.92558836356273,3.78467661226242,
2.1444639970924));
#119858=CARTESIAN_POINT('Ctrl Pts',(-7.225056424,3.785444214,0.600882408));
#119859=CARTESIAN_POINT('Ctrl Pts',(-7.192529353,3.720864611,0.991990426));
#119860=CARTESIAN_POINT('Ctrl Pts',(-7.117973011,3.655724827,1.377301786));
#119861=CARTESIAN_POINT('Ctrl Pts',(-7.490561537,3.785444214,0.376148724));
#119862=CARTESIAN_POINT('Ctrl Pts',(-7.470199788,3.720864611,0.781629111));
#119863=CARTESIAN_POINT('Ctrl Pts',(-7.406186214,3.655724827,1.182542078));
#119864=CARTESIAN_POINT('',(-7.22466832603432,3.78467661248487,0.605530842000411));
#119865=CARTESIAN_POINT('Origin',(0.193194190418122,3.62501420910875,-0.042612894957625));
#119866=CARTESIAN_POINT('Ctrl Pts',(-7.47395492118949,3.74576903857413,
0.624498063269066));
#119867=CARTESIAN_POINT('Ctrl Pts',(-7.44533641265202,3.75001846749754,
0.622369941210292));
#119868=CARTESIAN_POINT('Ctrl Pts',(-7.41672659636916,3.75433282935662,
0.620253089576217));
#119869=CARTESIAN_POINT('Ctrl Pts',(-7.38813104109206,3.75872286884412,
0.618101972734711));
#119870=CARTESIAN_POINT('Ctrl Pts',(-7.36086246801177,3.76290918771187,
0.616050678880527));
#119871=CARTESIAN_POINT('Ctrl Pts',(-7.33360570302689,3.76716275955502,
0.61397829698979));
#119872=CARTESIAN_POINT('Ctrl Pts',(-7.30636198266434,3.77148708938627,
0.611883583750487));
#119873=CARTESIAN_POINT('Ctrl Pts',(-7.2791174617877,3.77581154628119,0.609788808961313));
#119874=CARTESIAN_POINT('Ctrl Pts',(-7.25188578263253,3.78020679563828,
0.607671687265006));
#119875=CARTESIAN_POINT('Ctrl Pts',(-7.22466832542905,3.7846766125672,0.605530841610901));
#119876=CARTESIAN_POINT('Ctrl Pts',(-7.247637929,3.655724827,-0.185052556));
#119877=CARTESIAN_POINT('Ctrl Pts',(-7.255015499,3.703213228,0.103892131));
#119878=CARTESIAN_POINT('Ctrl Pts',(-7.23936725,3.75,0.392507087));
#119879=CARTESIAN_POINT('Ctrl Pts',(-7.233457948,3.76766825,0.501497748));
#119880=CARTESIAN_POINT('Ctrl Pts',(-7.2242703,3.785449891,0.610261121));
#119881=CARTESIAN_POINT('Ctrl Pts',(-7.499801582,3.655724827,0.054554802));
#119882=CARTESIAN_POINT('Ctrl Pts',(-7.497626623,3.703213228,0.353552605));
#119883=CARTESIAN_POINT('Ctrl Pts',(-7.471655851,3.75,0.651428311));
#119884=CARTESIAN_POINT('Ctrl Pts',(-7.461848419,3.76766825,0.76391614));
#119885=CARTESIAN_POINT('Ctrl Pts',(-7.448659129,3.785449891,0.876057748));
#119886=CARTESIAN_POINT('Ctrl Pts',(-7.24763792912991,3.65572482783619,
-0.18505255091221));
#119887=CARTESIAN_POINT('Ctrl Pts',(-7.25143535144642,3.68016831243512,
-0.0363253910426296));
#119888=CARTESIAN_POINT('Ctrl Pts',(-7.2506420949807,3.70444732310703,0.112185757815467));
#119889=CARTESIAN_POINT('Ctrl Pts',(-7.24533410011286,3.72849593402264,
0.260064953471494));
#119890=CARTESIAN_POINT('Ctrl Pts',(-7.24374731512805,3.73568508466364,
0.304272322369906));
#119891=CARTESIAN_POINT('Ctrl Pts',(-7.24175740340817,3.7428536705816,0.348423312034834));
#119892=CARTESIAN_POINT('Ctrl Pts',(-7.23936725054934,3.74999999996199,
0.392507087363699));
#119893=CARTESIAN_POINT('Ctrl Pts',(-7.23551978532587,3.76150355491796,
0.46346941028073));
#119894=CARTESIAN_POINT('Ctrl Pts',(-7.23062233359156,3.77306479251089,
0.534492781363057));
#119895=CARTESIAN_POINT('Ctrl Pts',(-7.2246683253825,3.78467661233474,0.605530841717469));
#119896=CARTESIAN_POINT('Ctrl Pts',(-7.185310576,3.785444214,-0.966339449));
#119897=CARTESIAN_POINT('Ctrl Pts',(-7.237620632,3.720864611,-0.57738296));
#119898=CARTESIAN_POINT('Ctrl Pts',(-7.24763792900001,3.655724827,-0.185052556));
#119899=CARTESIAN_POINT('Ctrl Pts',(-7.39629722700001,3.785444214,-1.242894736));
#119900=CARTESIAN_POINT('Ctrl Pts',(-7.463577823,3.720864611,-0.842517081));
#119901=CARTESIAN_POINT('Ctrl Pts',(-7.48724528700001,3.655724827,-0.437216209));
#119902=CARTESIAN_POINT('',(-7.18593082770886,3.7846766124854,-0.961716263426633));
#119903=CARTESIAN_POINT('Origin',(0.197837913337127,3.62501423301475,-8.55908097693869E-5));
#119904=CARTESIAN_POINT('Ctrl Pts',(-7.43346663201529,3.74576903857242,
-0.996781734613965));
#119905=CARTESIAN_POINT('Ctrl Pts',(-7.40505972491877,3.7500184674993,-0.992707968931452));
#119906=CARTESIAN_POINT('Ctrl Pts',(-7.37666372970027,3.75433282934856,
-0.988625064820828));
#119907=CARTESIAN_POINT('Ctrl Pts',(-7.34827429605646,3.75872286884045,
-0.98457869056506));
#119908=CARTESIAN_POINT('Ctrl Pts',(-7.32120227962763,3.76290918769198,
-0.980720089097213));
#119909=CARTESIAN_POINT('Ctrl Pts',(-7.29413726191584,3.7671627595281,-0.976884621059635));
#119910=CARTESIAN_POINT('Ctrl Pts',(-7.26708018324357,3.77148708936403,
-0.973073766491055));
#119911=CARTESIAN_POINT('Ctrl Pts',(-7.24002230959502,3.77581154625505,
-0.969262799954033));
#119912=CARTESIAN_POINT('Ctrl Pts',(-7.2129721734837,3.78020679562023,-0.965476418463916));
#119913=CARTESIAN_POINT('Ctrl Pts',(-7.18593082702751,3.78467661255006,
-0.961716263674782));
#119914=CARTESIAN_POINT('Ctrl Pts',(-7.038411352,3.655724827,-1.738754046));
#119915=CARTESIAN_POINT('Ctrl Pts',(-7.107731005,3.703213228,-1.458150685));
#119916=CARTESIAN_POINT('Ctrl Pts',(-7.154492288,3.75,-1.172919475));
#119917=CARTESIAN_POINT('Ctrl Pts',(-7.172150913,3.76766825,-1.06520663));
#119918=CARTESIAN_POINT('Ctrl Pts',(-7.186558977,3.785449891,-0.957011012));
#119919=CARTESIAN_POINT('Ctrl Pts',(-7.336188059,3.655724827,-1.558956307));
#119920=CARTESIAN_POINT('Ctrl Pts',(-7.39833963800001,3.703213228,-1.266481354));
#119921=CARTESIAN_POINT('Ctrl Pts',(-7.43701052,3.75,-0.969986869));
#119922=CARTESIAN_POINT('Ctrl Pts',(-7.451613939,3.76766825,-0.858020634));
#119923=CARTESIAN_POINT('Ctrl Pts',(-7.462840138,3.785449891,-0.745665527));
#119924=CARTESIAN_POINT('Ctrl Pts',(-7.03841135322059,3.65572482783619,
-1.73875404105908));
#119925=CARTESIAN_POINT('Ctrl Pts',(-7.07409192112379,3.68016830162473,
-1.59432043712552));
#119926=CARTESIAN_POINT('Ctrl Pts',(-7.10524270618244,3.70444730165851,
-1.44911093398924));
#119927=CARTESIAN_POINT('Ctrl Pts',(-7.13184845739956,3.72849590219442,
-1.30354807414556));
#119928=CARTESIAN_POINT('Ctrl Pts',(-7.13980206105466,3.73568506349874,
-1.26003307302222));
#119929=CARTESIAN_POINT('Ctrl Pts',(-7.14734984176541,3.74285366002429,
-1.21648647257524));
#119930=CARTESIAN_POINT('Ctrl Pts',(-7.15449228842347,3.74999999994902,
-1.17291947497001));
#119931=CARTESIAN_POINT('Ctrl Pts',(-7.16598957666898,3.76150355491072,
-1.10278912066276));
#119932=CARTESIAN_POINT('Ctrl Pts',(-7.17647455002868,3.77306479254669,
-1.03237342918396));
#119933=CARTESIAN_POINT('Ctrl Pts',(-7.18593082700197,3.78467661229154,
-0.961716263551076));
#119934=CARTESIAN_POINT('Ctrl Pts',(-6.809587591,3.785444214,-2.488376347));
#119935=CARTESIAN_POINT('Ctrl Pts',(-6.944288814,3.720864611,-2.119758561));
#119936=CARTESIAN_POINT('Ctrl Pts',(-7.038411352,3.655724827,-1.738754046));
#119937=CARTESIAN_POINT('Ctrl Pts',(-6.95619028,3.785444214,-2.803821818));
#119938=CARTESIAN_POINT('Ctrl Pts',(-7.107967253,3.720864611,-2.42726811));
#119939=CARTESIAN_POINT('Ctrl Pts',(-7.218209092,3.655724827,-2.036530753));
#119940=CARTESIAN_POINT('',(-6.81118718954655,3.78467661249988,-2.48399458494427));
#119941=CARTESIAN_POINT('Origin',(0.193231149625587,3.62501425022595,0.0424457680865267));
#119942=CARTESIAN_POINT('Ctrl Pts',(-7.04539770492945,3.74576903854636,
-2.57145312545179));
#119943=CARTESIAN_POINT('Ctrl Pts',(-7.01853067466861,3.75001846749528,
-2.56136795692049));
#119944=CARTESIAN_POINT('Ctrl Pts',(-6.99167626573214,3.75433282934435,
-2.55127620925497));
#119945=CARTESIAN_POINT('Ctrl Pts',(-6.96482041212457,3.75872286883609,
-2.54122154794212));
#119946=CARTESIAN_POINT('Ctrl Pts',(-6.93921080960062,3.76290918769569,
-2.5316334751332));
#119947=CARTESIAN_POINT('Ctrl Pts',(-6.91360306916377,3.76716275953997,
-2.52206949942425));
#119948=CARTESIAN_POINT('Ctrl Pts',(-6.88799779097978,3.77148708938402,
-2.51253126837146));
#119949=CARTESIAN_POINT('Ctrl Pts',(-6.86239176050391,3.77581154627836,
-2.50299275708217));
#119950=CARTESIAN_POINT('Ctrl Pts',(-6.83678800159914,3.78020679564683,
-2.49347991937481));
#119951=CARTESIAN_POINT('Ctrl Pts',(-6.81118718888813,3.78467661260747,
-2.48399458499447));
#119952=CARTESIAN_POINT('Ctrl Pts',(-6.500076484,3.655724827,-3.21115333));
#119953=CARTESIAN_POINT('Ctrl Pts',(-6.62809690900001,3.703213228,-2.952011995));
#119954=CARTESIAN_POINT('Ctrl Pts',(-6.735081219,3.75,-2.683501626));
#119955=CARTESIAN_POINT('Ctrl Pts',(-6.775482072,3.76766825,-2.58210313));
#119956=CARTESIAN_POINT('Ctrl Pts',(-6.812812143,3.785449891,-2.479534373));
#119957=CARTESIAN_POINT('Ctrl Pts',(-6.829542535,3.655724827,-3.099572351));
#119958=CARTESIAN_POINT('Ctrl Pts',(-6.953114514,3.703213228,-2.827296052));
#119959=CARTESIAN_POINT('Ctrl Pts',(-7.054618843,3.75,-2.54604654));
#119960=CARTESIAN_POINT('Ctrl Pts',(-7.092950272,3.76766825,-2.439837317));
#119961=CARTESIAN_POINT('Ctrl Pts',(-7.128067036,3.785449891,-2.332522311));
#119962=CARTESIAN_POINT('Ctrl Pts',(-6.50007648625421,3.65572482783619,
-3.21115332543699));
#119963=CARTESIAN_POINT('Ctrl Pts',(-6.5659718131589,3.68016830013526,-3.07776677391967));
#119964=CARTESIAN_POINT('Ctrl Pts',(-6.62761005750583,3.70444729873061,
-2.94264869413223));
#119965=CARTESIAN_POINT('Ctrl Pts',(-6.68488549041593,3.72849589790548,
-2.80620847119841));
#119966=CARTESIAN_POINT('Ctrl Pts',(-6.70200758579652,3.73568506065677,
-2.76542060819808));
#119967=CARTESIAN_POINT('Ctrl Pts',(-6.71874013893801,3.74285365862559,
-2.72451464466946));
#119968=CARTESIAN_POINT('Ctrl Pts',(-6.73508121915812,3.74999999998921,
-2.68350162598332));
#119969=CARTESIAN_POINT('Ctrl Pts',(-6.76138565968406,3.76150355498974,
-2.61748245745513));
#119970=CARTESIAN_POINT('Ctrl Pts',(-6.7867627926547,3.77306479254987,-2.55096700510787));
#119971=CARTESIAN_POINT('Ctrl Pts',(-6.81118718887542,3.78467661225419,
-2.48399458486229));
#119972=CARTESIAN_POINT('Ctrl Pts',(-6.115455858,3.785444214,-3.894059533));
#119973=CARTESIAN_POINT('Ctrl Pts',(-6.32624977,3.720864611,-3.563016607));
#119974=CARTESIAN_POINT('Ctrl Pts',(-6.500076484,3.655724827,-3.21115333));
#119975=CARTESIAN_POINT('Ctrl Pts',(-6.19081960600001,3.785444214,-4.233645309));
#119976=CARTESIAN_POINT('Ctrl Pts',(-6.419996035,3.720864611,-3.898522779));
#119977=CARTESIAN_POINT('Ctrl Pts',(-6.611657462,3.655724827,-3.540619381));
#119978=CARTESIAN_POINT('',(-6.11796000880229,3.78467661249981,-3.89012408040951));
#119979=CARTESIAN_POINT('Origin',(0.179589055403488,3.62501418376288,0.0829924647008767));
#119980=CARTESIAN_POINT('Ctrl Pts',(-6.32789381133271,3.74576903857982,
-4.02588622635888));
#119981=CARTESIAN_POINT('Ctrl Pts',(-6.30382293047905,3.75001846750999,
-4.01026122619376));
#119982=CARTESIAN_POINT('Ctrl Pts',(-6.27976579010809,3.75433282935617,
-3.99463251394156));
#119983=CARTESIAN_POINT('Ctrl Pts',(-6.25569926639655,3.75872286883614,
-3.97903971039016));
#119984=CARTESIAN_POINT('Ctrl Pts',(-6.23274955436762,3.76290918768585,
-3.96417049390017));
#119985=CARTESIAN_POINT('Ctrl Pts',(-6.20979648073913,3.76716275951515,
-3.94932521141505));
#119986=CARTESIAN_POINT('Ctrl Pts',(-6.18684027743799,3.77148708934838,
-3.93450560102785));
#119987=CARTESIAN_POINT('Ctrl Pts',(-6.16388339968018,3.77581154623106,
-3.91968555523829));
#119988=CARTESIAN_POINT('Ctrl Pts',(-6.140923221305,3.78020679559228,-3.90489107114311));
#119989=CARTESIAN_POINT('Ctrl Pts',(-6.11796000806892,3.78467661247508,
-3.89012408036331));
#119990=CARTESIAN_POINT('Ctrl Pts',(-5.657805263,3.655724827,-4.533402653));
#119991=CARTESIAN_POINT('Ctrl Pts',(-5.838540369,3.703213228,-4.307840506));
#119992=CARTESIAN_POINT('Ctrl Pts',(-6.000745237,3.75,-4.068606224));
#119993=CARTESIAN_POINT('Ctrl Pts',(-6.06199922,3.76766825,-3.978263357));
#119994=CARTESIAN_POINT('Ctrl Pts',(-6.120505785,3.785449891,-3.886117463));
#119995=CARTESIAN_POINT('Ctrl Pts',(-6.003555193,3.655724827,-4.495255837));
#119996=CARTESIAN_POINT('Ctrl Pts',(-6.182769484,3.703213228,-4.25590953));
#119997=CARTESIAN_POINT('Ctrl Pts',(-6.342361029,3.75,-4.003055905));
#119998=CARTESIAN_POINT('Ctrl Pts',(-6.402628134,3.76766825,-3.907569919));
#119999=CARTESIAN_POINT('Ctrl Pts',(-6.45999344200001,3.785449891,-3.810312944));
#120000=CARTESIAN_POINT('Ctrl Pts',(-5.65780526618243,3.65572482783619,
-4.53340264902825));
#120001=CARTESIAN_POINT('Ctrl Pts',(-5.75083422362151,3.68016831608079,
-4.41730007290052));
#120002=CARTESIAN_POINT('Ctrl Pts',(-5.84007784835361,3.70444733035584,
-4.29859130048564));
#120003=CARTESIAN_POINT('Ctrl Pts',(-5.92534487833161,3.72849594483852,
-4.17765341767066));
#120004=CARTESIAN_POINT('Ctrl Pts',(-5.95083479653685,3.73568509187778,
-4.14149997428622));
#120005=CARTESIAN_POINT('Ctrl Pts',(-5.97596966945381,3.74285367421748,
-4.10514745230995));
#120006=CARTESIAN_POINT('Ctrl Pts',(-6.00074523716432,3.75000000004653,
-4.06860622376149));
#120007=CARTESIAN_POINT('Ctrl Pts',(-6.04062686442943,3.76150355502397,
-4.00978522352873));
#120008=CARTESIAN_POINT('Ctrl Pts',(-6.07970954977572,3.77306479253944,
-3.95028019920642));
#120009=CARTESIAN_POINT('Ctrl Pts',(-6.11796000811214,3.78467661228328,
-3.89012408023804));
#120010=CARTESIAN_POINT('Ctrl Pts',(-5.135372207,3.785444214,-5.117660823));
#120011=CARTESIAN_POINT('Ctrl Pts',(-5.41240231700001,3.720864611,-4.839671956));
#120012=CARTESIAN_POINT('Ctrl Pts',(-5.657805263,3.655724827,-4.533402653));
#120013=CARTESIAN_POINT('Ctrl Pts',(-5.135973089,3.785444214,-5.46550825000001));
#120014=CARTESIAN_POINT('Ctrl Pts',(-5.431832937,3.720864611,-5.187486857));
#120015=CARTESIAN_POINT('Ctrl Pts',(-5.695952078,3.655724827,-4.879152583));
#120016=CARTESIAN_POINT('',(-5.13866381757032,3.78467661250474,-5.11435569747235));
#120017=CARTESIAN_POINT('Origin',(0.157549562756596,3.62501420442123,0.119658603587385));
#120018=CARTESIAN_POINT('Ctrl Pts',(-5.31450463650428,3.74576903856886,
-5.29207336192223));
#120019=CARTESIAN_POINT('Ctrl Pts',(-5.29435543258093,3.75001846751486,
-5.27163913767389));
#120020=CARTESIAN_POINT('Ctrl Pts',(-5.27422044602485,3.75433282934707,
-5.25120424192238));
#120021=CARTESIAN_POINT('Ctrl Pts',(-5.25406857613353,3.75872286882774,
-5.23080239827387));
#120022=CARTESIAN_POINT('Ctrl Pts',(-5.23485185760006,3.76290918769074,
-5.21134730606298));
#120023=CARTESIAN_POINT('Ctrl Pts',(-5.21562671092685,3.76716275954088,
-5.19191486568245));
#120024=CARTESIAN_POINT('Ctrl Pts',(-5.1963929890299,3.77148708939095,-5.17250682437492));
#120025=CARTESIAN_POINT('Ctrl Pts',(-5.17715870205999,3.77581154628672,
-5.15309821287304));
#120026=CARTESIAN_POINT('Ctrl Pts',(-5.15791569665113,3.78020679565695,
-5.13371385587399));
#120027=CARTESIAN_POINT('Ctrl Pts',(-5.13866381689417,3.78467661259413,
-5.11435569730711));
#120028=CARTESIAN_POINT('Ctrl Pts',(-4.550981356,3.655724827,-5.643675106));
#120029=CARTESIAN_POINT('Ctrl Pts',(-4.77598017,3.703213228,-5.462239182));
#120030=CARTESIAN_POINT('Ctrl Pts',(-4.985821077,3.75,-5.263467316));
#120031=CARTESIAN_POINT('Ctrl Pts',(-5.065064022,3.76766825,-5.188404412));
#120032=CARTESIAN_POINT('Ctrl Pts',(-5.14201138,3.785449891,-5.110990019));
#120033=CARTESIAN_POINT('Ctrl Pts',(-4.896848283,3.655724827,-5.680746157));
#120034=CARTESIAN_POINT('Ctrl Pts',(-5.123325024,3.703213228,-5.485521408));
#120035=CARTESIAN_POINT('Ctrl Pts',(-5.333541463,3.75,-5.272886825));
#120036=CARTESIAN_POINT('Ctrl Pts',(-5.41292622100001,3.76766825,-5.192588894));
#120037=CARTESIAN_POINT('Ctrl Pts',(-5.489857734,3.785449891,-5.109937579));
#120038=CARTESIAN_POINT('Ctrl Pts',(-4.55098135996182,3.65572482783619,
-5.64367510280524));
#120039=CARTESIAN_POINT('Ctrl Pts',(-4.66679394937079,3.68016831085496,
-5.55028543631377));
#120040=CARTESIAN_POINT('Ctrl Pts',(-4.77946996131795,3.7044473199498,-5.45353677174798));
#120041=CARTESIAN_POINT('Ctrl Pts',(-4.88874154317296,3.7284959293042,-5.35375626322254));
#120042=CARTESIAN_POINT('Ctrl Pts',(-4.9214074667792,3.7356850815309,-5.32392762513062));
#120043=CARTESIAN_POINT('Ctrl Pts',(-4.95376944141401,3.74285366902422,
-5.29382823817083));
#120044=CARTESIAN_POINT('Ctrl Pts',(-4.98582107706216,3.74999999996854,
-5.26346731613916));
#120045=CARTESIAN_POINT('Ctrl Pts',(-5.03741507037547,3.76150355490328,
-5.21459489019404));
#120046=CARTESIAN_POINT('Ctrl Pts',(-5.08837584583837,3.77306479260976,
-5.16488268167932));
#120047=CARTESIAN_POINT('Ctrl Pts',(-5.13866381694153,3.78467661224474,
-5.11435569717934));
#120048=CARTESIAN_POINT('Ctrl Pts',(-3.915164259,3.785444214,-6.101965981));
#120049=CARTESIAN_POINT('Ctrl Pts',(-4.245476948,3.720864611,-5.89002962400001));
#120050=CARTESIAN_POINT('Ctrl Pts',(-4.550981356,3.655724827,-5.643675106));
#120051=CARTESIAN_POINT('Ctrl Pts',(-3.840974177,3.785444214,-6.4418101));
#120052=CARTESIAN_POINT('Ctrl Pts',(-4.189683368,3.720864611,-6.233889815));
#120053=CARTESIAN_POINT('Ctrl Pts',(-4.513910305,3.655724827,-5.989542033));
#120054=CARTESIAN_POINT('',(-3.91908941653677,3.78467661230451,-6.09944572553291));
#120055=CARTESIAN_POINT('Origin',(0.128142893896167,3.62501424720021,0.150729317702604));
#120056=CARTESIAN_POINT('Ctrl Pts',(-4.05261513068026,3.74576903858172,
-6.31080902862542));
#120057=CARTESIAN_POINT('Ctrl Pts',(-4.03732975837536,3.75001846748708,
-6.2865210619541));
#120058=CARTESIAN_POINT('Ctrl Pts',(-4.02205841514173,3.75433282933544,
-6.26223549580967));
#120059=CARTESIAN_POINT('Ctrl Pts',(-4.00676347813404,3.758722868824,-6.23797857957129));
#120060=CARTESIAN_POINT('Ctrl Pts',(-3.99217830559993,3.76290918769149,
-6.21484731016465));
#120061=CARTESIAN_POINT('Ctrl Pts',(-3.9775800325423,3.7671627595409,-6.19173635117419));
#120062=CARTESIAN_POINT('Ctrl Pts',(-3.96296813980594,3.77148708935365,
-6.16864737757532));
#120063=CARTESIAN_POINT('Ctrl Pts',(-3.94835581754222,3.77581154628328,
-6.14555772525904));
#120064=CARTESIAN_POINT('Ctrl Pts',(-3.93372976681854,3.78020679564855,
-6.12248988635496));
#120065=CARTESIAN_POINT('Ctrl Pts',(-3.91908941594345,3.78467661291491,
-6.0994457254675));
#120066=CARTESIAN_POINT('Ctrl Pts',(-3.231358619,3.655724827,-6.490055583));
#120067=CARTESIAN_POINT('Ctrl Pts',(-3.490100446,3.703213228,-6.361229625));
#120068=CARTESIAN_POINT('Ctrl Pts',(-3.737765465,3.75,-6.212214527));
#120069=CARTESIAN_POINT('Ctrl Pts',(-3.831292059,3.76766825,-6.155941442));
#120070=CARTESIAN_POINT('Ctrl Pts',(-3.923082237,3.785449891,-6.096878362));
#120071=CARTESIAN_POINT('Ctrl Pts',(-3.561170189,3.655724827,-6.600611099));
#120072=CARTESIAN_POINT('Ctrl Pts',(-3.82431958,3.703213228,-6.458636401));
#120073=CARTESIAN_POINT('Ctrl Pts',(-4.075331425,3.75,-6.296163417));
#120074=CARTESIAN_POINT('Ctrl Pts',(-4.170121894,3.76766825,-6.23480818400001));
#120075=CARTESIAN_POINT('Ctrl Pts',(-4.26302238,3.785449891,-6.170627212));
#120076=CARTESIAN_POINT('Ctrl Pts',(-3.23135862351649,3.65572482782894,
-6.49005558075127));
#120077=CARTESIAN_POINT('Ctrl Pts',(-3.36453956354981,3.68016830479105,
-6.42374561295059));
#120078=CARTESIAN_POINT('Ctrl Pts',(-3.49537934446265,3.70444730795221,
-6.35348090887989));
#120079=CARTESIAN_POINT('Ctrl Pts',(-3.62354604724397,3.72849591153848,
-6.27952339325455));
#120080=CARTESIAN_POINT('Ctrl Pts',(-3.66186056706451,3.73568506971114,
-6.25741432251455));
#120081=CARTESIAN_POINT('Ctrl Pts',(-3.6999364466945,3.7428536631213,-6.2349754922436));
#120082=CARTESIAN_POINT('Ctrl Pts',(-3.73776546478839,3.74999999994898,
-6.21221452717703));
#120083=CARTESIAN_POINT('Ctrl Pts',(-3.79865934571585,3.76150355489174,
-6.17557589430039));
#120084=CARTESIAN_POINT('Ctrl Pts',(-3.85911534157287,3.77306479252643,
-6.1379809899611));
#120085=CARTESIAN_POINT('Ctrl Pts',(-3.91908941579481,3.78467661229662,
-6.09944572494293));
#120086=CARTESIAN_POINT('Ctrl Pts',(-2.511887581,3.785444214,-6.800949991));
#120087=CARTESIAN_POINT('Ctrl Pts',(-2.880037795,3.720864611,-6.664976053));
#120088=CARTESIAN_POINT('Ctrl Pts',(-3.231358619,3.655724827,-6.490055583));
#120089=CARTESIAN_POINT('Ctrl Pts',(-2.366375582,3.785444214,-7.11690007));
#120090=CARTESIAN_POINT('Ctrl Pts',(-2.751628862,3.720864611,-6.988803013));
#120091=CARTESIAN_POINT('Ctrl Pts',(-3.120803103,3.655724827,-6.819867154));
#120092=CARTESIAN_POINT('',(-2.51626275117737,3.78467661244294,-6.79933245108693));
#120093=CARTESIAN_POINT('Origin',(0.0927445870603161,3.62501424977788,0.174752169069451));
#120094=CARTESIAN_POINT('Ctrl Pts',(-2.60122984628958,3.74576903855236,
-7.03445827945423));
#120095=CARTESIAN_POINT('Ctrl Pts',(-2.59152303216242,3.75001846749456,
-7.00745224865496));
#120096=CARTESIAN_POINT('Ctrl Pts',(-2.58182940328144,3.7543328293346,-6.98045157812523));
#120097=CARTESIAN_POINT('Ctrl Pts',(-2.57210657331077,3.75872286882143,
-6.95347381572861));
#120098=CARTESIAN_POINT('Ctrl Pts',(-2.56283493314422,3.76290918767733,
-6.92774796161051));
#120099=CARTESIAN_POINT('Ctrl Pts',(-2.55354613256455,3.76716275952044,
-6.90203912684389));
#120100=CARTESIAN_POINT('Ctrl Pts',(-2.5442393045101,3.77148708932044,-6.87634883570633));
#120101=CARTESIAN_POINT('Ctrl Pts',(-2.53493220283023,3.77581154625792,
-6.85065778926127));
#120102=CARTESIAN_POINT('Ctrl Pts',(-2.52560700440847,3.78020679562409,
-6.82498509510151));
#120103=CARTESIAN_POINT('Ctrl Pts',(-2.51626275052791,3.78467661289218,
-6.79933245031635));
#120104=CARTESIAN_POINT('Ctrl Pts',(-1.760641144,3.655724827,-7.032968275));
#120105=CARTESIAN_POINT('Ctrl Pts',(-2.041027504,3.703213228,-6.96277604));
#120106=CARTESIAN_POINT('Ctrl Pts',(-2.314936093,3.75,-6.870485491));
#120107=CARTESIAN_POINT('Ctrl Pts',(-2.418373138,3.76766825,-6.835633493));
#120108=CARTESIAN_POINT('Ctrl Pts',(-2.520714129,3.785449891,-6.79768345));
#120109=CARTESIAN_POINT('Ctrl Pts',(-2.058975735,3.655724827,-7.211838803));
#120110=CARTESIAN_POINT('Ctrl Pts',(-2.346493203,3.703213228,-7.129752735));
#120111=CARTESIAN_POINT('Ctrl Pts',(-2.62656342,3.75,-7.025038406));
#120112=CARTESIAN_POINT('Ctrl Pts',(-2.732327301,3.76766825,-6.98549477199999));
#120113=CARTESIAN_POINT('Ctrl Pts',(-2.836852838,3.785449891,-6.94278517400001));
#120114=CARTESIAN_POINT('Ctrl Pts',(-1.76064114857457,3.65572482777479,
-7.03296827385479));
#120115=CARTESIAN_POINT('Ctrl Pts',(-1.90496309768958,3.6801683085245,-6.99683855557638));
#120116=CARTESIAN_POINT('Ctrl Pts',(-2.04784877368294,3.70444731544377,
-6.95634327951747));
#120117=CARTESIAN_POINT('Ctrl Pts',(-2.18891771140563,3.72849592276323,
-6.91166689384207));
#120118=CARTESIAN_POINT('Ctrl Pts',(-2.23108923368116,3.73568507719821,
-6.89831121665249));
#120119=CARTESIAN_POINT('Ctrl Pts',(-2.27309858376271,3.74285366689624,
-6.88458218934028));
#120120=CARTESIAN_POINT('Ctrl Pts',(-2.31493609343746,3.75000000004083,
-6.8704854910179));
#120121=CARTESIAN_POINT('Ctrl Pts',(-2.3822825332196,3.76150355503787,-6.84779383358611));
#120122=CARTESIAN_POINT('Ctrl Pts',(-2.44940689466729,3.77306479265215,
-6.82407412937982));
#120123=CARTESIAN_POINT('Ctrl Pts',(-2.51626275101608,3.78467661239246,
-6.79933245062732));
#120124=CARTESIAN_POINT('Ctrl Pts',(-0.991157832000001,3.785444214,-7.181929139));
#120125=CARTESIAN_POINT('Ctrl Pts',(-1.379931276,3.720864611,-7.12827561));
#120126=CARTESIAN_POINT('Ctrl Pts',(-1.760641144,3.655724827,-7.032968275));
#120127=CARTESIAN_POINT('Ctrl Pts',(-0.781127895000001,3.785444214,-7.459211702));
#120128=CARTESIAN_POINT('Ctrl Pts',(-1.184911248,3.720864611,-7.41692755));
#120129=CARTESIAN_POINT('Ctrl Pts',(-1.581770616,3.655724827,-7.331302866));
#120130=CARTESIAN_POINT('',(-0.995778437273178,3.78467661247787,-7.18128994900401));
#120131=CARTESIAN_POINT('Origin',(0.0530096971896153,3.62501423314348,0.190603709598965));
#120132=CARTESIAN_POINT('Ctrl Pts',(-1.02821394493559,3.74576903859535,
-7.42918407887292));
#120133=CARTESIAN_POINT('Ctrl Pts',(-1.02453956940242,3.7500184674844,-7.40072275602811));
#120134=CARTESIAN_POINT('Ctrl Pts',(-1.02087691824179,3.75433282933031,
-7.37226950252932));
#120135=CARTESIAN_POINT('Ctrl Pts',(-1.01718082414336,3.75872286881798,
-7.34383234421332));
#120136=CARTESIAN_POINT('Ctrl Pts',(-1.01365624800282,3.76290918767842,
-7.31671481770127));
#120137=CARTESIAN_POINT('Ctrl Pts',(-1.01011125400241,3.76716275952209,
-7.28961022365669));
#120138=CARTESIAN_POINT('Ctrl Pts',(-1.00654466763215,3.77148708935972,
-7.26251986408723));
#120139=CARTESIAN_POINT('Ctrl Pts',(-1.00297797646616,3.77581154625761,
-7.23542870853134));
#120140=CARTESIAN_POINT('Ctrl Pts',(-0.999389666409323,3.78020679562356,
-7.20835158568946));
#120141=CARTESIAN_POINT('Ctrl Pts',(-0.995778436939607,3.78467661259395,
-7.18128994843103));
#120142=CARTESIAN_POINT('Ctrl Pts',(-0.207598047,3.655724827,-7.247027187));
#120143=CARTESIAN_POINT('Ctrl Pts',(-0.496518385,3.703213228,-7.238750787));
#120144=CARTESIAN_POINT('Ctrl Pts',(-0.783862884,3.75,-7.207500189));
#120145=CARTESIAN_POINT('Ctrl Pts',(-0.892373777000001,3.76766825,-7.19569891800001));
#120146=CARTESIAN_POINT('Ctrl Pts',(-1.00048023,3.785449891,-7.18063641400001));
#120147=CARTESIAN_POINT('Ctrl Pts',(-0.460505865,3.655724827,-7.48584894));
#120148=CARTESIAN_POINT('Ctrl Pts',(-0.758947412,3.703213228,-7.467489755));
#120149=CARTESIAN_POINT('Ctrl Pts',(-1.054980228,3.75,-7.425430406));
#120150=CARTESIAN_POINT('Ctrl Pts',(-1.166772121,3.76766825,-7.409547389));
#120151=CARTESIAN_POINT('Ctrl Pts',(-1.27803521,3.785449891,-7.390306218));
#120152=CARTESIAN_POINT('Ctrl Pts',(-0.207598052087366,3.65572482783619,
-7.24702718685427));
#120153=CARTESIAN_POINT('Ctrl Pts',(-0.356312633948643,3.68016830504614,
-7.2427671150157));
#120154=CARTESIAN_POINT('Ctrl Pts',(-0.504562987970137,3.70444730845298,
-7.23393479450269));
#120155=CARTESIAN_POINT('Ctrl Pts',(-0.651937893342154,3.72849591226242,
-7.2206285727237));
#120156=CARTESIAN_POINT('Ctrl Pts',(-0.695994566083915,3.73568507018081,
-7.21665077299676));
#120157=CARTESIAN_POINT('Ctrl Pts',(-0.73997311729786,3.74285366333655,
-7.21227348925494));
#120158=CARTESIAN_POINT('Ctrl Pts',(-0.783862883953297,3.74999999990936,
-7.20750018947045));
#120159=CARTESIAN_POINT('Ctrl Pts',(-0.854512836360514,3.76150355485184,
-7.19981654407829));
#120160=CARTESIAN_POINT('Ctrl Pts',(-0.92516690338793,3.77306479249498,
-7.19108114729756));
#120161=CARTESIAN_POINT('Ctrl Pts',(-0.995778437045702,3.78467661227579,
-7.18128994836432));
#120162=CARTESIAN_POINT('Ctrl Pts',(0.575917356,3.785444214,-7.227089262));
#120163=CARTESIAN_POINT('Ctrl Pts',(0.184699296,3.720864611,-7.258264921));
#120164=CARTESIAN_POINT('Ctrl Pts',(-0.207598047,3.655724827,-7.247027187));
#120165=CARTESIAN_POINT('Ctrl Pts',(0.840644464,3.785444214,-7.452738885));
#120166=CARTESIAN_POINT('Ctrl Pts',(0.437211499,3.720864611,-7.498244798));
#120167=CARTESIAN_POINT('Ctrl Pts',(0.031223706,3.655724827,-7.499935005));
#120168=CARTESIAN_POINT('',(0.571267371189336,3.78467661250746,-7.22745830975374));
#120169=CARTESIAN_POINT('Origin',(0.0107961935969751,3.62501419796389,0.197543322221929));
#120170=CARTESIAN_POINT('Ctrl Pts',(0.592880097666729,3.74576903859534,
-7.47652948817413));
#120171=CARTESIAN_POINT('Ctrl Pts',(0.590350225508585,3.75001846753542,
-7.44794369301283));
#120172=CARTESIAN_POINT('Ctrl Pts',(0.587810637439167,3.75433282936884,
-7.4193682990325));
#120173=CARTESIAN_POINT('Ctrl Pts',(0.585307170438767,3.75872286884618,
-7.39080143468898));
#120174=CARTESIAN_POINT('Ctrl Pts',(0.582919877304075,3.76290918770063,
-7.36356022115747));
#120175=CARTESIAN_POINT('Ctrl Pts',(0.580555304784233,3.7671627595402,-7.336327248497));
#120176=CARTESIAN_POINT('Ctrl Pts',(0.578214879801036,3.77148708937742,
-7.30910353575974));
#120177=CARTESIAN_POINT('Ctrl Pts',(0.575874386056288,3.77581154626321,
-7.28187902319138));
#120178=CARTESIAN_POINT('Ctrl Pts',(0.573558022377638,3.78020679562105,
-7.2546635678004));
#120179=CARTESIAN_POINT('Ctrl Pts',(0.571267371386615,3.7846766125698,-7.22745830916289));
#120180=CARTESIAN_POINT('Ctrl Pts',(1.355152105,3.655724827,-7.122223162));
#120181=CARTESIAN_POINT('Ctrl Pts',(1.071207382,3.703213228,-7.176249592));
#120182=CARTESIAN_POINT('Ctrl Pts',(0.783862884,3.75,-7.207500189));
#120183=CARTESIAN_POINT('Ctrl Pts',(0.67535199,3.76766825,-7.21930146));
#120184=CARTESIAN_POINT('Ctrl Pts',(0.566535013,3.785449891,-7.22783080000001));
#120185=CARTESIAN_POINT('Ctrl Pts',(1.159496749,3.655724827,-7.4098291));
#120186=CARTESIAN_POINT('Ctrl Pts',(0.864085917,3.703213228,-7.456055254));
#120187=CARTESIAN_POINT('Ctrl Pts',(0.565932667,3.75,-7.478617534));
#120188=CARTESIAN_POINT('Ctrl Pts',(0.453340027,3.76766825,-7.487137805));
#120189=CARTESIAN_POINT('Ctrl Pts',(0.340541924,3.785449891,-7.492264758));
#120190=CARTESIAN_POINT('Ctrl Pts',(1.3551521000723,3.65572482782414,-7.1222231629376));
#120191=CARTESIAN_POINT('Ctrl Pts',(1.20899854655521,3.68016831274631,-7.15003193717776));
#120192=CARTESIAN_POINT('Ctrl Pts',(1.06231546936486,3.70444732374593,-7.17327556105714));
#120193=CARTESIAN_POINT('Ctrl Pts',(0.915525617098543,3.72849593500173,
-7.19196168252318));
#120194=CARTESIAN_POINT('Ctrl Pts',(0.871643901735247,3.73568508532593,
-7.19754775711046));
#120195=CARTESIAN_POINT('Ctrl Pts',(0.827752604260194,3.7428536709306,-7.20272689443133));
#120196=CARTESIAN_POINT('Ctrl Pts',(0.78386288387654,3.75000000000168,-7.20750018914185));
#120197=CARTESIAN_POINT('Ctrl Pts',(0.71321293074891,3.76150355496809,-7.21518383469371));
#120198=CARTESIAN_POINT('Ctrl Pts',(0.642332865126122,3.77306479247657,
-7.22184120228829));
#120199=CARTESIAN_POINT('Ctrl Pts',(0.571267371253685,3.78467661219437,
-7.2274583091124));
#120200=CARTESIAN_POINT('Ctrl Pts',(2.116063288,3.785444214,-6.93431872400001));
#120201=CARTESIAN_POINT('Ctrl Pts',(1.740693535,3.720864611,-7.048865831));
#120202=CARTESIAN_POINT('Ctrl Pts',(1.355152105,3.655724827,-7.122223162));
#120203=CARTESIAN_POINT('Ctrl Pts',(2.423109222,3.785444214,-7.097784281));
#120204=CARTESIAN_POINT('Ctrl Pts',(2.038890722,3.720864611,-7.228952453));
#120205=CARTESIAN_POINT('Ctrl Pts',(1.642758043,3.655724827,-7.31787851900001));
#120206=CARTESIAN_POINT('',(2.11160135187181,3.78467661255684,-6.93567875264863));
#120207=CARTESIAN_POINT('Origin',(-0.0319222393415766,3.62501423866122,
0.195245911636008));
#120208=CARTESIAN_POINT('Ctrl Pts',(2.18625172552362,3.74576903864184,-7.17428068773664));
#120209=CARTESIAN_POINT('Ctrl Pts',(2.17763589926571,3.75001846753479,-7.14690706044628));
#120210=CARTESIAN_POINT('Ctrl Pts',(2.16901282041789,3.75433282937659,-7.11954567964758));
#120211=CARTESIAN_POINT('Ctrl Pts',(2.16042685174653,3.75872286886273,-7.09218486411846));
#120212=CARTESIAN_POINT('Ctrl Pts',(2.15223931659581,3.76290918772571,-7.06609373247429));
#120213=CARTESIAN_POINT('Ctrl Pts',(2.14407574238575,3.76716275957337,-7.04000576478655));
#120214=CARTESIAN_POINT('Ctrl Pts',(2.13593774173399,3.7714870894253,-7.01392164950441));
#120215=CARTESIAN_POINT('Ctrl Pts',(2.12779950200521,3.77581154631678,-6.98783676792682));
#120216=CARTESIAN_POINT('Ctrl Pts',(2.11968677518882,3.78020679568715,-6.96175554450415));
#120217=CARTESIAN_POINT('Ctrl Pts',(2.11160135209104,3.78467661264949,-6.93567875210078));
#120218=CARTESIAN_POINT('Ctrl Pts',(2.85453685,3.655724827,-6.664391898));
#120219=CARTESIAN_POINT('Ctrl Pts',(2.588844683,3.703213228,-6.778194942));
#120220=CARTESIAN_POINT('Ctrl Pts',(2.314936093,3.75,-6.870485491));
#120221=CARTESIAN_POINT('Ctrl Pts',(2.211499049,3.76766825,-6.905337489));
#120222=CARTESIAN_POINT('Ctrl Pts',(2.107059708,3.785449891,-6.937059852));
#120223=CARTESIAN_POINT('Ctrl Pts',(2.725282582,3.655724827,-6.987333887));
#120224=CARTESIAN_POINT('Ctrl Pts',(2.446715548,3.703213228,-7.095983895));
#120225=CARTESIAN_POINT('Ctrl Pts',(2.160383179,3.75,-7.182112817));
#120226=CARTESIAN_POINT('Ctrl Pts',(2.052254499,3.76766825,-7.21463797899999));
#120227=CARTESIAN_POINT('Ctrl Pts',(1.943195696,3.785449891,-7.243893324));
#120228=CARTESIAN_POINT('Ctrl Pts',(2.85453684561659,3.65572482778347,-6.66439189987753));
#120229=CARTESIAN_POINT('Ctrl Pts',(2.71777836705026,3.68016830890369,-6.72296920496374));
#120230=CARTESIAN_POINT('Ctrl Pts',(2.57952137248556,3.70444731614839,-6.77720192375549));
#120231=CARTESIAN_POINT('Ctrl Pts',(2.44018037091755,3.72849592370944,-6.82700664690812));
#120232=CARTESIAN_POINT('Ctrl Pts',(2.39852540482211,3.73568507780856,-6.84189540205534));
#120233=CARTESIAN_POINT('Ctrl Pts',(2.35677360102747,3.7428536671656,-6.85638879336383));
#120234=CARTESIAN_POINT('Ctrl Pts',(2.31493609318094,3.74999999996342,-6.87048549099486));
#120235=CARTESIAN_POINT('Ctrl Pts',(2.24758965425263,3.76150355491197,-6.89317714831988));
#120236=CARTESIAN_POINT('Ctrl Pts',(2.17979786166445,3.77306479259842,-6.91491598961235));
#120237=CARTESIAN_POINT('Ctrl Pts',(2.11160135195229,3.78467661222486,-6.93567875207102));
#120238=CARTESIAN_POINT('Ctrl Pts',(3.557264453,3.785444214,-6.317307149));
#120239=CARTESIAN_POINT('Ctrl Pts',(3.215294878,3.720864611,-6.50986961));
#120240=CARTESIAN_POINT('Ctrl Pts',(2.85453685,3.655724827,-6.664391898));
#120241=CARTESIAN_POINT('Ctrl Pts',(3.892272087,3.785444214,-6.410945172));
#120242=CARTESIAN_POINT('Ctrl Pts',(3.545233681,3.720864611,-6.621642326));
#120243=CARTESIAN_POINT('Ctrl Pts',(3.177478839,3.655724827,-6.79364616600001));
#120244=CARTESIAN_POINT('',(3.5531991999166,3.78467661247843,-6.31959456523331));
#120245=CARTESIAN_POINT('Origin',(-0.0731479704522126,3.62501422279194,
0.183818735359169));
#120246=CARTESIAN_POINT('Ctrl Pts',(3.67739665301007,3.74576903856647,-6.53657049633276));
#120247=CARTESIAN_POINT('Ctrl Pts',(3.66309773951716,3.7500184675244,-6.51168899697415));
#120248=CARTESIAN_POINT('Ctrl Pts',(3.64879437539399,3.75433282937531,-6.48682101708142));
#120249=CARTESIAN_POINT('Ctrl Pts',(3.63452737529612,3.75872286886363,-6.46194561166964));
#120250=CARTESIAN_POINT('Ctrl Pts',(3.620922438067,3.76290918772969,-6.43822455420455));
#120251=CARTESIAN_POINT('Ctrl Pts',(3.6073415817108,3.76716275957753,-6.41450143583751));
#120252=CARTESIAN_POINT('Ctrl Pts',(3.59378652917745,3.77148708941549,-6.39077658231892));
#120253=CARTESIAN_POINT('Ctrl Pts',(3.58023107836183,3.77581154631337,-6.36705103170317));
#120254=CARTESIAN_POINT('Ctrl Pts',(3.56670133038181,3.78020679567546,-6.34332356926532));
#120255=CARTESIAN_POINT('Ctrl Pts',(3.55319919983689,3.78467661264265,-6.31959456457597));
#120256=CARTESIAN_POINT('Ctrl Pts',(4.220446625,3.655724827,-5.894941076));
#120257=CARTESIAN_POINT('Ctrl Pts',(3.985430483,3.703213228,-6.06319943));
#120258=CARTESIAN_POINT('Ctrl Pts',(3.737765465,3.75,-6.212214527));
#120259=CARTESIAN_POINT('Ctrl Pts',(3.64423887,3.76766825,-6.268487612));
#120260=CARTESIAN_POINT('Ctrl Pts',(3.549060633,3.785449891,-6.321919694));
#120261=CARTESIAN_POINT('Ctrl Pts',(4.163637232,3.655724827,-6.238118707));
#120262=CARTESIAN_POINT('Ctrl Pts',(3.91493948,3.703213228,-6.404112217));
#120263=CARTESIAN_POINT('Ctrl Pts',(3.653816575,3.75,-6.549780488));
#120264=CARTESIAN_POINT('Ctrl Pts',(3.555207832,3.76766825,-6.60478969900001));
#120265=CARTESIAN_POINT('Ctrl Pts',(3.454987798,3.785449891,-6.656805489));
#120266=CARTESIAN_POINT('Ctrl Pts',(4.22044662086179,3.65572482783619,-5.89494107896272));
#120267=CARTESIAN_POINT('Ctrl Pts',(4.09947783216379,3.68016831624432,-5.98154793527608));
#120268=CARTESIAN_POINT('Ctrl Pts',(3.97611160334085,3.70444733067044,-6.06423391356302));
#120269=CARTESIAN_POINT('Ctrl Pts',(3.85073482196067,3.7284959452959,-6.14282844728115));
#120270=CARTESIAN_POINT('Ctrl Pts',(3.81325440525329,3.7356850921816,-6.16632367376766));
#120271=CARTESIAN_POINT('Ctrl Pts',(3.77559442370857,3.74285367436812,-6.18945359777217));
#120272=CARTESIAN_POINT('Ctrl Pts',(3.73776546476096,3.75000000004461,-6.21221452715368));
#120273=CARTESIAN_POINT('Ctrl Pts',(3.67687158297574,3.76150355501617,-6.24885316009497));
#120274=CARTESIAN_POINT('Ctrl Pts',(3.61533793358737,3.77306479254825,-6.28465699023988));
#120275=CARTESIAN_POINT('Ctrl Pts',(3.55319919971644,3.78467661230877,-6.31959456458162));
#120276=CARTESIAN_POINT('Ctrl Pts',(4.83213188600001,3.785444214,-5.404905313));
#120277=CARTESIAN_POINT('Ctrl Pts',(4.539552606,3.720864611,-5.66647912100001));
#120278=CARTESIAN_POINT('Ctrl Pts',(4.220446625,3.655724827,-5.894941076));
#120279=CARTESIAN_POINT('Ctrl Pts',(5.179436634,3.785444214,-5.424337393));
#120280=CARTESIAN_POINT('Ctrl Pts',(4.885805454,3.720864611,-5.704711563));
#120281=CARTESIAN_POINT('Ctrl Pts',(4.563624257,3.655724827,-5.951750469));
#120282=CARTESIAN_POINT('',(4.82865340266755,3.78467661231159,-5.40801315903628));
#120283=CARTESIAN_POINT('Origin',(-0.110953360283951,3.62501423096888,0.163796429963448));
#120284=CARTESIAN_POINT('Ctrl Pts',(4.99659059962423,3.74576903861156,-5.5932175331691));
#120285=CARTESIAN_POINT('Ctrl Pts',(4.97727719960564,3.75001846750351,-5.57199159346776));
#120286=CARTESIAN_POINT('Ctrl Pts',(4.95796235959718,3.75433282936886,-5.55077981355134));
#120287=CARTESIAN_POINT('Ctrl Pts',(4.93868143718509,3.75872286886735,-5.52955296453581));
#120288=CARTESIAN_POINT('Ctrl Pts',(4.92029524972338,3.76290918773003,-5.50931115157272));
#120289=CARTESIAN_POINT('Ctrl Pts',(4.90193213712422,3.76716275957218,-5.48906214921159));
#120290=CARTESIAN_POINT('Ctrl Pts',(4.88359385225733,3.77148708938566,-5.46880590528075));
#120291=CARTESIAN_POINT('Ctrl Pts',(4.86525502831547,3.77581154631779,-5.44854906589434));
#120292=CARTESIAN_POINT('Ctrl Pts',(4.84694089549697,3.78020679569389,-5.4282848341132));
#120293=CARTESIAN_POINT('Ctrl Pts',(4.82865340282906,3.78467661285823,-5.4080131584029));
#120294=CARTESIAN_POINT('Ctrl Pts',(5.389013006,3.655724827,-4.84984936));
#120295=CARTESIAN_POINT('Ctrl Pts',(5.195661984,3.703213228,-5.06469545100001));
#120296=CARTESIAN_POINT('Ctrl Pts',(4.985821077,3.75,-5.263467316));
#120297=CARTESIAN_POINT('Ctrl Pts',(4.906578131,3.76766825,-5.338530221));
#120298=CARTESIAN_POINT('Ctrl Pts',(4.825111428,3.785449891,-5.411173598));
#120299=CARTESIAN_POINT('Ctrl Pts',(5.407304832,3.655724827,-5.19721603));
#120300=CARTESIAN_POINT('Ctrl Pts',(5.200105193,3.703213228,-5.412791369));
#120301=CARTESIAN_POINT('Ctrl Pts',(4.976401568,3.75,-5.611187702));
#120302=CARTESIAN_POINT('Ctrl Pts',(4.891923597,3.76766825,-5.686108794));
#120303=CARTESIAN_POINT('Ctrl Pts',(4.805228509,3.785449891,-5.75845282800001));
#120304=CARTESIAN_POINT('Ctrl Pts',(5.38901300259543,3.65572482783619,-4.84984936378305));
#120305=CARTESIAN_POINT('Ctrl Pts',(5.2894903402649,3.68016830914952,-4.96043608174435));
#120306=CARTESIAN_POINT('Ctrl Pts',(5.18678341734772,3.70444731657778,-5.06770897050535));
#120307=CARTESIAN_POINT('Ctrl Pts',(5.08123340919572,3.72849592434171,-5.17141828174666));
#120308=CARTESIAN_POINT('Ctrl Pts',(5.04968001283305,3.73568507824166,-5.20242141534551));
#120309=CARTESIAN_POINT('Ctrl Pts',(5.01787272000543,3.74285366740273,-5.23310638753778));
#120310=CARTESIAN_POINT('Ctrl Pts',(4.98582107694877,3.75000000000868,-5.26346731649106));
#120311=CARTESIAN_POINT('Ctrl Pts',(4.93422708289128,3.76150355498014,-5.31233974326661));
#120312=CARTESIAN_POINT('Ctrl Pts',(4.88182882144562,3.77306479250486,-5.36053441520924));
#120313=CARTESIAN_POINT('Ctrl Pts',(4.82865340234207,3.78467661251199,-5.40801315826926));
#120314=CARTESIAN_POINT('Ctrl Pts',(5.881054202,3.785444214,-4.239776111));
#120315=CARTESIAN_POINT('Ctrl Pts',(5.6515459,3.720864611,-4.558130366));
#120316=CARTESIAN_POINT('Ctrl Pts',(5.389013006,3.655724827,-4.84984936));
#120317=CARTESIAN_POINT('Ctrl Pts',(6.224416481,3.785444214,-4.184093626));
#120318=CARTESIAN_POINT('Ctrl Pts',(5.997922393,3.720864611,-4.521034827));
#120319=CARTESIAN_POINT('Ctrl Pts',(5.736379676,3.655724827,-4.831557535));
#120320=CARTESIAN_POINT('',(5.87832514029295,3.7846766124525,-4.24355907006547));
#120321=CARTESIAN_POINT('Origin',(-0.143570501109366,3.62501422270825,0.136115116627182));
#120322=CARTESIAN_POINT('Ctrl Pts',(6.08214952361695,3.74576903857924,-4.38833193459805));
#120323=CARTESIAN_POINT('Ctrl Pts',(6.05872471075178,3.75001846754309,-4.37175405532135));
#120324=CARTESIAN_POINT('Ctrl Pts',(6.03530153526747,3.75433282939705,-4.35519031474441));
#120325=CARTESIAN_POINT('Ctrl Pts',(6.01190824498433,3.75872286888058,-4.33860456609077));
#120326=CARTESIAN_POINT('Ctrl Pts',(5.98960052494431,3.76290918771721,-4.32278848237012));
#120327=CARTESIAN_POINT('Ctrl Pts',(5.96731379477278,3.76716275953038,-4.30696041691506));
#120328=CARTESIAN_POINT('Ctrl Pts',(5.94504975494914,3.77148708934424,-4.29111994183739));
#120329=CARTESIAN_POINT('Ctrl Pts',(5.92278506103885,3.77581154620093,-4.2752790013885));
#120330=CARTESIAN_POINT('Ctrl Pts',(5.90054289164115,3.78020679553293,-4.25942553337721));
#120331=CARTESIAN_POINT('Ctrl Pts',(5.87832513993511,3.78467661242694,-4.24355906945344));
#120332=CARTESIAN_POINT('Ctrl Pts',(6.305595129,3.655724827,-3.577984079));
#120333=CARTESIAN_POINT('Ctrl Pts',(6.162950104,3.703213228,-3.829371942));
#120334=CARTESIAN_POINT('Ctrl Pts',(6.000745237,3.75,-4.068606224));
#120335=CARTESIAN_POINT('Ctrl Pts',(5.939491253,3.76766825,-4.158949091));
#120336=CARTESIAN_POINT('Ctrl Pts',(5.875545374,3.785449891,-4.247407039));
#120337=CARTESIAN_POINT('Ctrl Pts',(6.398132867,3.655724827,-3.913297307));
#120338=CARTESIAN_POINT('Ctrl Pts',(6.242119767,3.703213228,-4.168374412));
#120339=CARTESIAN_POINT('Ctrl Pts',(6.066295556,3.75,-4.410222016));
#120340=CARTESIAN_POINT('Ctrl Pts',(5.99989845300001,3.76766825,-4.501551761));
#120341=CARTESIAN_POINT('Ctrl Pts',(5.930782076,3.785449891,-4.590841313));
#120342=CARTESIAN_POINT('Ctrl Pts',(6.30559512632834,3.65572482788943,-3.57798408370835));
#120343=CARTESIAN_POINT('Ctrl Pts',(6.23217209691088,3.68016831800515,-3.70737982273348));
#120344=CARTESIAN_POINT('Ctrl Pts',(6.15492687539684,3.70444733414286,-3.83422372830123));
#120345=CARTESIAN_POINT('Ctrl Pts',(6.07413897226622,3.72849595049746,-3.95819854833682));
#120346=CARTESIAN_POINT('Ctrl Pts',(6.04998806253253,3.73568509565773,-3.99525984801047));
#120347=CARTESIAN_POINT('Ctrl Pts',(6.0255207977836,3.74285367613321,-4.03206500559797));
#120348=CARTESIAN_POINT('Ctrl Pts',(6.00074523661453,3.75000000011495,-4.06860622465582));
#120349=CARTESIAN_POINT('Ctrl Pts',(5.9608636085474,3.76150355512892,-4.12742722500174));
#120350=CARTESIAN_POINT('Ctrl Pts',(5.92005081953396,3.77306479251279,-4.18575920929946));
#120351=CARTESIAN_POINT('Ctrl Pts',(5.87832513980401,3.78467661209925,-4.2435590695447));
#120352=CARTESIAN_POINT('Ctrl Pts',(6.65498496000001,3.785444214,-2.876399691));
#120353=CARTESIAN_POINT('Ctrl Pts',(6.499279189,3.720864611,-3.236648501));
#120354=CARTESIAN_POINT('Ctrl Pts',(6.305595129,3.655724827,-3.577984079));
#120355=CARTESIAN_POINT('Ctrl Pts',(6.978349531,3.785444214,-2.748206291));
#120356=CARTESIAN_POINT('Ctrl Pts',(6.829583148,3.720864611,-3.125959528));
#120357=CARTESIAN_POINT('Ctrl Pts',(6.640908357,3.655724827,-3.485446341));
#120358=CARTESIAN_POINT('',(6.65313292495336,3.78467661232429,-2.88068087308594));
#120359=CARTESIAN_POINT('Origin',(-0.169474684097664,3.62501422942962,0.102069408652304));
#120360=CARTESIAN_POINT('Ctrl Pts',(6.8833138953662,3.74576903858391,-2.97825281206827));
#120361=CARTESIAN_POINT('Ctrl Pts',(6.85687298764022,3.75001846751913,-2.96709815684438));
#120362=CARTESIAN_POINT('Ctrl Pts',(6.83043671842893,3.75433282937008,-2.95595695765276));
#120363=CARTESIAN_POINT('Ctrl Pts',(6.80402490463526,3.75872286884989,-2.9447878404987));
#120364=CARTESIAN_POINT('Ctrl Pts',(6.7788387361469,3.76290918770224,-2.93413702837705));
#120365=CARTESIAN_POINT('Ctrl Pts',(6.75367049107894,3.76716275953069,-2.92347000246075));
#120366=CARTESIAN_POINT('Ctrl Pts',(6.72852173843565,3.77148708931287,-2.9127859794265));
#120367=CARTESIAN_POINT('Ctrl Pts',(6.70337224640891,3.77581154623209,-2.90210164227767));
#120368=CARTESIAN_POINT('Ctrl Pts',(6.67824205949415,3.78020679557677,-2.89140022848748));
#120369=CARTESIAN_POINT('Ctrl Pts',(6.65313292455553,3.78467661284088,-2.88068087237092));
#120370=CARTESIAN_POINT('Ctrl Pts',(6.927334631,3.655724827,-2.138816239));
#120371=CARTESIAN_POINT('Ctrl Pts',(6.842065528,3.703213228,-2.414991257));
#120372=CARTESIAN_POINT('Ctrl Pts',(6.735081219,3.75,-2.683501626));
#120373=CARTESIAN_POINT('Ctrl Pts',(6.69468036500001,3.76766825,-2.784900123));
#120374=CARTESIAN_POINT('Ctrl Pts',(6.651245349,3.785449891,-2.885036447));
#120375=CARTESIAN_POINT('Ctrl Pts',(7.089791321,3.655724827,-2.446397152));
#120376=CARTESIAN_POINT('Ctrl Pts',(6.992259758,3.703213228,-2.7290489));
#120377=CARTESIAN_POINT('Ctrl Pts',(6.872536305,3.75,-3.00303925));
#120378=CARTESIAN_POINT('Ctrl Pts',(6.827324725,3.76766825,-3.106507171));
#120379=CARTESIAN_POINT('Ctrl Pts',(6.779018865,3.785449891,-3.208567161));
#120380=CARTESIAN_POINT('Ctrl Pts',(6.92733462964675,3.65572482775366,-2.138816243383));
#120381=CARTESIAN_POINT('Ctrl Pts',(6.88344445138572,3.68016831674824,-2.28097055623012));
#120382=CARTESIAN_POINT('Ctrl Pts',(6.83527287313895,3.70444733170435,-2.42145435399876));
#120383=CARTESIAN_POINT('Ctrl Pts',(6.78302467103386,3.72849594680057,-2.55989771550699));
#120384=CARTESIAN_POINT('Ctrl Pts',(6.76740547750231,3.73568509318686,-2.60128428134912));
#120385=CARTESIAN_POINT('Ctrl Pts',(6.75142226205709,3.74285367487235,-2.64248870044474));
#120386=CARTESIAN_POINT('Ctrl Pts',(6.73508121889342,3.75000000004661,-2.68350162626749));
#120387=CARTESIAN_POINT('Ctrl Pts',(6.70877677764511,3.76150355499729,-2.74952079523594));
#120388=CARTESIAN_POINT('Ctrl Pts',(6.68145782078675,3.77306479247725,-2.81526255334838));
#120389=CARTESIAN_POINT('Ctrl Pts',(6.65313292417658,3.7846766123365,-2.88068087229939));
#120390=CARTESIAN_POINT('Ctrl Pts',(7.117736018,3.785444214,-1.378526018));
#120391=CARTESIAN_POINT('Ctrl Pts',(7.043113406,3.720864611,-1.763824549));
#120392=CARTESIAN_POINT('Ctrl Pts',(6.927334631,3.655724827,-2.138816239));
#120393=CARTESIAN_POINT('Ctrl Pts',(7.405982713,3.785444214,-1.183815884));
#120394=CARTESIAN_POINT('Ctrl Pts',(7.341900185,3.720864611,-1.584717836));
#120395=CARTESIAN_POINT('Ctrl Pts',(7.234915544,3.655724827,-1.976359549));
#120396=CARTESIAN_POINT('',(7.11684761125436,3.78467661242663,-1.38310524218956));
#120397=CARTESIAN_POINT('Origin',(-0.187454685946141,3.62501420012553,0.0632511407711575));
#120398=CARTESIAN_POINT('Ctrl Pts',(7.3626221596976,3.74576903850582,-1.42891389841415));
#120399=CARTESIAN_POINT('Ctrl Pts',(7.33440150456421,3.75001846745712,-1.42370404627908));
#120400=CARTESIAN_POINT('Ctrl Pts',(7.30618827216532,3.75433282931056,-1.41850633850769));
#120401=CARTESIAN_POINT('Ctrl Pts',(7.27799292189132,3.75872286879844,-1.41327610827669));
#120402=CARTESIAN_POINT('Ctrl Pts',(7.25110598229676,3.76290918765531,-1.40828858789053));
#120403=CARTESIAN_POINT('Ctrl Pts',(7.22423306159013,3.76716275949081,-1.4032813797772));
#120404=CARTESIAN_POINT('Ctrl Pts',(7.19737552341408,3.77148708932007,-1.39825338164923));
#120405=CARTESIAN_POINT('Ctrl Pts',(7.17051719618115,3.77581154619532,-1.39322523580198));
#120406=CARTESIAN_POINT('Ctrl Pts',(7.14367405144934,3.78020679553876,-1.38817626253347));
#120407=CARTESIAN_POINT('Ctrl Pts',(7.1168476107115,3.78467661246488,-1.38310524176854));
#120408=CARTESIAN_POINT('Ctrl Pts',(7.225159666,3.655724827,-0.599639729));
#120409=CARTESIAN_POINT('Ctrl Pts',(7.201253572,3.703213228,-0.887688265));
#120410=CARTESIAN_POINT('Ctrl Pts',(7.154492288,3.75,-1.172919475));
#120411=CARTESIAN_POINT('Ctrl Pts',(7.136833664,3.76766825,-1.28063232));
#120412=CARTESIAN_POINT('Ctrl Pts',(7.11594048400001,3.785449891,-1.387764758));
#120413=CARTESIAN_POINT('Ctrl Pts',(7.449939012,3.655724827,-0.865106183999999));
#120414=CARTESIAN_POINT('Ctrl Pts',(7.41544945400001,3.703213228,-1.162116095));
#120415=CARTESIAN_POINT('Ctrl Pts',(7.357424895,3.75,-1.455437707));
#120416=CARTESIAN_POINT('Ctrl Pts',(7.335512881,3.76766825,-1.566205758));
#120417=CARTESIAN_POINT('Ctrl Pts',(7.310276266,3.785449891,-1.676263974));
#120418=CARTESIAN_POINT('Ctrl Pts',(7.22515966557906,3.65572482783619,-0.599639734072013));
#120419=CARTESIAN_POINT('Ctrl Pts',(7.2128545925476,3.68016831230712,-0.74790562150211));
#120420=CARTESIAN_POINT('Ctrl Pts',(7.19600910650006,3.70444732281126,-0.895460424408708));
#120421=CARTESIAN_POINT('Ctrl Pts',(7.17474367395376,3.72849593352359,-1.04189884946702));
#120422=CARTESIAN_POINT('Ctrl Pts',(7.16838653326402,3.73568508433717,-1.08567551229546));
#120423=CARTESIAN_POINT('Ctrl Pts',(7.16163472464087,3.7428536704232,-1.12935254070576));
#120424=CARTESIAN_POINT('Ctrl Pts',(7.15449228824709,3.74999999996714,-1.17291947509793));
#120425=CARTESIAN_POINT('Ctrl Pts',(7.14299500075388,3.76150355489508,-1.24304982931552));
#120426=CARTESIAN_POINT('Ctrl Pts',(7.13044728075292,3.7730647925216,-1.31312735085109));
#120427=CARTESIAN_POINT('Ctrl Pts',(7.11684761062354,3.78467661208736,-1.38310524190111));
#120428=CARTESIAN_POINT('Ctrl Pts',(7.24766965,3.785444214,0.183805999));
#120429=CARTESIAN_POINT('Ctrl Pts',(7.257619468,3.720864611,-0.208526122));
#120430=CARTESIAN_POINT('Ctrl Pts',(7.225159666,3.655724827,-0.599639729));
#120431=CARTESIAN_POINT('Ctrl Pts',(7.487320375,3.785444214,0.435928437));
#120432=CARTESIAN_POINT('Ctrl Pts',(7.510918129,3.720864611,0.030623501));
#120433=CARTESIAN_POINT('Ctrl Pts',(7.490626122,3.655724827,-0.374860382));
#120434=CARTESIAN_POINT('',(7.24778641184,3.78467661246146,0.179142853532766));
#120435=CARTESIAN_POINT('Origin',(-0.196669441527031,3.62501419190378,0.0214751493333531));
#120436=CARTESIAN_POINT('Ctrl Pts',(7.49766239486428,3.74576903859026,0.187239441344393));
#120437=CARTESIAN_POINT('Ctrl Pts',(7.46898155867307,3.75001846754567,0.186260883320056));
#120438=CARTESIAN_POINT('Ctrl Pts',(7.44031058236322,3.75433282937421,0.185272060355488));
#120439=CARTESIAN_POINT('Ctrl Pts',(7.41165007873406,3.75872286885703,0.184318843757048));
#120440=CARTESIAN_POINT('Ctrl Pts',(7.38431957143929,3.76290918769016,0.18340986136322));
#120441=CARTESIAN_POINT('Ctrl Pts',(7.35699852299701,3.76716275951432,0.182523120145202));
#120442=CARTESIAN_POINT('Ctrl Pts',(7.32968802821128,3.77148708934581,0.18165998977544));
#120443=CARTESIAN_POINT('Ctrl Pts',(7.30237673105925,3.77581154622358,0.180796834047416));
#120444=CARTESIAN_POINT('Ctrl Pts',(7.27507578416942,3.78020679558335,0.179957282699222));
#120445=CARTESIAN_POINT('Ctrl Pts',(7.24778641118233,3.78467661245961,0.179142853867999));
#120446=CARTESIAN_POINT('Ctrl Pts',(7.185144264,3.655724827,0.967575269));
#120447=CARTESIAN_POINT('Ctrl Pts',(7.223719002,3.703213228,0.681122044));
#120448=CARTESIAN_POINT('Ctrl Pts',(7.23936725,3.75,0.392507087));
#120449=CARTESIAN_POINT('Ctrl Pts',(7.245276552,3.76766825,0.283516426));
#120450=CARTESIAN_POINT('Ctrl Pts',(7.247902151,3.785449891,0.17439727));
#120451=CARTESIAN_POINT('Ctrl Pts',(7.461735836,3.655724827,0.756636186000001));
#120452=CARTESIAN_POINT('Ctrl Pts',(7.491900975,3.703213228,0.459155966));
#120453=CARTESIAN_POINT('Ctrl Pts',(7.498288474,3.75,0.160218487));
#120454=CARTESIAN_POINT('Ctrl Pts',(7.500700607,3.76766825,0.047329695));
#120455=CARTESIAN_POINT('Ctrl Pts',(7.49971327400001,3.785449891,-0.065580547));
#120456=CARTESIAN_POINT('Ctrl Pts',(7.18514426467923,3.65572482783619,0.967575263956075));
#120457=CARTESIAN_POINT('Ctrl Pts',(7.20499965519742,3.68016830563138,0.820130563806539));
#120458=CARTESIAN_POINT('Ctrl Pts',(7.220267925519,3.70444730961,0.672404268532776));
#120459=CARTESIAN_POINT('Ctrl Pts',(7.23097959932907,3.72849591398212,0.524818092604028));
#120460=CARTESIAN_POINT('Ctrl Pts',(7.23418177719071,3.7356850713341,0.480698266550486));
#120461=CARTESIAN_POINT('Ctrl Pts',(7.23697709503498,3.74285366392681,0.436590903575513));
#120462=CARTESIAN_POINT('Ctrl Pts',(7.23936725006134,3.7499999999406,0.392507087293556));
#120463=CARTESIAN_POINT('Ctrl Pts',(7.24321471544561,3.76150355488793,0.321544764621282));
#120464=CARTESIAN_POINT('Ctrl Pts',(7.24602495025561,3.77306479248825,0.250408227808213));
#120465=CARTESIAN_POINT('Ctrl Pts',(7.24778641115059,3.78467661224106,0.179142853732049));
#120466=CARTESIAN_POINT('Ctrl Pts',(7.038710305,3.785444214,1.737543452));
#120467=CARTESIAN_POINT('Ctrl Pts',(7.132767311,3.720864611,1.356522755));
#120468=CARTESIAN_POINT('Ctrl Pts',(7.18514426400001,3.655724827,0.967575269));
#120469=CARTESIAN_POINT('Ctrl Pts',(7.21855925700001,3.785444214,2.03528923));
#120470=CARTESIAN_POINT('Ctrl Pts',(7.32873389,3.720864611,1.644532917));
#120471=CARTESIAN_POINT('Ctrl Pts',(7.396083347,3.655724827,1.24416684));
#120472=CARTESIAN_POINT('',(7.03982677465566,3.78467661254277,1.73301442877743));
#120473=CARTESIAN_POINT('Origin',(-0.196687510874572,3.6250142158557,-0.0213049642278113));
#120474=CARTESIAN_POINT('Ctrl Pts',(7.2821202695864,3.7457690385624,1.7946376730135));
#120475=CARTESIAN_POINT('Ctrl Pts',(7.25432033648699,3.7500184675284,1.78751646127483));
#120476=CARTESIAN_POINT('Ctrl Pts',(7.22653223946043,3.75433282935617,1.78038734412676));
#120477=CARTESIAN_POINT('Ctrl Pts',(7.19874671596483,3.75872286883388,1.7732952521629));
#120478=CARTESIAN_POINT('Ctrl Pts',(7.17225058499085,3.76290918769164,1.76653227008039));
#120479=CARTESIAN_POINT('Ctrl Pts',(7.14575891054067,3.76716275953878,1.75979304253155));
#120480=CARTESIAN_POINT('Ctrl Pts',(7.11927246741103,3.77148708938777,1.75307914252952));
#120481=CARTESIAN_POINT('Ctrl Pts',(7.09278524606327,3.77581154629315,1.74636504526135));
#120482=CARTESIAN_POINT('Ctrl Pts',(7.06630305878795,3.7802067956747,1.73967622549821));
#120483=CARTESIAN_POINT('Ctrl Pts',(7.03982677401824,3.78467661262501,1.73301442899937));
#120484=CARTESIAN_POINT('Ctrl Pts',(6.809159503,3.655724827,2.489547522));
#120485=CARTESIAN_POINT('Ctrl Pts',(6.908411361,3.703213228,2.218083843));
#120486=CARTESIAN_POINT('Ctrl Pts',(6.985737446,3.75,1.939580454));
#120487=CARTESIAN_POINT('Ctrl Pts',(7.014938362,3.76766825,1.83440826));
#120488=CARTESIAN_POINT('Ctrl Pts',(7.040959969,3.785449891,1.728404675));
#120489=CARTESIAN_POINT('Ctrl Pts',(7.124630184,3.655724827,2.34299909));
#120490=CARTESIAN_POINT('Ctrl Pts',(7.218039533,3.703213228,2.058958406));
#120491=CARTESIAN_POINT('Ctrl Pts',(7.288540418,3.75,1.768383042));
#120492=CARTESIAN_POINT('Ctrl Pts',(7.31516391,3.76766825,1.658652065));
#120493=CARTESIAN_POINT('Ctrl Pts',(7.338472024,3.785449891,1.548169354));
#120494=CARTESIAN_POINT('Ctrl Pts',(6.80915950467478,3.65572482780133,2.4895475174193));
#120495=CARTESIAN_POINT('Ctrl Pts',(6.86024694711263,3.68016830932062,2.34981829336983));
#120496=CARTESIAN_POINT('Ctrl Pts',(6.90691504685433,3.70444731696092,2.20882796211418));
#120497=CARTESIAN_POINT('Ctrl Pts',(6.94910295791911,3.72849592491557,2.06699494043432));
#120498=CARTESIAN_POINT('Ctrl Pts',(6.9617147222808,3.7356850786114,2.02459500635401));
#120499=CARTESIAN_POINT('Ctrl Pts',(6.97392645999889,3.74285366756795,1.9821197811675));
#120500=CARTESIAN_POINT('Ctrl Pts',(6.98573744594791,3.74999999996848,1.93958045418761));
#120501=CARTESIAN_POINT('Ctrl Pts',(7.00474976135324,3.76150355491264,1.87110428296099));
#120502=CARTESIAN_POINT('Ctrl Pts',(7.0227865466034,3.77306479262606,1.80223499602672));
#120503=CARTESIAN_POINT('Ctrl Pts',(7.03982677400277,3.78467661236402,1.73301442888571));
#120504=CARTESIAN_POINT('Ctrl Pts',(6.500628688,3.785444214,3.210035304));
#120505=CARTESIAN_POINT('Ctrl Pts',(6.674394881,3.720864611,2.858142135));
#120506=CARTESIAN_POINT('Ctrl Pts',(6.809159503,3.655724827,2.489547522));
#120507=CARTESIAN_POINT('Ctrl Pts',(6.61226633200001,3.785444214,3.53948216));
#120508=CARTESIAN_POINT('Ctrl Pts',(6.803866199,3.720864611,3.181545802));
#120509=CARTESIAN_POINT('Ctrl Pts',(6.955707935,3.655724827,2.805018204));
#120510=CARTESIAN_POINT('',(6.50269266208612,3.78467661244381,3.20585217509439));
#120511=CARTESIAN_POINT('Origin',(-0.187509038755996,3.62501423310757,-0.063088837505566));
#120512=CARTESIAN_POINT('Ctrl Pts',(6.72607429382293,3.74576903860098,3.31812064141916));
#120513=CARTESIAN_POINT('Ctrl Pts',(6.70045515785978,3.75001846751968,3.30518975552696));
#120514=CARTESIAN_POINT('Ctrl Pts',(6.67484928050536,3.75433282935375,3.29225369376685));
#120515=CARTESIAN_POINT('Ctrl Pts',(6.64923795717537,3.75872286883744,3.27935434482528));
#120516=CARTESIAN_POINT('Ctrl Pts',(6.62481513221521,3.76290918769716,3.26705359264465));
#120517=CARTESIAN_POINT('Ctrl Pts',(6.60039155305013,3.76716275954495,3.25477699767267));
#120518=CARTESIAN_POINT('Ctrl Pts',(6.57596763822924,3.77148708938579,3.24252626267529));
#120519=CARTESIAN_POINT('Ctrl Pts',(6.55154300579018,3.77581154628315,3.23027516772947));
#120520=CARTESIAN_POINT('Ctrl Pts',(6.52711785581645,3.78020679564801,3.21804984148404));
#120521=CARTESIAN_POINT('Ctrl Pts',(6.5026926613042,3.78467661251154,3.2058521752322));
#120522=CARTESIAN_POINT('Ctrl Pts',(6.114786011,3.655724827,3.895111301));
#120523=CARTESIAN_POINT('Ctrl Pts',(6.270074082,3.703213228,3.651330506));
#120524=CARTESIAN_POINT('Ctrl Pts',(6.405462322,3.75,3.395961195));
#120525=CARTESIAN_POINT('Ctrl Pts',(6.45658945,3.76766825,3.299525202));
#120526=CARTESIAN_POINT('Ctrl Pts',(6.504790324,3.785449891,3.201593798));
#120527=CARTESIAN_POINT('Ctrl Pts',(6.454384744,3.655724827,3.819805961));
#120528=CARTESIAN_POINT('Ctrl Pts',(6.606670585,3.703213228,3.562486238));
#120529=CARTESIAN_POINT('Ctrl Pts',(6.737988312,3.75,3.293859971));
#120530=CARTESIAN_POINT('Ctrl Pts',(6.787578278,3.76766825,3.192417707));
#120531=CARTESIAN_POINT('Ctrl Pts',(6.834091979,3.785449891,3.089528577));
#120532=CARTESIAN_POINT('Ctrl Pts',(6.11478601373434,3.65572482783619,3.89511129670746));
#120533=CARTESIAN_POINT('Ctrl Pts',(6.19471672344615,3.68016831260846,3.76963113674948));
#120534=CARTESIAN_POINT('Ctrl Pts',(6.27060251193692,3.70444732345577,3.64196932547167));
#120535=CARTESIAN_POINT('Ctrl Pts',(6.34229400865791,3.72849593454659,3.51252141730028));
#120536=CARTESIAN_POINT('Ctrl Pts',(6.3637256395827,3.73568508501387,3.47382394383685));
#120537=CARTESIAN_POINT('Ctrl Pts',(6.38478278197638,3.74285367075939,3.43496694581494));
#120538=CARTESIAN_POINT('Ctrl Pts',(6.40546232230385,3.74999999996872,3.39596119504962));
#120539=CARTESIAN_POINT('Ctrl Pts',(6.43875049341836,3.76150355492492,3.33317304420941));
#120540=CARTESIAN_POINT('Ctrl Pts',(6.47117044971429,3.77306479256857,3.26979125879157));
#120541=CARTESIAN_POINT('Ctrl Pts',(6.5026926613336,3.78467661235723,3.20585217511677));
#120542=CARTESIAN_POINT('Ctrl Pts',(5.6585849,3.785444214,4.532429474));
#120543=CARTESIAN_POINT('Ctrl Pts',(5.903935165,3.720864611,4.226117966));
#120544=CARTESIAN_POINT('Ctrl Pts',(6.114786011,3.655724827,3.895111301));
#120545=CARTESIAN_POINT('Ctrl Pts',(5.696791181,3.785444214,4.878172838));
#120546=CARTESIAN_POINT('Ctrl Pts',(5.960857287,3.720864611,4.56979314100001));
#120547=CARTESIAN_POINT('Ctrl Pts',(6.190091351,3.655724827,4.234710034));
#120548=CARTESIAN_POINT('',(5.66149986688143,3.78467661242999,4.52878783667046));
#120549=CARTESIAN_POINT('Origin',(-0.169563074774411,3.62501420262947,-0.101922854223928));
#120550=CARTESIAN_POINT('Ctrl Pts',(5.85552455969347,3.74576903856604,4.68645197658526));
#120551=CARTESIAN_POINT('Ctrl Pts',(5.8332841429803,3.75001846752245,4.66831605084936));
#120552=CARTESIAN_POINT('Ctrl Pts',(5.81105778769237,3.75433282936489,4.65017792033751));
#120553=CARTESIAN_POINT('Ctrl Pts',(5.78881822167272,3.75872286883866,4.63207447348692));
#120554=CARTESIAN_POINT('Ctrl Pts',(5.76761068695466,3.76290918769358,4.61481112053925));
#120555=CARTESIAN_POINT('Ctrl Pts',(5.74639722263548,3.7671627595273,4.59757119782373));
#120556=CARTESIAN_POINT('Ctrl Pts',(5.72517787158082,3.77148708931804,4.58035645850533));
#120557=CARTESIAN_POINT('Ctrl Pts',(5.70395789665028,3.77581154624956,4.56314121305174));
#120558=CARTESIAN_POINT('Ctrl Pts',(5.68273187698867,3.78020679560976,4.54595102275112));
#120559=CARTESIAN_POINT('Ctrl Pts',(5.66149986605684,3.78467661289658,4.52878783714528));
#120560=CARTESIAN_POINT('Ctrl Pts',(5.134491921,3.655724827,5.118544003));
#120561=CARTESIAN_POINT('Ctrl Pts',(5.338555108,3.703213228,4.913845014));
#120562=CARTESIAN_POINT('Ctrl Pts',(5.5256749,3.75,4.693550565));
#120563=CARTESIAN_POINT('Ctrl Pts',(5.596337592,3.76766825,4.610360012));
#120564=CARTESIAN_POINT('Ctrl Pts',(5.664463913,3.785449891,4.525079953));
#120565=CARTESIAN_POINT('Ctrl Pts',(5.482339447,3.655724827,5.11800295));
#120566=CARTESIAN_POINT('Ctrl Pts',(5.686381063,3.703213228,4.899436174));
#120567=CARTESIAN_POINT('Ctrl Pts',(5.872375362,3.75,4.665319669));
#120568=CARTESIAN_POINT('Ctrl Pts',(5.94261303000001,3.76766825,4.57690944600001));
#120569=CARTESIAN_POINT('Ctrl Pts',(6.010157388,3.785449891,4.486424876));
#120570=CARTESIAN_POINT('Ctrl Pts',(5.1344919245932,3.65572482783619,5.11854399939561));
#120571=CARTESIAN_POINT('Ctrl Pts',(5.23952844189472,3.68016831678484,5.01318021847078));
#120572=CARTESIAN_POINT('Ctrl Pts',(5.34108359530637,3.70444733171498,4.90481625233483));
#120573=CARTESIAN_POINT('Ctrl Pts',(5.43892647385379,3.7284959468036,4.79380629735723));
#120574=CARTESIAN_POINT('Ctrl Pts',(5.46817584118771,3.73568509318852,4.76062073496305));
#120575=CARTESIAN_POINT('Ctrl Pts',(5.4970937687556,3.74285367487428,4.72719887388563));
#120576=CARTESIAN_POINT('Ctrl Pts',(5.52567490020155,3.7500000000504,4.69355056476271));
#120577=CARTESIAN_POINT('Ctrl Pts',(5.57168240855751,3.76150355498939,4.63938633814908));
#120578=CARTESIAN_POINT('Ctrl Pts',(5.61696961380205,3.77306479247568,4.58445571633938));
#120579=CARTESIAN_POINT('Ctrl Pts',(5.66149986636746,3.78467661236143,4.52878783624501));
#120580=CARTESIAN_POINT('Ctrl Pts',(4.55195197,3.785444214,5.642892278));
#120581=CARTESIAN_POINT('Ctrl Pts',(4.857414002,3.720864611,5.39648521799999));
#120582=CARTESIAN_POINT('Ctrl Pts',(5.134491921,3.655724827,5.118544003));
#120583=CARTESIAN_POINT('Ctrl Pts',(4.514940407,3.785444214,5.988765576));
#120584=CARTESIAN_POINT('Ctrl Pts',(4.839125312,3.720864611,5.744362032));
#120585=CARTESIAN_POINT('Ctrl Pts',(5.135032975,3.655724827,5.466391529));
#120586=CARTESIAN_POINT('',(4.55558163233989,3.78467661243338,5.63996241300083));
#120587=CARTESIAN_POINT('Origin',(-0.143688241515189,3.62501423950758,-0.135990833085079));
#120588=CARTESIAN_POINT('Ctrl Pts',(4.7111770047759,3.7457690385862,5.83565002581625));
#120589=CARTESIAN_POINT('Ctrl Pts',(4.69335524483929,3.75001846749632,5.81315707568708));
#120590=CARTESIAN_POINT('Ctrl Pts',(4.6755476913489,3.75433282933081,5.7906649951772));
#120591=CARTESIAN_POINT('Ctrl Pts',(4.65771977994644,3.75872286880854,5.76820394759314));
#120592=CARTESIAN_POINT('Ctrl Pts',(4.64071917619361,3.76290918766191,5.74678520923227));
#120593=CARTESIAN_POINT('Ctrl Pts',(4.62370774462027,3.7671627594984,5.72538807866446));
#120594=CARTESIAN_POINT('Ctrl Pts',(4.60668515011344,3.77148708932264,5.70401427703497));
#120595=CARTESIAN_POINT('Ctrl Pts',(4.58966205543604,3.77581154620756,5.68263984738451));
#120596=CARTESIAN_POINT('Ctrl Pts',(4.57262767108181,3.78020679555432,5.66128858746507));
#120597=CARTESIAN_POINT('Ctrl Pts',(4.5555816317836,3.78467661248386,5.6399624126005));
#120598=CARTESIAN_POINT('Ctrl Pts',(3.914114695,3.655724827,6.102639278));
#120599=CARTESIAN_POINT('Ctrl Pts',(4.157411231,3.703213228,5.94659359));
#120600=CARTESIAN_POINT('Ctrl Pts',(4.38751306,3.75,5.771674726));
#120601=CARTESIAN_POINT('Ctrl Pts',(4.474407207,3.76766825,5.705619513));
#120602=CARTESIAN_POINT('Ctrl Pts',(4.559273465,3.785449891,5.636978399));
#120603=CARTESIAN_POINT('Ctrl Pts',(4.25394605,3.655724827,6.176887809));
#120604=CARTESIAN_POINT('Ctrl Pts',(4.500202683,3.703213228,6.007293919));
#120605=CARTESIAN_POINT('Ctrl Pts',(4.732176666,3.75,5.818634204));
#120606=CARTESIAN_POINT('Ctrl Pts',(4.819777801,3.76766825,5.747389985));
#120607=CARTESIAN_POINT('Ctrl Pts',(4.905194518,3.785449891,5.67354093500001));
#120608=CARTESIAN_POINT('Ctrl Pts',(3.91411469962435,3.65572482790262,6.10263927503403));
#120609=CARTESIAN_POINT('Ctrl Pts',(4.03934556802192,3.68016830661403,6.02231862036379));
#120610=CARTESIAN_POINT('Ctrl Pts',(4.16182141836033,3.7044473115228,5.93831953563007));
#120611=CARTESIAN_POINT('Ctrl Pts',(4.28124059665187,3.7284959168111,5.85093829710996));
#120612=CARTESIAN_POINT('Ctrl Pts',(4.31694009517294,3.73568507320295,5.82481630866601));
#120613=CARTESIAN_POINT('Ctrl Pts',(4.35236669927942,3.74285366484134,5.79839229546968));
#120614=CARTESIAN_POINT('Ctrl Pts',(4.38751306021334,3.7499999999068,5.77167472643996));
#120615=CARTESIAN_POINT('Ctrl Pts',(4.44408864624166,3.76150355484585,5.7286670844108));
#120616=CARTESIAN_POINT('Ctrl Pts',(4.50012552270294,3.77306479247613,5.68475612009858));
#120617=CARTESIAN_POINT('Ctrl Pts',(4.55558163185474,3.78467661218761,5.63996241248155));
#120618=CARTESIAN_POINT('Ctrl Pts',(3.232474826,3.785444214,6.489499711));
#120619=CARTESIAN_POINT('Ctrl Pts',(3.583765559,3.720864611,6.31451881899999));
#120620=CARTESIAN_POINT('Ctrl Pts',(3.914114695,3.655724827,6.102639278));
#120621=CARTESIAN_POINT('Ctrl Pts',(3.121976037,3.785444214,6.81933029100001));
#120622=CARTESIAN_POINT('Ctrl Pts',(3.491121217,3.720864611,6.650330939));
#120623=CARTESIAN_POINT('Ctrl Pts',(3.839866164,3.655724827,6.442470632));
#120624=CARTESIAN_POINT('',(3.23664946277011,3.78467661248022,6.48741861533793));
#120625=CARTESIAN_POINT('Origin',(-0.111094888332385,3.6250142351479,-0.163700176824847));
#120626=CARTESIAN_POINT('Ctrl Pts',(3.34654004953935,3.74576903858902,6.71197956579666));
#120627=CARTESIAN_POINT('Ctrl Pts',(3.33397027170812,3.75001846752048,6.68618133683447));
#120628=CARTESIAN_POINT('Ctrl Pts',(3.32141418136731,3.75433282935661,6.66038701106181));
#120629=CARTESIAN_POINT('Ctrl Pts',(3.30883153794991,3.75872286883258,6.63461861631273));
#120630=CARTESIAN_POINT('Ctrl Pts',(3.29683279451946,3.76290918768263,6.61004600887627));
#120631=CARTESIAN_POINT('Ctrl Pts',(3.28481883139786,3.76716275951602,6.58549217638448));
#120632=CARTESIAN_POINT('Ctrl Pts',(3.2727889512392,3.77148708935664,6.560958727682));
#120633=CARTESIAN_POINT('Ctrl Pts',(3.26075871765674,3.77581154624101,6.53642455821551));
#120634=CARTESIAN_POINT('Ctrl Pts',(3.24871247748031,3.78020679560717,6.51191058980696));
#120635=CARTESIAN_POINT('Ctrl Pts',(3.2366494621999,3.78467661255436,6.48741861492866));
#120636=CARTESIAN_POINT('Ctrl Pts',(2.510717817,3.655724827,6.801381922));
#120637=CARTESIAN_POINT('Ctrl Pts',(2.781871425,3.703213228,6.70128605900001));
#120638=CARTESIAN_POINT('Ctrl Pts',(3.044195986,3.75,6.579921793));
#120639=CARTESIAN_POINT('Ctrl Pts',(3.143258515,3.76766825,6.534090586));
#120640=CARTESIAN_POINT('Ctrl Pts',(3.240896457,3.785449891,6.485298001));
#120641=CARTESIAN_POINT('Ctrl Pts',(2.826642864,3.655724827,6.94694826000001));
#120642=CARTESIAN_POINT('Ctrl Pts',(3.103599827,3.703213228,6.834257277));
#120643=CARTESIAN_POINT('Ctrl Pts',(3.370706649,3.75,6.699875871));
#120644=CARTESIAN_POINT('Ctrl Pts',(3.47157512,3.76766825,6.649128957));
#120645=CARTESIAN_POINT('Ctrl Pts',(3.570870203,3.785449891,6.59536852600001));
#120646=CARTESIAN_POINT('Ctrl Pts',(2.51071782177452,3.65572482783619,6.80138192023749));
#120647=CARTESIAN_POINT('Ctrl Pts',(2.65028748540186,3.68016831654245,6.74986003173072));
#120648=CARTESIAN_POINT('Ctrl Pts',(2.78795729369265,3.70444733127152,6.69415346213049));
#120649=CARTESIAN_POINT('Ctrl Pts',(2.92336895432209,3.72849594620015,6.63448671431067));
#120650=CARTESIAN_POINT('Ctrl Pts',(2.96384921821405,3.73568509279227,6.61664980361853));
#120651=CARTESIAN_POINT('Ctrl Pts',(3.00412789473792,3.74285367468743,6.59845926607656));
#120652=CARTESIAN_POINT('Ctrl Pts',(3.04419598642018,3.75000000007494,6.57992179280561));
#120653=CARTESIAN_POINT('Ctrl Pts',(3.10869423890095,3.76150355506134,6.55008172319584));
#120654=CARTESIAN_POINT('Ctrl Pts',(3.17286056324773,3.77306479246515,6.51924364565036));
#120655=CARTESIAN_POINT('Ctrl Pts',(3.23664946229233,3.78467661220444,6.48741861481928));
#120656=CARTESIAN_POINT('Ctrl Pts',(1.761850751,3.785444214,7.03266535));
#120657=CARTESIAN_POINT('Ctrl Pts',(2.142544221,3.720864611,6.937292538));
#120658=CARTESIAN_POINT('Ctrl Pts',(2.510717817,3.655724827,6.801381922));
#120659=CARTESIAN_POINT('Ctrl Pts',(1.583031538,3.785444214,7.331030702));
#120660=CARTESIAN_POINT('Ctrl Pts',(1.979876174,3.720864611,7.245337762));
#120661=CARTESIAN_POINT('Ctrl Pts',(2.365151479,3.655724827,7.11730696800001));
#120662=CARTESIAN_POINT('',(1.76637516134309,3.78467661248993,7.03153033211043));
#120663=CARTESIAN_POINT('Origin',(-0.0733069003038278,3.62501423486551,
-0.183755265501093));
#120664=CARTESIAN_POINT('Ctrl Pts',(1.8254226014359,3.7457690386059,7.27446440098778));
#120665=CARTESIAN_POINT('Ctrl Pts',(1.81869255493101,3.7500184674834,7.24656718951097));
#120666=CARTESIAN_POINT('Ctrl Pts',(1.81197503635231,3.75433282934033,7.2186767325143));
#120667=CARTESIAN_POINT('Ctrl Pts',(1.80522601115336,3.75872286882405,7.19080589214298));
#120668=CARTESIAN_POINT('Ctrl Pts',(1.79879017574622,3.76290918769458,7.1642284033945));
#120669=CARTESIAN_POINT('Ctrl Pts',(1.79233544045292,3.76716275954058,7.13766597884808));
#120670=CARTESIAN_POINT('Ctrl Pts',(1.78586077837975,3.77148708937977,7.11112003987493));
#120671=CARTESIAN_POINT('Ctrl Pts',(1.77938592606624,3.77581154627763,7.08457332092151));
#120672=CARTESIAN_POINT('Ctrl Pts',(1.77289109879307,3.78020679564289,7.05804288983037));
#120673=CARTESIAN_POINT('Ctrl Pts',(1.76637516089216,3.78467661258282,7.03153033156102));
#120674=CARTESIAN_POINT('Ctrl Pts',(0.989922564,3.655724827,7.18209950600001));
#120675=CARTESIAN_POINT('Ctrl Pts',(1.276254403,3.703213228,7.142633839));
#120676=CARTESIAN_POINT('Ctrl Pts',(1.558535692,3.75,7.080499029));
#120677=CARTESIAN_POINT('Ctrl Pts',(1.665134548,3.76766825,7.057034846));
#120678=CARTESIAN_POINT('Ctrl Pts',(1.770978732,3.785449891,7.030372275));
#120679=CARTESIAN_POINT('Ctrl Pts',(1.267168999,3.655724827,7.39217713));
#120680=CARTESIAN_POINT('Ctrl Pts',(1.561876092,3.703213228,7.341658361));
#120681=CARTESIAN_POINT('Ctrl Pts',(1.851626136,3.75,7.267838788));
#120682=CARTESIAN_POINT('Ctrl Pts',(1.961045444,3.76766825,7.23996204900001));
#120683=CARTESIAN_POINT('Ctrl Pts',(2.069575967,3.785449891,7.208804014));
#120684=CARTESIAN_POINT('Ctrl Pts',(0.989922569042201,3.65572482783626,
7.18209950530503));
#120685=CARTESIAN_POINT('Ctrl Pts',(1.13730475520406,3.68016830007153,7.16178553557222));
#120686=CARTESIAN_POINT('Ctrl Pts',(1.28373108860322,3.70444729863585,7.136976313866));
#120687=CARTESIAN_POINT('Ctrl Pts',(1.4288033920426,3.72849589780304,7.10781407124424));
#120688=CARTESIAN_POINT('Ctrl Pts',(1.47217175613058,3.73568506058438,7.09909622003723));
#120689=CARTESIAN_POINT('Ctrl Pts',(1.51541926466407,3.74285365858513,7.08998967248929));
#120690=CARTESIAN_POINT('Ctrl Pts',(1.55853569203865,3.74999999998231,7.08049902911643));
#120691=CARTESIAN_POINT('Ctrl Pts',(1.62794074349579,3.76150355498248,7.06522182162138));
#120692=CARTESIAN_POINT('Ctrl Pts',(1.69723617000859,3.77306479253841,7.04889858360392));
#120693=CARTESIAN_POINT('Ctrl Pts',(1.76637516099065,3.78467661232633,7.03153033149357));
#120694=CARTESIAN_POINT('Ctrl Pts',(0.208844493,3.785444214,7.246991374));
#120695=CARTESIAN_POINT('Ctrl Pts',(0.601139897,3.720864611,7.235686168));
#120696=CARTESIAN_POINT('Ctrl Pts',(0.989922564,3.655724827,7.182099506));
#120697=CARTESIAN_POINT('Ctrl Pts',(-0.029933757,3.785444214,7.499940264));
#120698=CARTESIAN_POINT('Ctrl Pts',(0.376054321,3.720864611,7.501560644));
#120699=CARTESIAN_POINT('Ctrl Pts',(0.77984494,3.655724827,7.459345941));
#120700=CARTESIAN_POINT('',(0.213507120844762,3.78467661246786,7.24685550681245));
#120701=CARTESIAN_POINT('Origin',(-0.0320910878355247,3.62501421661864,
-0.19521798448639));
#120702=CARTESIAN_POINT('Ctrl Pts',(0.218950420658305,3.74576903856463,
7.49680336600003));
#120703=CARTESIAN_POINT('Ctrl Pts',(0.218374794353158,3.75001846750272,
7.46811161477292));
#120704=CARTESIAN_POINT('Ctrl Pts',(0.217809951500075,3.75433282935218,
7.43942915323723));
#120705=CARTESIAN_POINT('Ctrl Pts',(0.217210121623312,3.75872286883286,
7.41075907670793));
#120706=CARTESIAN_POINT('Ctrl Pts',(0.216638126966634,3.76290918769233,
7.38341944055992));
#120707=CARTESIAN_POINT('Ctrl Pts',(0.216044435932847,3.76716275952922,
7.35609045350274));
#120708=CARTESIAN_POINT('Ctrl Pts',(0.215427740108189,3.7714870893588,7.32877328291361));
#120709=CARTESIAN_POINT('Ctrl Pts',(0.214811026164153,3.77581154624318,
7.30145530970816));
#120710=CARTESIAN_POINT('Ctrl Pts',(0.214171302877491,3.7802067955946,7.27414894952492));
#120711=CARTESIAN_POINT('Ctrl Pts',(0.213507120496326,3.78467661249255,
7.24685550621309));
#120712=CARTESIAN_POINT('Ctrl Pts',(-0.577160368,3.655724827,7.2269901));
#120713=CARTESIAN_POINT('Ctrl Pts',(-0.289038857,3.703213228,7.25000000000001));
#120714=CARTESIAN_POINT('Ctrl Pts',(0.,3.75,7.25));
#120715=CARTESIAN_POINT('Ctrl Pts',(0.10915074,3.76766825,7.25));
#120716=CARTESIAN_POINT('Ctrl Pts',(0.218252011,3.785449891,7.246714156));
#120717=CARTESIAN_POINT('Ctrl Pts',(-0.35155628,3.655724827,7.491756015));
#120718=CARTESIAN_POINT('Ctrl Pts',(-0.052879233,3.703213228,7.505771659));
#120719=CARTESIAN_POINT('Ctrl Pts',(0.245965642,3.75,7.495965642));
#120720=CARTESIAN_POINT('Ctrl Pts',(0.358819462,3.76766825,7.492262562));
#120721=CARTESIAN_POINT('Ctrl Pts',(0.471510658,3.785449891,7.48516383900001));
#120722=CARTESIAN_POINT('Ctrl Pts',(-0.577160365809908,3.655724827,7.22699010257026));
#120723=CARTESIAN_POINT('Ctrl Pts',(-0.428857240241091,3.68016825824677,
7.23883385462487));
#120724=CARTESIAN_POINT('Ctrl Pts',(-0.280521273726523,3.7044472163737,
7.24608198666862));
#120725=CARTESIAN_POINT('Ctrl Pts',(-0.132571908922941,3.72849577568566,
7.24878780841957));
#120726=CARTESIAN_POINT('Ctrl Pts',(-0.0883431417441284,3.73568497945282,
7.24959670111343));
#120727=CARTESIAN_POINT('Ctrl Pts',(-0.0441488467817412,3.74285361818873,
7.25000000004411));
#120728=CARTESIAN_POINT('Ctrl Pts',(2.36530813326477E-10,3.75000000003403,
7.25000000002632));
#120729=CARTESIAN_POINT('Ctrl Pts',(0.0710665482390681,3.76150355500044,
7.24999999999768));
#120730=CARTESIAN_POINT('Ctrl Pts',(0.142250900143361,3.77306479256824,
7.24895485867233));
#120731=CARTESIAN_POINT('Ctrl Pts',(0.213507120622118,3.78467661225502,
7.24685550617113));
#120732=CARTESIAN_POINT('Ctrl Pts',(0.209270709,2.233426833,7.246979079));
#120733=CARTESIAN_POINT('Ctrl Pts',(0.602449449,2.169174758,7.235625273));
#120734=CARTESIAN_POINT('Ctrl Pts',(0.992091961,2.104034486,7.18180016));
#120735=CARTESIAN_POINT('Ctrl Pts',(-0.029492665,2.233426833,7.499942012));
#120736=CARTESIAN_POINT('Ctrl Pts',(0.377410366,2.169174758,7.501542112));
#120737=CARTESIAN_POINT('Ctrl Pts',(0.782098092,2.104034486,7.45911003900001));
#120738=CARTESIAN_POINT('',(0.221277496030376,2.19371102278168,7.49673504087804));
#120739=CARTESIAN_POINT('',(0.782098084443547,2.10403448602304,7.45911003971491));
#120740=CARTESIAN_POINT('Origin',(-0.0334709911476522,2.01789494501912,
-0.18672642780092));
#120741=CARTESIAN_POINT('',(0.887095018906516,2.10403448477417,7.32045510042018));
#120742=CARTESIAN_POINT('Ctrl Pts',(0.221277495100879,2.19371102279664,
7.49673504090519));
#120743=CARTESIAN_POINT('Ctrl Pts',(0.220158920792203,2.19989438507272,
7.45504412804595));
#120744=CARTESIAN_POINT('Ctrl Pts',(0.218990649590036,2.20622738122548,
7.41335239673016));
#120745=CARTESIAN_POINT('Ctrl Pts',(0.216548003071353,2.2192010688388,7.33006921341966));
#120746=CARTESIAN_POINT('Ctrl Pts',(0.21527218294975,2.22584946938312,7.28842824146336));
#120747=CARTESIAN_POINT('Ctrl Pts',(0.213937948795667,2.23266407510067,
7.24684279883278));
#120748=CARTESIAN_POINT('Ctrl Pts',(0.984221732802958,2.10273945758871,
7.18288735118082));
#120749=CARTESIAN_POINT('Ctrl Pts',(0.988156846901479,2.10338697179435,
7.18234375559041));
#120750=CARTESIAN_POINT('Ctrl Pts',(0.992091961000001,2.104034486,7.18180016));
#120751=CARTESIAN_POINT('Ctrl Pts',(1.110469927,2.123513315,7.16544746));
#120752=CARTESIAN_POINT('Ctrl Pts',(1.228244647,2.142857143,7.145202243));
#120753=CARTESIAN_POINT('Ctrl Pts',(1.502027081,2.18782435,7.098139641));
#120754=CARTESIAN_POINT('Ctrl Pts',(1.77140546,2.233445087,7.030264767));
#120755=CARTESIAN_POINT('Ctrl Pts',(1.26130148850622,2.10273945758871,7.39318511227826));
#120756=CARTESIAN_POINT('Ctrl Pts',(1.26535166425311,2.10338697179435,7.39248957063913));
#120757=CARTESIAN_POINT('Ctrl Pts',(1.26940184,2.104034486,7.39179402900001));
#120758=CARTESIAN_POINT('Ctrl Pts',(1.391241145,2.123513315,7.370870416));
#120759=CARTESIAN_POINT('Ctrl Pts',(1.51232468,2.142857143,7.345942694));
#120760=CARTESIAN_POINT('Ctrl Pts',(1.793798878,2.18782435,7.287995009));
#120761=CARTESIAN_POINT('Ctrl Pts',(2.070013524,2.233445087,7.208678382));
#120762=CARTESIAN_POINT('',(1.26940183221411,2.10403448602285,7.39179403024986));
#120763=CARTESIAN_POINT('',(1.82768058314702,2.19371102273794,7.27389742077111));
#120764=CARTESIAN_POINT('Ctrl Pts',(1.26940183226555,2.10403448479508,7.39179403014459));
#120765=CARTESIAN_POINT('Ctrl Pts',(1.35075679015265,2.11704095516579,7.37782284375772));
#120766=CARTESIAN_POINT('Ctrl Pts',(1.43175196247422,2.12998516342569,7.36253036882388));
#120767=CARTESIAN_POINT('Ctrl Pts',(1.51232468132839,2.14285714321222,7.34594269372652));
#120768=CARTESIAN_POINT('Ctrl Pts',(1.61770521265512,2.15969232100109,7.32424778213805));
#120769=CARTESIAN_POINT('Ctrl Pts',(1.72287450736513,2.17665108707963,7.30023158799395));
#120770=CARTESIAN_POINT('Ctrl Pts',(1.82768058353484,2.19371102295844,7.27389742079628));
#120771=CARTESIAN_POINT('Ctrl Pts',(1.76679318445803,2.23266407503808,7.03142530635304));
#120772=CARTESIAN_POINT('Ctrl Pts',(1.77703575218887,2.22584954505362,7.07175123545953));
#120773=CARTESIAN_POINT('Ctrl Pts',(1.78723319543015,2.21920122285034,7.11214388952697));
#120774=CARTESIAN_POINT('Ctrl Pts',(1.80752239779132,2.20622738127396,7.19295582045961));
#120775=CARTESIAN_POINT('Ctrl Pts',(1.81762584542517,2.19989438509207,7.23342167862178));
#120776=CARTESIAN_POINT('Ctrl Pts',(1.82768058214188,2.19371102275407,7.27389742102327));
#120777=CARTESIAN_POINT('',(1.13074689248641,2.10403448732041,7.28679709574353));
#120778=CARTESIAN_POINT('Origin',(2.88506198098393E-13,2.19479107899967,
1.24553145575135E-12));
#120779=CARTESIAN_POINT('',(1.82046088170416,2.01370168037458,7.27570767520946));
#120780=CARTESIAN_POINT('Origin',(-0.0461554580507678,2.0178579971655,-0.187186739991818));
#120781=CARTESIAN_POINT('',(2.36730123479692,2.10403448602304,7.11659222239181));
#120782=CARTESIAN_POINT('Origin',(-0.0234499208926006,1.87510628711794,
-0.184916550569142));
#120783=CARTESIAN_POINT('Origin',(-0.0728291832817074,2.01789495839557,
-0.175165815870086));
#120784=CARTESIAN_POINT('Ctrl Pts',(1.762264358,2.233426833,7.032561719));
#120785=CARTESIAN_POINT('Ctrl Pts',(2.143810065,2.169174758,6.936951552));
#120786=CARTESIAN_POINT('Ctrl Pts',(2.512772145,2.104034486,6.800623218));
#120787=CARTESIAN_POINT('Ctrl Pts',(1.583462693,2.233426833,7.330937587));
#120788=CARTESIAN_POINT('Ctrl Pts',(1.981196531,2.169174758,7.245028153));
#120789=CARTESIAN_POINT('Ctrl Pts',(2.367301242,2.104034486,7.11659222000001));
#120790=CARTESIAN_POINT('',(2.44003668628186,2.10403448477417,6.95860772153105));
#120791=CARTESIAN_POINT('Ctrl Pts',(2.50531963238596,2.10273945758871,6.80337685771357));
#120792=CARTESIAN_POINT('Ctrl Pts',(2.50904588869298,2.10338697179435,6.80200003785678));
#120793=CARTESIAN_POINT('Ctrl Pts',(2.512772145,2.104034486,6.80062321800001));
#120794=CARTESIAN_POINT('Ctrl Pts',(2.624867152,2.123513315,6.759205071));
#120795=CARTESIAN_POINT('Ctrl Pts',(2.735536241,2.142857143,6.714115092));
#120796=CARTESIAN_POINT('Ctrl Pts',(2.992800725,2.18782435,6.60929765800001));
#120797=CARTESIAN_POINT('Ctrl Pts',(3.241290096,2.233445087,6.485101272));
#120798=CARTESIAN_POINT('Ctrl Pts',(2.82112921903791,2.10273945758871,6.94919401667824));
#120799=CARTESIAN_POINT('Ctrl Pts',(2.82493518301896,2.10338697179435,6.94764406833912));
#120800=CARTESIAN_POINT('Ctrl Pts',(2.828741147,2.104034486,6.94609412));
#120801=CARTESIAN_POINT('Ctrl Pts',(2.943233958,2.123513315,6.89946784));
#120802=CARTESIAN_POINT('Ctrl Pts',(3.056127904,2.142857143,6.849093534));
#120803=CARTESIAN_POINT('Ctrl Pts',(3.318564352,2.18782435,6.731992001));
#120804=CARTESIAN_POINT('Ctrl Pts',(3.571270523,2.233445087,6.595151768));
#120805=CARTESIAN_POINT('',(2.82874113964746,2.10403448602284,6.94609412285167));
#120806=CARTESIAN_POINT('',(3.34862335744545,2.19371102277393,6.71094044162914));
#120807=CARTESIAN_POINT('Ctrl Pts',(2.82874113969246,2.10403448479508,6.9460941227805));
#120808=CARTESIAN_POINT('Ctrl Pts',(2.90519067147956,2.11704095516575,6.91496066358089));
#120809=CARTESIAN_POINT('Ctrl Pts',(2.98100479150848,2.12998516342585,6.88261415040418));
#120810=CARTESIAN_POINT('Ctrl Pts',(3.05612790518021,2.14285714325508,6.84909353320588));
#120811=CARTESIAN_POINT('Ctrl Pts',(3.15438093342072,2.1596923211117,6.80525213688257));
#120812=CARTESIAN_POINT('Ctrl Pts',(3.2519286566968,2.1766510870814,6.75918913885246));
#120813=CARTESIAN_POINT('Ctrl Pts',(3.34862335742491,2.19371102292536,6.71094044145691));
#120814=CARTESIAN_POINT('Ctrl Pts',(3.23703513543889,2.23266407512044,6.4872261814177));
#120815=CARTESIAN_POINT('Ctrl Pts',(3.25570709552928,2.22584955417931,6.52440741393398));
#120816=CARTESIAN_POINT('Ctrl Pts',(3.27434932678514,2.2192012413584,6.56166350465828));
#120817=CARTESIAN_POINT('Ctrl Pts',(3.31153637344353,2.20622739343214,6.63622455513787));
#120818=CARTESIAN_POINT('Ctrl Pts',(3.3301025323744,2.19989440977418,6.6735723221256));
#120819=CARTESIAN_POINT('Ctrl Pts',(3.34862335692001,2.1937110227988,6.71094044189368));
#120820=CARTESIAN_POINT('',(2.67075663844113,2.1040344873204,6.87335867193713));
#120821=CARTESIAN_POINT('Origin',(1.10154940724527E-13,2.19479107899989,
1.74773390204663E-13));
#120822=CARTESIAN_POINT('',(3.34196159990719,2.01370168036029,6.71426039577534));
#120823=CARTESIAN_POINT('Origin',(-0.0853159245424984,2.01785799516844,
-0.172888221673519));
#120824=CARTESIAN_POINT('',(3.84181201039925,2.10403448602304,6.4413104627498));
#120825=CARTESIAN_POINT('Origin',(-0.0626532618141579,1.87510632037829,
-0.175552255440798));
#120826=CARTESIAN_POINT('Origin',(-0.108781860044905,2.01789497339341,-0.155414262569433));
#120827=CARTESIAN_POINT('Ctrl Pts',(3.232856486,2.233426833,6.489309589));
#120828=CARTESIAN_POINT('Ctrl Pts',(3.584928506,2.169174758,6.313913686));
#120829=CARTESIAN_POINT('Ctrl Pts',(3.915957895,2.104034486,6.101456692));
#120830=CARTESIAN_POINT('Ctrl Pts',(3.122377096,2.233426833,6.81914666800001));
#120831=CARTESIAN_POINT('Ctrl Pts',(3.492344149,2.169174758,6.649744731));
#120832=CARTESIAN_POINT('Ctrl Pts',(3.841812017,2.104034486,6.441310459));
#120833=CARTESIAN_POINT('',(3.87888494949472,2.10403448477417,6.27138357952356));
#120834=CARTESIAN_POINT('Ctrl Pts',(3.90927156911326,2.10273945758871,6.1057480230819));
#120835=CARTESIAN_POINT('Ctrl Pts',(3.91261473205663,2.10338697179435,6.10360235754095));
#120836=CARTESIAN_POINT('Ctrl Pts',(3.915957895,2.104034486,6.101456692));
#120837=CARTESIAN_POINT('Ctrl Pts',(4.016528506,2.123513315,6.036909765));
#120838=CARTESIAN_POINT('Ctrl Pts',(4.114917201,2.142857143,5.969083383));
#120839=CARTESIAN_POINT('Ctrl Pts',(4.343634335,2.18782435,5.811412262));
#120840=CARTESIAN_POINT('Ctrl Pts',(4.55961561000001,2.233445087,5.636701649));
#120841=CARTESIAN_POINT('Ctrl Pts',(4.24904408282165,2.10273945758871,6.18026633229042));
#120842=CARTESIAN_POINT('Ctrl Pts',(4.25242787241083,2.10338697179435,6.17793445114522));
#120843=CARTESIAN_POINT('Ctrl Pts',(4.255811662,2.104034486,6.17560257000001));
#120844=CARTESIAN_POINT('Ctrl Pts',(4.357604423,2.123513315,6.105453817));
#120845=CARTESIAN_POINT('Ctrl Pts',(4.457029984,2.142857143,6.031988372));
#120846=CARTESIAN_POINT('Ctrl Pts',(4.68815744500001,2.18782435,5.86120852900001));
#120847=CARTESIAN_POINT('Ctrl Pts',(4.905538882,2.233445087,5.673243189));
#120848=CARTESIAN_POINT('',(4.25581165537718,2.10403448602284,6.17560257428551));
#120849=CARTESIAN_POINT('',(4.71298822490245,2.19371102275907,5.83418734600645));
#120850=CARTESIAN_POINT('Ctrl Pts',(4.25581165546101,2.10403448479508,6.17560257428641));
#120851=CARTESIAN_POINT('Ctrl Pts',(4.32378106640512,2.11704095516577,6.12876260887064));
#120852=CARTESIAN_POINT('Ctrl Pts',(4.39086915015339,2.12998516342558,6.080874544256));
#120853=CARTESIAN_POINT('Ctrl Pts',(4.45702998493875,2.14285714318264,6.03198837130636));
#120854=CARTESIAN_POINT('Ctrl Pts',(4.54356130742803,2.15969232094174,5.96805046617741));
#120855=CARTESIAN_POINT('Ctrl Pts',(4.62892623627878,2.17665108709072,5.90209451773462));
#120856=CARTESIAN_POINT('Ctrl Pts',(4.71298822516702,2.19371102296318,5.83418734583089));
#120857=CARTESIAN_POINT('Ctrl Pts',(4.55591692076068,2.2326640751634,5.63969156977356));
#120858=CARTESIAN_POINT('Ctrl Pts',(4.58214553279196,2.22584946947947,5.6719900080537));
#120859=CARTESIAN_POINT('Ctrl Pts',(4.6083612467119,2.21920106896372,5.70436800343796));
#120860=CARTESIAN_POINT('Ctrl Pts',(4.66070659567174,2.20622739621349,5.7691908669884));
#120861=CARTESIAN_POINT('Ctrl Pts',(4.68686734132964,2.19989441540384,5.8016742728421));
#120862=CARTESIAN_POINT('Ctrl Pts',(4.71298822419491,2.19371102277413,5.83418734657775));
#120863=CARTESIAN_POINT('',(4.08588477174921,2.10403448732041,6.13852963549342));
#120864=CARTESIAN_POINT('Origin',(-9.68843061333047E-13,2.19479107900022,
-1.23252102968152E-12));
#120865=CARTESIAN_POINT('',(4.70719590771126,2.013701680375,5.83886176247297));
#120866=CARTESIAN_POINT('Origin',(-0.120487294631751,2.01785797603456,-0.150505974900553));
#120867=CARTESIAN_POINT('',(5.13668392641915,2.10403448602304,5.46484018414439));
#120868=CARTESIAN_POINT('Origin',(-0.0989268749541183,1.87510626229254,
-0.157979202217122));
#120869=CARTESIAN_POINT('Origin',(-0.139648184984119,2.01789496832727,-0.128396010934203));
#120870=CARTESIAN_POINT('Ctrl Pts',(4.552283837,2.233426833,5.642624555));
#120871=CARTESIAN_POINT('Ctrl Pts',(4.858419675,2.169174758,5.395644234));
#120872=CARTESIAN_POINT('Ctrl Pts',(5.136037807,2.104034486,5.116992833));
#120873=CARTESIAN_POINT('Ctrl Pts',(4.515292615,2.233426833,5.988500029));
#120874=CARTESIAN_POINT('Ctrl Pts',(4.84019363500001,2.169174758,5.74352663500001));
#120875=CARTESIAN_POINT('Ctrl Pts',(5.136683932,2.104034486,5.464840179));
#120876=CARTESIAN_POINT('',(5.13636086401175,2.10403448477417,5.29091651132793));
#120877=CARTESIAN_POINT('Ctrl Pts',(5.13043031307457,2.10273945758871,5.12262119754958));
#120878=CARTESIAN_POINT('Ctrl Pts',(5.13323406003728,2.10338697179435,5.11980701527479));
#120879=CARTESIAN_POINT('Ctrl Pts',(5.136037807,2.104034486,5.11699283300001));
#120880=CARTESIAN_POINT('Ctrl Pts',(5.220381451,2.123513315,5.032335269));
#120881=CARTESIAN_POINT('Ctrl Pts',(5.301889206,2.142857143,4.944943968));
#120882=CARTESIAN_POINT('Ctrl Pts',(5.49136443000001,2.18782435,4.741791688));
#120883=CARTESIAN_POINT('Ctrl Pts',(5.664738566,2.233445087,4.524736122));
#120884=CARTESIAN_POINT('Ctrl Pts',(5.47827836712804,2.10273945758871,5.12235626254307));
#120885=CARTESIAN_POINT('Ctrl Pts',(5.48108176006402,2.10338697179435,5.11935148477153));
#120886=CARTESIAN_POINT('Ctrl Pts',(5.483885153,2.104034486,5.116346707));
#120887=CARTESIAN_POINT('Ctrl Pts',(5.568218147,2.123513315,5.025955559));
#120888=CARTESIAN_POINT('Ctrl Pts',(5.649526295,2.142857143,4.932834139));
#120889=CARTESIAN_POINT('Ctrl Pts',(5.838537507,2.18782435,4.71636146100001));
#120890=CARTESIAN_POINT('Ctrl Pts',(6.010429695,2.233445087,4.486060063));
#120891=CARTESIAN_POINT('',(5.48388515162104,2.10403448644943,5.11634671002942));
#120892=CARTESIAN_POINT('',(5.85697900152487,2.19371102277848,4.68463413472096));
#120893=CARTESIAN_POINT('Ctrl Pts',(5.48388515081103,2.10403448555181,5.11634670908027));
#120894=CARTESIAN_POINT('Ctrl Pts',(5.5401962652435,2.11704095566781,5.05599042349386));
#120895=CARTESIAN_POINT('Ctrl Pts',(5.59542134742777,2.12998516367539,4.9948000018663));
#120896=CARTESIAN_POINT('Ctrl Pts',(5.64952629587031,2.14285714323533,4.93283413787128));
#120897=CARTESIAN_POINT('Ctrl Pts',(5.72028980490418,2.1596923210693,4.85178938829458));
#120898=CARTESIAN_POINT('Ctrl Pts',(5.78948036981908,2.17665108709428,4.76902451731539));
#120899=CARTESIAN_POINT('Ctrl Pts',(5.85697900143682,2.19371102292441,4.68463413468002));
#120900=CARTESIAN_POINT('Ctrl Pts',(5.66176909438834,2.2326640750986,4.52845124925428));
#120901=CARTESIAN_POINT('Ctrl Pts',(5.69432770564971,2.22584946943075,4.55435619166373));
#120902=CARTESIAN_POINT('Ctrl Pts',(5.72689082273297,2.21920106893194,4.58034160385709));
#120903=CARTESIAN_POINT('Ctrl Pts',(5.79194737442727,2.20622739455584,4.63239624867638));
#120904=CARTESIAN_POINT('Ctrl Pts',(5.8244794777516,2.19989441206853,4.65849643099321));
#120905=CARTESIAN_POINT('Ctrl Pts',(5.85697900107028,2.19371102279883,4.68463413529101));
#120906=CARTESIAN_POINT('',(5.30996147437299,2.10403448732041,5.11666977583958));
#120907=CARTESIAN_POINT('Origin',(8.50014503228635E-14,2.19479107899956,
-6.0281640790194E-14));
#120908=CARTESIAN_POINT('',(5.85232696648488,2.01370168039118,4.69044444290746));
#120909=CARTESIAN_POINT('Origin',(-0.150024755449846,2.01785801005925,-0.121086082215633));
#120910=CARTESIAN_POINT('',(6.19137021059321,2.10403448602304,4.23284005318077));
#120911=CARTESIAN_POINT('Origin',(-0.130574934157813,1.87510630182543,-0.133019420198138));
#120912=CARTESIAN_POINT('Origin',(-0.163984545083379,2.01789498312784,-0.0953738858012115));
#120913=CARTESIAN_POINT('Ctrl Pts',(5.658851455,2.233426833,4.532096669));
#120914=CARTESIAN_POINT('Ctrl Pts',(5.904736539,2.169174758,4.225080454));
#120915=CARTESIAN_POINT('Ctrl Pts',(6.115962299,2.104034486,3.893264076));
#120916=CARTESIAN_POINT('Ctrl Pts',(5.697078071,2.233426833,4.877837785));
#120917=CARTESIAN_POINT('Ctrl Pts',(5.961721047,2.169174758,4.568747618));
#120918=CARTESIAN_POINT('Ctrl Pts',(6.191370215,2.104034486,4.232840047));
#120919=CARTESIAN_POINT('',(6.15366625278541,2.10403448477417,4.06305206788318));
#120920=CARTESIAN_POINT('Ctrl Pts',(6.11169583714959,2.10273945758871,3.89996629798646));
#120921=CARTESIAN_POINT('Ctrl Pts',(6.1138290680748,2.10338697179435,3.89661518699323));
#120922=CARTESIAN_POINT('Ctrl Pts',(6.115962299,2.104034486,3.893264076));
#120923=CARTESIAN_POINT('Ctrl Pts',(6.180135162,2.123513315,3.792454368));
#120924=CARTESIAN_POINT('Ctrl Pts',(6.240950764,2.142857143,3.68958447));
#120925=CARTESIAN_POINT('Ctrl Pts',(6.382324428,2.18782435,3.450450204));
#120926=CARTESIAN_POINT('Ctrl Pts',(6.504984643,2.233445087,3.201198963));
#120927=CARTESIAN_POINT('Ctrl Pts',(6.45135444343917,2.10273945758871,3.82493050776523));
#120928=CARTESIAN_POINT('Ctrl Pts',(6.45344635621958,2.10338697179435,3.82139333338262));
#120929=CARTESIAN_POINT('Ctrl Pts',(6.455538269,2.104034486,3.817856159));
#120930=CARTESIAN_POINT('Ctrl Pts',(6.51846818000001,2.123513315,3.711449204));
#120931=CARTESIAN_POINT('Ctrl Pts',(6.577857036,2.142857143,3.603026063));
#120932=CARTESIAN_POINT('Ctrl Pts',(6.71591404400001,2.18782435,3.350982573));
#120933=CARTESIAN_POINT('Ctrl Pts',(6.834279495,2.233445087,3.089113754));
#120934=CARTESIAN_POINT('',(6.45553826687932,2.10403448645287,3.81785616360662));
#120935=CARTESIAN_POINT('',(6.72710394928449,2.19371102277434,3.31603263760013));
#120936=CARTESIAN_POINT('Ctrl Pts',(6.45553826486484,2.10403448479514,3.81785616563568));
#120937=CARTESIAN_POINT('Ctrl Pts',(6.49755804059041,2.11704095516578,3.74680574940807));
#120938=CARTESIAN_POINT('Ctrl Pts',(6.53833786010976,2.1299851634258,3.67517416401284));
#120939=CARTESIAN_POINT('Ctrl Pts',(6.57785703661758,2.14285714324141,3.60302606167866));
#120940=CARTESIAN_POINT('Ctrl Pts',(6.62954390864494,2.15969232108233,3.50866403078514));
#120941=CARTESIAN_POINT('Ctrl Pts',(6.67932483578951,2.17665108709007,3.41296023049362));
#120942=CARTESIAN_POINT('Ctrl Pts',(6.72710394921967,2.19371102294551,3.31603263741837));
#120943=CARTESIAN_POINT('Ctrl Pts',(6.50288323742489,2.23266407508744,3.20546558167077));
#120944=CARTESIAN_POINT('Ctrl Pts',(6.54024908133438,2.22584953542554,3.22376556438151));
#120945=CARTESIAN_POINT('Ctrl Pts',(6.57763657488875,2.21920120319565,3.24214314013562));
#120946=CARTESIAN_POINT('Ctrl Pts',(6.65236312620955,2.20622739415915,3.27899592300733));
#120947=CARTESIAN_POINT('Ctrl Pts',(6.68974541749201,2.19989441124867,3.29749245826285));
#120948=CARTESIAN_POINT('Ctrl Pts',(6.72710394898493,2.1937110227962,3.31603263821102));
#120949=CARTESIAN_POINT('',(6.28575027975988,2.10403448732041,3.8555601244127));
#120950=CARTESIAN_POINT('Origin',(-4.78783679369599E-13,2.19479107899967,
-2.39391839684799E-13));
#120951=CARTESIAN_POINT('',(6.72380972100024,2.01370168038612,3.32270715385081));
#120952=CARTESIAN_POINT('Origin',(-0.172547194246069,2.01785801023315,-0.0860042763948671));
#120953=CARTESIAN_POINT('',(6.95655490512516,2.10403448602304,2.80291702502399));
#120954=CARTESIAN_POINT('Origin',(-0.156117583468591,1.87510627379371,-0.101839827848934));
#120955=CARTESIAN_POINT('Origin',(-0.180653106157236,2.01789493165625,-0.0578921944339506));
#120956=CARTESIAN_POINT('Ctrl Pts',(6.500817468,2.233426833,3.209652979));
#120957=CARTESIAN_POINT('Ctrl Pts',(6.674954485,2.169174758,2.856956608));
#120958=CARTESIAN_POINT('Ctrl Pts',(6.809911191,2.104034486,2.487490617));
#120959=CARTESIAN_POINT('Ctrl Pts',(6.612474487,2.233426833,3.539093268));
#120960=CARTESIAN_POINT('Ctrl Pts',(6.804485009,2.169174758,3.180339039));
#120961=CARTESIAN_POINT('Ctrl Pts',(6.956554908,2.104034486,2.802917018));
#120962=CARTESIAN_POINT('',(6.88323304675614,2.10403448477417,2.64520382463995));
#120963=CARTESIAN_POINT('Ctrl Pts',(6.80718525625549,2.10273945758871,2.49495330789937));
#120964=CARTESIAN_POINT('Ctrl Pts',(6.80854822362774,2.10338697179435,2.49122196244969));
#120965=CARTESIAN_POINT('Ctrl Pts',(6.809911191,2.104034486,2.487490617));
#120966=CARTESIAN_POINT('Ctrl Pts',(6.850912621,2.123513315,2.375242516));
#120967=CARTESIAN_POINT('Ctrl Pts',(6.888192401,2.142857143,2.261704102));
#120968=CARTESIAN_POINT('Ctrl Pts',(6.974854028,2.18782435,1.997769504));
#120969=CARTESIAN_POINT('Ctrl Pts',(7.041064867,2.233445087,1.727977298));
#120970=CARTESIAN_POINT('Ctrl Pts',(7.1227723568037,2.10273945758871,2.34865525323209));
#120971=CARTESIAN_POINT('Ctrl Pts',(7.12405497390185,2.10338697179435,2.34475107661605));
#120972=CARTESIAN_POINT('Ctrl Pts',(7.125337591,2.104034486,2.3408469));
#120973=CARTESIAN_POINT('Ctrl Pts',(7.163921886,2.123513315,2.22339961));
#120974=CARTESIAN_POINT('Ctrl Pts',(7.198614493,2.142857143,2.104744493));
#120975=CARTESIAN_POINT('Ctrl Pts',(7.279261905,2.18782435,1.828915464));
#120976=CARTESIAN_POINT('Ctrl Pts',(7.338565982,2.233445087,1.547723919));
#120977=CARTESIAN_POINT('',(7.12533758978023,2.10403448645145,2.34084690533364));
#120978=CARTESIAN_POINT('',(7.28267699335155,2.19371102276864,1.7923771396886));
#120979=CARTESIAN_POINT('Ctrl Pts',(7.125337588388,2.10403448479513,2.34084690736949));
#120980=CARTESIAN_POINT('Ctrl Pts',(7.15110122605881,2.11704095516579,2.26242460083382));
#120981=CARTESIAN_POINT('Ctrl Pts',(7.17552896264762,2.12998516342569,2.18370126632093));
#120982=CARTESIAN_POINT('Ctrl Pts',(7.19861449338138,2.14285714321265,2.1047444916956));
#120983=CARTESIAN_POINT('Ctrl Pts',(7.22880790787021,2.15969232101418,2.00147744319749));
#120984=CARTESIAN_POINT('Ctrl Pts',(7.25685149639181,2.17665108709078,1.8973097164389));
#120985=CARTESIAN_POINT('Ctrl Pts',(7.28267699333017,2.1937110229533,1.79237713946812));
#120986=CARTESIAN_POINT('Ctrl Pts',(7.03992978818633,2.23266407510364,1.73259590538724));
#120987=CARTESIAN_POINT('Ctrl Pts',(7.08035593384536,2.22584954571016,1.74243547782734));
#120988=CARTESIAN_POINT('Ctrl Pts',(7.12081989475702,2.21920122410525,1.75234617281721));
#120989=CARTESIAN_POINT('Ctrl Pts',(7.20172176572101,2.20622739487872,1.77227338946031));
#120990=CARTESIAN_POINT('Ctrl Pts',(7.24220628307591,2.19989441271045,1.78230139712961));
#120991=CARTESIAN_POINT('Ctrl Pts',(7.2826769931679,2.19371102278755,1.79237714043786));
#120992=CARTESIAN_POINT('',(6.96762438834504,2.10403448732041,2.41416876616258));
#120993=CARTESIAN_POINT('Origin',(-5.96311194867027E-13,2.194791079001,
-9.15066633577766E-14));
#120994=CARTESIAN_POINT('',(7.28089460575536,2.01370168035532,1.79960377154688));
#120995=CARTESIAN_POINT('Origin',(-0.187001519079321,2.01785800852069,-0.0469009978311266));
#120996=CARTESIAN_POINT('',(7.39645882446895,2.10403448602304,1.24193271243861));
#120997=CARTESIAN_POINT('Origin',(-0.174359959711083,1.87510632648327,-0.0658981560518858));
#120998=CARTESIAN_POINT('Origin',(-0.188874785710973,2.01789494957119,-0.0177036690202756));
#120999=CARTESIAN_POINT('Ctrl Pts',(7.038812482,2.233426833,1.737129483));
#121000=CARTESIAN_POINT('Ctrl Pts',(7.133058978,2.169174758,1.355244646));
#121001=CARTESIAN_POINT('Ctrl Pts',(7.185436205,2.104034486,0.965404863000001));
#121002=CARTESIAN_POINT('Ctrl Pts',(7.218678946,2.233426833,2.034864682));
#121003=CARTESIAN_POINT('Ctrl Pts',(7.329078814,2.169174758,1.643221342));
#121004=CARTESIAN_POINT('Ctrl Pts',(7.39645882600001,2.104034486,1.241932705));
#121005=CARTESIAN_POINT('',(7.29094751435517,2.10403448477417,1.10366879156288));
#121006=CARTESIAN_POINT('Ctrl Pts',(7.18437825902062,2.10273945758871,0.973279075776289));
#121007=CARTESIAN_POINT('Ctrl Pts',(7.18490723201031,2.10338697179435,0.969341969388144));
#121008=CARTESIAN_POINT('Ctrl Pts',(7.185436205,2.104034486,0.965404863));
#121009=CARTESIAN_POINT('Ctrl Pts',(7.201349021,2.123513315,0.846966964));
#121010=CARTESIAN_POINT('Ctrl Pts',(7.213349817,2.142857143,0.728068964));
#121011=CARTESIAN_POINT('Ctrl Pts',(7.241247207,2.18782435,0.451675322));
#121012=CARTESIAN_POINT('Ctrl Pts',(7.24791272300001,2.233445087,0.173957335));
#121013=CARTESIAN_POINT('Ctrl Pts',(7.46113735175124,2.10273945758871,0.762559489829848));
#121014=CARTESIAN_POINT('Ctrl Pts',(7.46155069937562,2.10338697179435,0.758470865914925));
#121015=CARTESIAN_POINT('Ctrl Pts',(7.461964047,2.104034486,0.754382242));
#121016=CARTESIAN_POINT('Ctrl Pts',(7.474398566,2.123513315,0.631386321));
#121017=CARTESIAN_POINT('Ctrl Pts',(7.482772737,2.142857143,0.50804741));
#121018=CARTESIAN_POINT('Ctrl Pts',(7.50223956900001,2.18782435,0.221330301));
#121019=CARTESIAN_POINT('Ctrl Pts',(7.49970928,2.233445087,-0.066035765));
#121020=CARTESIAN_POINT('Ctrl Pts',(7.24779704645756,2.23266407511293,0.178711969599128));
#121021=CARTESIAN_POINT('Ctrl Pts',(7.28939373424232,2.22584946942467,0.179631082645235));
#121022=CARTESIAN_POINT('Ctrl Pts',(7.33104270738621,2.21920106891639,0.180611530318155));
#121023=CARTESIAN_POINT('Ctrl Pts',(7.4143359909464,2.20622738129719,0.182681326636278));
#121024=CARTESIAN_POINT('Ctrl Pts',(7.45602982682077,2.19989438512088,0.183771913550348));
#121025=CARTESIAN_POINT('Ctrl Pts',(7.49772015495655,2.19371102281662,0.184912080174598));
#121026=CARTESIAN_POINT('',(7.32370012505434,2.10403448732041,0.859893560554172));
#121027=CARTESIAN_POINT('Ctrl Pts',(7.247680448,2.233426833,0.183379743));
#121028=CARTESIAN_POINT('Ctrl Pts',(7.257629561,2.169174758,-0.209837049));
#121029=CARTESIAN_POINT('Ctrl Pts',(7.224978208,2.104034486,-0.601822151));
#121030=CARTESIAN_POINT('Ctrl Pts',(7.487346,2.233426833,0.435488086));
#121031=CARTESIAN_POINT('Ctrl Pts',(7.510973039,2.169174758,0.029268441));
#121032=CARTESIAN_POINT('Ctrl Pts',(7.490512549,2.104034486,-0.377123002));
#121033=CARTESIAN_POINT('',(7.35774537900773,2.10403448477417,-0.489472568867835));
#121034=CARTESIAN_POINT('Ctrl Pts',(7.22563771925764,2.10273945758871,-0.593904605882857));
#121035=CARTESIAN_POINT('Ctrl Pts',(7.22530796362882,2.10338697179435,-0.597863378441428));
#121036=CARTESIAN_POINT('Ctrl Pts',(7.224978208,2.104034486,-0.601822151));
#121037=CARTESIAN_POINT('Ctrl Pts',(7.215058343,2.123513315,-0.720911822));
#121038=CARTESIAN_POINT('Ctrl Pts',(7.201219013,2.142857143,-0.839609869));
#121039=CARTESIAN_POINT('Ctrl Pts',(7.169047714,2.18782435,-1.115538695));
#121040=CARTESIAN_POINT('Ctrl Pts',(7.115856237,2.233445087,-1.38819668));
#121041=CARTESIAN_POINT('Ctrl Pts',(7.45062785596414,2.10273945758871,-0.859192708687909));
#121042=CARTESIAN_POINT('Ctrl Pts',(7.45015260648208,2.10338697179435,-0.863274600343954));
#121043=CARTESIAN_POINT('Ctrl Pts',(7.449677357,2.104034486,-0.867356492));
#121044=CARTESIAN_POINT('Ctrl Pts',(7.435380677,2.123513315,-0.99014989));
#121045=CARTESIAN_POINT('Ctrl Pts',(7.417044844,2.142857143,-1.112405405));
#121046=CARTESIAN_POINT('Ctrl Pts',(7.37442085,2.18782435,-1.396604021));
#121047=CARTESIAN_POINT('Ctrl Pts',(7.310174507,2.233445087,-1.676707691));
#121048=CARTESIAN_POINT('',(7.44967735805002,2.10403448645287,-0.86735648699064));
#121049=CARTESIAN_POINT('',(7.36217825550271,2.19371102279854,-1.43119926446366));
#121050=CARTESIAN_POINT('Ctrl Pts',(7.44967735772419,2.10403448479508,-0.867356484214936));
#121051=CARTESIAN_POINT('Ctrl Pts',(7.44013112972914,2.11704095516576,-0.94934851233994));
#121052=CARTESIAN_POINT('Ctrl Pts',(7.42924607263757,2.12998516342571,-1.03105281584612));
#121053=CARTESIAN_POINT('Ctrl Pts',(7.41704484379483,2.14285714321645,-1.11240540636801));
#121054=CARTESIAN_POINT('Ctrl Pts',(7.40108693653606,2.15969232103061,-1.21880592696433));
#121055=CARTESIAN_POINT('Ctrl Pts',(7.38279971496218,2.17665108712091,-1.32512119247307));
#121056=CARTESIAN_POINT('Ctrl Pts',(7.36217825556157,2.19371102302331,-1.43119926485229));
#121057=CARTESIAN_POINT('Ctrl Pts',(7.11676536986912,2.2326640751513,-1.3835283379909));
#121058=CARTESIAN_POINT('Ctrl Pts',(7.15758669679708,2.22584954216184,-1.39157268591327));
#121059=CARTESIAN_POINT('Ctrl Pts',(7.19847221067012,2.21920121681727,-1.39956836349629));
#121060=CARTESIAN_POINT('Ctrl Pts',(7.28026402078548,2.20622738133191,-1.41545273276343));
#121061=CARTESIAN_POINT('Ctrl Pts',(7.32121752195779,2.19989438514916,-1.42335058539379));
#121062=CARTESIAN_POINT('Ctrl Pts',(7.36217825570581,2.19371102281618,-1.43119926341763));
#121063=CARTESIAN_POINT('',(7.33732778330786,2.10403448732041,-0.734589313430841));
#121064=CARTESIAN_POINT('Origin',(-4.32379826387219E-13,2.19479107899978,
7.35089072945172E-14));
#121065=CARTESIAN_POINT('',(7.36359498823949,2.01370168036158,-1.42389214627152));
#121066=CARTESIAN_POINT('Origin',(-0.189411173610758,2.01785802215147,0.0359537117828659));
#121067=CARTESIAN_POINT('',(7.23431823199796,2.10403448602304,-1.97854484767787));
#121068=CARTESIAN_POINT('Origin',(-0.185914974555001,1.8751063385133,0.0134043706131987));
#121069=CARTESIAN_POINT('Origin',(-0.178851690633703,2.01789495737722,0.0632390566086299));
#121070=CARTESIAN_POINT('Ctrl Pts',(7.11765493,2.233426833,-1.37894463));
#121071=CARTESIAN_POINT('Ctrl Pts',(7.042841452,2.169174758,-1.765106997));
#121072=CARTESIAN_POINT('Ctrl Pts',(6.926688259,2.104034486,-2.140908629));
#121073=CARTESIAN_POINT('Ctrl Pts',(7.405913077,2.233426833,-1.184251449));
#121074=CARTESIAN_POINT('Ctrl Pts',(7.341662513,2.169174758,-1.586053019));
#121075=CARTESIAN_POINT('Ctrl Pts',(7.23431823,2.104034486,-1.978544855));
#121076=CARTESIAN_POINT('',(7.08050324663655,2.10403448477417,-2.05972673465542));
#121077=CARTESIAN_POINT('Ctrl Pts',(6.92903438933913,2.10273945758871,-2.13331796710826));
#121078=CARTESIAN_POINT('Ctrl Pts',(6.92786132416957,2.10338697179435,-2.13711329805413));
#121079=CARTESIAN_POINT('Ctrl Pts',(6.926688259,2.104034486,-2.140908629));
#121080=CARTESIAN_POINT('Ctrl Pts',(6.891399557,2.123513315,-2.255081572));
#121081=CARTESIAN_POINT('Ctrl Pts',(6.852367211,2.142857143,-2.368029478));
#121082=CARTESIAN_POINT('Ctrl Pts',(6.761631518,2.18782435,-2.630591364));
#121083=CARTESIAN_POINT('Ctrl Pts',(6.65107022100001,2.233445087,-2.88544016));
#121084=CARTESIAN_POINT('Ctrl Pts',(7.09173528189306,2.10273945758871,-2.44077001058573));
#121085=CARTESIAN_POINT('Ctrl Pts',(7.09039365744652,2.10338697179435,-2.44465430529287));
#121086=CARTESIAN_POINT('Ctrl Pts',(7.089052033,2.104034486,-2.4485386));
#121087=CARTESIAN_POINT('Ctrl Pts',(7.048692651,2.123513315,-2.565387793));
#121088=CARTESIAN_POINT('Ctrl Pts',(7.004504177,2.142857143,-2.68084338));
#121089=CARTESIAN_POINT('Ctrl Pts',(6.901782407,2.18782435,-2.949234692));
#121090=CARTESIAN_POINT('Ctrl Pts',(6.778824099,2.233445087,-3.208978629));
#121091=CARTESIAN_POINT('',(7.08905203541496,2.10403448602284,-2.44853859249194));
#121092=CARTESIAN_POINT('',(6.88238908334387,2.19371102272824,-2.98038932157766));
#121093=CARTESIAN_POINT('Ctrl Pts',(7.08905203538081,2.10403448479508,-2.44853859255263));
#121094=CARTESIAN_POINT('Ctrl Pts',(7.06210313077159,2.11704095516578,-2.52656153578999));
#121095=CARTESIAN_POINT('Ctrl Pts',(7.03390855006303,2.1299851634255,-2.60401567259929));
#121096=CARTESIAN_POINT('Ctrl Pts',(7.00450417663004,2.14285714316195,-2.68084338096663));
#121097=CARTESIAN_POINT('Ctrl Pts',(6.96604638994939,2.15969232088389,-2.78132583779706));
#121098=CARTESIAN_POINT('Ctrl Pts',(6.92533207396718,2.1766510870693,-2.88122430014084));
#121099=CARTESIAN_POINT('Ctrl Pts',(6.88238908322556,2.19371102292877,-2.98038932185199));
#121100=CARTESIAN_POINT('Ctrl Pts',(6.65296165455413,2.23266407514811,-2.88107639833952));
#121101=CARTESIAN_POINT('Ctrl Pts',(6.69109930720342,2.22584954166836,-2.89770805379725));
#121102=CARTESIAN_POINT('Ctrl Pts',(6.72931010913872,2.21920121582914,-2.91430597519197));
#121103=CARTESIAN_POINT('Ctrl Pts',(6.80577491209313,2.20622739563285,-2.94740175930617));
#121104=CARTESIAN_POINT('Ctrl Pts',(6.84407304226061,2.1998944142384,-2.96391871576311));
#121105=CARTESIAN_POINT('Ctrl Pts',(6.88238908369198,2.19371102274336,-2.98038932077352));
#121106=CARTESIAN_POINT('',(7.00787014852359,2.1040344873204,-2.2947236067932));
#121107=CARTESIAN_POINT('Origin',(-9.86190296092815E-13,2.19479107899967,
4.562322741819E-13));
#121108=CARTESIAN_POINT('',(6.88534350783936,2.01370168036146,-2.97355759565002));
#121109=CARTESIAN_POINT('Origin',(-0.177253920966249,2.01785798996329,0.0758309605004354));
#121110=CARTESIAN_POINT('',(6.63985523530347,2.10403448602304,-3.48745214416206));
#121111=CARTESIAN_POINT('Origin',(-0.178686657155458,1.87510628692599,0.0530570999994617));
#121112=CARTESIAN_POINT('Origin',(-0.161075815931262,2.01789495313179,0.100208434369154));
#121113=CARTESIAN_POINT('Ctrl Pts',(6.654815779,2.233426833,-2.876791084));
#121114=CARTESIAN_POINT('Ctrl Pts',(6.498737904,2.169174758,-3.237842504));
#121115=CARTESIAN_POINT('Ctrl Pts',(6.304514067,2.104034486,-3.579888599));
#121116=CARTESIAN_POINT('Ctrl Pts',(6.97818789,2.233426833,-2.748616702));
#121117=CARTESIAN_POINT('Ctrl Pts',(6.829064008,2.169174758,-3.127212403));
#121118=CARTESIAN_POINT('Ctrl Pts',(6.639855232,2.104034486,-3.487452151));
#121119=CARTESIAN_POINT('',(6.47218465316547,2.10403448477417,-3.53367036828643));
#121120=CARTESIAN_POINT('Ctrl Pts',(6.30843711407222,2.10273945758871,-3.5729797511861));
#121121=CARTESIAN_POINT('Ctrl Pts',(6.30647559053612,2.10338697179435,-3.57643417509305));
#121122=CARTESIAN_POINT('Ctrl Pts',(6.30451406700001,2.104034486,-3.579888599));
#121123=CARTESIAN_POINT('Ctrl Pts',(6.245506587,2.123513315,-3.683806215));
#121124=CARTESIAN_POINT('Ctrl Pts',(6.183106334,2.142857143,-3.785722661));
#121125=CARTESIAN_POINT('Ctrl Pts',(6.038048947,2.18782435,-4.022640503));
#121126=CARTESIAN_POINT('Ctrl Pts',(5.875287554,2.233445087,-4.247763666));
#121127=CARTESIAN_POINT('Ctrl Pts',(6.4012410481422,2.10273945758871,-3.90821961906406));
#121128=CARTESIAN_POINT('Ctrl Pts',(6.39909578157111,2.10338697179435,-3.91172469153203));
#121129=CARTESIAN_POINT('Ctrl Pts',(6.39695051500001,2.104034486,-3.915229764));
#121130=CARTESIAN_POINT('Ctrl Pts',(6.33241559,2.123513315,-4.020671014));
#121131=CARTESIAN_POINT('Ctrl Pts',(6.264440681,2.142857143,-4.123928098));
#121132=CARTESIAN_POINT('Ctrl Pts',(6.10642429,2.18782435,-4.363962426));
#121133=CARTESIAN_POINT('Ctrl Pts',(5.93050341,2.233445087,-4.591201292));
#121134=CARTESIAN_POINT('',(6.39695051908625,2.10403448602285,-3.91522975725624));
#121135=CARTESIAN_POINT('',(6.08078704656053,2.19371102280142,-4.39021968642618));
#121136=CARTESIAN_POINT('Ctrl Pts',(6.39695051892612,2.10403448479508,-3.91522975723856));
#121137=CARTESIAN_POINT('Ctrl Pts',(6.35385903796573,2.11704095516575,-3.98563534974328));
#121138=CARTESIAN_POINT('Ctrl Pts',(6.30967328131607,2.12998516342593,-4.055217650617));
#121139=CARTESIAN_POINT('Ctrl Pts',(6.26444067997456,2.14285714327577,-4.12392809923762));
#121140=CARTESIAN_POINT('Ctrl Pts',(6.20528125616144,2.15969232116965,-4.2137940452781));
#121141=CARTESIAN_POINT('Ctrl Pts',(6.14404360261655,2.17665108712213,-4.3026045618202));
#121142=CARTESIAN_POINT('Ctrl Pts',(6.08078704643701,2.1937110230209,-4.39021968677865));
#121143=CARTESIAN_POINT('Ctrl Pts',(5.87807284688596,2.23266407510804,-4.24390852932449));
#121144=CARTESIAN_POINT('Ctrl Pts',(5.91174353685336,2.22584954390413,-4.26834980573084));
#121145=CARTESIAN_POINT('Ctrl Pts',(5.94549291609518,2.21920122043011,-4.29277386055344));
#121146=CARTESIAN_POINT('Ctrl Pts',(6.0130554977416,2.20622738131649,-4.34153362698864));
#121147=CARTESIAN_POINT('Ctrl Pts',(6.04690766649077,2.19989438513347,-4.36589745271608));
#121148=CARTESIAN_POINT('Ctrl Pts',(6.0807870471606,2.19371102281822,-4.3902196855946));
#121149=CARTESIAN_POINT('',(6.35073229512134,2.10403448732041,-3.74755917451584));
#121150=CARTESIAN_POINT('Origin',(-9.68843061333047E-13,2.194791079,6.74807432154978E-13));
#121151=CARTESIAN_POINT('',(6.08514101776743,2.01370168035776,-4.3841827961962));
#121152=CARTESIAN_POINT('Origin',(-0.15680816817603,2.01785800931407,0.112162256881573));
#121153=CARTESIAN_POINT('',(5.7349199867538,2.10403448602304,-4.83329005408069));
#121154=CARTESIAN_POINT('Origin',(-0.163103671603423,1.87510627865103,0.0902292551797146));
#121155=CARTESIAN_POINT('Origin',(-0.135768119198344,2.01789496108694,0.13249216721638));
#121156=CARTESIAN_POINT('Ctrl Pts',(5.880804839,2.233426833,-4.240121985));
#121157=CARTESIAN_POINT('Ctrl Pts',(5.650760595,2.169174758,-4.559180094));
#121158=CARTESIAN_POINT('Ctrl Pts',(5.38754780300001,2.104034486,-4.851476957));
#121159=CARTESIAN_POINT('Ctrl Pts',(6.224170392,2.233426833,-4.184459694));
#121160=CARTESIAN_POINT('Ctrl Pts',(5.997146059,2.169174758,-4.522146811));
#121161=CARTESIAN_POINT('Ctrl Pts',(5.734919982,2.104034486,-4.83329006));
#121162=CARTESIAN_POINT('',(5.56123389752302,2.10403448477417,-4.84238350273132));
#121163=CARTESIAN_POINT('Ctrl Pts',(5.39286432943003,2.10273945758871,-4.84557297336042));
#121164=CARTESIAN_POINT('Ctrl Pts',(5.39020606621502,2.10338697179435,-4.84852496518022));
#121165=CARTESIAN_POINT('Ctrl Pts',(5.387547803,2.104034486,-4.851476957));
#121166=CARTESIAN_POINT('Ctrl Pts',(5.30758067,2.123513315,-4.940280173));
#121167=CARTESIAN_POINT('Ctrl Pts',(5.224730277,2.142857143,-5.026399659));
#121168=CARTESIAN_POINT('Ctrl Pts',(5.032133918,2.18782435,-5.22659544400001));
#121169=CARTESIAN_POINT('Ctrl Pts',(4.82478297,2.233445087,-5.411466464));
#121170=CARTESIAN_POINT('Ctrl Pts',(5.41143189778815,2.10273945758871,-5.19292522215096));
#121171=CARTESIAN_POINT('Ctrl Pts',(5.40858329939408,2.10338697179435,-5.19588717907548));
#121172=CARTESIAN_POINT('Ctrl Pts',(5.405734701,2.104034486,-5.198849136));
#121173=CARTESIAN_POINT('Ctrl Pts',(5.320041815,2.123513315,-5.28795212699999));
#121174=CARTESIAN_POINT('Ctrl Pts',(5.2314589,2.142857143,-5.374182522));
#121175=CARTESIAN_POINT('Ctrl Pts',(5.02553655899999,2.18782435,-5.574636127));
#121176=CARTESIAN_POINT('Ctrl Pts',(4.804878973,2.233445087,-5.758744486));
#121177=CARTESIAN_POINT('',(5.40573470643701,2.10403448602284,-5.19884913028904));
#121178=CARTESIAN_POINT('',(4.9948541657922,2.19371102276988,-5.59476825811766));
#121179=CARTESIAN_POINT('Ctrl Pts',(5.40573470628783,2.10403448479508,-5.19884913024064));
#121180=CARTESIAN_POINT('Ctrl Pts',(5.34851555915554,2.11704095516575,-5.25834528453067));
#121181=CARTESIAN_POINT('Ctrl Pts',(5.29040470290504,2.12998516342573,-5.31680215845702));
#121182=CARTESIAN_POINT('Ctrl Pts',(5.23145889897971,2.14285714322178,-5.37418252274678));
#121183=CARTESIAN_POINT('Ctrl Pts',(5.15436406791138,2.15969232103608,-5.44922992492733));
#121184=CARTESIAN_POINT('Ctrl Pts',(5.07546648035821,2.17665108709335,-5.52279981598171));
#121185=CARTESIAN_POINT('Ctrl Pts',(4.99485416557968,2.1937110229587,-5.59476825821744));
#121186=CARTESIAN_POINT('Ctrl Pts',(4.82833188497325,2.2326640750528,-5.40830021369509));
#121187=CARTESIAN_POINT('Ctrl Pts',(4.85596119964846,2.22584954915282,-5.43940824552606));
#121188=CARTESIAN_POINT('Ctrl Pts',(4.88367106275028,2.21920123117121,-5.47051637100757));
#121189=CARTESIAN_POINT('Ctrl Pts',(4.93917214762191,2.2062273950432,-5.53266010496482));
#121190=CARTESIAN_POINT('Ctrl Pts',(4.96699530202773,2.1998944130555,-5.56373145926826));
#121191=CARTESIAN_POINT('Ctrl Pts',(4.9948541663831,2.1937110227882,-5.59476825759091));
#121192=CARTESIAN_POINT('',(5.39664125752638,2.10403448732041,-5.02516304056509));
#121193=CARTESIAN_POINT('Origin',(2.53703308361608E-13,2.19479107899989,
-1.61762964134837E-13));
#121194=CARTESIAN_POINT('',(5.00040409668657,2.01370168037898,-5.58980848202957));
#121195=CARTESIAN_POINT('Origin',(-0.129030496864432,2.01785801116634,0.143249073428582));
#121196=CARTESIAN_POINT('',(4.56182625396996,2.10403448602304,-5.95312869231247));
#121197=CARTESIAN_POINT('Origin',(-0.139893566805733,1.87510629126109,0.123181968685396));
#121198=CARTESIAN_POINT('Origin',(-0.104112042392351,2.01789493571883,0.158580727431307));
#121199=CARTESIAN_POINT('Ctrl Pts',(4.831814,2.233426833,-5.405189494));
#121200=CARTESIAN_POINT('Ctrl Pts',(4.538560001,2.169174758,-5.667335489));
#121201=CARTESIAN_POINT('Ctrl Pts',(4.218665792,2.104034486,-5.896215645));
#121202=CARTESIAN_POINT('Ctrl Pts',(5.179117605,2.233426833,-5.424642001));
#121203=CARTESIAN_POINT('Ctrl Pts',(4.884808226,2.169174758,-5.70563066));
#121204=CARTESIAN_POINT('Ctrl Pts',(4.561826248,2.104034486,-5.953128697));
#121205=CARTESIAN_POINT('',(4.39024602614564,2.10403448477417,-5.92467216644601));
#121206=CARTESIAN_POINT('Ctrl Pts',(4.2251272029383,2.10273945758871,-5.89159258926902));
#121207=CARTESIAN_POINT('Ctrl Pts',(4.22189649746915,2.10338697179435,-5.89390411713451));
#121208=CARTESIAN_POINT('Ctrl Pts',(4.218665792,2.104034486,-5.896215645));
#121209=CARTESIAN_POINT('Ctrl Pts',(4.12147818,2.123513315,-5.965752121));
#121210=CARTESIAN_POINT('Ctrl Pts',(4.022051639,2.142857143,-6.032047796));
#121211=CARTESIAN_POINT('Ctrl Pts',(3.7909219,2.18782435,-6.186160591));
#121212=CARTESIAN_POINT('Ctrl Pts',(3.548676898,2.233445087,-6.322135104));
#121213=CARTESIAN_POINT('Ctrl Pts',(4.16859020585149,2.10273945758871,-6.2348154138769));
#121214=CARTESIAN_POINT('Ctrl Pts',(4.16517147292575,2.10338697179435,-6.23709575743844));
#121215=CARTESIAN_POINT('Ctrl Pts',(4.16175274,2.104034486,-6.239376101));
#121216=CARTESIAN_POINT('Ctrl Pts',(4.058908797,2.123513315,-6.307974476));
#121217=CARTESIAN_POINT('Ctrl Pts',(3.953859916,2.142857143,-6.373146144));
#121218=CARTESIAN_POINT('Ctrl Pts',(3.709660325,2.18782435,-6.52464603900001));
#121219=CARTESIAN_POINT('Ctrl Pts',(3.454583735,2.233445087,-6.657015188));
#121220=CARTESIAN_POINT('',(4.16175274651115,2.10403448602285,-6.23937609655172));
#121221=CARTESIAN_POINT('',(3.67536745575486,2.19371102277769,-6.53771168431448));
#121222=CARTESIAN_POINT('Ctrl Pts',(4.1617527464023,2.10403448479508,-6.23937609651201));
#121223=CARTESIAN_POINT('Ctrl Pts',(4.093081436751,2.11704095516575,-6.28518083842335));
#121224=CARTESIAN_POINT('Ctrl Pts',(4.02376268037025,2.12998516342593,-6.32977890670614));
#121225=CARTESIAN_POINT('Ctrl Pts',(3.9538599145795,2.14285714327501,-6.37314614456156));
#121226=CARTESIAN_POINT('Ctrl Pts',(3.86243454430784,2.15969232116114,-6.42986587055072));
#121227=CARTESIAN_POINT('Ctrl Pts',(3.76956618710414,2.17665108709805,-6.48475508920061));
#121228=CARTESIAN_POINT('Ctrl Pts',(3.67536745552681,2.19371102296706,-6.5377116843956));
#121229=CARTESIAN_POINT('Ctrl Pts',(3.55282349131177,2.23266407508749,-6.31980579090035));
#121230=CARTESIAN_POINT('Ctrl Pts',(3.57311955964696,2.2258495427368,-6.35612605452519));
#121231=CARTESIAN_POINT('Ctrl Pts',(3.5934942760525,2.21920121809161,-6.39246372980776));
#121232=CARTESIAN_POINT('Ctrl Pts',(3.63433866877511,2.20622739519198,-6.46508559643128));
#121233=CARTESIAN_POINT('Ctrl Pts',(3.65483191001531,2.19989441336666,-6.50141167452851));
#121234=CARTESIAN_POINT('Ctrl Pts',(3.67536745646046,2.19371102279552,-6.53771168391835));
#121235=CARTESIAN_POINT('',(4.19020927267301,2.10403448732041,-6.06779586839186));
#121236=CARTESIAN_POINT('Origin',(8.17054757185076E-13,2.194791079,-1.56038376664114E-12));
#121237=CARTESIAN_POINT('',(3.68185383757781,2.01370168038203,-6.53406093588962));
#121238=CARTESIAN_POINT('Origin',(-0.0952194678829571,2.0178580037239,0.167637656801262));
#121239=CARTESIAN_POINT('',(3.17542659582,2.10403448602304,-6.79460564966676));
#121240=CARTESIAN_POINT('Origin',(-0.110142518719101,1.87510629248459,0.150375150613581));
#121241=CARTESIAN_POINT('Origin',(-0.0675876867919295,2.01789496007953,
0.177253998031647));
#121242=CARTESIAN_POINT('Ctrl Pts',(3.556892909,2.233426833,-6.31751635));
#121243=CARTESIAN_POINT('Ctrl Pts',(3.214141385,2.169174758,-6.510492576));
#121244=CARTESIAN_POINT('Ctrl Pts',(2.852523658,2.104034486,-6.665253842));
#121245=CARTESIAN_POINT('Ctrl Pts',(3.891895034,2.233426833,-6.411174077));
#121246=CARTESIAN_POINT('Ctrl Pts',(3.54406219,2.169174758,-6.622325561));
#121247=CARTESIAN_POINT('Ctrl Pts',(3.175426589,2.104034486,-6.794605653));
#121248=CARTESIAN_POINT('',(3.01397513048093,2.10403448477417,-6.72992974437362));
#121249=CARTESIAN_POINT('Ctrl Pts',(2.85982782510034,2.10273945758871,-6.66212788310327));
#121250=CARTESIAN_POINT('Ctrl Pts',(2.85617574155017,2.10338697179435,-6.66369086255163));
#121251=CARTESIAN_POINT('Ctrl Pts',(2.852523658,2.104034486,-6.66525384200001));
#121252=CARTESIAN_POINT('Ctrl Pts',(2.742659951,2.123513315,-6.71227213));
#121253=CARTESIAN_POINT('Ctrl Pts',(2.631306337,2.142857143,-6.755644082));
#121254=CARTESIAN_POINT('Ctrl Pts',(2.372450588,2.18782435,-6.856467744));
#121255=CARTESIAN_POINT('Ctrl Pts',(2.106638638,2.233445087,-6.937187734));
#121256=CARTESIAN_POINT('Ctrl Pts',(2.73082986964227,2.10273945758871,-6.98517256627893));
#121257=CARTESIAN_POINT('Ctrl Pts',(2.72700085832114,2.10338697179435,-6.98666467013946));
#121258=CARTESIAN_POINT('Ctrl Pts',(2.723171847,2.104034486,-6.98815677400001));
#121259=CARTESIAN_POINT('Ctrl Pts',(2.607985715,2.123513315,-7.033042949));
#121260=CARTESIAN_POINT('Ctrl Pts',(2.491382836,2.142857143,-7.074108535));
#121261=CARTESIAN_POINT('Ctrl Pts',(2.220324497,2.18782435,-7.169570753));
#121262=CARTESIAN_POINT('Ctrl Pts',(1.942756002,2.233445087,-7.244011259));
#121263=CARTESIAN_POINT('',(2.72317185035002,2.10403448644945,-6.98815677381845));
#121264=CARTESIAN_POINT('',(2.18402464846601,2.19371102276864,-7.17495897777774));
#121265=CARTESIAN_POINT('Ctrl Pts',(2.72317184977156,2.1040344855469,-6.98815677272572));
#121266=CARTESIAN_POINT('Ctrl Pts',(2.6462593728704,2.11704095566462,-7.0181283226553));
#121267=CARTESIAN_POINT('Ctrl Pts',(2.56897398538449,2.12998516367377,-7.04678222845144));
#121268=CARTESIAN_POINT('Ctrl Pts',(2.4913828346596,2.14285714322954,-7.07410853538889));
#121269=CARTESIAN_POINT('Ctrl Pts',(2.38990187464735,2.15969232105421,-7.10984843377403));
#121270=CARTESIAN_POINT('Ctrl Pts',(2.28740516825367,2.17665108710236,-7.14349042110731));
#121271=CARTESIAN_POINT('Ctrl Pts',(2.18402464850465,2.19371102292762,-7.17495897781848));
#121272=CARTESIAN_POINT('Ctrl Pts',(2.11118901954595,2.2326640751888,-6.93580427336281));
#121273=CARTESIAN_POINT('Ctrl Pts',(2.12320280378213,2.22584953741119,-6.97563847567611));
#121274=CARTESIAN_POINT('Ctrl Pts',(2.13528965577598,2.21920120713672,-7.01550659406681));
#121275=CARTESIAN_POINT('Ctrl Pts',(2.15956758010625,2.20622738131793,-7.09521095647696));
#121276=CARTESIAN_POINT('Ctrl Pts',(2.17177269769327,2.19989438511491,-7.13509328890588));
#121277=CARTESIAN_POINT('Ctrl Pts',(2.18402464940508,2.19371102278408,-7.17495897749153));
#121278=CARTESIAN_POINT('',(2.78784776000761,2.10403448732041,-6.82670530493409));
#121279=CARTESIAN_POINT('Origin',(1.07444435293313E-13,2.19479107900022,
-2.87096735274162E-13));
#121280=CARTESIAN_POINT('',(2.1911441852037,2.01370168036753,-7.1727879625103));
#121281=CARTESIAN_POINT('Origin',(-0.0569562509952645,2.01785797429459,
0.184188081689782));
#121282=CARTESIAN_POINT('',(1.64054751841348,2.10403448602304,-7.31837439837307));
#121283=CARTESIAN_POINT('Origin',(-0.0752411761825214,1.87510627598791,
0.17053664232371));
#121284=CARTESIAN_POINT('Origin',(-0.0279031774344973,2.01789493616642,
0.187639359023223));
#121285=CARTESIAN_POINT('Ctrl Pts',(2.115655458,2.233426833,-6.934443163));
#121286=CARTESIAN_POINT('Ctrl Pts',(1.739433091,2.169174758,-7.049226266));
#121287=CARTESIAN_POINT('Ctrl Pts',(1.353000687,2.104034486,-7.122632178));
#121288=CARTESIAN_POINT('Ctrl Pts',(2.422691778,2.233426833,-7.097926778));
#121289=CARTESIAN_POINT('Ctrl Pts',(2.037599744,2.169174758,-7.229367878));
#121290=CARTESIAN_POINT('Ctrl Pts',(1.640547511,2.104034486,-7.3183744));
#121291=CARTESIAN_POINT('',(1.49677410648981,2.10403448477417,-7.22050328744741));
#121292=CARTESIAN_POINT('Ctrl Pts',(1.36080607551578,2.10273945758871,-7.12114948230861));
#121293=CARTESIAN_POINT('Ctrl Pts',(1.35690338125789,2.10338697179435,-7.12189083015431));
#121294=CARTESIAN_POINT('Ctrl Pts',(1.353000687,2.104034486,-7.12263217800001));
#121295=CARTESIAN_POINT('Ctrl Pts',(1.23559799,2.123513315,-7.144933755));
#121296=CARTESIAN_POINT('Ctrl Pts',(1.117524075,2.142857143,-7.163353959));
#121297=CARTESIAN_POINT('Ctrl Pts',(0.843046122000001,2.18782435,-7.206174085));
#121298=CARTESIAN_POINT('Ctrl Pts',(0.566096296,2.233445087,-7.227865175));
#121299=CARTESIAN_POINT('Ctrl Pts',(1.16537896377316,2.10273945758871,-7.40891081180722));
#121300=CARTESIAN_POINT('Ctrl Pts',(1.16131871438658,2.10338697179435,-7.40954490690361));
#121301=CARTESIAN_POINT('Ctrl Pts',(1.157258465,2.104034486,-7.410179002));
#121302=CARTESIAN_POINT('Ctrl Pts',(1.03511612,2.123513315,-7.429254151));
#121303=CARTESIAN_POINT('Ctrl Pts',(0.912411464,2.142857143,-7.444293474));
#121304=CARTESIAN_POINT('Ctrl Pts',(0.627168763000001,2.18782435,-7.47925430800001));
#121305=CARTESIAN_POINT('Ctrl Pts',(0.340087157,2.233445087,-7.492285414));
#121306=CARTESIAN_POINT('',(1.15725847007385,2.10403448645287,-7.41017900172129));
#121307=CARTESIAN_POINT('',(0.59055927596526,2.19371102275364,-7.47671316452157));
#121308=CARTESIAN_POINT('Ctrl Pts',(1.15725847269504,2.10403448479508,-7.41017900061506));
#121309=CARTESIAN_POINT('Ctrl Pts',(1.07570116794104,2.11704095516578,-7.42291592453183));
#121310=CARTESIAN_POINT('Ctrl Pts',(0.994062925427622,2.12998516342565,
-7.43428584478598));
#121311=CARTESIAN_POINT('Ctrl Pts',(0.91241146271857,2.14285714320201,-7.44429347415706));
#121312=CARTESIAN_POINT('Ctrl Pts',(0.805620049540351,2.15969232098381,
-7.4573823870384));
#121313=CARTESIAN_POINT('Ctrl Pts',(0.698287626122133,2.17665108708032,
-7.46820408109766));
#121314=CARTESIAN_POINT('Ctrl Pts',(0.590559275733128,2.19371102293932,
-7.47671316449973));
#121315=CARTESIAN_POINT('Ctrl Pts',(0.570837695248524,2.23266407508929,
-7.22749225713458));
#121316=CARTESIAN_POINT('Ctrl Pts',(0.574007422813354,2.22584954795846,
-7.26897770171532));
#121317=CARTESIAN_POINT('Ctrl Pts',(0.577241217928545,2.21920122871194,
-7.31051196769929));
#121318=CARTESIAN_POINT('Ctrl Pts',(0.583817460117917,2.20622739501542,
-7.3935719730685));
#121319=CARTESIAN_POINT('Ctrl Pts',(0.58716369802571,2.19989441300601,-7.43514551846265));
#121320=CARTESIAN_POINT('Ctrl Pts',(0.590559276757404,2.19371102277163,
-7.47671316445954));
#121321=CARTESIAN_POINT('',(1.25512958399116,2.10403448732041,-7.26640558861968));
#121322=CARTESIAN_POINT('Origin',(-1.06953156183906E-13,2.19479107900022,
-1.30104260698261E-15));
#121323=CARTESIAN_POINT('',(0.597979065930106,2.01370168036969,-7.47612339603309));
#121324=CARTESIAN_POINT('Origin',(-0.0160296328144827,2.01785795518985,
0.192125553256562));
#121325=CARTESIAN_POINT('',(0.0289582635899551,2.10403448602304,-7.4999440940205));
#121326=CARTESIAN_POINT('Origin',(-0.0368217379804399,1.87510631679366,
0.18272430212099));
#121327=CARTESIAN_POINT('Origin',(0.0130861037075583,2.01789498920075,0.189250678432509));
#121328=CARTESIAN_POINT('Ctrl Pts',(0.57549231,2.233426833,-7.227123121));
#121329=CARTESIAN_POINT('Ctrl Pts',(0.183390838,2.169174758,-7.258345971));
#121330=CARTESIAN_POINT('Ctrl Pts',(-0.209787092,2.104034486,-7.246964149));
#121331=CARTESIAN_POINT('Ctrl Pts',(0.840206146,2.233426833,-7.452788313));
#121332=CARTESIAN_POINT('Ctrl Pts',(0.4358614,2.169174758,-7.498372989));
#121333=CARTESIAN_POINT('Ctrl Pts',(0.028958256,2.104034486,-7.499944094));
#121334=CARTESIAN_POINT('',(-0.0904144103515404,2.10403448477418,-7.37345412159379));
#121335=CARTESIAN_POINT('Ctrl Pts',(-0.201845453451927,2.10273945758871,
-7.24719404571963));
#121336=CARTESIAN_POINT('Ctrl Pts',(-0.205816272725964,2.10338697179435,
-7.24707909735982));
#121337=CARTESIAN_POINT('Ctrl Pts',(-0.209787092,2.104034486,-7.246964149));
#121338=CARTESIAN_POINT('Ctrl Pts',(-0.329239158,2.123513315,-7.24350621800001));
#121339=CARTESIAN_POINT('Ctrl Pts',(-0.448512371,2.142857143,-7.236113367));
#121340=CARTESIAN_POINT('Ctrl Pts',(-0.725778243,2.18782435,-7.21892773600001));
#121341=CARTESIAN_POINT('Ctrl Pts',(-1.000916079,2.233445087,-7.180575673));
#121342=CARTESIAN_POINT('Ctrl Pts',(-0.454563767573315,2.10273945758871,
-7.48621662364792));
#121343=CARTESIAN_POINT('Ctrl Pts',(-0.458665402286658,2.10338697179435,
-7.48596306032396));
#121344=CARTESIAN_POINT('Ctrl Pts',(-0.462767037,2.104034486,-7.48570949700001));
#121345=CARTESIAN_POINT('Ctrl Pts',(-0.586154355,2.123513315,-7.478081685));
#121346=CARTESIAN_POINT('Ctrl Pts',(-0.709223254,2.142857143,-7.466391523));
#121347=CARTESIAN_POINT('Ctrl Pts',(-0.995312685000001,2.18782435,-7.439216243));
#121348=CARTESIAN_POINT('Ctrl Pts',(-1.278483785,2.233445087,-7.39022863000001));
#121349=CARTESIAN_POINT('',(-0.462767031955311,2.10403448645287,-7.48570949779066));
#121350=CARTESIAN_POINT('',(-1.03051999194114,2.19371102277752,-7.42886455274631));
#121351=CARTESIAN_POINT('Ctrl Pts',(-0.462767029187143,2.10403448479507,
-7.48570949730166));
#121352=CARTESIAN_POINT('Ctrl Pts',(-0.545155631601333,2.11704095516578,
-7.48061622867985));
#121353=CARTESIAN_POINT('Ctrl Pts',(-0.627329414052753,2.12998516342569,
-7.47417051724953));
#121354=CARTESIAN_POINT('Ctrl Pts',(-0.709223255345179,2.14285714321143,
-7.46639152287222));
#121355=CARTESIAN_POINT('Ctrl Pts',(-0.816331674104039,2.15969232101307,
-7.45621742708153));
#121356=CARTESIAN_POINT('Ctrl Pts',(-0.923481069260558,2.17665108708536,
-7.44371281763971));
#121357=CARTESIAN_POINT('Ctrl Pts',(-1.030519991955,2.19371102293018,-7.42886455253598));
#121358=CARTESIAN_POINT('Ctrl Pts',(-0.996205364718836,2.23266407509814,
-7.1812307344084));
#121359=CARTESIAN_POINT('Ctrl Pts',(-1.00202789610967,2.2258495383401,-7.2224277285144));
#121360=CARTESIAN_POINT('Ctrl Pts',(-1.00779835385358,2.21920120912754,
-7.26368618337483));
#121361=CARTESIAN_POINT('Ctrl Pts',(-1.01923129090295,2.2062273932737,-7.34621787628459));
#121362=CARTESIAN_POINT('Ctrl Pts',(-1.02490037136756,2.19989440942399,
-7.38753881040581));
#121363=CARTESIAN_POINT('Ctrl Pts',(-1.03051999137907,2.19371102280297,
-7.42886455282655));
#121364=CARTESIAN_POINT('',(-0.336277056398938,2.10403448732041,-7.36633682336982));
#121365=CARTESIAN_POINT('Origin',(4.82741017299171E-14,2.19479107899978,
2.63677968348475E-13));
#121366=CARTESIAN_POINT('',(-1.02314689010353,2.01370168036372,-7.42988360835676));
#121367=CARTESIAN_POINT('Origin',(0.025646473847156,2.0178579822224,0.19107986823753));
#121368=CARTESIAN_POINT('',(-1.58398504857694,2.10403448602304,-7.3308247395824));
#121369=CARTESIAN_POINT('Origin',(0.00331945828723729,1.8751062980361,0.186367960182877));
#121370=CARTESIAN_POINT('Origin',(0.0534634732188782,2.01789498208132,0.182013091687114));
#121371=CARTESIAN_POINT('Ctrl Pts',(-0.991580219,2.233426833,-7.181870833));
#121372=CARTESIAN_POINT('Ctrl Pts',(-1.381226566,2.169174758,-7.128073485));
#121373=CARTESIAN_POINT('Ctrl Pts',(-1.76276546,2.104034486,-7.032436131));
#121374=CARTESIAN_POINT('Ctrl Pts',(-0.781566591,2.233426833,-7.459165749));
#121375=CARTESIAN_POINT('Ctrl Pts',(-1.18625734,2.169174758,-7.416762512));
#121376=CARTESIAN_POINT('Ctrl Pts',(-1.583985056,2.104034486,-7.330824738));
#121377=CARTESIAN_POINT('',(-1.67337525055052,2.10403448477417,-7.18163043623579));
#121378=CARTESIAN_POINT('Ctrl Pts',(-1.75505891355549,2.10273945758871,
-7.03436787041624));
#121379=CARTESIAN_POINT('Ctrl Pts',(-1.75891218677774,2.10338697179435,
-7.03340200070812));
#121380=CARTESIAN_POINT('Ctrl Pts',(-1.76276546,2.104034486,-7.032436131));
#121381=CARTESIAN_POINT('Ctrl Pts',(-1.87868145,2.123513315,-7.003380381));
#121382=CARTESIAN_POINT('Ctrl Pts',(-1.993576877,2.142857143,-6.970520155));
#121383=CARTESIAN_POINT('Ctrl Pts',(-2.260666024,2.18782435,-6.894132348));
#121384=CARTESIAN_POINT('Ctrl Pts',(-2.521126731,2.233445087,-6.797530434));
#121385=CARTESIAN_POINT('Ctrl Pts',(-2.05325160269057,2.10273945758871,
-7.21347526574446));
#121386=CARTESIAN_POINT('Ctrl Pts',(-2.05720283484529,2.10338697179435,
-7.21234590037223));
#121387=CARTESIAN_POINT('Ctrl Pts',(-2.061154067,2.104034486,-7.211216535));
#121388=CARTESIAN_POINT('Ctrl Pts',(-2.180016904,2.123513315,-7.177242431));
#121389=CARTESIAN_POINT('Ctrl Pts',(-2.297695481,2.142857143,-7.139369403));
#121390=CARTESIAN_POINT('Ctrl Pts',(-2.571254418,2.18782435,-7.05132869600001));
#121391=CARTESIAN_POINT('Ctrl Pts',(-2.837274247,2.233445087,-6.94261297));
#121392=CARTESIAN_POINT('',(-2.06115405937038,2.10403448602285,-7.2112165369986));
#121393=CARTESIAN_POINT('',(-2.6034132904615,2.19371102279527,-7.03365049153161));
#121394=CARTESIAN_POINT('Ctrl Pts',(-2.06115405943465,2.10403448479507,
-7.21121653697413));
#121395=CARTESIAN_POINT('Ctrl Pts',(-2.14052155993136,2.11704095516577,
-7.18853123205384));
#121396=CARTESIAN_POINT('Ctrl Pts',(-2.2193885275124,2.12998516342558,-7.16457128357355));
#121397=CARTESIAN_POINT('Ctrl Pts',(-2.29769548211535,2.14285714318334,
-7.13936940264104));
#121398=CARTESIAN_POINT('Ctrl Pts',(-2.40011263545933,2.15969232095406,
-7.10640802805374));
#121399=CARTESIAN_POINT('Ctrl Pts',(-2.50206881644122,2.17665108712062,
-7.07116181681474));
#121400=CARTESIAN_POINT('Ctrl Pts',(-2.60341329084455,2.19371102302222,
-7.03365049150481));
#121401=CARTESIAN_POINT('Ctrl Pts',(-2.51666696932107,2.23266407506185,
-6.79918284486745));
#121402=CARTESIAN_POINT('Ctrl Pts',(-2.53120951025225,2.22584953775784,
-6.8381650071174));
#121403=CARTESIAN_POINT('Ctrl Pts',(-2.54571440735249,2.21920120797771,
-6.87721838802777));
#121404=CARTESIAN_POINT('Ctrl Pts',(-2.57462194694882,2.20622738131974,
-6.95536285752602));
#121405=CARTESIAN_POINT('Ctrl Pts',(-2.58904129656605,2.19989438514245,
-6.99449912828361));
#121406=CARTESIAN_POINT('Ctrl Pts',(-2.60341328946789,2.19371102281277,
-7.03365049189911));
#121407=CARTESIAN_POINT('',(-1.91195975566783,2.10403448732041,-7.12182633510266));
#121408=CARTESIAN_POINT('Origin',(3.30247981739085E-13,2.19479107899967,
1.03172678733721E-12));
#121409=CARTESIAN_POINT('',(-2.59643163431786,2.01370168038089,-7.03623072141384));
#121410=CARTESIAN_POINT('Origin',(0.0661234049200093,2.01785800203912,0.181099350435265));
#121411=CARTESIAN_POINT('',(-3.12286297908654,2.10403448602304,-6.81892416813213));
#121412=CARTESIAN_POINT('Origin',(0.0433053581726939,1.87510630668807,0.181296946708333));
#121413=CARTESIAN_POINT('Origin',(0.0913409759321476,2.01789493322103,0.166264684052931));
#121414=CARTESIAN_POINT('Ctrl Pts',(-2.512287559,2.233426833,-6.800802248));
#121415=CARTESIAN_POINT('Ctrl Pts',(-2.881259352,2.169174758,-6.664500205));
#121416=CARTESIAN_POINT('Ctrl Pts',(-3.233318874,2.104034486,-6.489079215));
#121417=CARTESIAN_POINT('Ctrl Pts',(-2.366794143,2.233426833,-7.116760884));
#121418=CARTESIAN_POINT('Ctrl Pts',(-2.752908005,2.169174758,-6.988352463));
#121419=CARTESIAN_POINT('Ctrl Pts',(-3.122862986,2.104034486,-6.81892416500001));
#121420=CARTESIAN_POINT('',(-3.17809092309783,2.10403448477417,-6.65400169329663));
#121421=CARTESIAN_POINT('Ctrl Pts',(-3.22620776921482,2.10273945758871,
-6.49262247109658));
#121422=CARTESIAN_POINT('Ctrl Pts',(-3.22976332160741,2.10338697179435,
-6.4908508430483));
#121423=CARTESIAN_POINT('Ctrl Pts',(-3.233318874,2.104034486,-6.489079215));
#121424=CARTESIAN_POINT('Ctrl Pts',(-3.340278685,2.123513315,-6.435784261));
#121425=CARTESIAN_POINT('Ctrl Pts',(-3.445423944,2.142857143,-6.378993169));
#121426=CARTESIAN_POINT('Ctrl Pts',(-3.689847575,2.18782435,-6.246974995));
#121427=CARTESIAN_POINT('Ctrl Pts',(-3.923452299,2.233445087,-6.096640227));
#121428=CARTESIAN_POINT('Ctrl Pts',(-3.5559316742459,2.10273945758871,-6.60343982105814));
#121429=CARTESIAN_POINT('Ctrl Pts',(-3.55954774862295,2.10338697179435,
-6.60148746152907));
#121430=CARTESIAN_POINT('Ctrl Pts',(-3.563163823,2.104034486,-6.599535102));
#121431=CARTESIAN_POINT('Ctrl Pts',(-3.671944285,2.123513315,-6.540803298));
#121432=CARTESIAN_POINT('Ctrl Pts',(-3.778730021,2.142857143,-6.478518305));
#121433=CARTESIAN_POINT('Ctrl Pts',(-4.026967153,2.18782435,-6.333728855));
#121434=CARTESIAN_POINT('Ctrl Pts',(-4.263396918,2.233445087,-6.170368443));
#121435=CARTESIAN_POINT('',(-3.56316381608928,2.10403448602284,-6.59953510579737));
#121436=CARTESIAN_POINT('',(-4.0545738770561,2.19371102273927,-6.30955075083422));
#121437=CARTESIAN_POINT('Ctrl Pts',(-3.56316381603591,2.10403448479508,
-6.5995351055543));
#121438=CARTESIAN_POINT('Ctrl Pts',(-3.63579907860376,2.11704095516575,
-6.56031850441903));
#121439=CARTESIAN_POINT('Ctrl Pts',(-3.7076714997741,2.1299851634257,-6.51996465977361));
#121440=CARTESIAN_POINT('Ctrl Pts',(-3.77873002219237,2.14285714321599,
-6.47851830430452));
#121441=CARTESIAN_POINT('Ctrl Pts',(-3.87166699851752,2.15969232101281,
-6.42431088745251));
#121442=CARTESIAN_POINT('Ctrl Pts',(-3.96366260665177,2.17665108707702,
-6.36797114815556));
#121443=CARTESIAN_POINT('Ctrl Pts',(-4.05457387729845,2.19371102294006,
-6.3095507506677));
#121444=CARTESIAN_POINT('Ctrl Pts',(-3.91945202306782,2.23266407511321,
-6.09921272201927));
#121445=CARTESIAN_POINT('Ctrl Pts',(-3.94203458296659,2.22584953691232,
-6.13415729112328));
#121446=CARTESIAN_POINT('Ctrl Pts',(-3.96459568950821,2.2192012061956,-6.16917950680068));
#121447=CARTESIAN_POINT('Ctrl Pts',(-4.00962608213548,2.20622739562724,
-6.23928264841866));
#121448=CARTESIAN_POINT('Ctrl Pts',(-4.03212140082664,2.19989441423173,
-6.27440411284586));
#121449=CARTESIAN_POINT('Ctrl Pts',(-4.05457387632248,2.19371102275467,
-6.30955075130558));
#121450=CARTESIAN_POINT('',(-3.39824134130296,2.10403448732041,-6.54430716223719));
#121451=CARTESIAN_POINT('Origin',(8.03393809811759E-13,2.19479107900055,
1.33096658694321E-12));
#121452=CARTESIAN_POINT('',(-4.04831012106117,2.01370168036841,-6.31357150582532));
#121453=CARTESIAN_POINT('Origin',(0.103508509358519,2.0178580184687,0.162650835382203));
#121454=CARTESIAN_POINT('',(-4.51571930876562,2.10403448602304,-5.98817828133842));
#121455=CARTESIAN_POINT('Origin',(0.0812663913473916,1.87510629006869,0.167748984339933));
#121456=CARTESIAN_POINT('Origin',(0.124947457768929,2.01789494613023,0.14274189675082));
#121457=CARTESIAN_POINT('Ctrl Pts',(-3.915523125,2.233426833,-6.101735708));
#121458=CARTESIAN_POINT('Ctrl Pts',(-4.246567652,2.169174758,-5.889302302));
#121459=CARTESIAN_POINT('Ctrl Pts',(-4.552685891,2.104034486,-5.642300168));
#121460=CARTESIAN_POINT('Ctrl Pts',(-3.841353031,2.233426833,-6.441584191));
#121461=CARTESIAN_POINT('Ctrl Pts',(-4.190835751,2.169174758,-6.233174821));
#121462=CARTESIAN_POINT('Ctrl Pts',(-4.515719315,2.104034486,-5.988178277));
#121463=CARTESIAN_POINT('',(-4.53420259696787,2.10403448477417,-5.81523922720332));
#121464=CARTESIAN_POINT('Ctrl Pts',(-4.54650273517165,2.10273945758871,
-5.64728926211416));
#121465=CARTESIAN_POINT('Ctrl Pts',(-4.54959431308582,2.10338697179435,
-5.64479471505708));
#121466=CARTESIAN_POINT('Ctrl Pts',(-4.552685891,2.104034486,-5.64230016800001));
#121467=CARTESIAN_POINT('Ctrl Pts',(-4.645688202,2.123513315,-5.567258022));
#121468=CARTESIAN_POINT('Ctrl Pts',(-4.736166816,2.142857143,-5.489191552));
#121469=CARTESIAN_POINT('Ctrl Pts',(-4.946495953,2.18782435,-5.30771603400001));
#121470=CARTESIAN_POINT('Ctrl Pts',(-5.142321598,2.233445087,-5.110677899));
#121471=CARTESIAN_POINT('Ctrl Pts',(-4.89234033307211,2.10273945758871,
-5.6846348711734));
#121472=CARTESIAN_POINT('Ctrl Pts',(-4.89545216603606,2.10338697179435,
-5.6819508075867));
#121473=CARTESIAN_POINT('Ctrl Pts',(-4.898563999,2.104034486,-5.679266744));
#121474=CARTESIAN_POINT('Ctrl Pts',(-4.992175632,2.123513315,-5.598523472));
#121475=CARTESIAN_POINT('Ctrl Pts',(-5.083075345,2.142857143,-5.514738891));
#121476=CARTESIAN_POINT('Ctrl Pts',(-5.29438337900001,2.18782435,-5.319970893));
#121477=CARTESIAN_POINT('Ctrl Pts',(-5.490167888,2.233445087,-5.109604345));
#121478=CARTESIAN_POINT('',(-4.89856399292584,2.10403448602284,-5.67926674903035));
#121479=CARTESIAN_POINT('',(-5.31614709538626,2.19371102275033,-5.29042342922392));
#121480=CARTESIAN_POINT('Ctrl Pts',(-4.89856399296279,2.10403448479507,
-5.67926674896828));
#121481=CARTESIAN_POINT('Ctrl Pts',(-4.9610706731201,2.11704095516573,-5.62535257504612));
#121482=CARTESIAN_POINT('Ctrl Pts',(-5.02258787329021,2.12998516342565,
-5.57049173451762));
#121483=CARTESIAN_POINT('Ctrl Pts',(-5.08307534592545,2.14285714320276,
-5.51473889011978));
#121484=CARTESIAN_POINT('Ctrl Pts',(-5.16218651501869,2.15969232098375,
-5.44182011015275));
#121485=CARTESIAN_POINT('Ctrl Pts',(-5.23991993861851,2.17665108708914,
-5.36702122616938));
#121486=CARTESIAN_POINT('Ctrl Pts',(-5.31614709572608,2.19371102297335,
-5.29042342904008));
#121487=CARTESIAN_POINT('Ctrl Pts',(-5.1389678569471,2.23266407517315,-5.11405019133426));
#121488=CARTESIAN_POINT('Ctrl Pts',(-5.16853448282782,2.22584954056946,
-5.14332317738498));
#121489=CARTESIAN_POINT('Ctrl Pts',(-5.19809684655265,2.21920121356828,
-5.17267660435743));
#121490=CARTESIAN_POINT('Ctrl Pts',(-5.25714465533372,2.20622738130656,
-5.23146066835532));
#121491=CARTESIAN_POINT('Ctrl Pts',(-5.28666419622672,2.19989438510761,
-5.26092525794062));
#121492=CARTESIAN_POINT('Ctrl Pts',(-5.31614709465043,2.1937110227668,-5.29042342996282));
#121493=CARTESIAN_POINT('',(-4.72562493877461,2.10403448732041,-5.66078346119696));
#121494=CARTESIAN_POINT('Origin',(-1.26201132877313E-13,2.19479107899967,
-2.07299455379228E-13));
#121495=CARTESIAN_POINT('',(-5.31089412610488,2.01370168037457,-5.29569670366414));
#121496=CARTESIAN_POINT('Origin',(0.136053719833905,2.0178579893417,0.136596925122779));
#121497=CARTESIAN_POINT('',(-5.69742562195829,2.10403448602304,-4.87743183267503));
#121498=CARTESIAN_POINT('Origin',(0.115427610369099,1.87510627655157,0.146357328943851));
#121499=CARTESIAN_POINT('Origin',(0.152711537184925,2.01789496111607,0.11254465378285));
#121500=CARTESIAN_POINT('Ctrl Pts',(-5.135673182,2.233426833,-5.117358788));
#121501=CARTESIAN_POINT('Ctrl Pts',(-5.413311169,2.169174758,-4.83872717));
#121502=CARTESIAN_POINT('Ctrl Pts',(-5.659174375,2.104034486,-4.531693435));
#121503=CARTESIAN_POINT('Ctrl Pts',(-5.136294521,2.233426833,-5.46520618));
#121504=CARTESIAN_POINT('Ctrl Pts',(-5.432804675,2.169174758,-5.186540851));
#121505=CARTESIAN_POINT('Ctrl Pts',(-5.697425627,2.104034486,-4.877431827));
#121506=CARTESIAN_POINT('',(-5.67829999611998,2.10403448477417,-4.70456263689009));
#121507=CARTESIAN_POINT('Ctrl Pts',(-5.65420828564301,2.10273945758871,
-4.53789508252579));
#121508=CARTESIAN_POINT('Ctrl Pts',(-5.6566913303215,2.10338697179435,-4.5347942587629));
#121509=CARTESIAN_POINT('Ctrl Pts',(-5.659174375,2.104034486,-4.531693435));
#121510=CARTESIAN_POINT('Ctrl Pts',(-5.733870501,2.123513315,-4.438412986));
#121511=CARTESIAN_POINT('Ctrl Pts',(-5.805451792,2.142857143,-4.342721438));
#121512=CARTESIAN_POINT('Ctrl Pts',(-5.971851679,2.18782435,-4.12027417));
#121513=CARTESIAN_POINT('Ctrl Pts',(-6.120741654,2.233445087,-3.885745952));
#121514=CARTESIAN_POINT('Ctrl Pts',(-5.99998859553901,2.10273945758871,
-4.50002271153911));
#121515=CARTESIAN_POINT('Ctrl Pts',(-6.00245068126951,2.10338697179435,
-4.49673244776956));
#121516=CARTESIAN_POINT('Ctrl Pts',(-6.004912767,2.104034486,-4.493442184));
#121517=CARTESIAN_POINT('Ctrl Pts',(-6.078978396,2.123513315,-4.394462911));
#121518=CARTESIAN_POINT('Ctrl Pts',(-6.149741715,2.142857143,-4.293096416));
#121519=CARTESIAN_POINT('Ctrl Pts',(-6.314240122,2.18782435,-4.057457004));
#121520=CARTESIAN_POINT('Ctrl Pts',(-6.460224709,2.233445087,-3.809920827));
#121521=CARTESIAN_POINT('',(-6.00491276435706,2.10403448645287,-4.49344218835448));
#121522=CARTESIAN_POINT('',(-6.32914318402187,2.19371102275985,-4.02392178800931));
#121523=CARTESIAN_POINT('Ctrl Pts',(-6.00491276217198,2.10403448479507,
-4.49344219014995));
#121524=CARTESIAN_POINT('Ctrl Pts',(-6.05436811763821,2.11704095516577,
-4.42735141118761));
#121525=CARTESIAN_POINT('Ctrl Pts',(-6.10265362072263,2.12998516342579,
-4.36054880719136));
#121526=CARTESIAN_POINT('Ctrl Pts',(-6.14974171586987,2.14285714323779,
-4.29309641475394));
#121527=CARTESIAN_POINT('Ctrl Pts',(-6.21132792766173,2.15969232106977,
-4.20487587204554));
#121528=CARTESIAN_POINT('Ctrl Pts',(-6.27116443763095,2.17665108708656,
-4.11511535646212));
#121529=CARTESIAN_POINT('Ctrl Pts',(-6.32914318408443,2.19371102294831,
-4.02392178778338));
#121530=CARTESIAN_POINT('Ctrl Pts',(-6.11819126499426,2.23266407510997,
-3.8897603574231));
#121531=CARTESIAN_POINT('Ctrl Pts',(-6.15335945352216,2.22584954299481,
-3.9119929986438));
#121532=CARTESIAN_POINT('Ctrl Pts',(-6.18854077009955,2.21920121859506,
-3.93430511501348));
#121533=CARTESIAN_POINT('Ctrl Pts',(-6.25884486332238,2.20622739499845,
-3.97902127689778));
#121534=CARTESIAN_POINT('Ctrl Pts',(-6.29400818557493,2.19989441296563,
-4.00145111797627));
#121535=CARTESIAN_POINT('Ctrl Pts',(-6.32914318359895,2.19371102277812,
-4.02392178867561));
#121536=CARTESIAN_POINT('',(-5.83204356603735,2.10403448732041,-4.51256781591374));
#121537=CARTESIAN_POINT('Origin',(-9.6710833785707E-14,2.19479107899956,
-6.91720986045752E-14));
#121538=CARTESIAN_POINT('',(-6.32514662437653,2.01370168036548,-4.03020100929145));
#121539=CARTESIAN_POINT('Origin',(0.162236843553594,2.0178579794846,0.104155616411823));
#121540=CARTESIAN_POINT('',(-6.61272664530214,2.10403448602304,-3.53862209262939));
#121541=CARTESIAN_POINT('Origin',(0.144191659737194,1.87510624665707,0.118122165376416));
#121542=CARTESIAN_POINT('Origin',(0.17333485522942,2.01789499684262,0.0770848752727871));
#121543=CARTESIAN_POINT('Ctrl Pts',(-6.115684868,2.233426833,-3.893699859));
#121544=CARTESIAN_POINT('Ctrl Pts',(-6.326934271,2.169174758,-3.561898533));
#121545=CARTESIAN_POINT('Ctrl Pts',(-6.501046156,2.104034486,-3.209189754));
#121546=CARTESIAN_POINT('Ctrl Pts',(-6.191068588,2.233426833,-4.233281202));
#121547=CARTESIAN_POINT('Ctrl Pts',(-6.420741691,2.169174758,-3.897389996));
#121548=CARTESIAN_POINT('Ctrl Pts',(-6.61272664900001,2.104034486,-3.538622086));
#121549=CARTESIAN_POINT('',(-6.55688639900026,2.10403448477417,-3.37390592680144));
#121550=CARTESIAN_POINT('Ctrl Pts',(-6.49752934201089,2.10273945758871,
-3.21631397286633));
#121551=CARTESIAN_POINT('Ctrl Pts',(-6.49928774900544,2.10338697179435,
-3.21275186343316));
#121552=CARTESIAN_POINT('Ctrl Pts',(-6.50104615600001,2.104034486,-3.209189754));
#121553=CARTESIAN_POINT('Ctrl Pts',(-6.553943388,2.123513315,-3.102032691));
#121554=CARTESIAN_POINT('Ctrl Pts',(-6.603280295,2.142857143,-2.993190497));
#121555=CARTESIAN_POINT('Ctrl Pts',(-6.71797025700001,2.18782435,-2.740172865));
#121556=CARTESIAN_POINT('Ctrl Pts',(-6.812962634,2.233445087,-2.479120843));
#121557=CARTESIAN_POINT('Ctrl Pts',(-6.82708405989073,2.10273945758871,
-3.1049944917374));
#121558=CARTESIAN_POINT('Ctrl Pts',(-6.82878127394536,2.10338697179435,
-3.1012518768687));
#121559=CARTESIAN_POINT('Ctrl Pts',(-6.830478488,2.104034486,-3.097509262));
#121560=CARTESIAN_POINT('Ctrl Pts',(-6.881534885,2.123513315,-2.984922149));
#121561=CARTESIAN_POINT('Ctrl Pts',(-6.928852998,2.142857143,-2.870713524));
#121562=CARTESIAN_POINT('Ctrl Pts',(-7.038850015,2.18782435,-2.605220935));
#121563=CARTESIAN_POINT('Ctrl Pts',(-7.128208603,2.233445087,-2.332089646));
#121564=CARTESIAN_POINT('',(-6.83047848457064,2.10403448602288,-3.09750926910287));
#121565=CARTESIAN_POINT('',(-7.04619557178843,2.1937110227552,-2.56926603626331));
#121566=CARTESIAN_POINT('Ctrl Pts',(-6.83047848460633,2.10403448479516,
-3.09750926904382));
#121567=CARTESIAN_POINT('Ctrl Pts',(-6.86457003691931,2.11704095516579,
-3.02233221654642));
#121568=CARTESIAN_POINT('Ctrl Pts',(-6.89736606667674,2.12998516342585,
-2.94671146444441));
#121569=CARTESIAN_POINT('Ctrl Pts',(-6.92885299821979,2.14285714325619,
-2.87071352264051));
#121570=CARTESIAN_POINT('Ctrl Pts',(-6.97003454902749,2.1596923211106,-2.77131631200742));
#121571=CARTESIAN_POINT('Ctrl Pts',(-7.00917625783354,2.17665108708345,
-2.67079126633463));
#121572=CARTESIAN_POINT('Ctrl Pts',(-7.04619557181963,2.19371102294448,
-2.56926603602451));
#121573=CARTESIAN_POINT('Ctrl Pts',(-6.81133484948218,2.23266407509841,
-2.48358965246892));
#121574=CARTESIAN_POINT('Ctrl Pts',(-6.85046022076444,2.22584953695752,
-2.49774239831446));
#121575=CARTESIAN_POINT('Ctrl Pts',(-6.88961550288228,2.21920120628502,
-2.51196994118742));
#121576=CARTESIAN_POINT('Ctrl Pts',(-6.96788850361665,2.20622739510165,
-2.54052733481638));
#121577=CARTESIAN_POINT('Ctrl Pts',(-7.00705147916311,2.19989441314747,
-2.55487370363071));
#121578=CARTESIAN_POINT('Ctrl Pts',(-7.04619557151431,2.19371102277301,
-2.56926603701651));
#121579=CARTESIAN_POINT('',(-6.66576231853214,2.10403448732041,-3.15334951533061));
#121580=CARTESIAN_POINT('Origin',(-6.08020578329871E-13,2.19479107900044,
-2.8275992658422E-13));
#121581=CARTESIAN_POINT('',(-7.04364229628566,2.01370168036341,-2.57625759529277));
#121582=CARTESIAN_POINT('Origin',(0.180834155255899,2.01785799584734,0.0668443661232415));
#121583=CARTESIAN_POINT('',(-7.21882391984097,2.10403448602303,-2.0343503172764));
#121584=CARTESIAN_POINT('Origin',(0.166213305598615,1.8751063277391,0.0843635730378581));
#121585=CARTESIAN_POINT('Origin',(0.185853546571361,2.01789499323372,0.0380208633381401));
#121586=CARTESIAN_POINT('Ctrl Pts',(-6.809733927,2.233426833,-2.487975852));
#121587=CARTESIAN_POINT('Ctrl Pts',(-6.94471696,2.169174758,-2.118519479));
#121588=CARTESIAN_POINT('Ctrl Pts',(-7.03893624400001,2.104034486,-1.736627927));
#121589=CARTESIAN_POINT('Ctrl Pts',(-6.956355169,2.233426833,-2.8034127));
#121590=CARTESIAN_POINT('Ctrl Pts',(-7.108451961,2.169174758,-2.426001516));
#121591=CARTESIAN_POINT('Ctrl Pts',(-7.218823922,2.104034486,-2.03435031));
#121592=CARTESIAN_POINT('',(-7.12888008104419,2.10403448477417,-1.88548912589476));
#121593=CARTESIAN_POINT('Ctrl Pts',(-7.03703314764056,2.10273945758871,
-1.74434159666193));
#121594=CARTESIAN_POINT('Ctrl Pts',(-7.03798469582028,2.10338697179435,
-1.74048476183097));
#121595=CARTESIAN_POINT('Ctrl Pts',(-7.038936244,2.104034486,-1.736627927));
#121596=CARTESIAN_POINT('Ctrl Pts',(-7.067561167,2.123513315,-1.620604795));
#121597=CARTESIAN_POINT('Ctrl Pts',(-7.09234675,2.142857143,-1.503701295));
#121598=CARTESIAN_POINT('Ctrl Pts',(-7.149964013,2.18782435,-1.231944122));
#121599=CARTESIAN_POINT('Ctrl Pts',(-7.18661705200001,2.233445087,-0.956574799));
#121600=CARTESIAN_POINT('Ctrl Pts',(-7.33495266083656,2.10273945758871,
-1.5647801799305));
#121601=CARTESIAN_POINT('Ctrl Pts',(-7.33580564341827,2.10338697179435,
-1.56076021446525));
#121602=CARTESIAN_POINT('Ctrl Pts',(-7.33665862600001,2.104034486,-1.556740249));
#121603=CARTESIAN_POINT('Ctrl Pts',(-7.362318452,2.123513315,-1.435809744));
#121604=CARTESIAN_POINT('Ctrl Pts',(-7.383978815,2.142857143,-1.314099258));
#121605=CARTESIAN_POINT('Ctrl Pts',(-7.43433110500001,2.18782435,-1.031167631));
#121606=CARTESIAN_POINT('Ctrl Pts',(-7.462885385,2.233445087,-0.745212545));
#121607=CARTESIAN_POINT('',(-7.33665862544321,2.10403448645287,-1.55674025405362));
#121608=CARTESIAN_POINT('',(-7.43377568585854,2.19371102273836,-0.994474260409655));
#121609=CARTESIAN_POINT('Ctrl Pts',(-7.3366586242005,2.10403448479508,-1.55674025660878));
#121610=CARTESIAN_POINT('Ctrl Pts',(-7.35379229118596,2.11704095516578,
-1.47599212581495));
#121611=CARTESIAN_POINT('Ctrl Pts',(-7.36956534162783,2.12998516342583,
-1.39508916805695));
#121612=CARTESIAN_POINT('Ctrl Pts',(-7.38397881522071,2.1428571432493,-1.31409925646942));
#121613=CARTESIAN_POINT('Ctrl Pts',(-7.40283010283332,2.15969232108844,
-1.20817308110037));
#121614=CARTESIAN_POINT('Ctrl Pts',(-7.41944678640928,2.17665108707894,
-1.10158394513924));
#121615=CARTESIAN_POINT('Ctrl Pts',(-7.43377568598252,2.19371102295089,
-0.994474260071402));
#121616=CARTESIAN_POINT('Ctrl Pts',(-7.18598798653499,2.23266407510434,
-0.961289055387706));
#121617=CARTESIAN_POINT('Ctrl Pts',(-7.22724102058186,2.22584954186998,
-0.96670011587034));
#121618=CARTESIAN_POINT('Ctrl Pts',(-7.26853934111409,2.21920121629529,
-0.972177793950064));
#121619=CARTESIAN_POINT('Ctrl Pts',(-7.35112150980201,2.20622738128115,
-0.983241170647898));
#121620=CARTESIAN_POINT('Ctrl Pts',(-7.39245302161804,2.19989438508059,
-0.98883326110024));
#121621=CARTESIAN_POINT('Ctrl Pts',(-7.43377568572892,2.19371102275314,
-0.994474261375388));
#121622=CARTESIAN_POINT('',(-7.18779743318908,2.10403448732041,-1.64668409590472));
#121623=CARTESIAN_POINT('Origin',(-6.24934132220645E-13,2.19479107899956,
-4.32596666821716E-14));
#121624=CARTESIAN_POINT('',(-7.43278508299951,2.01370168036821,-1.0018512392213));
#121625=CARTESIAN_POINT('Origin',(0.190975910079478,2.01785797598412,0.0264075854711586));
#121626=CARTESIAN_POINT('',(-7.48737701144199,2.10403448602304,-0.434954581570202));
#121627=CARTESIAN_POINT('Origin',(0.18046278998651,1.87510630430002,0.046660235261801));
#121628=CARTESIAN_POINT('Origin',(0.189681877241171,2.0178949369342,-0.00282105850883979));
#121629=CARTESIAN_POINT('Ctrl Pts',(-7.185367396,2.233426833,-0.965916859000001));
#121630=CARTESIAN_POINT('Ctrl Pts',(-7.237772401,2.169174758,-0.576080809));
#121631=CARTESIAN_POINT('Ctrl Pts',(-7.247693496,2.104034486,-0.182863309));
#121632=CARTESIAN_POINT('Ctrl Pts',(-7.396370313,2.233426833,-1.242459737));
#121633=CARTESIAN_POINT('Ctrl Pts',(-7.463778918,2.169174758,-0.841175901));
#121634=CARTESIAN_POINT('Ctrl Pts',(-7.487377012,2.104034486,-0.434954574));
#121635=CARTESIAN_POINT('',(-7.36753525367957,2.10403448477417,-0.30890894914232));
#121636=CARTESIAN_POINT('Ctrl Pts',(-7.24749310390195,2.10273945758871,
-0.190805746883936));
#121637=CARTESIAN_POINT('Ctrl Pts',(-7.24759329995098,2.10338697179435,
-0.186834527941968));
#121638=CARTESIAN_POINT('Ctrl Pts',(-7.247693496,2.104034486,-0.182863309));
#121639=CARTESIAN_POINT('Ctrl Pts',(-7.250707641,2.123513315,-0.06339922));
#121640=CARTESIAN_POINT('Ctrl Pts',(-7.249782953,2.142857143,0.056099309));
#121641=CARTESIAN_POINT('Ctrl Pts',(-7.247633398,2.18782435,0.333888958));
#121642=CARTESIAN_POINT('Ctrl Pts',(-7.224233245,2.233445087,0.61069962));
#121643=CARTESIAN_POINT('Ctrl Pts',(-7.49984702782103,2.10273945758871,
0.0486015141103503));
#121644=CARTESIAN_POINT('Ctrl Pts',(-7.49981589441051,2.10338697179435,
0.0527108610551751));
#121645=CARTESIAN_POINT('Ctrl Pts',(-7.499784761,2.104034486,0.056820208));
#121646=CARTESIAN_POINT('Ctrl Pts',(-7.498848191,2.123513315,0.180439529));
#121647=CARTESIAN_POINT('Ctrl Pts',(-7.49383799,2.142857143,0.303960829));
#121648=CARTESIAN_POINT('Ctrl Pts',(-7.482191134,2.18782435,0.591101925));
#121649=CARTESIAN_POINT('Ctrl Pts',(-7.44860594,2.233445087,0.876509867));
#121650=CARTESIAN_POINT('',(-7.49978476100023,2.10403448602285,0.0568202001146768));
#121651=CARTESIAN_POINT('',(-7.4737607105466,2.19371102281187,0.626818027942189));
#121652=CARTESIAN_POINT('Ctrl Pts',(-7.49978476087731,2.10403448481428,
0.0568202003041735));
#121653=CARTESIAN_POINT('Ctrl Pts',(-7.49915939127319,2.11704095516578,
0.139363716427324));
#121654=CARTESIAN_POINT('Ctrl Pts',(-7.49717193224029,2.12998516342591,
0.221765947480715));
#121655=CARTESIAN_POINT('Ctrl Pts',(-7.49383798972033,2.14285714327001,
0.30396083051117));
#121656=CARTESIAN_POINT('Ctrl Pts',(-7.4894775475308,2.15969232121401,0.41146298053867));
#121657=CARTESIAN_POINT('Ctrl Pts',(-7.48279222887186,2.17665108720123,
0.519132217772847));
#121658=CARTESIAN_POINT('Ctrl Pts',(-7.47376071040789,2.19371102307763,
0.626818027888455));
#121659=CARTESIAN_POINT('Ctrl Pts',(-7.22463231248959,2.23266407510154,
0.605960349779416));
#121660=CARTESIAN_POINT('Ctrl Pts',(-7.26608408384316,2.22584954313154,
0.609543979184151));
#121661=CARTESIAN_POINT('Ctrl Pts',(-7.30759440260203,2.21920121886999,
0.613072283660542));
#121662=CARTESIAN_POINT('Ctrl Pts',(-7.39062361859046,2.20622746610293,
0.620020243728127));
#121663=CARTESIAN_POINT('Ctrl Pts',(-7.43219034000722,2.19989455756702,
0.623443897837998));
#121664=CARTESIAN_POINT('Ctrl Pts',(-7.47376071067519,2.19371102281321,
0.626818026360383));
#121665=CARTESIAN_POINT('',(-7.3737391284307,2.10403448732041,-0.0630215586092022));
#121666=CARTESIAN_POINT('Ctrl Pts',(-7.225021072,2.233426833,0.601307333));
#121667=CARTESIAN_POINT('Ctrl Pts',(-7.19239765,2.169174758,0.993294759999999));
#121668=CARTESIAN_POINT('Ctrl Pts',(-7.117556656,2.104034486,1.379451795));
#121669=CARTESIAN_POINT('Ctrl Pts',(-7.490539402,2.233426833,0.376589264));
#121670=CARTESIAN_POINT('Ctrl Pts',(-7.470107869,2.169174758,0.782982164));
#121671=CARTESIAN_POINT('Ctrl Pts',(-7.405828674,2.104034486,1.184779155));
#121672=CARTESIAN_POINT('',(-7.40582866653834,2.10403448559146,1.18477915314357));
#121673=CARTESIAN_POINT('Origin',(0.184637716951742,2.01789546140875,-0.043530754871078));
#121674=CARTESIAN_POINT('',(-7.26169266632994,2.10403448477417,1.28211546746747));
#121675=CARTESIAN_POINT('Origin',(1.42160588856299E-12,2.19479107900078,
3.61174848709234E-15));
#121676=CARTESIAN_POINT('',(-7.47437910004272,2.01370168037301,0.619400567520569));
#121677=CARTESIAN_POINT('Origin',(0.192188080730424,2.01785800239135,-0.0152639928727116));
#121678=CARTESIAN_POINT('Origin',(0.186271580860661,1.87510603428352,0.00677543665428812));
#121679=CARTESIAN_POINT('Ctrl Pts',(-7.11906833833695,2.10273945758871,
1.37165196852683));
#121680=CARTESIAN_POINT('Ctrl Pts',(-7.11831249716848,2.10338697179435,
1.37555188176341));
#121681=CARTESIAN_POINT('Ctrl Pts',(-7.11755665600001,2.104034486,1.379451795));
#121682=CARTESIAN_POINT('Ctrl Pts',(-7.094819084,2.123513315,1.496770832));
#121683=CARTESIAN_POINT('Ctrl Pts',(-7.068227363,2.142857143,1.613276771));
#121684=CARTESIAN_POINT('Ctrl Pts',(-7.006411501,2.18782435,1.884109762));
#121685=CARTESIAN_POINT('Ctrl Pts',(-6.92405232,2.233445087,2.149418403));
#121686=CARTESIAN_POINT('Ctrl Pts',(-7.3140568833428,2.10273945758871,1.65971065413927));
#121687=CARTESIAN_POINT('Ctrl Pts',(-7.3131430896714,2.10338697179435,1.66371723406964));
#121688=CARTESIAN_POINT('Ctrl Pts',(-7.31222929600001,2.104034486,1.667723814));
#121689=CARTESIAN_POINT('Ctrl Pts',(-7.284740122,2.123513315,1.788251649));
#121690=CARTESIAN_POINT('Ctrl Pts',(-7.253293629,2.142857143,1.907808045));
#121691=CARTESIAN_POINT('Ctrl Pts',(-7.180192223,2.18782435,2.185732212));
#121692=CARTESIAN_POINT('Ctrl Pts',(-7.086037961,2.233445087,2.457247651));
#121693=CARTESIAN_POINT('',(-7.31222929770186,2.10403448602284,1.66772380630061));
#121694=CARTESIAN_POINT('',(-7.21489297767554,2.1040344873204,1.52358779656554));
#121695=CARTESIAN_POINT('',(-7.16428099143325,2.19371102282214,2.21880099966736));
#121696=CARTESIAN_POINT('Ctrl Pts',(-7.31222929756165,2.10403448479508,
1.66772380633891));
#121697=CARTESIAN_POINT('Ctrl Pts',(-7.29387413230456,2.11704095516578,
1.74820306499409));
#121698=CARTESIAN_POINT('Ctrl Pts',(-7.27421909503796,2.12998516342588,
1.82825153285545));
#121699=CARTESIAN_POINT('Ctrl Pts',(-7.25329362833213,2.14285714326307,
1.90780804624363));
#121700=CARTESIAN_POINT('Ctrl Pts',(-7.22592534663195,2.15969232114706,
2.01185948903283));
#121701=CARTESIAN_POINT('Ctrl Pts',(-7.19625062404025,2.17665108713607,
2.11557433372164));
#121702=CARTESIAN_POINT('Ctrl Pts',(-7.16428099143183,2.19371102304242,
2.21880100004067));
#121703=CARTESIAN_POINT('Ctrl Pts',(-6.92546086042238,2.23266407511715,
2.14487572194143));
#121704=CARTESIAN_POINT('Ctrl Pts',(-6.96517311709716,2.22584954676187,
2.15728646692895));
#121705=CARTESIAN_POINT('Ctrl Pts',(-7.00495444262849,2.21920122623209,
2.169655765656));
#121706=CARTESIAN_POINT('Ctrl Pts',(-7.08454944101889,2.20622738134269,
2.19429028818731));
#121707=CARTESIAN_POINT('Ctrl Pts',(-7.12440896293867,2.19989438516438,
2.20656969562189));
#121708=CARTESIAN_POINT('Ctrl Pts',(-7.16428099173822,2.19371102283936,
2.21880099868191));
#121709=CARTESIAN_POINT('Origin',(-8.89045781438114E-14,2.19479107900022,
1.4734307524078E-13));
#121710=CARTESIAN_POINT('',(-6.97799202168079,2.10403448602303,2.74911391989858));
#121711=CARTESIAN_POINT('Origin',(0.170966029185567,2.0178949611216,-0.0822056528557094));
#121712=CARTESIAN_POINT('',(-7.16647945764014,2.01370168037485,2.21168989156015));
#121713=CARTESIAN_POINT('Origin',(0.184413421002589,2.01785795354705,-0.0562218673240203));
#121714=CARTESIAN_POINT('Origin',(0.183375927438085,1.87510628547333,-0.0334267439278485));
#121715=CARTESIAN_POINT('Ctrl Pts',(-6.926840792,2.233426833,2.140415062));
#121716=CARTESIAN_POINT('Ctrl Pts',(-6.810714378,2.169174758,2.516224969));
#121717=CARTESIAN_POINT('Ctrl Pts',(-6.654610777,2.104034486,2.877265266));
#121718=CARTESIAN_POINT('Ctrl Pts',(-7.234459193,2.233426833,1.978029369));
#121719=CARTESIAN_POINT('Ctrl Pts',(-7.127142877,2.169174758,2.370528853));
#121720=CARTESIAN_POINT('Ctrl Pts',(-6.977992019,2.104034486,2.749113927));
#121721=CARTESIAN_POINT('',(-6.81630140091813,2.10403448477417,2.81318958942943));
#121722=CARTESIAN_POINT('Ctrl Pts',(-6.65776384915911,2.10273945758871,
2.86997276216926));
#121723=CARTESIAN_POINT('Ctrl Pts',(-6.65618731307956,2.10338697179435,
2.87361901408463));
#121724=CARTESIAN_POINT('Ctrl Pts',(-6.654610777,2.104034486,2.877265266));
#121725=CARTESIAN_POINT('Ctrl Pts',(-6.60718467200001,2.123513315,2.986953543));
#121726=CARTESIAN_POINT('Ctrl Pts',(-6.556169318,2.142857143,3.095019205));
#121727=CARTESIAN_POINT('Ctrl Pts',(-6.437577588,2.18782435,3.346231687));
#121728=CARTESIAN_POINT('Ctrl Pts',(-6.300110404,2.233445087,3.58763277));
#121729=CARTESIAN_POINT('Ctrl Pts',(-6.78626956786007,2.10273945758871,
3.19321356957691));
#121730=CARTESIAN_POINT('Ctrl Pts',(-6.78451584193003,2.10338697179435,
3.19693003928845));
#121731=CARTESIAN_POINT('Ctrl Pts',(-6.782762116,2.104034486,3.200646509));
#121732=CARTESIAN_POINT('Ctrl Pts',(-6.730005702,2.123513315,3.312447111));
#121733=CARTESIAN_POINT('Ctrl Pts',(-6.673593319,2.142857143,3.422448278));
#121734=CARTESIAN_POINT('Ctrl Pts',(-6.542455503,2.18782435,3.678160091));
#121735=CARTESIAN_POINT('Ctrl Pts',(-6.392134722,2.233445087,3.923087266));
#121736=CARTESIAN_POINT('',(-6.78276211930204,2.10403448602284,3.20064650183925));
#121737=CARTESIAN_POINT('',(-6.51980745556354,2.19371102277151,3.7070353038849));
#121738=CARTESIAN_POINT('Ctrl Pts',(-6.78276211917204,2.10403448479508,
3.20064650185367));
#121739=CARTESIAN_POINT('Ctrl Pts',(-6.74753542590802,2.11704095516576,
3.27529838263622));
#121740=CARTESIAN_POINT('Ctrl Pts',(-6.71113185801136,2.12998516342577,
3.34925010984637));
#121741=CARTESIAN_POINT('Ctrl Pts',(-6.67359331829007,2.14285714323346,
3.42244827924652));
#121742=CARTESIAN_POINT('Ctrl Pts',(-6.62449690776747,2.15969232106281,
3.5181836857061));
#121743=CARTESIAN_POINT('Ctrl Pts',(-6.57322033755702,2.17665108710102,
3.61309454621992));
#121744=CARTESIAN_POINT('Ctrl Pts',(-6.51980745545966,2.19371102298407,
3.70703530422561));
#121745=CARTESIAN_POINT('Ctrl Pts',(-6.30246255588908,2.23266407512598,
3.58349908979831));
#121746=CARTESIAN_POINT('Ctrl Pts',(-6.33857882852142,2.22584946944336,
3.60415687408536));
#121747=CARTESIAN_POINT('Ctrl Pts',(-6.37477152369063,2.21920106892251,
3.62478905923907));
#121748=CARTESIAN_POINT('Ctrl Pts',(-6.44720906296556,2.20622738129678,
3.66595771293647));
#121749=CARTESIAN_POINT('Ctrl Pts',(-6.48349698183141,2.19989438510489,
3.68651865357025));
#121750=CARTESIAN_POINT('Ctrl Pts',(-6.51980745604546,2.19371102278678,
3.7070353030366));
#121751=CARTESIAN_POINT('',(-6.71868644984205,2.1040344873204,3.03895588011123));
#121752=CARTESIAN_POINT('Origin',(-9.28510740516586E-13,2.19479107900033,
5.17164436275586E-13));
#121753=CARTESIAN_POINT('',(-6.52348320100087,2.01370168036228,3.70056305468784));
#121754=CARTESIAN_POINT('Origin',(0.168016078881957,2.01785801084683,-0.0945509464054189));
#121755=CARTESIAN_POINT('',(-6.22387221623701,2.10403448602303,4.18490318070215));
#121756=CARTESIAN_POINT('Origin',(0.171902718429249,1.87510629435436,-0.0720655236513112));
#121757=CARTESIAN_POINT('Origin',(0.149296957399963,2.01789501609392,-0.117036249363178));
#121758=CARTESIAN_POINT('Ctrl Pts',(-6.304769136,2.233426833,3.579439362));
#121759=CARTESIAN_POINT('Ctrl Pts',(-6.110569671,2.169174758,3.921499296));
#121760=CARTESIAN_POINT('Ctrl Pts',(-5.880502694,2.104034486,4.240541011));
#121761=CARTESIAN_POINT('Ctrl Pts',(-6.640103713,2.233426833,3.486979019));
#121762=CARTESIAN_POINT('Ctrl Pts',(-6.450920607,2.169174758,3.847232247));
#121763=CARTESIAN_POINT('Ctrl Pts',(-6.223872212,2.104034486,4.184903187));
#121764=CARTESIAN_POINT('',(-6.05218745737027,2.10403448477406,4.21272209272149));
#121765=CARTESIAN_POINT('Ctrl Pts',(-5.8851497218288,2.10273945758871,4.23409681912444));
#121766=CARTESIAN_POINT('Ctrl Pts',(-5.8828262079144,2.10338697179435,4.23731891506222));
#121767=CARTESIAN_POINT('Ctrl Pts',(-5.880502694,2.104034486,4.240541011));
#121768=CARTESIAN_POINT('Ctrl Pts',(-5.810605648,2.123513315,4.337469627));
#121769=CARTESIAN_POINT('Ctrl Pts',(-5.737552082,2.142857143,4.43204198));
#121770=CARTESIAN_POINT('Ctrl Pts',(-5.567729703,2.18782435,4.651887538));
#121771=CARTESIAN_POINT('Ctrl Pts',(-5.381582328,2.233445087,4.85809341700001));
#121772=CARTESIAN_POINT('Ctrl Pts',(-5.94116382984549,2.10273945758871,
4.57740536707451));
#121773=CARTESIAN_POINT('Ctrl Pts',(-5.93865217392275,2.10338697179435,
4.58065794853725));
#121774=CARTESIAN_POINT('Ctrl Pts',(-5.936140518,2.104034486,4.58391053));
#121775=CARTESIAN_POINT('Ctrl Pts',(-5.860583695,2.123513315,4.681756226));
#121776=CARTESIAN_POINT('Ctrl Pts',(-5.781843203,2.142857143,4.777058632));
#121777=CARTESIAN_POINT('Ctrl Pts',(-5.598800835,2.18782435,4.998601291));
#121778=CARTESIAN_POINT('Ctrl Pts',(-5.399342368,2.233445087,5.205487681));
#121779=CARTESIAN_POINT('',(-5.93614052278719,2.10403448602287,4.58391052373464));
#121780=CARTESIAN_POINT('',(-5.57047496931209,2.19371102277816,5.02193275707079));
#121781=CARTESIAN_POINT('Ctrl Pts',(-5.93614052263355,2.1040344847952,4.58391052370258));
#121782=CARTESIAN_POINT('Ctrl Pts',(-5.88568946219855,2.11704095516577,
4.64924438689608));
#121783=CARTESIAN_POINT('Ctrl Pts',(-5.83423955417546,2.12998516342584,
4.71364147262295));
#121784=CARTESIAN_POINT('Ctrl Pts',(-5.78184320195303,2.14285714325256,
4.77705863309712));
#121785=CARTESIAN_POINT('Ctrl Pts',(-5.713314355531,2.15969232111075,4.86000152207673));
#121786=CARTESIAN_POINT('Ctrl Pts',(-5.6428335737432,2.17665108710259,4.94167047258073));
#121787=CARTESIAN_POINT('Ctrl Pts',(-5.57047496910811,2.19371102297666,
5.02193275725284));
#121788=CARTESIAN_POINT('Ctrl Pts',(-5.38476810723808,2.23266407504934,
4.85456202239123));
#121789=CARTESIAN_POINT('Ctrl Pts',(-5.41559884105151,2.22584954617779,
4.88250045523468));
#121790=CARTESIAN_POINT('Ctrl Pts',(-5.44650966311776,2.21920122513509,
4.91043027399371));
#121791=CARTESIAN_POINT('Ctrl Pts',(-5.50840428648849,2.20622739557511,
4.96620896750364));
#121792=CARTESIAN_POINT('Ctrl Pts',(-5.53942374179524,2.19989441414187,
4.99408996540044));
#121793=CARTESIAN_POINT('Ctrl Pts',(-5.57047496988285,2.19371102279481,
5.02193275643796));
#121794=CARTESIAN_POINT('',(-5.90832161085208,2.10403448732034,4.41222576400268));
#121795=CARTESIAN_POINT('Origin',(5.00034041950315E-13,2.19479107899967,
-5.16513914972094E-13));
#121796=CARTESIAN_POINT('',(-5.57545611979481,2.01370168035743,5.01640200242529));
#121797=CARTESIAN_POINT('Origin',(0.143762228792316,2.01785801671927,-0.128458831064288));
#121798=CARTESIAN_POINT('',(-5.17873106354523,2.10403448602303,5.42501101981358));
#121799=CARTESIAN_POINT('Origin',(0.152391677768917,1.87510625869217,-0.107334577256234));
#121800=CARTESIAN_POINT('Origin',(0.120647118062397,2.017894964074,-0.146394430512981));
#121801=CARTESIAN_POINT('Ctrl Pts',(-5.387893482,2.233426833,4.851093055));
#121802=CARTESIAN_POINT('Ctrl Pts',(-5.124701518,2.169174758,5.143408673));
#121803=CARTESIAN_POINT('Ctrl Pts',(-4.831428841,2.104034486,5.405533772));
#121804=CARTESIAN_POINT('Ctrl Pts',(-5.735264364,2.233426833,4.832881405));
#121805=CARTESIAN_POINT('Ctrl Pts',(-5.473060458,2.169174758,5.144043338));
#121806=CARTESIAN_POINT('Ctrl Pts',(-5.178731058,2.104034486,5.425011025));
#121807=CARTESIAN_POINT('',(-5.00507995511935,2.10403448477372,5.41527239330631));
#121808=CARTESIAN_POINT('Ctrl Pts',(-4.83735253472086,2.10273945758871,
5.40023921543883));
#121809=CARTESIAN_POINT('Ctrl Pts',(-4.83439068786043,2.10338697179435,
5.40288649371942));
#121810=CARTESIAN_POINT('Ctrl Pts',(-4.83142884100001,2.104034486,5.405533772));
#121811=CARTESIAN_POINT('Ctrl Pts',(-4.742329161,2.123513315,5.485170451));
#121812=CARTESIAN_POINT('Ctrl Pts',(-4.650653287,2.142857143,5.561827398));
#121813=CARTESIAN_POINT('Ctrl Pts',(-4.437540965,2.18782435,5.740026298));
#121814=CARTESIAN_POINT('Ctrl Pts',(-4.211417444,2.233445087,5.90139501400001));
#121815=CARTESIAN_POINT('Ctrl Pts',(-4.81825587435657,2.10273945758871,
5.74756277776072));
#121816=CARTESIAN_POINT('Ctrl Pts',(-4.81510373067829,2.10338697179435,
5.75019938388036));
#121817=CARTESIAN_POINT('Ctrl Pts',(-4.81195158700001,2.104034486,5.75283599));
#121818=CARTESIAN_POINT('Ctrl Pts',(-4.717127308,2.123513315,5.832151624));
#121819=CARTESIAN_POINT('Ctrl Pts',(-4.619740525,2.142857143,5.908299035));
#121820=CARTESIAN_POINT('Ctrl Pts',(-4.393352463,2.18782435,6.085313451));
#121821=CARTESIAN_POINT('Ctrl Pts',(-4.154082765,2.233445087,6.244485277));
#121822=CARTESIAN_POINT('',(-4.81195159151963,2.10403448645145,5.75283598686443));
#121823=CARTESIAN_POINT('',(-4.36067326450885,2.19371102278376,6.10201021640601));
#121824=CARTESIAN_POINT('Ctrl Pts',(-4.81195159287894,2.10403448479521,
5.75283598484611));
#121825=CARTESIAN_POINT('Ctrl Pts',(-4.74863520074105,2.11704095516583,
5.80579689162016));
#121826=CARTESIAN_POINT('Ctrl Pts',(-4.68454469311788,2.12998516342591,
5.85762819990044));
#121827=CARTESIAN_POINT('Ctrl Pts',(-4.61974052367469,2.14285714327157,
5.90829903559918));
#121828=CARTESIAN_POINT('Ctrl Pts',(-4.53498357418592,2.15969232115578,
5.97457108920442));
#121829=CARTESIAN_POINT('Ctrl Pts',(-4.44859418376242,2.17665108710306,
6.03917938074946));
#121830=CARTESIAN_POINT('Ctrl Pts',(-4.36067326428603,2.19371102297454,
6.10201021650341));
#121831=CARTESIAN_POINT('Ctrl Pts',(-4.21528788658319,2.23266407510532,
5.89863103047213));
#121832=CARTESIAN_POINT('Ctrl Pts',(-4.23939186650286,2.22584954934901,
5.93254395921881));
#121833=CARTESIAN_POINT('Ctrl Pts',(-4.26357591243212,2.21920123154142,
5.96646568966808));
#121834=CARTESIAN_POINT('Ctrl Pts',(-4.3120327286523,2.2062273952247,6.03424585800495));
#121835=CARTESIAN_POINT('Ctrl Pts',(-4.3363333774625,2.19989441341491,6.06814328174801));
#121836=CARTESIAN_POINT('Ctrl Pts',(-4.36067326516774,2.19371102280167,
6.10201021593574));
#121837=CARTESIAN_POINT('',(-4.82169022013528,2.10403448732032,5.57918487569773));
#121838=CARTESIAN_POINT('Origin',(2.21610924056037E-13,2.19479107900044,
-2.77555756156289E-13));
#121839=CARTESIAN_POINT('',(-4.36672690753537,2.01370168035468,6.09767956787779));
#121840=CARTESIAN_POINT('Origin',(0.112786245340395,2.01785802450165,-0.156360098587847));
#121841=CARTESIAN_POINT('',(-3.89143820237535,2.10403448602303,6.41145137387601));
#121842=CARTESIAN_POINT('Origin',(0.125755312133621,1.87510628134173,-0.137585200689151));
#121843=CARTESIAN_POINT('Origin',(0.0863561570362009,2.01789497217148,-0.168907619351457));
#121844=CARTESIAN_POINT('Ctrl Pts',(-4.219085917,2.233426833,5.895915029));
#121845=CARTESIAN_POINT('Ctrl Pts',(-3.899208018,2.169174758,6.12481797800001));
#121846=CARTESIAN_POINT('Ctrl Pts',(-3.556442745,2.104034486,6.317769781));
#121847=CARTESIAN_POINT('Ctrl Pts',(-4.562250427,2.233426833,5.952803629));
#121848=CARTESIAN_POINT('Ctrl Pts',(-4.239286085,2.169174758,6.200324679));
#121849=CARTESIAN_POINT('Ctrl Pts',(-3.891438196,2.104034486,6.411451378));
#121850=CARTESIAN_POINT('',(-3.72394047710203,2.10403448477417,6.36461057563715));
#121851=CARTESIAN_POINT('Ctrl Pts',(-3.56336611914592,2.10273945758871,
6.31387242722715));
#121852=CARTESIAN_POINT('Ctrl Pts',(-3.55990443207296,2.10338697179435,
6.31582110411357));
#121853=CARTESIAN_POINT('Ctrl Pts',(-3.556442745,2.104034486,6.317769781));
#121854=CARTESIAN_POINT('Ctrl Pts',(-3.452306635,2.123513315,6.376390802));
#121855=CARTESIAN_POINT('Ctrl Pts',(-3.346295113,2.142857143,6.431547949));
#121856=CARTESIAN_POINT('Ctrl Pts',(-3.099857743,2.18782435,6.559767807));
#121857=CARTESIAN_POINT('Ctrl Pts',(-2.84433136,2.233445087,6.66875394));
#121858=CARTESIAN_POINT('Ctrl Pts',(-3.47005162939066,2.10273945758871,
6.64897053993112));
#121859=CARTESIAN_POINT('Ctrl Pts',(-3.46640638869533,2.10338697179435,
6.65086788596556));
#121860=CARTESIAN_POINT('Ctrl Pts',(-3.462761148,2.104034486,6.652765232));
#121861=CARTESIAN_POINT('Ctrl Pts',(-3.353103291,2.123513315,6.709842094));
#121862=CARTESIAN_POINT('Ctrl Pts',(-3.241623914,2.142857143,6.763273941));
#121863=CARTESIAN_POINT('Ctrl Pts',(-2.982475812,2.18782435,6.887483117));
#121864=CARTESIAN_POINT('Ctrl Pts',(-2.71458287,2.233445087,6.991497682));
#121865=CARTESIAN_POINT('',(-3.46276115129472,2.10403448644941,6.65276523147423));
#121866=CARTESIAN_POINT('',(-2.94697132435592,2.19371102277444,6.89676445962475));
#121867=CARTESIAN_POINT('Ctrl Pts',(-3.46276115059833,2.10403448555034,
6.65276523044313));
#121868=CARTESIAN_POINT('Ctrl Pts',(-3.38954003234906,2.11704095566684,
6.69087678746824));
#121869=CARTESIAN_POINT('Ctrl Pts',(-3.31580572724131,2.12998516367491,
6.72771874325727));
#121870=CARTESIAN_POINT('Ctrl Pts',(-3.24162391269829,2.14285714324092,
6.76327394139065));
#121871=CARTESIAN_POINT('Ctrl Pts',(-3.14460200116611,2.15969232108241,
6.80977635259009));
#121872=CARTESIAN_POINT('Ctrl Pts',(-3.04634347358902,2.17665108710011,
6.85430297270454));
#121873=CARTESIAN_POINT('Ctrl Pts',(-2.94697132436812,2.19371102292601,
6.89676445959237));
#121874=CARTESIAN_POINT('Ctrl Pts',(-2.84870548848617,2.23266407512427,
6.66688660753919));
#121875=CARTESIAN_POINT('Ctrl Pts',(-2.86495564567119,2.22584955275781,
6.70518829479386));
#121876=CARTESIAN_POINT('Ctrl Pts',(-2.88128210347658,2.21920123846776,
6.74351578719786));
#121877=CARTESIAN_POINT('Ctrl Pts',(-2.91403531030025,2.20622739559012,
6.82012811461766));
#121878=CARTESIAN_POINT('Ctrl Pts',(-2.93048087823981,2.19989441416818,
6.85845695408517));
#121879=CARTESIAN_POINT('Ctrl Pts',(-2.94697132514375,2.19371102279083,
6.89676445928825));
#121880=CARTESIAN_POINT('',(-3.50960195363171,2.10403448732032,6.48526750264057));
#121881=CARTESIAN_POINT('Origin',(2.78423117894278E-13,2.19479107900055,
-7.29451221648247E-13));
#121882=CARTESIAN_POINT('',(-2.95381439771729,2.01370168036686,6.89383641367547));
#121883=CARTESIAN_POINT('Origin',(0.0765365434508686,2.01785800296307,-0.176950156993154));
#121884=CARTESIAN_POINT('',(-2.42218601520132,2.10403448602303,7.0980993866009));
#121885=CARTESIAN_POINT('Origin',(0.0932382937642756,1.87510628672111,-0.161401769551879));
#121886=CARTESIAN_POINT('Origin',(0.0480269101018865,2.01789493634255,-0.183522341499351));
#121887=CARTESIAN_POINT('Ctrl Pts',(-2.852998583,2.233426833,6.665050569));
#121888=CARTESIAN_POINT('Ctrl Pts',(-2.491391884,2.169174758,6.819837601));
#121889=CARTESIAN_POINT('Ctrl Pts',(-2.115161339,2.104034486,6.934593897));
#121890=CARTESIAN_POINT('Ctrl Pts',(-3.175910731,2.233426833,6.79437937));
#121891=CARTESIAN_POINT('Ctrl Pts',(-2.807287406,2.169174758,6.96668573000001));
#121892=CARTESIAN_POINT('Ctrl Pts',(-2.422186008,2.104034486,7.098099389));
#121893=CARTESIAN_POINT('',(-2.26867368077852,2.1040344847741,7.01634664064656));
#121894=CARTESIAN_POINT('Ctrl Pts',(-2.12276066440802,2.10273945758871,
6.93227598202678));
#121895=CARTESIAN_POINT('Ctrl Pts',(-2.11896100170401,2.10338697179436,
6.93343493951339));
#121896=CARTESIAN_POINT('Ctrl Pts',(-2.115161339,2.104034486,6.934593897));
#121897=CARTESIAN_POINT('Ctrl Pts',(-2.000858086,2.123513315,6.969458205));
#121898=CARTESIAN_POINT('Ctrl Pts',(-1.885467899,2.142857143,7.000536465));
#121899=CARTESIAN_POINT('Ctrl Pts',(-1.617228618,2.18782435,7.072781865));
#121900=CARTESIAN_POINT('Ctrl Pts',(-1.344247503,2.233445087,7.124289344));
#121901=CARTESIAN_POINT('Ctrl Pts',(-1.95959162658564,2.10273945758871,
7.23947982964323));
#121902=CARTESIAN_POINT('Ctrl Pts',(-1.95562373629282,2.10338697179436,
7.24054919782161));
#121903=CARTESIAN_POINT('Ctrl Pts',(-1.951655846,2.104034486,7.241618566));
#121904=CARTESIAN_POINT('Ctrl Pts',(-1.832291891,2.123513315,7.273787806));
#121905=CARTESIAN_POINT('Ctrl Pts',(-1.711932572,2.142857143,7.302005674));
#121906=CARTESIAN_POINT('Ctrl Pts',(-1.432141907,2.18782435,7.367601728));
#121907=CARTESIAN_POINT('Ctrl Pts',(-1.148152096,2.233445087,7.411595426));
#121908=CARTESIAN_POINT('',(-1.95165585101424,2.10403448645285,7.24161856517329));
#121909=CARTESIAN_POINT('',(-1.39547228056022,2.19371102271546,7.36903366209712));
#121910=CARTESIAN_POINT('Ctrl Pts',(-1.95165585349977,2.10403448479518,
7.241618563791));
#121911=CARTESIAN_POINT('Ctrl Pts',(-1.87195374484221,2.11704095516582,
7.26309871897641));
#121912=CARTESIAN_POINT('Ctrl Pts',(-1.79202337387582,2.12998516342552,
7.28322863460931));
#121913=CARTESIAN_POINT('Ctrl Pts',(-1.71193257096122,2.14285714316695,
7.30200567424354));
#121914=CARTESIAN_POINT('Ctrl Pts',(-1.60718233439155,2.15969232089214,
7.32656404244406));
#121915=CARTESIAN_POINT('Ctrl Pts',(-1.50164912869463,2.17665108706648,
7.3489269758674));
#121916=CARTESIAN_POINT('Ctrl Pts',(-1.39547228022281,2.19371102293117,
7.36903366220398));
#121917=CARTESIAN_POINT('Ctrl Pts',(-1.34892078850231,2.23266407510437,
7.12340597657611));
#121918=CARTESIAN_POINT('Ctrl Pts',(-1.35655729175984,2.22584955593532,
7.1643054758536));
#121919=CARTESIAN_POINT('Ctrl Pts',(-1.36426276392943,2.21920124492997,
7.20524657681581));
#121920=CARTESIAN_POINT('Ctrl Pts',(-1.37978085812241,2.20622738124446,
7.28710885303433));
#121921=CARTESIAN_POINT('Ctrl Pts',(-1.38760239028112,2.19989438504379,
7.32807699882485));
#121922=CARTESIAN_POINT('Ctrl Pts',(-1.39547228150767,2.19371102272976,
7.36903366191723));
#121923=CARTESIAN_POINT('',(-2.03340860029468,2.10403448732034,7.0881062292639));
#121924=CARTESIAN_POINT('Origin',(2.7451999007333E-13,2.19479107900011,
-1.07466119336763E-12));
#121925=CARTESIAN_POINT('',(-1.40278480996379,2.0137016803479,7.36764513069795));
#121926=CARTESIAN_POINT('Origin',(0.036708161759855,2.01785799579938,-0.189266476262751));
#121927=CARTESIAN_POINT('',(-0.839675102517359,2.10403448602304,7.4528481619308));
#121928=CARTESIAN_POINT('Origin',(0.0563618769601583,1.87510629880602,-0.177672048156901));
#121929=CARTESIAN_POINT('Origin',(0.00745225203801603,2.01789496330402,
-0.189556365350569));
#121930=CARTESIAN_POINT('Ctrl Pts',(-1.353508207,2.233426833,7.122535752));
#121931=CARTESIAN_POINT('Ctrl Pts',(-0.967081035,2.169174758,7.195969198));
#121932=CARTESIAN_POINT('Ctrl Pts',(-0.574977339,2.104034486,7.227164109));
#121933=CARTESIAN_POINT('Ctrl Pts',(-1.641068979,2.233426833,7.318257484));
#121934=CARTESIAN_POINT('Ctrl Pts',(-1.244023089,2.169174758,7.407292298));
#121935=CARTESIAN_POINT('Ctrl Pts',(-0.839675095000001,2.104034486,7.452848163));
#121936=CARTESIAN_POINT('',(-0.707326224613765,2.10403448477417,7.34000613526629));
#121937=CARTESIAN_POINT('Origin',(8.67361737988404E-16,2.19479107900078,
3.20056481317721E-13));
#121938=CARTESIAN_POINT('',(0.213837435912966,2.01370168036516,7.4969509500413));
#121939=CARTESIAN_POINT('',(-0.349293291499008,2.10403448645148,7.49186186523539));
#121940=CARTESIAN_POINT('Origin',(-0.00483675568053087,2.01785801767571,
-0.192732460490868));
#121941=CARTESIAN_POINT('Origin',(0.0168499294777102,1.87510630843667,-0.185634169925616));
#121942=CARTESIAN_POINT('Ctrl Pts',(-0.349293293799583,2.10403448479561,
7.49186186445147));
#121943=CARTESIAN_POINT('Ctrl Pts',(-0.266836977566266,2.11704095516595,
7.49570622743379));
#121944=CARTESIAN_POINT('Ctrl Pts',(-0.184447997517407,2.12998516342579,
7.49818284972337));
#121945=CARTESIAN_POINT('Ctrl Pts',(-0.102193164471361,2.14285714323922,
7.49930373802083));
#121946=CARTESIAN_POINT('Ctrl Pts',(0.00538739360841867,2.15969232107956,
7.50076974064817));
#121947=CARTESIAN_POINT('Ctrl Pts',(0.113260660248663,2.17665108710564,
7.49992332144283));
#121948=CARTESIAN_POINT('Ctrl Pts',(0.221277496359257,2.19371102298715,
7.4967350409221));
#121949=CARTESIAN_POINT('Ctrl Pts',(-0.58289727953186,2.10273945758871,
7.2265340158684));
#121950=CARTESIAN_POINT('Ctrl Pts',(-0.57893730926593,2.10338697179435,
7.2268490624342));
#121951=CARTESIAN_POINT('Ctrl Pts',(-0.574977339,2.104034486,7.227164109));
#121952=CARTESIAN_POINT('Ctrl Pts',(-0.455851638000001,2.123513315,7.236641489));
#121953=CARTESIAN_POINT('Ctrl Pts',(-0.336478302,2.142857143,7.242187677));
#121954=CARTESIAN_POINT('Ctrl Pts',(-0.0589796810000001,2.18782435,7.255080503));
#121955=CARTESIAN_POINT('Ctrl Pts',(0.218691873,2.233445087,7.246700895));
#121956=CARTESIAN_POINT('Ctrl Pts',(-0.357503297558422,2.10273945758871,
7.49147908942938));
#121957=CARTESIAN_POINT('Ctrl Pts',(-0.353398291779211,2.10338697179435,
7.49167047721469));
#121958=CARTESIAN_POINT('Ctrl Pts',(-0.349293286,2.104034486,7.491861865));
#121959=CARTESIAN_POINT('Ctrl Pts',(-0.225804558,2.123513315,7.497619283));
#121960=CARTESIAN_POINT('Ctrl Pts',(-0.102193166,2.142857143,7.499303738));
#121961=CARTESIAN_POINT('Ctrl Pts',(0.185157361,2.18782435,7.50321947));
#121962=CARTESIAN_POINT('Ctrl Pts',(0.471964993,2.233445087,7.485135206));
#121963=CARTESIAN_POINT('',(-0.462135320593557,2.10403448732041,7.35951298649177));
#121964=CARTESIAN_POINT('Ctrl Pts',(-1.153454472,3.784676613,7.410772077));
#121965=CARTESIAN_POINT('Ctrl Pts',(-0.75228298,3.720089779,7.473212677));
#121966=CARTESIAN_POINT('Ctrl Pts',(-0.346715327,3.654947264,7.491981613));
#121967=CARTESIAN_POINT('Ctrl Pts',(-1.349344274,3.784676613,7.12332577));
#121968=CARTESIAN_POINT('Ctrl Pts',(-0.963733275,3.720089779,7.196370583));
#121969=CARTESIAN_POINT('Ctrl Pts',(-0.572490449,3.654947264,7.22736153));
#121970=CARTESIAN_POINT('',(-0.595569424151332,3.69493258270807,7.47631574084745));
#121971=CARTESIAN_POINT('Ctrl Pts',(-0.595569427165582,3.69493258262019,
7.47631574064059));
#121972=CARTESIAN_POINT('Ctrl Pts',(-0.592533546838534,3.6887188543259,
7.43471764119767));
#121973=CARTESIAN_POINT('Ctrl Pts',(-0.589480876022489,3.68234999899509,
7.3931195546627));
#121974=CARTESIAN_POINT('Ctrl Pts',(-0.583346580461599,3.66929201047644,
7.31002507177171));
#121975=CARTESIAN_POINT('Ctrl Pts',(-0.580261328340382,3.66259515856785,
7.26847951121063));
#121976=CARTESIAN_POINT('Ctrl Pts',(-0.577160368804072,3.65572482644946,
7.22699010136305));
#121977=CARTESIAN_POINT('',(-1.15345447430354,3.78467661255986,7.41077207811034));
#121978=CARTESIAN_POINT('Origin',(0.0039120167552463,3.62502539284573,-0.190456296094067));
#121979=CARTESIAN_POINT('',(-1.25139938100297,3.78467661169947,7.26704892212187));
#121980=CARTESIAN_POINT('Ctrl Pts',(-2.428996377,3.654941533,7.095771741));
#121981=CARTESIAN_POINT('Ctrl Pts',(-2.143769523,3.702826767,7.193409464));
#121982=CARTESIAN_POINT('Ctrl Pts',(-1.851626136,3.75,7.267838788));
#121983=CARTESIAN_POINT('Ctrl Pts',(-1.744586692,3.767283967,7.29510921));
#121984=CARTESIAN_POINT('Ctrl Pts',(-1.636790581,3.784676613,7.319215572));
#121985=CARTESIAN_POINT('Ctrl Pts',(-2.121814945,3.654941533,6.932560951));
#121986=CARTESIAN_POINT('Ctrl Pts',(-1.843148632,3.702826767,7.01785098300001));
#121987=CARTESIAN_POINT('Ctrl Pts',(-1.558535692,3.75,7.080499029));
#121988=CARTESIAN_POINT('Ctrl Pts',(-1.454255355,3.767283967,7.103452867));
#121989=CARTESIAN_POINT('Ctrl Pts',(-1.349344274,3.784676613,7.12332577));
#121990=CARTESIAN_POINT('',(-1.63679058102371,3.78467661265395,7.31921557283982));
#121991=CARTESIAN_POINT('',(-1.49306742272831,3.78467661221161,7.2212706719866));
#121992=CARTESIAN_POINT('',(-2.18883222389661,3.69493258295591,7.17349381339529));
#121993=CARTESIAN_POINT('Ctrl Pts',(-1.63679058234593,3.78467661270495,
7.3192155712621));
#121994=CARTESIAN_POINT('Ctrl Pts',(-1.70875829796881,3.77306479305815,
7.30312148604201));
#121995=CARTESIAN_POINT('Ctrl Pts',(-1.78038472622913,3.76150355535518,
7.28598895022121));
#121996=CARTESIAN_POINT('Ctrl Pts',(-1.85162613527264,3.750000000057,7.26783878785067));
#121997=CARTESIAN_POINT('Ctrl Pts',(-1.9644656106393,3.73177948540332,7.23909069274917));
#121998=CARTESIAN_POINT('Ctrl Pts',(-2.07693173261751,3.71341418930112,
7.20763776133147));
#121999=CARTESIAN_POINT('Ctrl Pts',(-2.18883221719789,3.69493258478878,
7.17349381504735));
#122000=CARTESIAN_POINT('Ctrl Pts',(-2.11725592328059,3.6557248262931,6.93395466940919));
#122001=CARTESIAN_POINT('Ctrl Pts',(-2.12920338773,3.66259516242469,6.97380748842239));
#122002=CARTESIAN_POINT('Ctrl Pts',(-2.14114758426415,3.66929201878043,
7.01371852726311));
#122003=CARTESIAN_POINT('Ctrl Pts',(-2.16500130557688,3.68234999887378,
7.09355156358785));
#122004=CARTESIAN_POINT('Ctrl Pts',(-2.17692496583076,3.68871885430259,
7.13352087664977));
#122005=CARTESIAN_POINT('Ctrl Pts',(-2.18883223082714,3.6949325826302,7.17349381138143));
#122006=CARTESIAN_POINT('Ctrl Pts',(-2.719584283,3.784676613,6.989553729));
#122007=CARTESIAN_POINT('Ctrl Pts',(-2.341214841,3.720089779,7.136774514));
#122008=CARTESIAN_POINT('Ctrl Pts',(-1.949163901,3.654947264,7.242289699));
#122009=CARTESIAN_POINT('Ctrl Pts',(-2.849101831,3.784676613,6.66671724));
#122010=CARTESIAN_POINT('Ctrl Pts',(-2.488208678,3.720089779,6.820949271));
#122011=CARTESIAN_POINT('Ctrl Pts',(-2.11277503,3.654947264,6.93532131));
#122012=CARTESIAN_POINT('',(-2.71958428550801,3.78467661255987,6.98955372957205));
#122013=CARTESIAN_POINT('Origin',(0.0447630885962563,3.62502541599822,-0.185162737300266));
#122014=CARTESIAN_POINT('',(-2.78434306451961,3.78467661169947,6.82813548143369));
#122015=CARTESIAN_POINT('Origin',(2.03504747775529E-13,3.87542691999989,
-7.01261965163624E-13));
#122016=CARTESIAN_POINT('',(-2.18502660827734,3.87435041278773,7.17465390913854));
#122017=CARTESIAN_POINT('Origin',(0.015141183425918,3.62514700711987,-0.184193113378951));
#122018=CARTESIAN_POINT('Origin',(0.0318996984283249,4.01774292436015,-0.183314131582852));
#122019=CARTESIAN_POINT('Ctrl Pts',(-3.897588966,3.654941533,6.40771412100001));
#122020=CARTESIAN_POINT('Ctrl Pts',(-3.640019782,3.702826767,6.56438447000001));
#122021=CARTESIAN_POINT('Ctrl Pts',(-3.370706649,3.75,6.699875871));
#122022=CARTESIAN_POINT('Ctrl Pts',(-3.272032063,3.767283967,6.74951904200001));
#122023=CARTESIAN_POINT('Ctrl Pts',(-3.17193832,3.784676613,6.796234788));
#122024=CARTESIAN_POINT('Ctrl Pts',(-3.56250377,3.654941533,6.314354036));
#122025=CARTESIAN_POINT('Ctrl Pts',(-3.308687357,3.702826767,6.457555054));
#122026=CARTESIAN_POINT('Ctrl Pts',(-3.044195986,3.75,6.579921793));
#122027=CARTESIAN_POINT('Ctrl Pts',(-2.947288063,3.767283967,6.62475617200001));
#122028=CARTESIAN_POINT('Ctrl Pts',(-2.849101831,3.784676613,6.66671724));
#122029=CARTESIAN_POINT('',(-3.17193832006988,3.78467661264219,6.79623478881948));
#122030=CARTESIAN_POINT('',(-3.01052007105196,3.78467661221161,6.7314760159893));
#122031=CARTESIAN_POINT('',(-3.67974766537335,3.69493258296101,6.53524728790441));
#122032=CARTESIAN_POINT('Ctrl Pts',(-3.17193832115586,3.78467661270495,
6.79623478699001));
#122033=CARTESIAN_POINT('Ctrl Pts',(-3.23876371927838,3.77306479305815,
6.76504604108857));
#122034=CARTESIAN_POINT('Ctrl Pts',(-3.30503257260356,3.76150355535501,
6.73291648968132));
#122035=CARTESIAN_POINT('Ctrl Pts',(-3.37070664861055,3.75000000000425,
6.69987587087807));
#122036=CARTESIAN_POINT('Ctrl Pts',(-3.47472800982055,3.73177948527608,
6.6475427381026));
#122037=CARTESIAN_POINT('Ctrl Pts',(-3.57780328498725,3.71341418931372,
6.59264826720419));
#122038=CARTESIAN_POINT('Ctrl Pts',(-3.67974765917455,3.69493258479731,
6.53524729096345));
#122039=CARTESIAN_POINT('Ctrl Pts',(-3.55835094392697,3.65572482629106,
6.31669522493169));
#122040=CARTESIAN_POINT('Ctrl Pts',(-3.5785862593756,3.66259516175953,6.35304795193743));
#122041=CARTESIAN_POINT('Ctrl Pts',(-3.59883089848927,3.66929201740613,
6.3894582395044));
#122042=CARTESIAN_POINT('Ctrl Pts',(-3.63928868009484,3.68234999884861,
6.46229698630405));
#122043=CARTESIAN_POINT('Ctrl Pts',(-3.65952579260872,3.68871885429276,
6.49876860462018));
#122044=CARTESIAN_POINT('Ctrl Pts',(-3.67974767172092,3.69493258263467,
6.53524728444124));
#122045=CARTESIAN_POINT('Ctrl Pts',(-4.158549356,3.784676613,6.241511616));
#122046=CARTESIAN_POINT('Ctrl Pts',(-3.820674098,3.720089779,6.466628707));
#122047=CARTESIAN_POINT('Ctrl Pts',(-3.460471736,3.654947264,6.653956369));
#122048=CARTESIAN_POINT('Ctrl Pts',(-4.215638554,3.784676613,5.898380421));
#122049=CARTESIAN_POINT('Ctrl Pts',(-3.89633821,3.720089779,6.126587953));
#122050=CARTESIAN_POINT('Ctrl Pts',(-3.554268599,3.654947264,6.318993173));
#122051=CARTESIAN_POINT('',(-4.15854935856325,3.78467661255987,6.24151161603186));
#122052=CARTESIAN_POINT('Origin',(0.0835210236929956,3.62502542756177,-0.171210912967148));
#122053=CARTESIAN_POINT('',(-4.18709396168464,3.78467661169947,6.06994601388889));
#122054=CARTESIAN_POINT('Origin',(-1.94939550612894E-13,3.87542691999978,
3.09214459592866E-13));
#122055=CARTESIAN_POINT('',(-3.67628040958875,3.87435041277305,6.53719835590231));
#122056=CARTESIAN_POINT('Origin',(0.0543832873474687,3.62514703295402,-0.176631898517006));
#122057=CARTESIAN_POINT('Origin',(0.070561184785547,4.01774295255202,-0.172171126850401));
#122058=CARTESIAN_POINT('Ctrl Pts',(-5.183934627,3.654941533,5.42003891));
#122059=CARTESIAN_POINT('Ctrl Pts',(-4.966066761,3.702826767,5.62841615400001));
#122060=CARTESIAN_POINT('Ctrl Pts',(-4.732176666,3.75,5.818634204));
#122061=CARTESIAN_POINT('Ctrl Pts',(-4.646480852,3.767283967,5.888328864));
#122062=CARTESIAN_POINT('Ctrl Pts',(-4.558769749,3.784676613,5.95546961800001));
#122063=CARTESIAN_POINT('Ctrl Pts',(-4.836613879,3.654941533,5.400894943));
#122064=CARTESIAN_POINT('Ctrl Pts',(-4.619515538,3.702826767,5.59531102800001));
#122065=CARTESIAN_POINT('Ctrl Pts',(-4.38751306,3.75,5.771674726));
#122066=CARTESIAN_POINT('Ctrl Pts',(-4.302508856,3.767283967,5.836293242));
#122067=CARTESIAN_POINT('Ctrl Pts',(-4.215638554,3.784676613,5.898380421));
#122068=CARTESIAN_POINT('',(-4.55876974925585,3.784676612643,5.95546961878348));
#122069=CARTESIAN_POINT('',(-4.38720414758359,3.78467661221161,5.92692502239899));
#122070=CARTESIAN_POINT('',(-4.99860219645893,3.69493258290123,5.59141986218738));
#122071=CARTESIAN_POINT('Ctrl Pts',(-4.55876974991172,3.78467661270495,
5.95546961676514));
#122072=CARTESIAN_POINT('Ctrl Pts',(-4.6173281493066,3.77306479305815,5.91064456103513));
#122073=CARTESIAN_POINT('Ctrl Pts',(-4.67514076981802,3.76150355535487,
5.86502033620042));
#122074=CARTESIAN_POINT('Ctrl Pts',(-4.73217666580034,3.74999999996496,
5.81863420380783));
#122075=CARTESIAN_POINT('Ctrl Pts',(-4.82251598914285,3.73177948513261,
5.74516307240019));
#122076=CARTESIAN_POINT('Ctrl Pts',(-4.91138073268572,3.71341418923768,
5.66939386676725));
#122077=CARTESIAN_POINT('Ctrl Pts',(-4.99860219118283,3.69493258469624,
5.59141986640992));
#122078=CARTESIAN_POINT('Ctrl Pts',(-4.83306143014278,3.65572482629796,
5.404074131136));
#122079=CARTESIAN_POINT('Ctrl Pts',(-4.86063842297878,3.66259516332046,
5.43522696430087));
#122080=CARTESIAN_POINT('Ctrl Pts',(-4.88823689646622,3.66929202062442,
5.46643400910792));
#122081=CARTESIAN_POINT('Ctrl Pts',(-4.94340696137908,3.68234999884373,
5.52887258421955));
#122082=CARTESIAN_POINT('Ctrl Pts',(-4.97101126117534,3.6887188542611,5.56014113531008));
#122083=CARTESIAN_POINT('Ctrl Pts',(-4.9986022017914,3.6949325825822,5.59141985754699));
#122084=CARTESIAN_POINT('Ctrl Pts',(-5.403065283,3.784676613,5.201623357));
#122085=CARTESIAN_POINT('Ctrl Pts',(-5.121482881,3.720089779,5.494110528));
#122086=CARTESIAN_POINT('Ctrl Pts',(-4.80997176,3.654947264,5.754491434));
#122087=CARTESIAN_POINT('Ctrl Pts',(-5.385056702,3.784676613,4.854241888));
#122088=CARTESIAN_POINT('Ctrl Pts',(-5.122279297,3.720089779,5.145754191));
#122089=CARTESIAN_POINT('Ctrl Pts',(-4.829568519,3.654947264,5.407195939));
#122090=CARTESIAN_POINT('',(-5.40306528551253,3.78467661255987,5.2016233564748));
#122091=CARTESIAN_POINT('Origin',(0.118373689425329,3.62502544195215,-0.149253603691564));
#122092=CARTESIAN_POINT('',(-5.3940609980371,3.78467661169947,5.02793261655969));
#122093=CARTESIAN_POINT('Origin',(1.72171304990698E-13,3.87542691999967,
-5.76795555762288E-14));
#122094=CARTESIAN_POINT('',(-4.99563542483049,3.87435041277173,5.59407067324547));
#122095=CARTESIAN_POINT('Origin',(0.0910824517895525,3.62514697033697,-0.160811540126664));
#122096=CARTESIAN_POINT('Origin',(0.10592302656507,4.0177429632892,-0.152977109250126));
#122097=CARTESIAN_POINT('Ctrl Pts',(-6.227885267,3.654941533,4.178928703));
#122098=CARTESIAN_POINT('Ctrl Pts',(-6.05990597900001,3.702826767,4.429269354));
#122099=CARTESIAN_POINT('Ctrl Pts',(-5.872375362,3.75,4.665319669));
#122100=CARTESIAN_POINT('Ctrl Pts',(-5.803665359,3.767283967,4.751806974));
#122101=CARTESIAN_POINT('Ctrl Pts',(-5.732438171,3.784676613,4.836233308));
#122102=CARTESIAN_POINT('Ctrl Pts',(-5.884569297,3.654941533,4.234896006));
#122103=CARTESIAN_POINT('Ctrl Pts',(-5.714340306,3.702826767,4.471436477));
#122104=CARTESIAN_POINT('Ctrl Pts',(-5.5256749,3.75,4.693550565));
#122105=CARTESIAN_POINT('Ctrl Pts',(-5.456549118,3.767283967,4.774931727));
#122106=CARTESIAN_POINT('Ctrl Pts',(-5.385056702,3.784676613,4.854241888));
#122107=CARTESIAN_POINT('',(-5.73243817153119,3.78467661265427,4.8362333086525));
#122108=CARTESIAN_POINT('',(-5.55874743329835,3.78467661221161,4.84523760167313));
#122109=CARTESIAN_POINT('',(-6.08372764417876,3.69493258299157,4.38614385873408));
#122110=CARTESIAN_POINT('Ctrl Pts',(-5.73243817162459,3.78467661270495,
4.83623330659804));
#122111=CARTESIAN_POINT('Ctrl Pts',(-5.77999144574589,3.77306479305815,
4.7798679114699));
#122112=CARTESIAN_POINT('Ctrl Pts',(-5.8266445798002,3.76150355535494,4.72288235128597));
#122113=CARTESIAN_POINT('Ctrl Pts',(-5.87237536131112,3.74999999998527,
4.66531966898717));
#122114=CARTESIAN_POINT('Ctrl Pts',(-5.94480847923997,3.73177948523852,
4.57414596793933));
#122115=CARTESIAN_POINT('Ctrl Pts',(-6.01530747597372,3.71341418934238,
4.48104491092565));
#122116=CARTESIAN_POINT('Ctrl Pts',(-6.08372763978926,3.69493258484955,
4.38614386417697));
#122117=CARTESIAN_POINT('Ctrl Pts',(-5.88178333421816,3.65572482624985,
4.23876453771841));
#122118=CARTESIAN_POINT('Ctrl Pts',(-5.91541252772084,3.66259516269456,
4.26326079454881));
#122119=CARTESIAN_POINT('Ctrl Pts',(-5.94907435307606,3.6692920193845,4.28780537752084));
#122120=CARTESIAN_POINT('Ctrl Pts',(-6.01637702712757,3.68234999888808,
4.33692424506331));
#122121=CARTESIAN_POINT('Ctrl Pts',(-6.05005776801226,3.68871885432269,
4.36152764636592));
#122122=CARTESIAN_POINT('Ctrl Pts',(-6.08372764853543,3.69493258266148,
4.38614385285839));
#122123=CARTESIAN_POINT('Ctrl Pts',(-6.394939882,3.784676613,3.918512972));
#122124=CARTESIAN_POINT('Ctrl Pts',(-6.182816816,3.720089779,4.264693848));
#122125=CARTESIAN_POINT('Ctrl Pts',(-5.93456285000001,3.654947264,4.585952876));
#122126=CARTESIAN_POINT('Ctrl Pts',(-6.30267558499999,3.784676613,3.583124401));
#122127=CARTESIAN_POINT('Ctrl Pts',(-6.108708297,3.720089779,3.924310682));
#122128=CARTESIAN_POINT('Ctrl Pts',(-5.879043182,3.654947264,4.242564232));
#122129=CARTESIAN_POINT('',(-6.39493988502584,3.78467661255746,3.91851296839459));
#122130=CARTESIAN_POINT('Origin',(0.147691334653877,3.62502544960019,-0.120317321946553));
#122131=CARTESIAN_POINT('',(-6.34880773763066,3.78467661169947,3.75081867950825));
#122132=CARTESIAN_POINT('Origin',(6.5746019739521E-13,3.87542692000089,
-4.11129463806503E-13));
#122133=CARTESIAN_POINT('',(-6.08140007977474,3.87435041276949,4.38937046332155));
#122134=CARTESIAN_POINT('Origin',(0.123522468772804,3.62514698942111,-0.137471620475743));
#122135=CARTESIAN_POINT('Origin',(0.136332299683514,4.01774292398868,-0.126630361102386));
#122136=CARTESIAN_POINT('Ctrl Pts',(-6.980626913,3.654941533,2.742416435));
#122137=CARTESIAN_POINT('Ctrl Pts',(-6.87039072700001,3.702826767,3.023014843));
#122138=CARTESIAN_POINT('Ctrl Pts',(-6.737988312,3.75,3.293859971));
#122139=CARTESIAN_POINT('Ctrl Pts',(-6.689476925,3.767283967,3.39309587));
#122140=CARTESIAN_POINT('Ctrl Pts',(-6.638064156,3.784676613,3.490860104));
#122141=CARTESIAN_POINT('Ctrl Pts',(-6.657368796,3.654941533,2.870878039));
#122142=CARTESIAN_POINT('Ctrl Pts',(-6.541968873,3.702826767,3.138482526));
#122143=CARTESIAN_POINT('Ctrl Pts',(-6.405462322,3.75,3.395961195));
#122144=CARTESIAN_POINT('Ctrl Pts',(-6.355447207,3.767283967,3.49029971));
#122145=CARTESIAN_POINT('Ctrl Pts',(-6.302675585,3.784676613,3.583124401));
#122146=CARTESIAN_POINT('',(-6.63806415663382,3.78467661265215,3.49086010454012));
#122147=CARTESIAN_POINT('',(-6.47036986816281,3.78467661221161,3.53699225677551));
#122148=CARTESIAN_POINT('',(-6.8843847484949,3.69493258292739,2.9757766430664));
#122149=CARTESIAN_POINT('Ctrl Pts',(-6.63806415630895,3.78467661270495,
3.49086010249646));
#122150=CARTESIAN_POINT('Ctrl Pts',(-6.67238876700937,3.77306479305815,
3.42558995016941));
#122151=CARTESIAN_POINT('Ctrl Pts',(-6.70570096541578,3.76150355535494,
3.35990763583552));
#122152=CARTESIAN_POINT('Ctrl Pts',(-6.73798831140227,3.74999999998515,
3.29385997111107));
#122153=CARTESIAN_POINT('Ctrl Pts',(-6.78912833275206,3.73177948520444,
3.18924688147208));
#122154=CARTESIAN_POINT('Ctrl Pts',(-6.83796512675053,3.71341418927237,
3.0831672751429));
#122155=CARTESIAN_POINT('Ctrl Pts',(-6.88438474544995,3.69493258474057,
2.97577664917517));
#122156=CARTESIAN_POINT('Ctrl Pts',(-6.65547958725748,3.6557248262485,2.87525502630231));
#122157=CARTESIAN_POINT('Ctrl Pts',(-6.69358851777076,3.66259516228845,
2.89194929059024));
#122158=CARTESIAN_POINT('Ctrl Pts',(-6.73173970549951,3.66929201854781,
2.90868373622512));
#122159=CARTESIAN_POINT('Ctrl Pts',(-6.80802798946081,3.68234999883,2.94218614845776));
#122160=CARTESIAN_POINT('Ctrl Pts',(-6.84621029730883,3.68871885426788,
2.95897397227035));
#122161=CARTESIAN_POINT('Ctrl Pts',(-6.88438475141514,3.69493258260516,
2.97577663655099));
#122162=CARTESIAN_POINT('Ctrl Pts',(-7.0877942,3.784676613,2.452177274));
#122163=CARTESIAN_POINT('Ctrl Pts',(-6.955049108,3.720089779,2.835864823));
#122164=CARTESIAN_POINT('Ctrl Pts',(-6.781660377,3.654947264,3.202980258));
#122165=CARTESIAN_POINT('Ctrl Pts',(-6.925588362,3.784676613,2.144463998));
#122166=CARTESIAN_POINT('Ctrl Pts',(-6.809500887,3.720089779,2.519370767));
#122167=CARTESIAN_POINT('Ctrl Pts',(-6.65362032,3.654947264,2.879554937));
#122168=CARTESIAN_POINT('',(-7.0877942021837,3.78467661255747,2.45217726983537));
#122169=CARTESIAN_POINT('Origin',(0.170103244611084,3.62502542055922,-0.0857551768533432));
#122170=CARTESIAN_POINT('',(-7.00669128353107,3.78467661169947,2.29832062828375));
#122171=CARTESIAN_POINT('Origin',(-1.05991604382183E-12,3.87542691999911,
5.15212872365112E-13));
#122172=CARTESIAN_POINT('',(-6.88280522652425,3.87435041281037,2.97942816863292));
#122173=CARTESIAN_POINT('Origin',(0.150187169775698,3.62514698409845,-0.107704045563386));
#122174=CARTESIAN_POINT('Origin',(0.160366692848825,4.01774291427557,-0.0943623854139694));
#122175=CARTESIAN_POINT('Ctrl Pts',(-7.406962203,3.654941533,1.177671822));
#122176=CARTESIAN_POINT('Ctrl Pts',(-7.359623641,3.702826767,1.475407516));
#122177=CARTESIAN_POINT('Ctrl Pts',(-7.288540418,3.75,1.768383042));
#122178=CARTESIAN_POINT('Ctrl Pts',(-7.262495985,3.767283967,1.875727375));
#122179=CARTESIAN_POINT('Ctrl Pts',(-7.23330163800001,3.784676613,1.982258161));
#122180=CARTESIAN_POINT('Ctrl Pts',(-7.118877129,3.654941533,1.372621005));
#122181=CARTESIAN_POINT('Ctrl Pts',(-7.063702247,3.702826767,1.65877662));
#122182=CARTESIAN_POINT('Ctrl Pts',(-6.985737446,3.75,1.939580454));
#122183=CARTESIAN_POINT('Ctrl Pts',(-6.957171648,3.767283967,2.042465159));
#122184=CARTESIAN_POINT('Ctrl Pts',(-6.92558836200001,3.784676613,2.144463998));
#122185=CARTESIAN_POINT('',(-7.23330163873809,3.78467661265248,1.98225816138796));
#122186=CARTESIAN_POINT('',(-7.07944499863657,3.78467661221161,2.06336108417798));
#122187=CARTESIAN_POINT('',(-7.36313567399622,3.69493258296679,1.42626541837353));
#122188=CARTESIAN_POINT('Ctrl Pts',(-7.23330163797819,3.78467661270495,
1.98225815946538));
#122189=CARTESIAN_POINT('Ctrl Pts',(-7.25279260523575,3.77306479305815,
1.9111352104377));
#122190=CARTESIAN_POINT('Ctrl Pts',(-7.27120622711416,3.76150355535477,
1.83982737421093));
#122191=CARTESIAN_POINT('Ctrl Pts',(-7.28854041727107,3.74999999993373,
1.76838304205702));
#122192=CARTESIAN_POINT('Ctrl Pts',(-7.31599609085907,3.73177948507314,
1.65522215470338));
#122193=CARTESIAN_POINT('Ctrl Pts',(-7.3408871284668,3.71341418929527,1.54112416376592));
#122194=CARTESIAN_POINT('Ctrl Pts',(-7.36313567231283,3.69493258480758,
1.42626542509399));
#122195=CARTESIAN_POINT('Ctrl Pts',(-7.11797301180835,3.65572482627641,
1.37730178494789));
#122196=CARTESIAN_POINT('Ctrl Pts',(-7.15877975551595,3.66259516323431,
1.38541345409399));
#122197=CARTESIAN_POINT('Ctrl Pts',(-7.19963640720115,3.66929202046406,
1.39355528123289));
#122198=CARTESIAN_POINT('Ctrl Pts',(-7.28134313014978,3.68234999887737,
1.40987469711569));
#122199=CARTESIAN_POINT('Ctrl Pts',(-7.32224164272322,3.68871885430734,
1.41806196326326));
#122200=CARTESIAN_POINT('Ctrl Pts',(-7.3631356754694,3.69493258263972,1.42626541127745));
#122201=CARTESIAN_POINT('Ctrl Pts',(-7.449231138,3.784676613,0.871180493));
#122202=CARTESIAN_POINT('Ctrl Pts',(-7.402071035,3.720089779,1.274433911));
#122203=CARTESIAN_POINT('Ctrl Pts',(-7.311655002,3.654947264,1.670239842));
#122204=CARTESIAN_POINT('Ctrl Pts',(-7.224668324,3.784676613,0.605530843));
#122205=CARTESIAN_POINT('Ctrl Pts',(-7.191888783,3.720089779,0.996627876));
#122206=CARTESIAN_POINT('Ctrl Pts',(-7.117081567,3.654947264,1.381900854));
#122207=CARTESIAN_POINT('',(-7.44923113925812,3.78467661255747,0.871180488487826));
#122208=CARTESIAN_POINT('Origin',(0.184560763367131,3.6250254182926,-0.0471830310168703));
#122209=CARTESIAN_POINT('',(-7.33694973181313,3.78467661169947,0.738355659920048));
#122210=CARTESIAN_POINT('Origin',(-9.93129189996722E-13,3.87542691999967,
2.2253249590265E-13));
#122211=CARTESIAN_POINT('',(-7.36237804979258,3.87435041279178,1.43017112447896));
#122212=CARTESIAN_POINT('Origin',(0.169829105002478,3.62514697679868,-0.072900190738982));
#122213=CARTESIAN_POINT('Origin',(0.176902520092889,4.01774291269509,-0.0576821437523266));
#122214=CARTESIAN_POINT('Ctrl Pts',(-7.486956173,3.654941533,-0.442139416));
#122215=CARTESIAN_POINT('Ctrl Pts',(-7.504728734,3.702826767,-0.141188225));
#122216=CARTESIAN_POINT('Ctrl Pts',(-7.498288474,3.75,0.160218487));
#122217=CARTESIAN_POINT('Ctrl Pts',(-7.49592880400001,3.767283967,0.270651952));
#122218=CARTESIAN_POINT('Ctrl Pts',(-7.490317975,3.784676613,0.380968029));
#122219=CARTESIAN_POINT('Ctrl Pts',(-7.247514679,3.654941533,-0.189818262));
#122220=CARTESIAN_POINT('Ctrl Pts',(-7.255144754,3.702826767,0.101508163));
#122221=CARTESIAN_POINT('Ctrl Pts',(-7.23936725,3.75,0.392507087));
#122222=CARTESIAN_POINT('Ctrl Pts',(-7.23358647600001,3.767283967,0.499127207));
#122223=CARTESIAN_POINT('Ctrl Pts',(-7.224668324,3.784676613,0.605530843));
#122224=CARTESIAN_POINT('',(-7.49031797580076,3.78467661265198,0.380968029226118));
#122225=CARTESIAN_POINT('',(-7.35749314917407,3.78467661221161,0.493249440861707));
#122226=CARTESIAN_POINT('',(-7.49759455824446,3.69493258292492,-0.189936391004461));
#122227=CARTESIAN_POINT('Ctrl Pts',(-7.49031797464904,3.78467661270495,
0.380968027505726));
#122228=CARTESIAN_POINT('Ctrl Pts',(-7.49406392197607,3.77306479305815,
0.307317911724217));
#122229=CARTESIAN_POINT('Ctrl Pts',(-7.49671796648463,3.76150355535484,
0.233718828824487));
#122230=CARTESIAN_POINT('Ctrl Pts',(-7.49828847349936,3.7499999999552,0.16021848716836));
#122231=CARTESIAN_POINT('Ctrl Pts',(-7.50077600364447,3.73177948513637,
0.04380108050615));
#122232=CARTESIAN_POINT('Ctrl Pts',(-7.50055740678639,3.71341418928101,
-0.0729801998009269));
#122233=CARTESIAN_POINT('Ctrl Pts',(-7.49759455804428,3.69493258473592,
-0.189936384188764));
#122234=CARTESIAN_POINT('Ctrl Pts',(-7.24763792913635,3.65572482635196,
-0.185052557384502));
#122235=CARTESIAN_POINT('Ctrl Pts',(-7.28923440487671,3.66259516360214,
-0.185902778062423));
#122236=CARTESIAN_POINT('Ctrl Pts',(-7.33088610520975,3.66929202115375,
-0.186734274564594));
#122237=CARTESIAN_POINT('Ctrl Pts',(-7.4141907581793,3.68234999887337,-0.188360927321621));
#122238=CARTESIAN_POINT('Ctrl Pts',(-7.45589310641358,3.68871885428542,
-0.189157045999112));
#122239=CARTESIAN_POINT('Ctrl Pts',(-7.49759455815914,3.69493258260301,
-0.189936398136369));
#122240=CARTESIAN_POINT('Ctrl Pts',(-7.462350308,3.784676613,-0.750551720000001));
#122241=CARTESIAN_POINT('Ctrl Pts',(-7.502980346,3.720089779,-0.346588114));
#122242=CARTESIAN_POINT('Ctrl Pts',(-7.49976476500001,3.654947264,0.059400869));
#122243=CARTESIAN_POINT('Ctrl Pts',(-7.185930826,3.784676613,-0.961716262));
#122244=CARTESIAN_POINT('Ctrl Pts',(-7.237991953,3.720089779,-0.572716228));
#122245=CARTESIAN_POINT('Ctrl Pts',(-7.24775599,3.654947264,-0.180369377));
#122246=CARTESIAN_POINT('',(-7.46235030922085,3.78467661255987,-0.750551722266326));
#122247=CARTESIAN_POINT('Origin',(0.190388983462796,3.62502540451372,-0.0064048087139305));
#122248=CARTESIAN_POINT('',(-7.32414056605717,3.78467661169947,-0.856133999065892));
#122249=CARTESIAN_POINT('Origin',(1.04343617080005E-12,3.87542692000022,
-3.97089045672816E-14));
#122250=CARTESIAN_POINT('',(-7.49769425871509,3.87435041278221,-0.185959132095994));
#122251=CARTESIAN_POINT('Origin',(0.18153000267657,3.62514693102631,-0.0346875952443603));
#122252=CARTESIAN_POINT('Origin',(0.185166703032014,4.01774291708685,-0.0183047507880639));
#122253=CARTESIAN_POINT('Ctrl Pts',(-7.216868393,3.654941533,-2.041276707));
#122254=CARTESIAN_POINT('Ctrl Pts',(-7.298921051,3.702826767,-1.751182163));
#122255=CARTESIAN_POINT('Ctrl Pts',(-7.357424895,3.75,-1.455437707));
#122256=CARTESIAN_POINT('Ctrl Pts',(-7.37886032399999,3.767283967,-1.347078855));
#122257=CARTESIAN_POINT('Ctrl Pts',(-7.397095368,3.784676613,-1.238135744));
#122258=CARTESIAN_POINT('Ctrl Pts',(-7.037266498,3.654941533,-1.743381837));
#122259=CARTESIAN_POINT('Ctrl Pts',(-7.10734475600001,3.702826767,-1.460506703));
#122260=CARTESIAN_POINT('Ctrl Pts',(-7.154492288,3.75,-1.172919475));
#122261=CARTESIAN_POINT('Ctrl Pts',(-7.171766839,3.767283967,-1.067549379));
#122262=CARTESIAN_POINT('Ctrl Pts',(-7.185930826,3.784676613,-0.961716262));
#122263=CARTESIAN_POINT('',(-7.39709536883232,3.78467661265234,-1.23813574395619));
#122264=CARTESIAN_POINT('',(-7.29151309772682,3.78467661221161,-1.09992599818185));
#122265=CARTESIAN_POINT('',(-7.28147425473844,3.69493258302597,-1.79725698725771));
#122266=CARTESIAN_POINT('Ctrl Pts',(-7.39709536733601,3.78467661270495,
-1.23813574538389));
#122267=CARTESIAN_POINT('Ctrl Pts',(-7.38492113915177,3.77306479305815,
-1.31086923046358));
#122268=CARTESIAN_POINT('Ctrl Pts',(-7.37169150633935,3.76150355535505,
-1.38331814913354));
#122269=CARTESIAN_POINT('Ctrl Pts',(-7.35742489468756,3.75000000001838,
-1.45543770641804));
#122270=CARTESIAN_POINT('Ctrl Pts',(-7.33482796656171,3.73177948531458,
-1.5696680836393));
#122271=CARTESIAN_POINT('Ctrl Pts',(-7.30950995692274,3.71341418935042,
-1.68367209139032));
#122272=CARTESIAN_POINT('Ctrl Pts',(-7.28147425606393,3.69493258490811,
-1.79725698030097));
#122273=CARTESIAN_POINT('Ctrl Pts',(-7.03841135207602,3.65572482629248,
-1.73875404728258));
#122274=CARTESIAN_POINT('Ctrl Pts',(-7.07885255327227,3.66259516359781,
-1.74852640327108));
#122275=CARTESIAN_POINT('Ctrl Pts',(-7.11935171309557,3.66929202120471,
-1.75829234449999));
#122276=CARTESIAN_POINT('Ctrl Pts',(-7.20035906707951,3.6823499989136,-1.77778900530806));
#122277=CARTESIAN_POINT('Ctrl Pts',(-7.24091529565991,3.68871885434777,
-1.78753128353635));
#122278=CARTESIAN_POINT('Ctrl Pts',(-7.28147425305936,3.69493258269165,
-1.79725699447353));
#122279=CARTESIAN_POINT('Ctrl Pts',(-7.126538271,3.784676613,-2.337188968));
#122280=CARTESIAN_POINT('Ctrl Pts',(-7.253058636,3.720089779,-1.951404065));
#122281=CARTESIAN_POINT('Ctrl Pts',(-7.337193864,3.654947264,-1.554215624));
#122282=CARTESIAN_POINT('Ctrl Pts',(-6.811187188,3.784676613,-2.483994583));
#122283=CARTESIAN_POINT('Ctrl Pts',(-6.945654664,3.720089779,-2.115280757));
#122284=CARTESIAN_POINT('Ctrl Pts',(-7.039533398,3.654947264,-1.734205737));
#122285=CARTESIAN_POINT('',(-7.12653827171353,3.78467661255986,-2.33718897046504));
#122286=CARTESIAN_POINT('Origin',(0.187314493622497,3.62502543456919,0.0346729102936216));
#122287=CARTESIAN_POINT('',(-6.96886272684527,3.78467661169947,-2.41059178317464));
#122288=CARTESIAN_POINT('Origin',(-7.80625564189563E-15,3.87542691999945,
-1.14925430283463E-14));
#122289=CARTESIAN_POINT('',(-7.2824266169875,3.87435041280466,-1.79339414632136));
#122290=CARTESIAN_POINT('Origin',(0.184742667813114,3.62514698225076,0.00514695786445446));
#122291=CARTESIAN_POINT('Origin',(0.184772441726333,4.01774288341306,0.0219285383710868));
#122292=CARTESIAN_POINT('Ctrl Pts',(-6.609327869,3.654941533,-3.544966167));
#122293=CARTESIAN_POINT('Ctrl Pts',(-6.75182393300001,3.702826767,-3.279292768));
#122294=CARTESIAN_POINT('Ctrl Pts',(-6.872536305,3.75,-3.00303925));
#122295=CARTESIAN_POINT('Ctrl Pts',(-6.916764535,3.767283967,-2.901821752));
#122296=CARTESIAN_POINT('Ctrl Pts',(-6.957992803,3.784676613,-2.799345666));
#122297=CARTESIAN_POINT('Ctrl Pts',(-6.497963557,3.654941533,-3.215426816));
#122298=CARTESIAN_POINT('Ctrl Pts',(-6.62721321600001,3.702826767,-2.954229899));
#122299=CARTESIAN_POINT('Ctrl Pts',(-6.735081219,3.75,-2.683501626));
#122300=CARTESIAN_POINT('Ctrl Pts',(-6.77460335600001,3.767283967,-2.584308542));
#122301=CARTESIAN_POINT('Ctrl Pts',(-6.811187188,3.784676613,-2.483994583));
#122302=CARTESIAN_POINT('',(-6.95799280382198,3.78467661265224,-2.79934566613447));
#122303=CARTESIAN_POINT('',(-6.88458999724559,3.78467661221161,-2.64167011995074));
#122304=CARTESIAN_POINT('',(-6.72488030715598,3.69493258291181,-3.3205398430634));
#122305=CARTESIAN_POINT('Ctrl Pts',(-6.95799280205389,3.78467661270495,
-2.79934566720847));
#122306=CARTESIAN_POINT('Ctrl Pts',(-6.93046765080907,3.77306479305815,
-2.86776158452025));
#122307=CARTESIAN_POINT('Ctrl Pts',(-6.90197294353504,3.76150355535485,
-2.9356727074718));
#122308=CARTESIAN_POINT('Ctrl Pts',(-6.87253630462734,3.74999999995688,
-3.00303924964273));
#122309=CARTESIAN_POINT('Ctrl Pts',(-6.82591152545913,3.73177948512204,
-3.10974131322218));
#122310=CARTESIAN_POINT('Ctrl Pts',(-6.77667794548035,3.71341418925438,
-3.21563734638589));
#122311=CARTESIAN_POINT('Ctrl Pts',(-6.72488030982493,3.69493258471435,
-3.32053983682491));
#122312=CARTESIAN_POINT('Ctrl Pts',(-6.5000764830721,3.65572482634468,-3.21115333069244));
#122313=CARTESIAN_POINT('Ctrl Pts',(-6.53747141465312,3.6625951619445,-3.22939087267071));
#122314=CARTESIAN_POINT('Ctrl Pts',(-6.57492432725294,3.66929201774574,
-3.24763460849258));
#122315=CARTESIAN_POINT('Ctrl Pts',(-6.64984658820229,3.68234999883056,
-3.28408964402176));
#122316=CARTESIAN_POINT('Ctrl Pts',(-6.68736033292733,3.68871885425686,
-3.30232254341066));
#122317=CARTESIAN_POINT('Ctrl Pts',(-6.7248803040988,3.69493258259148,-3.32053984946918));
#122318=CARTESIAN_POINT('Ctrl Pts',(-6.457497225,3.784676613,-3.814541858));
#122319=CARTESIAN_POINT('Ctrl Pts',(-6.663991964,3.720089779,-3.46497453));
#122320=CARTESIAN_POINT('Ctrl Pts',(-6.83154393200001,3.654947264,-3.095158721));
#122321=CARTESIAN_POINT('Ctrl Pts',(-6.117960008,3.784676613,-3.890124078));
#122322=CARTESIAN_POINT('Ctrl Pts',(-6.328546282,3.720089779,-3.558937109));
#122323=CARTESIAN_POINT('Ctrl Pts',(-6.502150048,3.654947264,-3.206952564));
#122324=CARTESIAN_POINT('',(-6.45749722517541,3.78467661255985,-3.8145418605538));
#122325=CARTESIAN_POINT('Origin',(0.175481749935874,3.62502544254973,0.0741294711214169));
#122326=CARTESIAN_POINT('',(-6.28772861225752,3.78467661169946,-3.85233297492452));
#122327=CARTESIAN_POINT('Origin',(-2.54136989230602E-13,3.87542692000067,
-1.61762964134837E-13));
#122328=CARTESIAN_POINT('',(-6.72664080054465,3.87435041277593,-3.3169720436542));
#122329=CARTESIAN_POINT('Origin',(0.179317325669673,3.62514694770728,0.0447409567355106));
#122330=CARTESIAN_POINT('Origin',(0.175738402230885,4.01774290648807,0.0611363810192611));
#122331=CARTESIAN_POINT('Ctrl Pts',(-5.692742518,3.654941533,-4.882896949));
#122332=CARTESIAN_POINT('Ctrl Pts',(-5.889019031,3.702826767,-4.654067289));
#122333=CARTESIAN_POINT('Ctrl Pts',(-6.066295556,3.75,-4.410222016));
#122334=CARTESIAN_POINT('Ctrl Pts',(-6.131248525,3.767283967,-4.320878689));
#122335=CARTESIAN_POINT('Ctrl Pts',(-6.193542228,3.784676613,-4.229661295));
#122336=CARTESIAN_POINT('Ctrl Pts',(-5.654823062,3.654941533,-4.53712201));
#122337=CARTESIAN_POINT('Ctrl Pts',(-5.837200552,3.702826767,-4.309816588));
#122338=CARTESIAN_POINT('Ctrl Pts',(-6.000745237,3.75,-4.068606224));
#122339=CARTESIAN_POINT('Ctrl Pts',(-6.06066694900001,3.767283967,-3.98022831));
#122340=CARTESIAN_POINT('Ctrl Pts',(-6.117960008,3.784676613,-3.890124078));
#122341=CARTESIAN_POINT('',(-6.19354222877282,3.78467661265299,-4.22966129531913));
#122342=CARTESIAN_POINT('',(-6.15575112068274,3.78467661221161,-4.05989268243235));
#122343=CARTESIAN_POINT('',(-5.8538384305328,3.69493258295246,-4.68855794658045));
#122344=CARTESIAN_POINT('Ctrl Pts',(-6.1935422268163,3.78467661270495,-4.22966129597718));
#122345=CARTESIAN_POINT('Ctrl Pts',(-6.15195319866575,3.77306479305815,
-4.29056059385924));
#122346=CARTESIAN_POINT('Ctrl Pts',(-6.10952579781268,3.76150355535484,
-4.35075847299217));
#122347=CARTESIAN_POINT('Ctrl Pts',(-6.06629555573076,3.74999999995653,
-4.41022201567284));
#122348=CARTESIAN_POINT('Ctrl Pts',(-5.99782304821393,3.73177948514419,
-4.50440649522614));
#122349=CARTESIAN_POINT('Ctrl Pts',(-5.92697600490363,3.71341418929997,
-4.59724297326434));
#122350=CARTESIAN_POINT('Ctrl Pts',(-5.85383843453696,3.69493258478171,
-4.68855794097464));
#122351=CARTESIAN_POINT('Ctrl Pts',(-5.6578052618491,3.65572482628151,-4.53340265369335));
#122352=CARTESIAN_POINT('Ctrl Pts',(-5.69040539293398,3.66259516290112,
-4.5592526205251));
#122353=CARTESIAN_POINT('Ctrl Pts',(-5.72306081877124,3.66929201977292,
-4.58512110127768));
#122354=CARTESIAN_POINT('Ctrl Pts',(-5.78839467372621,3.68234999888282,
-4.63682990164374));
#122355=CARTESIAN_POINT('Ctrl Pts',(-5.82111183342389,3.6887188543046,-4.66270087208794));
#122356=CARTESIAN_POINT('Ctrl Pts',(-5.85383842610379,3.69493258262724,
-4.68855795226429));
#122357=CARTESIAN_POINT('Ctrl Pts',(-5.486510786,3.784676613,-5.11353101));
#122358=CARTESIAN_POINT('Ctrl Pts',(-5.763324435,3.720089779,-4.816526637));
#122359=CARTESIAN_POINT('Ctrl Pts',(-6.006458598,3.654947264,-4.491375636));
#122360=CARTESIAN_POINT('Ctrl Pts',(-5.138663817,3.784676613,-5.114355695));
#122361=CARTESIAN_POINT('Ctrl Pts',(-5.41552211,3.720089779,-4.836181517));
#122362=CARTESIAN_POINT('Ctrl Pts',(-5.660733389,3.654947264,-4.529745854));
#122363=CARTESIAN_POINT('',(-5.48651078539378,3.78467661259838,-5.11353101337042));
#122364=CARTESIAN_POINT('Origin',(0.155443362235889,3.62502545473262,0.110119686174778));
#122365=CARTESIAN_POINT('',(-5.31258729586815,3.78467661169946,-5.11394335885062));
#122366=CARTESIAN_POINT('Origin',(4.09828421199521E-13,3.87542691999967,
3.73832909073002E-13));
#122367=CARTESIAN_POINT('',(-5.85632473619676,3.8743504128077,-4.68545201434567));
#122368=CARTESIAN_POINT('Origin',(0.165506588395413,3.62514705308022,0.0822425757635481));
#122369=CARTESIAN_POINT('Origin',(0.158487625325135,4.01774296008671,0.0974859321624588));
#122370=CARTESIAN_POINT('Ctrl Pts',(-4.509970855,3.654941533,-5.992508897));
#122371=CARTESIAN_POINT('Ctrl Pts',(-4.75085014500001,3.702826767,-5.811222796));
#122372=CARTESIAN_POINT('Ctrl Pts',(-4.976401568,3.75,-5.611187702));
#122373=CARTESIAN_POINT('Ctrl Pts',(-5.059042148,3.767283967,-5.537896141));
#122374=CARTESIAN_POINT('Ctrl Pts',(-5.139488502,3.784676613,-5.462202664));
#122375=CARTESIAN_POINT('Ctrl Pts',(-4.54726932600001,3.654941533,-5.646666422));
#122376=CARTESIAN_POINT('Ctrl Pts',(-4.77424687800001,3.702826767,-5.463881043));
#122377=CARTESIAN_POINT('Ctrl Pts',(-4.985821077,3.75,-5.263467316));
#122378=CARTESIAN_POINT('Ctrl Pts',(-5.063340492,3.767283967,-5.190037026));
#122379=CARTESIAN_POINT('Ctrl Pts',(-5.138663817,3.784676613,-5.114355695));
#122380=CARTESIAN_POINT('',(-5.13948850268994,3.78467661265216,-5.46220266446606));
#122381=CARTESIAN_POINT('',(-5.13907616299444,3.78467661221161,-5.28827917610415));
#122382=CARTESIAN_POINT('',(-4.70907757523346,3.6949325829312,-5.83734429200579));
#122383=CARTESIAN_POINT('Ctrl Pts',(-5.13948850063391,3.78467661270495,
-5.46220266469957));
#122384=CARTESIAN_POINT('Ctrl Pts',(-5.0857802520988,3.77306479305815,-5.51273775897462));
#122385=CARTESIAN_POINT('Ctrl Pts',(-5.03140401545385,3.76150355535523,
-5.56240760790579));
#122386=CARTESIAN_POINT('Ctrl Pts',(-4.97640156835124,3.75000000007195,
-5.61118770142894));
#122387=CARTESIAN_POINT('Ctrl Pts',(-4.88928303217232,3.73177948542768,
-5.68845063510256));
#122388=CARTESIAN_POINT('Ctrl Pts',(-4.80013525362314,3.71341418927266,
-5.76388662848969));
#122389=CARTESIAN_POINT('Ctrl Pts',(-4.70907758031102,3.69493258474665,
-5.83734428743019));
#122390=CARTESIAN_POINT('Ctrl Pts',(-4.55098135569828,3.65572482635055,
-5.64367510635039));
#122391=CARTESIAN_POINT('Ctrl Pts',(-4.5772623290225,3.66259516142306,-5.67592877291498));
#122392=CARTESIAN_POINT('Ctrl Pts',(-4.60359332345062,3.66929201666084,
-5.70821240602175));
#122393=CARTESIAN_POINT('Ctrl Pts',(-4.65628385779129,3.6823499988366,-5.77275714643303));
#122394=CARTESIAN_POINT('Ctrl Pts',(-4.68267461454173,3.68871885427104,
-5.80505649036733));
#122395=CARTESIAN_POINT('Ctrl Pts',(-4.70907756972931,3.69493258260853,
-5.83734429656885));
#122396=CARTESIAN_POINT('Ctrl Pts',(-4.2589812,3.784676613,-6.173417136));
#122397=CARTESIAN_POINT('Ctrl Pts',(-4.593170261,3.720089779,-5.942863312));
#122398=CARTESIAN_POINT('Ctrl Pts',(-4.900517936,3.654947264,-5.677580819));
#122399=CARTESIAN_POINT('Ctrl Pts',(-3.919089417,3.784676613,-6.09944572399999));
#122400=CARTESIAN_POINT('Ctrl Pts',(-4.249274143,3.720089779,-5.887291453));
#122401=CARTESIAN_POINT('Ctrl Pts',(-4.554627128,3.654947264,-5.640733261));
#122402=CARTESIAN_POINT('',(-4.25898119661183,3.78467661255747,-6.1734171392271));
#122403=CARTESIAN_POINT('Origin',(0.128136702922485,3.62502543316226,0.140960870947283));
#122404=CARTESIAN_POINT('',(-4.08903530174211,3.78467661169946,-6.13643143450315));
#122405=CARTESIAN_POINT('Origin',(7.28150179041265E-13,3.87542691999978,
8.21391565875018E-13));
#122406=CARTESIAN_POINT('',(-4.71217343633271,3.87435041277489,-5.83484545661085));
#122407=CARTESIAN_POINT('Origin',(0.143957591579971,3.62514698264479,0.115899004331725));
#122408=CARTESIAN_POINT('Origin',(0.133825468097622,4.01774292011938,0.129276663896634));
#122409=CARTESIAN_POINT('Ctrl Pts',(-3.116317967,3.654941533,-6.82191779));
#122410=CARTESIAN_POINT('Ctrl Pts',(-3.390536786,3.702826767,-6.69665198300001));
#122411=CARTESIAN_POINT('Ctrl Pts',(-3.653816575,3.75,-6.549780488));
#122412=CARTESIAN_POINT('Ctrl Pts',(-3.750280582,3.767283967,-6.495967724));
#122413=CARTESIAN_POINT('Ctrl Pts',(-3.845118005,3.784676613,-6.439337507));
#122414=CARTESIAN_POINT('Ctrl Pts',(-3.22709033,3.654941533,-6.492178987));
#122415=CARTESIAN_POINT('Ctrl Pts',(-3.488054726,3.702826767,-6.362460494));
#122416=CARTESIAN_POINT('Ctrl Pts',(-3.737765465,3.75,-6.212214527));
#122417=CARTESIAN_POINT('Ctrl Pts',(-3.82925786,3.767283967,-6.157165379));
#122418=CARTESIAN_POINT('Ctrl Pts',(-3.919089417,3.784676613,-6.099445724));
#122419=CARTESIAN_POINT('',(-3.84511800556879,3.7846766126528,-6.43933750761177));
#122420=CARTESIAN_POINT('',(-3.88210371514274,3.78467661221161,-6.26939161293474));
#122421=CARTESIAN_POINT('',(-3.34412548649015,3.69493258295384,-6.71318290578519));
#122422=CARTESIAN_POINT('Ctrl Pts',(-3.8451180035154,3.78467661270495,-6.43933750738985));
#122423=CARTESIAN_POINT('Ctrl Pts',(-3.78180187253579,3.77306479305815,
-6.4771454331204));
#122424=CARTESIAN_POINT('Ctrl Pts',(-3.71801937323458,3.76150355535473,
-6.51396474519606));
#122425=CARTESIAN_POINT('Ctrl Pts',(-3.65381657476172,3.74999999992168,
-6.54978048744424));
#122426=CARTESIAN_POINT('Ctrl Pts',(-3.55212557335821,3.73177948505058,
-6.60650914605142));
#122427=CARTESIAN_POINT('Ctrl Pts',(-3.44884551331829,3.71341418929757,
-6.6610173506864));
#122428=CARTESIAN_POINT('Ctrl Pts',(-3.34412549248534,3.69493258478546,
-6.71318290238093));
#122429=CARTESIAN_POINT('Ctrl Pts',(-3.23135861816428,3.6557248262122,-6.49005558377445));
#122430=CARTESIAN_POINT('Ctrl Pts',(-3.2500915766167,3.66259516294686,-6.52720481884039));
#122431=CARTESIAN_POINT('Ctrl Pts',(-3.26886694552431,3.66929201994454,
-6.56439407440542));
#122432=CARTESIAN_POINT('Ctrl Pts',(-3.30645038375794,3.68234999883342,
-6.63875668313945));
#122433=CARTESIAN_POINT('Ctrl Pts',(-3.32528073514068,3.68871885427786,
-6.6759741189413));
#122434=CARTESIAN_POINT('Ctrl Pts',(-3.34412548007839,3.69493258262837,
-6.71318290908683));
#122435=CARTESIAN_POINT('Ctrl Pts',(-2.832306387,3.784676613,-6.944641137));
#122436=CARTESIAN_POINT('Ctrl Pts',(-3.208244551,3.720089779,-6.791318303));
#122437=CARTESIAN_POINT('Ctrl Pts',(-3.565434502,3.654947264,-6.598308633));
#122438=CARTESIAN_POINT('Ctrl Pts',(-2.516262752,3.784676613,-6.79933245));
#122439=CARTESIAN_POINT('Ctrl Pts',(-2.884334839,3.720089779,-6.663118183));
#122440=CARTESIAN_POINT('Ctrl Pts',(-3.235551564,3.654947264,-6.487966251));
#122441=CARTESIAN_POINT('',(-2.83230638302414,3.78467661255746,-6.94464113943562));
#122442=CARTESIAN_POINT('Origin',(0.0948385248949762,3.62502540108089,0.165210910142309));
#122443=CARTESIAN_POINT('',(-2.67428456193206,3.78467661169946,-6.87198679644513));
#122444=CARTESIAN_POINT('Origin',(-2.3787395664332E-13,3.87542691999945,
-7.92768628521401E-13));
#122445=CARTESIAN_POINT('',(-3.34768614346571,3.87435041276815,-6.71140801018691));
#122446=CARTESIAN_POINT('Origin',(0.115677207989847,3.62514695239622,0.144136193356513));
#122447=CARTESIAN_POINT('Origin',(0.102905937121066,4.01774294932997,0.155022531962715));
#122448=CARTESIAN_POINT('Ctrl Pts',(-1.576949515,3.654941533,-7.332341388));
#122449=CARTESIAN_POINT('Ctrl Pts',(-1.871685696,3.702826767,-7.268953167));
#122450=CARTESIAN_POINT('Ctrl Pts',(-2.160383179,3.75,-7.182112817));
#122451=CARTESIAN_POINT('Ctrl Pts',(-2.266160065,3.767283967,-7.150295076));
#122452=CARTESIAN_POINT('Ctrl Pts',(-2.370954065,3.784676613,-7.115376084));
#122453=CARTESIAN_POINT('Ctrl Pts',(-1.756016176,3.654941533,-7.034124479));
#122454=CARTESIAN_POINT('Ctrl Pts',(-2.038765011,3.702826767,-6.96353836300001));
#122455=CARTESIAN_POINT('Ctrl Pts',(-2.314936093,3.75,-6.870485491));
#122456=CARTESIAN_POINT('Ctrl Pts',(-2.416123388,3.767283967,-6.836391522));
#122457=CARTESIAN_POINT('Ctrl Pts',(-2.516262752,3.784676613,-6.79933245));
#122458=CARTESIAN_POINT('',(-2.37095406541212,3.78467661265402,-7.11537608473225));
#122459=CARTESIAN_POINT('',(-2.44360841309735,3.78467661221161,-6.95735426538529));
#122460=CARTESIAN_POINT('',(-1.82280580688747,3.69493258293707,-7.27512054808345));
#122461=CARTESIAN_POINT('Ctrl Pts',(-2.37095406346643,3.78467661270495,
-7.11537608406131));
#122462=CARTESIAN_POINT('Ctrl Pts',(-2.30099064162556,3.77306479305815,
-7.13868898533261));
#122463=CARTESIAN_POINT('Ctrl Pts',(-2.23078427769843,3.76150355535498,
-7.16093613044395));
#122464=CARTESIAN_POINT('Ctrl Pts',(-2.16038317911554,3.749999999997,-7.18211281673554));
#122465=CARTESIAN_POINT('Ctrl Pts',(-2.04887467270013,3.73177948523619,
-7.21565463245062));
#122466=CARTESIAN_POINT('Ctrl Pts',(-1.93629158990197,3.71341418927889,
-7.24668630494625));
#122467=CARTESIAN_POINT('Ctrl Pts',(-1.82280581343427,3.69493258475776,
-7.27512054606235));
#122468=CARTESIAN_POINT('Ctrl Pts',(-1.76064114319113,3.65572482631164,
-7.03296827586369));
#122469=CARTESIAN_POINT('Ctrl Pts',(-1.77095014868274,3.66259516333785,
-7.07327601647927));
#122470=CARTESIAN_POINT('Ctrl Pts',(-1.78129196996794,3.66929202064669,
-7.11363195929011));
#122471=CARTESIAN_POINT('Ctrl Pts',(-1.8020109648606,3.68234999887879,-7.19433533590008));
#122472=CARTESIAN_POINT('Ctrl Pts',(-1.81240042463632,3.68871885429569,
-7.2347306175881));
#122473=CARTESIAN_POINT('Ctrl Pts',(-1.8228057999587,3.69493258261361,-7.27512054991822));
#122474=CARTESIAN_POINT('Ctrl Pts',(-1.273196075,3.784676613,-7.391141438));
#122475=CARTESIAN_POINT('Ctrl Pts',(-1.673304891,3.720089779,-7.322218799));
#122476=CARTESIAN_POINT('Ctrl Pts',(-2.063635314,3.654947264,-7.210506868));
#122477=CARTESIAN_POINT('Ctrl Pts',(-0.995778438,3.784676613,-7.181289947));
#122478=CARTESIAN_POINT('Ctrl Pts',(-1.384527244,3.720089779,-7.127384913));
#122479=CARTESIAN_POINT('Ctrl Pts',(-1.765185206,3.654947264,-7.03182915));
#122480=CARTESIAN_POINT('',(-1.27319607054881,3.78467661255747,-7.39114143949019));
#122481=CARTESIAN_POINT('Origin',(0.0571057823865292,3.62502542317003,0.181735794487139));
#122482=CARTESIAN_POINT('',(-1.13448724847587,3.78467661169946,-7.28621569374938));
#122483=CARTESIAN_POINT('Origin',(1.40078920685127E-13,3.87542691999967,
2.1163626406917E-13));
#122484=CARTESIAN_POINT('',(-1.82666476757934,3.8743504127621,-7.27415258434626));
#122485=CARTESIAN_POINT('Origin',(0.0819875193912198,3.62514702744759,0.165632892872857));
#122486=CARTESIAN_POINT('Origin',(0.0671748843628595,4.01774297204972,0.173520298462304));
#122487=CARTESIAN_POINT('Ctrl Pts',(0.036155345,3.654941533,-7.499912852));
#122488=CARTESIAN_POINT('Ctrl Pts',(-0.265316662,3.702826767,-7.501366179));
#122489=CARTESIAN_POINT('Ctrl Pts',(-0.565932667,3.75,-7.478617534));
#122490=CARTESIAN_POINT('Ctrl Pts',(-0.676076422,3.767283967,-7.470282578));
#122491=CARTESIAN_POINT('Ctrl Pts',(-0.785926947,3.784676613,-7.458707585));
#122492=CARTESIAN_POINT('Ctrl Pts',(-0.202832658,3.654941533,-7.247162128));
#122493=CARTESIAN_POINT('Ctrl Pts',(-0.494144911,3.702826767,-7.23900891800001));
#122494=CARTESIAN_POINT('Ctrl Pts',(-0.783862884,3.75,-7.207500189));
#122495=CARTESIAN_POINT('Ctrl Pts',(-0.890013671,3.767283967,-7.195955596));
#122496=CARTESIAN_POINT('Ctrl Pts',(-0.995778438,3.784676613,-7.18128994700001));
#122497=CARTESIAN_POINT('',(-0.890852697336977,3.78467661221161,-7.31999876541133));
#122498=CARTESIAN_POINT('Ctrl Pts',(-0.20759804596496,3.65572482631731,
-7.24702718706223));
#122499=CARTESIAN_POINT('Ctrl Pts',(-0.209001059456919,3.66259516224294,
-7.2886086799602));
#122500=CARTESIAN_POINT('Ctrl Pts',(-0.210425759463657,3.66929201838331,
-7.33024430135007));
#122501=CARTESIAN_POINT('Ctrl Pts',(-0.213311515592496,3.68234999884975,
-7.4135148635547));
#122502=CARTESIAN_POINT('Ctrl Pts',(-0.214774283997655,3.68871885431118,
-7.45519915301341));
#122503=CARTESIAN_POINT('Ctrl Pts',(-0.216253745842927,3.69493258264677,
-7.49688163937647));
#122504=CARTESIAN_POINT('Ctrl Pts',(0.34544747,3.784676613,-7.49204017899999));
#122505=CARTESIAN_POINT('Ctrl Pts',(-0.060123354,3.720089779,-7.510740481));
#122506=CARTESIAN_POINT('Ctrl Pts',(-0.465342831,3.654947264,-7.485549816));
#122507=CARTESIAN_POINT('Ctrl Pts',(0.57126737,3.784676613,-7.227458308));
#122508=CARTESIAN_POINT('Ctrl Pts',(0.180019305,3.720089779,-7.258383046));
#122509=CARTESIAN_POINT('Ctrl Pts',(-0.212280749,3.654947264,-7.246891532));
#122510=CARTESIAN_POINT('',(0.458357428105106,3.78467661169946,-7.35974924299523));
#122511=CARTESIAN_POINT('Ctrl Pts',(1.64756962,3.654941533,-7.316796727));
#122512=CARTESIAN_POINT('Ctrl Pts',(1.353458284,3.702826767,-7.383023646));
#122513=CARTESIAN_POINT('Ctrl Pts',(1.054980228,3.75,-7.425430406));
#122514=CARTESIAN_POINT('Ctrl Pts',(0.945619802999998,3.767283967,-7.440967968));
#122515=CARTESIAN_POINT('Ctrl Pts',(0.835849241000001,3.784676613,-7.453278208));
#122516=CARTESIAN_POINT('Ctrl Pts',(1.35983509,3.654941533,-7.121330531));
#122517=CARTESIAN_POINT('Ctrl Pts',(1.073580856,3.702826767,-7.175991461));
#122518=CARTESIAN_POINT('Ctrl Pts',(0.783862884,3.75,-7.207500189));
#122519=CARTESIAN_POINT('Ctrl Pts',(0.677712097,3.767283967,-7.21904478299999));
#122520=CARTESIAN_POINT('Ctrl Pts',(0.57126737,3.784676613,-7.227458308));
#122521=CARTESIAN_POINT('',(0.835849240921721,3.78467661265316,-7.45327820883271));
#122522=CARTESIAN_POINT('',(0.703558300649563,3.78467661221161,-7.3403682584649));
#122523=CARTESIAN_POINT('',(1.40041008554965,3.69493258292194,-7.36809687647276));
#122524=CARTESIAN_POINT('Ctrl Pts',(0.835849242417206,3.78467661270495,
-7.45327820741139));
#122525=CARTESIAN_POINT('Ctrl Pts',(0.909135157053171,3.77306479305815,
-7.44505954502045));
#122526=CARTESIAN_POINT('Ctrl Pts',(0.982194061001742,3.76150355535505,
-7.43577161989865));
#122527=CARTESIAN_POINT('Ctrl Pts',(1.05498022756045,3.7500000000188,-7.42543040575917));
#122528=CARTESIAN_POINT('Ctrl Pts',(1.17026644958751,3.73177948530145,-7.40905092646273));
#122529=CARTESIAN_POINT('Ctrl Pts',(1.28547394979438,3.71341418927964,-7.38994210007725));
#122530=CARTESIAN_POINT('Ctrl Pts',(1.4004100787995,3.69493258473014,-7.36809687737378));
#122531=CARTESIAN_POINT('Ctrl Pts',(1.35515210599328,3.65572482629701,-7.12222316244251));
#122532=CARTESIAN_POINT('Ctrl Pts',(1.36272068683348,3.66259516309388,-7.163134114624));
#122533=CARTESIAN_POINT('Ctrl Pts',(1.37027972438359,3.66929202016128,-7.20410259268216));
#122534=CARTESIAN_POINT('Ctrl Pts',(1.38536214280068,3.68234999884869,-7.28604667629));
#122535=CARTESIAN_POINT('Ctrl Pts',(1.39289446304458,3.68871885427417,-7.32707086185062));
#122536=CARTESIAN_POINT('Ctrl Pts',(1.40041009256457,3.69493258260044,-7.36809687523637));
#122537=CARTESIAN_POINT('Ctrl Pts',(1.947938275,3.784676613,-7.242619448));
#122538=CARTESIAN_POINT('Ctrl Pts',(1.555869484,3.720089779,-7.348068286));
#122539=CARTESIAN_POINT('Ctrl Pts',(1.154708565,3.654947264,-7.410576774));
#122540=CARTESIAN_POINT('Ctrl Pts',(2.11160135,3.784676613,-6.935678751));
#122541=CARTESIAN_POINT('Ctrl Pts',(1.736148353,3.720089779,-7.049987254));
#122542=CARTESIAN_POINT('Ctrl Pts',(1.35054972,3.654947264,-7.123097322));
#122543=CARTESIAN_POINT('',(1.94793827739633,3.78467661255984,-7.24261944886446));
#122544=CARTESIAN_POINT('Origin',(-0.0244810821294403,3.62502541707946,
0.188917070851253));
#122545=CARTESIAN_POINT('',(2.0297698203071,3.78467661169946,-7.08914909726467));
#122546=CARTESIAN_POINT('Origin',(-9.24824453130135E-14,3.87542691999989,
-1.16226472890446E-13));
#122547=CARTESIAN_POINT('',(1.39650135063367,3.8743504127644,-7.36883871276101));
#122548=CARTESIAN_POINT('Origin',(0.00486236478177832,3.62514700919744,
0.184750327287636));
#122549=CARTESIAN_POINT('Origin',(-0.0118929950341548,4.01774294200309,
0.185688624677329));
#122550=CARTESIAN_POINT('Ctrl Pts',(3.181945371,3.654941533,-6.791555319));
#122551=CARTESIAN_POINT('Ctrl Pts',(2.908947024,3.702826767,-6.919459133));
#122552=CARTESIAN_POINT('Ctrl Pts',(2.62656342,3.75,-7.025038406));
#122553=CARTESIAN_POINT('Ctrl Pts',(2.523099898,3.767283967,-7.063721967));
#122554=CARTESIAN_POINT('Ctrl Pts',(2.418542048,3.784676613,-7.09934182600001));
#122555=CARTESIAN_POINT('Ctrl Pts',(2.85891846,3.654941533,-6.662513432));
#122556=CARTESIAN_POINT('Ctrl Pts',(2.591107176,3.702826767,-6.777432619));
#122557=CARTESIAN_POINT('Ctrl Pts',(2.314936093,3.75,-6.870485491));
#122558=CARTESIAN_POINT('Ctrl Pts',(2.213748799,3.767283967,-6.90457946));
#122559=CARTESIAN_POINT('Ctrl Pts',(2.11160135,3.784676613,-6.935678751));
#122560=CARTESIAN_POINT('',(2.41854204810109,3.78467661265302,-7.09934182683003));
#122561=CARTESIAN_POINT('',(2.26507169436299,3.78467661221163,-7.0175102899967));
#122562=CARTESIAN_POINT('',(2.95159230542166,3.69493258288868,-6.89478809371964));
#122563=CARTESIAN_POINT('Ctrl Pts',(2.4185420492583,3.78467661270494,-7.09934182512084));
#122564=CARTESIAN_POINT('Ctrl Pts',(2.48834781076507,3.77306479305814,-7.07556100546958));
#122565=CARTESIAN_POINT('Ctrl Pts',(2.55770200877317,3.76150355535497,-7.050784722334));
#122566=CARTESIAN_POINT('Ctrl Pts',(2.62656341956181,3.74999999999367,-7.0250384057497));
#122567=CARTESIAN_POINT('Ctrl Pts',(2.73563320979076,3.73177948519891,-6.98425873926709));
#122568=CARTESIAN_POINT('Ctrl Pts',(2.84403938978583,3.71341418922258,-6.94083045977405));
#122569=CARTESIAN_POINT('Ctrl Pts',(2.95159229910395,3.69493258467529,-6.8947880960262));
#122570=CARTESIAN_POINT('Ctrl Pts',(2.85453685143343,3.65572482630255,-6.66439189757751));
#122571=CARTESIAN_POINT('Ctrl Pts',(2.87072312912744,3.66259516339516,-6.70271935502675));
#122572=CARTESIAN_POINT('Ctrl Pts',(2.88691245315828,3.66929202076924,-6.74110504524683));
#122573=CARTESIAN_POINT('Ctrl Pts',(2.91925780735638,3.68234999885248,-6.81789104437783));
#122574=CARTESIAN_POINT('Ctrl Pts',(2.93543301341889,3.68871885426192,-6.85633688116857));
#122575=CARTESIAN_POINT('Ctrl Pts',(2.95159231192568,3.69493258257117,-6.8947880910376));
#122576=CARTESIAN_POINT('Ctrl Pts',(3.459345652,3.784676613,-6.654541882));
#122577=CARTESIAN_POINT('Ctrl Pts',(3.099111595,3.720089779,-6.84180858500001));
#122578=CARTESIAN_POINT('Ctrl Pts',(2.720767072,3.654947264,-6.989093399));
#122579=CARTESIAN_POINT('Ctrl Pts',(3.553199198,3.784676613,-6.319594564));
#122580=CARTESIAN_POINT('Ctrl Pts',(3.211097032,3.720089779,-6.511941894));
#122581=CARTESIAN_POINT('Ctrl Pts',(2.850229985,3.654947264,-6.66623499700001));
#122582=CARTESIAN_POINT('',(3.45934565454573,3.78467661255985,-6.65454188230779));
#122583=CARTESIAN_POINT('Origin',(-0.0645203334186512,3.62502544807729,
0.179237618766572));
#122584=CARTESIAN_POINT('',(3.50627243214405,3.78467661169946,-6.48706821913863));
#122585=CARTESIAN_POINT('Origin',(7.61109925084824E-14,3.87542692,-1.89518539750466E-13));
#122586=CARTESIAN_POINT('',(2.94793442701482,3.8743504127991,-6.89635284844599));
#122587=CARTESIAN_POINT('Origin',(-0.0349672952314722,3.62514694700665,
0.181476572229583));
#122588=CARTESIAN_POINT('Origin',(-0.0515325411352557,4.01774291754067,
0.178790762305159));
#122589=CARTESIAN_POINT('Ctrl Pts',(4.567536894,3.654941533,-5.948748333));
#122590=CARTESIAN_POINT('Ctrl Pts',(4.328416635,3.702826767,-6.13234840100001));
#122591=CARTESIAN_POINT('Ctrl Pts',(4.075331425,3.75,-6.296163417));
#122592=CARTESIAN_POINT('Ctrl Pts',(3.98260264499999,3.767283967,-6.356184177));
#122593=CARTESIAN_POINT('Ctrl Pts',(3.888146516,3.784676613,-6.41344811100001));
#122594=CARTESIAN_POINT('Ctrl Pts',(4.224321981,3.654941533,-5.892164611));
#122595=CARTESIAN_POINT('Ctrl Pts',(3.987476203,3.702826767,-6.061968561));
#122596=CARTESIAN_POINT('Ctrl Pts',(3.737765465,3.75,-6.212214527));
#122597=CARTESIAN_POINT('Ctrl Pts',(3.646273069,3.767283967,-6.267263675));
#122598=CARTESIAN_POINT('Ctrl Pts',(3.553199198,3.784676613,-6.319594564));
#122599=CARTESIAN_POINT('',(3.88814651615013,3.78467661264165,-6.41344811180752));
#122600=CARTESIAN_POINT('',(3.72067285279307,3.78467661221161,-6.36652133995858));
#122601=CARTESIAN_POINT('',(4.36476134892142,3.69493258293937,-6.09908668245247));
#122602=CARTESIAN_POINT('Ctrl Pts',(3.88814651703987,3.78467661270495,-6.41344810987096));
#122603=CARTESIAN_POINT('Ctrl Pts',(3.95120808549809,3.77306479305815,-6.37521709697566));
#122604=CARTESIAN_POINT('Ctrl Pts',(4.01361465239844,3.76150355535501,-6.33611096684481));
#122605=CARTESIAN_POINT('Ctrl Pts',(4.075331424686,3.75000000000677,-6.29616341695445));
#122606=CARTESIAN_POINT('Ctrl Pts',(4.17308480125791,3.7317794852682,-6.23289037585193));
#122607=CARTESIAN_POINT('Ctrl Pts',(4.26962070823788,3.71341418928686,-6.16717330105097));
#122608=CARTESIAN_POINT('Ctrl Pts',(4.36476134313645,3.69493258476044,-6.09908668613228));
#122609=CARTESIAN_POINT('Ctrl Pts',(4.22044662611337,3.65572482627337,-5.89494107521926));
#122610=CARTESIAN_POINT('Ctrl Pts',(4.24449374406195,3.66259516224952,-5.92889288124631));
#122611=CARTESIAN_POINT('Ctrl Pts',(4.26855635478161,3.6692920184403,-5.96290090268654));
#122612=CARTESIAN_POINT('Ctrl Pts',(4.3166522209443,3.68234999883244,-6.03093840455968));
#122613=CARTESIAN_POINT('Ctrl Pts',(4.34071397816382,3.68871885427257,-6.0650082078822));
#122614=CARTESIAN_POINT('Ctrl Pts',(4.3647613548088,3.69493258261569,-6.09908667835707));
#122615=CARTESIAN_POINT('Ctrl Pts',(4.808997871,3.784676613,-5.755305333));
#122616=CARTESIAN_POINT('Ctrl Pts',(4.497442691,3.720089779,-6.015633519));
#122617=CARTESIAN_POINT('Ctrl Pts',(4.159605534,3.654947264,-6.240807784));
#122618=CARTESIAN_POINT('Ctrl Pts',(4.828653401,3.784676613,-5.408013159));
#122619=CARTESIAN_POINT('Ctrl Pts',(4.535898384,3.720089779,-5.669405369));
#122620=CARTESIAN_POINT('Ctrl Pts',(4.216636664,3.654947264,-5.897666932));
#122621=CARTESIAN_POINT('',(4.80899787355245,3.78467661255986,-5.75530533275323));
#122622=CARTESIAN_POINT('Origin',(-0.10154261991247,3.6250254170349,0.161177119320642));
#122623=CARTESIAN_POINT('',(4.81882564214694,3.78467661169946,-5.58165924069315));
#122624=CARTESIAN_POINT('Origin',(-8.1380215066762E-13,3.87542692000056,
1.09287578986539E-12));
#122625=CARTESIAN_POINT('',(4.36152536599514,3.8743504127714,-6.10140118956461));
#122626=CARTESIAN_POINT('Origin',(-0.0731616365008658,3.6251470099273,0.169716425061738));
#122627=CARTESIAN_POINT('Origin',(-0.0887624311096608,4.01774290295748,
0.163532712363043));
#122628=CARTESIAN_POINT('Ctrl Pts',(5.739555467,3.654941533,-4.827784486));
#122629=CARTESIAN_POINT('Ctrl Pts',(5.54549429500001,3.702826767,-5.05849587400001));
#122630=CARTESIAN_POINT('Ctrl Pts',(5.333541463,3.75,-5.272886825));
#122631=CARTESIAN_POINT('Ctrl Pts',(5.255883319,3.767283967,-5.351438279));
#122632=CARTESIAN_POINT('Ctrl Pts',(5.175945575,3.784676613,-5.42766869));
#122633=CARTESIAN_POINT('Ctrl Pts',(5.392200901,3.654941533,-4.846304721));
#122634=CARTESIAN_POINT('Ctrl Pts',(5.197395276,3.702826767,-5.06305359));
#122635=CARTESIAN_POINT('Ctrl Pts',(4.985821077,3.75,-5.263467316));
#122636=CARTESIAN_POINT('Ctrl Pts',(4.908301662,3.767283967,-5.336897607));
#122637=CARTESIAN_POINT('Ctrl Pts',(4.828653401,3.784676613,-5.40801315900001));
#122638=CARTESIAN_POINT('',(5.17594557543062,3.78467661265236,-5.4276686907134));
#122639=CARTESIAN_POINT('',(5.00229948441995,3.78467661221161,-5.41784092780546));
#122640=CARTESIAN_POINT('',(5.57383900329526,3.69493258294351,-5.01819875675396));
#122641=CARTESIAN_POINT('Ctrl Pts',(5.17594557577235,3.78467661270495,-5.42766868867377));
#122642=CARTESIAN_POINT('Ctrl Pts',(5.22931426206921,3.77306479305815,-5.37677512226711));
#122643=CARTESIAN_POINT('Ctrl Pts',(5.28185513625994,3.76150355535484,-5.32516770467289));
#122644=CARTESIAN_POINT('Ctrl Pts',(5.33354146241084,3.7499999999535,-5.27288682476706));
#122645=CARTESIAN_POINT('Ctrl Pts',(5.41540758530399,3.73177948512943,-5.19007898539102));
#122646=CARTESIAN_POINT('Ctrl Pts',(5.49555930847529,3.71341418928853,-5.10514597349467));
#122647=CARTESIAN_POINT('Ctrl Pts',(5.57383899842944,3.69493258476864,-5.01819876160287));
#122648=CARTESIAN_POINT('Ctrl Pts',(5.38901300709273,3.65572482636599,-4.84984936019253));
#122649=CARTESIAN_POINT('Ctrl Pts',(5.41979654877931,3.66259516170139,-4.87783796967264));
#122650=CARTESIAN_POINT('Ctrl Pts',(5.45060730516922,3.66929201721005,-4.90587814937095));
#122651=CARTESIAN_POINT('Ctrl Pts',(5.51220477454759,3.68234999884185,-4.96198578808013));
#122652=CARTESIAN_POINT('Ctrl Pts',(5.5430279819644,3.68871885427849,-4.99008649180989));
#122653=CARTESIAN_POINT('Ctrl Pts',(5.57383900817425,3.69493258261921,-5.01819875147828));
#122654=CARTESIAN_POINT('Ctrl Pts',(5.93378669400001,3.784676613,-4.586957103));
#122655=CARTESIAN_POINT('Ctrl Pts',(5.685478366,3.720089779,-4.908174115));
#122656=CARTESIAN_POINT('Ctrl Pts',(5.403945465,3.654947264,-5.200708934));
#122657=CARTESIAN_POINT('Ctrl Pts',(5.878325138,3.784676613,-4.24355907));
#122658=CARTESIAN_POINT('Ctrl Pts',(5.648606168,3.720089779,-4.56177375));
#122659=CARTESIAN_POINT('Ctrl Pts',(5.385878098,3.654947264,-4.853330517));
#122660=CARTESIAN_POINT('',(5.93378669740299,3.7846766125581,-4.58695709980869));
#122661=CARTESIAN_POINT('Origin',(-0.133816982094878,3.62502543110219,0.135580259674121));
#122662=CARTESIAN_POINT('',(5.90605592085549,3.78467661170132,-4.41525808000507));
#122663=CARTESIAN_POINT('Origin',(1.24466409401336E-12,3.875426919999,-1.06685493772574E-12));
#122664=CARTESIAN_POINT('',(5.57117622608685,3.87435041281487,-5.02115479259927));
#122665=CARTESIAN_POINT('Origin',(-0.107935379660555,3.62514703452631,0.150021153177837));
#122666=CARTESIAN_POINT('Origin',(-0.121841914116984,4.01774292735558,0.140628110217738));
#122667=CARTESIAN_POINT('Ctrl Pts',(6.643198806,3.654941533,-3.481078802));
#122668=CARTESIAN_POINT('Ctrl Pts',(6.503270805,3.702826767,-3.748113702));
#122669=CARTESIAN_POINT('Ctrl Pts',(6.342361029,3.75,-4.003055905));
#122670=CARTESIAN_POINT('Ctrl Pts',(6.28340473,3.767283967,-4.096465076));
#122671=CARTESIAN_POINT('Ctrl Pts',(6.221723171,3.784676613,-4.188097513));
#122672=CARTESIAN_POINT('Ctrl Pts',(6.307946499,3.654941533,-3.573837008));
#122673=CARTESIAN_POINT('Ctrl Pts',(6.164289921,3.702826767,-3.82739586));
#122674=CARTESIAN_POINT('Ctrl Pts',(6.000745237,3.75,-4.068606224));
#122675=CARTESIAN_POINT('Ctrl Pts',(5.940823524,3.767283967,-4.156984138));
#122676=CARTESIAN_POINT('Ctrl Pts',(5.87832513800001,3.784676613,-4.24355907));
#122677=CARTESIAN_POINT('',(6.22172317159642,3.78467661265403,-4.1880975135927));
#122678=CARTESIAN_POINT('',(6.05002415171423,3.78467661221161,-4.21582829549779));
#122679=CARTESIAN_POINT('',(6.52229014041628,3.69493258292203,-3.70266543424931));
#122680=CARTESIAN_POINT('Ctrl Pts',(6.22172317147013,3.78467661270495,-4.18809751153862));
#122681=CARTESIAN_POINT('Ctrl Pts',(6.26290351519349,3.77306479305815,-4.12692111936028));
#122682=CARTESIAN_POINT('Ctrl Pts',(6.30312194364033,3.76150355535514,-4.06522551979907));
#122683=CARTESIAN_POINT('Ctrl Pts',(6.34236102849552,3.75000000004468,-4.003055905309));
#122684=CARTESIAN_POINT('Ctrl Pts',(6.40451192965349,3.73177948536437,-3.90458527148364));
#122685=CARTESIAN_POINT('Ctrl Pts',(6.46453166289258,3.71341418927574,-3.80440769392256));
#122686=CARTESIAN_POINT('Ctrl Pts',(6.52229013673516,3.69493258473157,-3.70266543998151));
#122687=CARTESIAN_POINT('Ctrl Pts',(6.30559512923655,3.65572482628442,-3.5779840780076));
#122688=CARTESIAN_POINT('Ctrl Pts',(6.34167569982709,3.66259516300955,-3.59870078211737));
#122689=CARTESIAN_POINT('Ctrl Pts',(6.37779393621342,3.66929202000516,-3.61946200121221));
#122690=CARTESIAN_POINT('Ctrl Pts',(6.45001275926347,3.68234999884121,-3.66101623074809));
#122691=CARTESIAN_POINT('Ctrl Pts',(6.48615615776691,3.68871885426855,-3.68183387725921));
#122692=CARTESIAN_POINT('Ctrl Pts',(6.52229014401681,3.69493258260042,-3.70266542809982));
#122693=CARTESIAN_POINT('Ctrl Pts',(6.781118246,3.784676613,-3.204127858));
#122694=CARTESIAN_POINT('Ctrl Pts',(6.607667391,3.720089779,-3.571213945));
#122695=CARTESIAN_POINT('Ctrl Pts',(6.395602912,3.654947264,-3.917430713));
#122696=CARTESIAN_POINT('Ctrl Pts',(6.653132924,3.784676613,-2.880680874));
#122697=CARTESIAN_POINT('Ctrl Pts',(6.497191406,3.720089779,-3.24083866));
#122698=CARTESIAN_POINT('Ctrl Pts',(6.303281859,3.654947264,-3.582057761));
#122699=CARTESIAN_POINT('',(6.78111824863517,3.78467661255781,-3.20412785413918));
#122700=CARTESIAN_POINT('Origin',(-0.159834164648105,3.62502540404964,0.103643783894751));
#122701=CARTESIAN_POINT('',(6.71712558834799,3.78467661170044,-3.04240435860819));
#122702=CARTESIAN_POINT('Origin',(6.63965410430123E-13,3.87542691999967,
-2.56955914879065E-13));
#122703=CARTESIAN_POINT('',(6.52032507813851,3.87435041281238,-3.70612477802144));
#122704=CARTESIAN_POINT('Origin',(-0.137661888874591,3.62514700884721,0.12331075786046));
#122705=CARTESIAN_POINT('Origin',(-0.149224008936868,4.01774292818933,0.111147792207484));
#122706=CARTESIAN_POINT('Ctrl Pts',(7.236213552,3.654941533,-1.971601742));
#122707=CARTESIAN_POINT('Ctrl Pts',(7.1569616,3.702826767,-2.262473898));
#122708=CARTESIAN_POINT('Ctrl Pts',(7.054618843,3.75,-2.54604654));
#122709=CARTESIAN_POINT('Ctrl Pts',(7.01712112,3.767283967,-2.649945718));
#122710=CARTESIAN_POINT('Ctrl Pts',(6.976579907,3.784676613,-2.752695552));
#122711=CARTESIAN_POINT('Ctrl Pts',(6.92873953,3.654941533,-2.134260649));
#122712=CARTESIAN_POINT('Ctrl Pts',(6.84294922100001,3.702826767,-2.412773354));
#122713=CARTESIAN_POINT('Ctrl Pts',(6.735081219,3.75,-2.683501626));
#122714=CARTESIAN_POINT('Ctrl Pts',(6.695559082,3.767283967,-2.78269471));
#122715=CARTESIAN_POINT('Ctrl Pts',(6.653132924,3.784676613,-2.880680874));
#122716=CARTESIAN_POINT('',(6.97657990769681,3.78467661265293,-2.75269555246126));
#122717=CARTESIAN_POINT('',(6.81485641363876,3.78467661221161,-2.81668821750318));
#122718=CARTESIAN_POINT('',(7.16576624024253,3.69493258298315,-2.21399959103629));
#122719=CARTESIAN_POINT('Ctrl Pts',(6.97657990714416,3.78467661270495,-2.75269555047203));
#122720=CARTESIAN_POINT('Ctrl Pts',(7.003646361286,3.77306479305815,-2.68409687135126));
#122721=CARTESIAN_POINT('Ctrl Pts',(7.02966177503315,3.76150355535505,-2.61519790717972));
#122722=CARTESIAN_POINT('Ctrl Pts',(7.05461884248965,3.7500000000164,-2.54604654030279));
#122723=CARTESIAN_POINT('Ctrl Pts',(7.09414841436022,3.73177948530313,-2.43651748824419));
#122724=CARTESIAN_POINT('Ctrl Pts',(7.13122970190591,3.713414189321,-2.32577953856128));
#122725=CARTESIAN_POINT('Ctrl Pts',(7.16576623782883,3.69493258483551,-2.21399959757585));
#122726=CARTESIAN_POINT('Ctrl Pts',(6.92733463179486,3.65572482628702,-2.13881623762723));
#122727=CARTESIAN_POINT('Ctrl Pts',(6.96702513999574,3.66259516342404,-2.15129234134254));
#122728=CARTESIAN_POINT('Ctrl Pts',(7.00676200318601,3.66929202084997,-2.16380382232231));
#122729=CARTESIAN_POINT('Ctrl Pts',(7.0862253164602,3.68234999889486,-2.1888616232306));
#122730=CARTESIAN_POINT('Ctrl Pts',(7.12599888104864,3.68871885432242,-2.20142280235593));
#122731=CARTESIAN_POINT('Ctrl Pts',(7.16576624248811,3.69493258265407,-2.21399958409845));
#122732=CARTESIAN_POINT('Ctrl Pts',(7.311372246,3.784676613,-1.671477154));
#122733=CARTESIAN_POINT('Ctrl Pts',(7.220889234,3.720089779,-2.067267779));
#122734=CARTESIAN_POINT('Ctrl Pts',(7.088209075,3.654947264,-2.450977787));
#122735=CARTESIAN_POINT('Ctrl Pts',(7.116847609,3.784676613,-1.383105243));
#122736=CARTESIAN_POINT('Ctrl Pts',(7.041975195,3.720089779,-1.768365556));
#122737=CARTESIAN_POINT('Ctrl Pts',(6.925951166,3.654947264,-2.143291965));
#122738=CARTESIAN_POINT('',(7.3113722477471,3.78467661255746,-1.67147714966288));
#122739=CARTESIAN_POINT('Origin',(-0.178377525387388,3.62502544882287,0.0668609742983872));
#122740=CARTESIAN_POINT('',(7.21410992918197,3.78467661169946,-1.52729119055528));
#122741=CARTESIAN_POINT('Origin',(-1.86786350275803E-12,3.87542691999978,
5.44269490587723E-13));
#122742=CARTESIAN_POINT('',(7.16459077629712,3.87435041280689,-2.21780048786891));
#122743=CARTESIAN_POINT('Origin',(-0.160951713076786,3.62514696513198,0.0908346270462984));
#122744=CARTESIAN_POINT('Origin',(-0.169628826863583,4.01774292196974,0.0764704926359777));
#122745=CARTESIAN_POINT('Ctrl Pts',(7.490870995,3.654941533,-0.369934777));
#122746=CARTESIAN_POINT('Ctrl Pts',(7.476000825,3.702826767,-0.67104333));
#122747=CARTESIAN_POINT('Ctrl Pts',(7.43701052,3.75,-0.969986869));
#122748=CARTESIAN_POINT('Ctrl Pts',(7.422724725,3.767283967,-1.079517843));
#122749=CARTESIAN_POINT('Ctrl Pts',(7.40521952,3.784676613,-1.188580606));
#122750=CARTESIAN_POINT('Ctrl Pts',(7.225552402,3.654941533,-0.594888634));
#122751=CARTESIAN_POINT('Ctrl Pts',(7.201639821,3.702826767,-0.885332247));
#122752=CARTESIAN_POINT('Ctrl Pts',(7.154492288,3.75,-1.172919475));
#122753=CARTESIAN_POINT('Ctrl Pts',(7.137217738,3.767283967,-1.278289571));
#122754=CARTESIAN_POINT('Ctrl Pts',(7.116847609,3.784676613,-1.383105243));
#122755=CARTESIAN_POINT('',(7.40521952078668,3.78467661265378,-1.18858060629129));
#122756=CARTESIAN_POINT('',(7.26103356365033,3.78467661221161,-1.28584292929801));
#122757=CARTESIAN_POINT('',(7.47417907411976,3.69493258291695,-0.621809588034605));
#122758=CARTESIAN_POINT('Ctrl Pts',(7.40521951981189,3.78467661270495,-1.18858060447705));
#122759=CARTESIAN_POINT('Ctrl Pts',(7.41690648710047,3.77306479305815,-1.11576723638085));
#122760=CARTESIAN_POINT('Ctrl Pts',(7.4275024342893,3.76150355535484,-1.04288654688099));
#122761=CARTESIAN_POINT('Ctrl Pts',(7.43701051966161,3.749999999954,-0.969986868978883));
#122762=CARTESIAN_POINT('Ctrl Pts',(7.45207040391301,3.73177948512167,-0.854520854919855));
#122763=CARTESIAN_POINT('Ctrl Pts',(7.46447936555569,3.71341418926482,-0.738400517224669));
#122764=CARTESIAN_POINT('Ctrl Pts',(7.47417907318899,3.69493258472366,-0.621809594771243));
#122765=CARTESIAN_POINT('Ctrl Pts',(7.22515966610095,3.65572482629693,-0.599639727402921));
#122766=CARTESIAN_POINT('Ctrl Pts',(7.26660422586383,3.66259516346406,-0.603291860843454));
#122767=CARTESIAN_POINT('Ctrl Pts',(7.30810166197504,3.66929202091486,-0.606968579461314));
#122768=CARTESIAN_POINT('Ctrl Pts',(7.39109385304935,3.68234999886983,-0.614358279513562));
#122769=CARTESIAN_POINT('Ctrl Pts',(7.43263781594534,3.68871885428331,-0.618075644577407));
#122770=CARTESIAN_POINT('Ctrl Pts',(7.47417907480425,3.69493258259591,-0.621809580953705));
#122771=CARTESIAN_POINT('Ctrl Pts',(7.499754606,3.784676613,-0.060670037));
#122772=CARTESIAN_POINT('Ctrl Pts',(7.496470321,3.720089779,-0.46665847));
#122773=CARTESIAN_POINT('Ctrl Pts',(7.449378459,3.654947264,-0.869919863));
#122774=CARTESIAN_POINT('Ctrl Pts',(7.24778641,3.784676613,0.179142852));
#122775=CARTESIAN_POINT('Ctrl Pts',(7.25748405,3.720089779,-0.213205645));
#122776=CARTESIAN_POINT('Ctrl Pts',(7.22477069400001,3.654947264,-0.604308219));
#122777=CARTESIAN_POINT('',(7.4997546067426,3.78467661255817,-0.0606700323674423));
#122778=CARTESIAN_POINT('Origin',(-0.188580229804709,3.6250254421705,0.0269519150140703));
#122779=CARTESIAN_POINT('',(7.37377050793487,3.78467661170154,0.0592364156075977));
#122780=CARTESIAN_POINT('Origin',(-1.06685493772574E-12,3.87542692000011,
1.41617132517341E-13));
#122781=CARTESIAN_POINT('',(7.47384817270334,3.87435041278447,-0.6257743120038));
#122782=CARTESIAN_POINT('Origin',(-0.176715334483249,3.62514697594731,0.0541110863649678));
#122783=CARTESIAN_POINT('Origin',(-0.182101924228347,4.01774293762491,0.0382174800455872));
#122784=CARTESIAN_POINT('Ctrl Pts',(7.395263635,3.654941533,1.249029928));
#122785=CARTESIAN_POINT('Ctrl Pts',(7.44547056,3.702826767,0.951764478));
#122786=CARTESIAN_POINT('Ctrl Pts',(7.471655851,3.75,0.651428311));
#122787=CARTESIAN_POINT('Ctrl Pts',(7.481249972,3.767283967,0.541387086));
#122788=CARTESIAN_POINT('Ctrl Pts',(7.487599299,3.784676613,0.431111049));
#122789=CARTESIAN_POINT('Ctrl Pts',(7.184506474,3.654941533,0.972299712));
#122790=CARTESIAN_POINT('Ctrl Pts',(7.223589747,3.702826767,0.683506012));
#122791=CARTESIAN_POINT('Ctrl Pts',(7.23936725,3.75,0.392507087));
#122792=CARTESIAN_POINT('Ctrl Pts',(7.245148025,3.767283967,0.285886968));
#122793=CARTESIAN_POINT('Ctrl Pts',(7.24778641,3.784676613,0.179142852));
#122794=CARTESIAN_POINT('',(7.48759929982812,3.78467661265328,0.43111104887842));
#122795=CARTESIAN_POINT('',(7.36769285470162,3.78467661221161,0.305126945631554));
#122796=CARTESIAN_POINT('',(7.43310760180177,3.69493258296357,0.999455540430897));
#122797=CARTESIAN_POINT('Ctrl Pts',(7.48759929848919,3.78467661270495,0.431111050447227));
#122798=CARTESIAN_POINT('Ctrl Pts',(7.48336030927576,3.77306479305815,0.504734434406425));
#122799=CARTESIAN_POINT('Ctrl Pts',(7.47804133512577,3.76150355535511,0.578189029261445));
#122800=CARTESIAN_POINT('Ctrl Pts',(7.47165585077238,3.75000000003437,0.651428310506225));
#122801=CARTESIAN_POINT('Ctrl Pts',(7.46154186354479,3.73177948533219,0.767432222086782));
#122802=CARTESIAN_POINT('Ctrl Pts',(7.4486982702273,3.71341418929205,0.883505291650194));
#122803=CARTESIAN_POINT('Ctrl Pts',(7.43310760235171,3.69493258480238,0.999455533532112));
#122804=CARTESIAN_POINT('Ctrl Pts',(7.18514426466047,3.65572482627106,0.967575270075688));
#122805=CARTESIAN_POINT('Ctrl Pts',(7.22640497355284,3.66259516332048,0.97291787694699));
#122806=CARTESIAN_POINT('Ctrl Pts',(7.26772260757813,3.66929202065056,0.978247840087374));
#122807=CARTESIAN_POINT('Ctrl Pts',(7.35036305591922,3.68234999887543,0.988871775223886));
#122808=CARTESIAN_POINT('Ctrl Pts',(7.3917348676734,3.68871885430748,0.994172044021346));
#122809=CARTESIAN_POINT('Ctrl Pts',(7.43310760093298,3.69493258263685,0.999455547618201));
#122810=CARTESIAN_POINT('Ctrl Pts',(7.337456775,3.784676613,1.552973944));
#122811=CARTESIAN_POINT('Ctrl Pts',(7.421524787,3.720089779,1.15577127));
#122812=CARTESIAN_POINT('Ctrl Pts',(7.462223187,3.654947264,0.751814547));
#122813=CARTESIAN_POINT('Ctrl Pts',(7.039826773,3.784676613,1.733014427));
#122814=CARTESIAN_POINT('Ctrl Pts',(7.133641018,3.720089779,1.351923526));
#122815=CARTESIAN_POINT('Ctrl Pts',(7.18576797400001,3.654947264,0.962932308));
#122816=CARTESIAN_POINT('',(7.33745677598408,3.7846766125602,1.55297394635713));
#122817=CARTESIAN_POINT('Origin',(-0.189965454764864,3.62502539034957,-0.0142174262418361));
#122818=CARTESIAN_POINT('',(7.18864177219204,3.78467661170049,1.64299419341043));
#122819=CARTESIAN_POINT('Origin',(1.69742692124331E-12,3.875426919999,2.83952548973954E-13));
#122820=CARTESIAN_POINT('',(7.43363673487299,3.87435041278443,0.995512375213104));
#122821=CARTESIAN_POINT('Origin',(-0.184216316489234,3.62514695593933,0.0148574046262219));
#122822=CARTESIAN_POINT('Origin',(-0.186060340080447,4.01774294148807,-0.00182259763174569));
#122823=CARTESIAN_POINT('Ctrl Pts',(6.953861968,3.654941533,2.809591382));
#122824=CARTESIAN_POINT('Ctrl Pts',(7.06679836700001,3.702826767,2.530068838));
#122825=CARTESIAN_POINT('Ctrl Pts',(7.156934859,3.75,2.242383426));
#122826=CARTESIAN_POINT('Ctrl Pts',(7.189960285,3.767283967,2.136977356));
#122827=CARTESIAN_POINT('Ctrl Pts',(7.219867256,3.784676613,2.030644429));
#122828=CARTESIAN_POINT('Ctrl Pts',(6.807521008,3.654941533,2.494024404));
#122829=CARTESIAN_POINT('Ctrl Pts',(6.907772645,3.702826767,2.220384289));
#122830=CARTESIAN_POINT('Ctrl Pts',(6.985737446,3.75,1.939580454));
#122831=CARTESIAN_POINT('Ctrl Pts',(7.014303243,3.767283967,1.83669575));
#122832=CARTESIAN_POINT('Ctrl Pts',(7.039826773,3.784676613,1.733014427));
#122833=CARTESIAN_POINT('',(7.21986725684003,3.78467661265474,2.03064442908069));
#122834=CARTESIAN_POINT('',(7.12984701574349,3.78467661221161,1.88182942328867));
#122835=CARTESIAN_POINT('',(7.04447227901576,3.69493258292078,2.57398723862445));
#122836=CARTESIAN_POINT('Ctrl Pts',(7.21986725519049,3.78467661270495,2.03064443030433));
#122837=CARTESIAN_POINT('Ctrl Pts',(7.1999005202516,3.77306479305815,2.10163528313903));
#122838=CARTESIAN_POINT('Ctrl Pts',(7.17891533445251,3.76150355535492,2.17222912823678));
#122839=CARTESIAN_POINT('Ctrl Pts',(7.15693485866925,3.74999999998004,2.24238342560418));
#122840=CARTESIAN_POINT('Ctrl Pts',(7.12211991836894,3.73177948519665,2.35350102255827));
#122841=CARTESIAN_POINT('Ctrl Pts',(7.08462432257388,3.71341418927471,2.46409937521361));
#122842=CARTESIAN_POINT('Ctrl Pts',(7.04447228100107,3.69493258472953,2.57398723211122));
#122843=CARTESIAN_POINT('Ctrl Pts',(6.80915950283612,3.65572482629022,2.48954752285279));
#122844=CARTESIAN_POINT('Ctrl Pts',(6.8483070455585,3.66259516136376,2.503635051298));
#122845=CARTESIAN_POINT('Ctrl Pts',(6.88751289855184,3.66929201659142,2.5177224682113));
#122846=CARTESIAN_POINT('Ctrl Pts',(6.96593745121808,3.68234999882244,2.54586328409005));
#122847=CARTESIAN_POINT('Ctrl Pts',(7.00520261193498,3.6887188542613,2.55993335229255));
#122848=CARTESIAN_POINT('Ctrl Pts',(7.04447227666092,3.69493258259933,2.57398724534652));
#122849=CARTESIAN_POINT('Ctrl Pts',(6.832067621,3.784676613,3.094002589));
#122850=CARTESIAN_POINT('Ctrl Pts',(6.999557003,3.720089779,2.724158431));
#122851=CARTESIAN_POINT('Ctrl Pts',(7.126142651,3.654947264,2.338394944));
#122852=CARTESIAN_POINT('Ctrl Pts',(6.502692661,3.784676613,3.205852173));
#122853=CARTESIAN_POINT('Ctrl Pts',(6.676236859,3.720089779,2.853838255));
#122854=CARTESIAN_POINT('Ctrl Pts',(6.810766729,3.654947264,2.48514719));
#122855=CARTESIAN_POINT('',(6.8320676214468,3.78467661256008,3.09400259152216));
#122856=CARTESIAN_POINT('Origin',(-0.182467702143871,3.62502542581436,-0.0547219315056946));
#122857=CARTESIAN_POINT('',(6.66738013753278,3.78467661170011,3.14992738833899));
#122858=CARTESIAN_POINT('Origin',(-1.01091010562548E-12,3.87542692000078,
-3.56485674313234E-13));
#122859=CARTESIAN_POINT('',(7.04583670518564,3.87435041281413,2.57025001060989));
#122860=CARTESIAN_POINT('Origin',(-0.183103012010924,3.62514699798789,-0.0250909105996028));
#122861=CARTESIAN_POINT('Origin',(-0.181318334342333,4.0177429538234,-0.0417773652865977));
#122862=CARTESIAN_POINT('Ctrl Pts',(6.187305443,3.654941533,4.238779465));
#122863=CARTESIAN_POINT('Ctrl Pts',(6.357690537,3.702826767,3.99006999));
#122864=CARTESIAN_POINT('Ctrl Pts',(6.507563547,3.75,3.728487185));
#122865=CARTESIAN_POINT('Ctrl Pts',(6.562476046,3.767283967,3.632644941));
#122866=CARTESIAN_POINT('Ctrl Pts',(6.614542245,3.784676613,3.535227133));
#122867=CARTESIAN_POINT('Ctrl Pts',(6.112223425,3.654941533,3.899131288));
#122868=CARTESIAN_POINT('Ctrl Pts',(6.268955771,3.702826767,3.653439864));
#122869=CARTESIAN_POINT('Ctrl Pts',(6.405462322,3.75,3.395961195));
#122870=CARTESIAN_POINT('Ctrl Pts',(6.455477438,3.767283967,3.30162268));
#122871=CARTESIAN_POINT('Ctrl Pts',(6.502692661,3.784676613,3.205852173));
#122872=CARTESIAN_POINT('',(6.61454224581363,3.78467661264356,3.53522713313392));
#122873=CARTESIAN_POINT('',(6.55861745522635,3.78467661221192,3.37053964866783));
#122874=CARTESIAN_POINT('',(6.32644526234173,3.69493258293484,4.02816215414154));
#122875=CARTESIAN_POINT('Ctrl Pts',(6.61454224392794,3.78467661270466,3.53522713410086));
#122876=CARTESIAN_POINT('Ctrl Pts',(6.57978138511409,3.77306479305805,3.60026600275559));
#122877=CARTESIAN_POINT('Ctrl Pts',(6.5441112313165,3.76150355535493,3.66469820841077));
#122878=CARTESIAN_POINT('Ctrl Pts',(6.50756354677996,3.74999999998162,3.72848718457547));
#122879=CARTESIAN_POINT('Ctrl Pts',(6.4496755619513,3.73177948520058,3.82952273065416));
#122880=CARTESIAN_POINT('Ctrl Pts',(6.38928121584586,3.71341418928213,3.92947491035372));
#122881=CARTESIAN_POINT('Ctrl Pts',(6.32644526570093,3.69493258475378,4.02816214817663));
#122882=CARTESIAN_POINT('Ctrl Pts',(6.11478601007337,3.65572482633407,3.89511130188058));
#122883=CARTESIAN_POINT('Ctrl Pts',(6.14998991154971,3.66259516307394,3.91728504138573));
#122884=CARTESIAN_POINT('Ctrl Pts',(6.18525078550877,3.66929202007563,3.93947120792721));
#122885=CARTESIAN_POINT('Ctrl Pts',(6.25579235404782,3.6823499988899,3.98381305591855));
#122886=CARTESIAN_POINT('Ctrl Pts',(6.29111486838206,3.68871885430092,4.00599502244057));
#122887=CARTESIAN_POINT('Ctrl Pts',(6.32644525857656,3.69493258261167,4.02816216023313));
#122888=CARTESIAN_POINT('Ctrl Pts',(6.007218578,3.784676613,4.490359112));
#122889=CARTESIAN_POINT('Ctrl Pts',(6.250297713,3.720089779,4.165166971));
#122890=CARTESIAN_POINT('Ctrl Pts',(6.456851606,3.654947264,3.815634592));
#122891=CARTESIAN_POINT('Ctrl Pts',(5.661499867,3.784676613,4.528787835));
#122892=CARTESIAN_POINT('Ctrl Pts',(5.906659286,3.720089779,4.222310679));
#122893=CARTESIAN_POINT('Ctrl Pts',(6.117301603,3.654947264,3.891159352));
#122894=CARTESIAN_POINT('',(6.00721857789413,3.78467661255989,4.49035911456038));
#122895=CARTESIAN_POINT('Origin',(-0.166438120794062,3.62502543736376,-0.0926677379736934));
#122896=CARTESIAN_POINT('',(5.834359217534,3.78467661169954,4.50957347992487));
#122897=CARTESIAN_POINT('Origin',(-4.28043017697277E-13,3.87542691999933,
-2.07733136248223E-13));
#122898=CARTESIAN_POINT('',(6.32858118252462,3.87435041281544,4.02480561184882));
#122899=CARTESIAN_POINT('Origin',(-0.173428612544835,3.62514700340954,-0.0638661794404793));
#122900=CARTESIAN_POINT('Origin',(-0.168098172405629,4.01774290969785,-0.0797786309649051));
#122901=CARTESIAN_POINT('Ctrl Pts',(5.131437393,3.654941533,5.469766932));
#122902=CARTESIAN_POINT('Ctrl Pts',(5.351304163,3.702826767,5.263499904));
#122903=CARTESIAN_POINT('Ctrl Pts',(5.553905796,3.75,5.040251027));
#122904=CARTESIAN_POINT('Ctrl Pts',(5.62813772100001,3.767283967,4.958454085));
#122905=CARTESIAN_POINT('Ctrl Pts',(5.69992859,3.784676613,4.874506546));
#122906=CARTESIAN_POINT('Ctrl Pts',(5.131125069,3.654941533,5.121919125));
#122907=CARTESIAN_POINT('Ctrl Pts',(5.337009493,3.702826767,4.915664652));
#122908=CARTESIAN_POINT('Ctrl Pts',(5.5256749,3.75,4.693550565));
#122909=CARTESIAN_POINT('Ctrl Pts',(5.594800682,3.767283967,4.612169403));
#122910=CARTESIAN_POINT('Ctrl Pts',(5.661499867,3.784676613,4.528787835));
#122911=CARTESIAN_POINT('',(5.69992859076987,3.78467661264248,4.87450654629026));
#122912=CARTESIAN_POINT('',(5.68071423160659,3.78467661221167,4.7016471867465));
#122913=CARTESIAN_POINT('',(5.31260069589747,3.69493258285852,5.2939846841393));
#122914=CARTESIAN_POINT('Ctrl Pts',(5.69992858871736,3.7846766127049,4.87450654684343));
#122915=CARTESIAN_POINT('Ctrl Pts',(5.65199898542052,3.77306479305813,4.93055228505985));
#122916=CARTESIAN_POINT('Ctrl Pts',(5.60331176036077,3.76150355535504,4.98581007269591));
#122917=CARTESIAN_POINT('Ctrl Pts',(5.55390579601133,3.75000000001507,5.04025102627296));
#122918=CARTESIAN_POINT('Ctrl Pts',(5.47565154445195,3.73177948527118,5.12648021133348));
#122919=CARTESIAN_POINT('Ctrl Pts',(5.395182420043,3.7134141892243,5.21111256605488));
#122920=CARTESIAN_POINT('Ctrl Pts',(5.31260070032299,3.69493258462341,5.29398467918044));
#122921=CARTESIAN_POINT('Ctrl Pts',(5.13449192012045,3.65572482626041,5.11854400406274));
#122922=CARTESIAN_POINT('Ctrl Pts',(5.16410607726281,3.66259516344758,5.14776713409778));
#122923=CARTESIAN_POINT('Ctrl Pts',(5.19377320384533,3.66929202093393,5.17701464831315));
#122924=CARTESIAN_POINT('Ctrl Pts',(5.25313335869222,3.68234999880056,5.23548415631472));
#122925=CARTESIAN_POINT('Ctrl Pts',(5.2828615851379,3.68871885422111,5.26474081721335));
#122926=CARTESIAN_POINT('Ctrl Pts',(5.31260069105651,3.69493258254474,5.29398468912891));
#122927=CARTESIAN_POINT('Ctrl Pts',(4.901478671,3.784676613,5.67675143300001));
#122928=CARTESIAN_POINT('Ctrl Pts',(5.208781448,3.720089779,5.41141693200001));
#122929=CARTESIAN_POINT('Ctrl Pts',(5.485645355,3.654947264,5.11445940800001));
#122930=CARTESIAN_POINT('Ctrl Pts',(4.555581632,3.784676613,5.639962411));
#122931=CARTESIAN_POINT('Ctrl Pts',(4.860892888,3.720089779,5.393352549));
#122932=CARTESIAN_POINT('Ctrl Pts',(5.137798252,3.654947264,5.115225227));
#122933=CARTESIAN_POINT('',(4.90147867036157,3.78467661255985,5.67675143547201));
#122934=CARTESIAN_POINT('Origin',(-0.142626193212273,3.62502542072744,-0.126280622329832));
#122935=CARTESIAN_POINT('',(4.72853014526859,3.78467661169946,5.65835692720741));
#122936=CARTESIAN_POINT('Origin',(6.89552581700781E-14,3.87542691999978,
4.59701721133854E-14));
#122937=CARTESIAN_POINT('',(5.31540823698528,3.87435041276596,5.29116577603125));
#122938=CARTESIAN_POINT('Origin',(-0.155644556110387,3.62514698104704,-0.0996550053936607));
#122939=CARTESIAN_POINT('Origin',(-0.14701820053967,4.01774292527244,-0.114049714748815));
#122940=CARTESIAN_POINT('Ctrl Pts',(3.835629033,3.654941533,6.444994175));
#122941=CARTESIAN_POINT('Ctrl Pts',(4.094696754,3.702826767,6.290814413));
#122942=CARTESIAN_POINT('Ctrl Pts',(4.340553583,3.75,6.116338332));
#122943=CARTESIAN_POINT('Ctrl Pts',(4.430633931,3.767283967,6.052411428));
#122944=CARTESIAN_POINT('Ctrl Pts',(4.518792609,3.784676613,5.98585945));
#122945=CARTESIAN_POINT('Ctrl Pts',(3.910101007,3.654941533,6.105211717));
#122946=CARTESIAN_POINT('Ctrl Pts',(4.155510583,3.702826767,5.948038425));
#122947=CARTESIAN_POINT('Ctrl Pts',(4.38751306,3.75,5.771674726));
#122948=CARTESIAN_POINT('Ctrl Pts',(4.472517264,3.767283967,5.707056211));
#122949=CARTESIAN_POINT('Ctrl Pts',(4.555581632,3.784676613,5.639962411));
#122950=CARTESIAN_POINT('',(4.51879260962801,3.7846766126534,5.98585945055455));
#122951=CARTESIAN_POINT('',(4.53718712434111,3.78467661221161,5.81291092750187));
#122952=CARTESIAN_POINT('',(4.05034482615765,3.69493258293517,6.31226637490125));
#122953=CARTESIAN_POINT('Ctrl Pts',(4.51879260756625,3.78467661270495,5.98585945054807));
#122954=CARTESIAN_POINT('Ctrl Pts',(4.45993539460359,3.77306479305815,6.03029142297988));
#122955=CARTESIAN_POINT('Ctrl Pts',(4.4005076589704,3.76150355535495,6.07379099976697));
#122956=CARTESIAN_POINT('Ctrl Pts',(4.34055358297325,3.74999999998799,6.11633833178121));
#122957=CARTESIAN_POINT('Ctrl Pts',(4.24559214605223,3.73177948520062,6.18372917663367));
#122958=CARTESIAN_POINT('Ctrl Pts',(4.14881089109748,3.71341418926484,6.24908438995837));
#122959=CARTESIAN_POINT('Ctrl Pts',(4.05034483171224,3.6949325847545,6.31226637089826));
#122960=CARTESIAN_POINT('Ctrl Pts',(3.91411469426839,3.65572482628045,6.10263927833785));
#122961=CARTESIAN_POINT('Ctrl Pts',(3.93675437896973,3.66259516319504,6.13754535472069));
#122962=CARTESIAN_POINT('Ctrl Pts',(3.95944055256593,3.66929202038164,6.17248663184647));
#122963=CARTESIAN_POINT('Ctrl Pts',(4.00484368630039,3.68234999886763,6.24234983720333));
#122964=CARTESIAN_POINT('Ctrl Pts',(4.02758756605168,3.68871885428794,6.27731318362012));
#122965=CARTESIAN_POINT('Ctrl Pts',(4.05034482018178,3.69493258261195,6.31226637884947));
#122966=CARTESIAN_POINT('Ctrl Pts',(3.566551069,3.784676613,6.597705167));
#122967=CARTESIAN_POINT('Ctrl Pts',(3.923708353,3.720089779,6.40463505300001));
#122968=CARTESIAN_POINT('Ctrl Pts',(4.257936425,3.654947264,6.174137786));
#122969=CARTESIAN_POINT('Ctrl Pts',(3.236649463,3.784676613,6.487418613));
#122970=CARTESIAN_POINT('Ctrl Pts',(3.587836542,3.720089779,6.312207247));
#122971=CARTESIAN_POINT('Ctrl Pts',(3.918057165,3.654947264,6.100108856));
#122972=CARTESIAN_POINT('',(3.56655106527544,3.78467661255747,6.5977051698394));
#122973=CARTESIAN_POINT('Origin',(-0.112144915021962,3.62502542437372,-0.15398841209647));
#122974=CARTESIAN_POINT('',(3.40160025879484,3.78467661169946,6.5425618937461));
#122975=CARTESIAN_POINT('Origin',(3.88144377749811E-14,3.87542691999956,
7.80625564189563E-14));
#122976=CARTESIAN_POINT('',(4.05369271029252,3.87435041278445,6.31011690930621));
#122977=CARTESIAN_POINT('Origin',(-0.130582748923885,3.62514698298211,-0.13078403823463));
#122978=CARTESIAN_POINT('Origin',(-0.119063806199796,4.01774296137409,-0.142988065470824));
#122979=CARTESIAN_POINT('Ctrl Pts',(2.360470923,3.654941533,7.118860655));
#122980=CARTESIAN_POINT('Ctrl Pts',(2.646625875,3.702826767,7.023977432));
#122981=CARTESIAN_POINT('Ctrl Pts',(2.924241908,3.75,6.906432456));
#122982=CARTESIAN_POINT('Ctrl Pts',(3.025958623,3.767283967,6.86336473800001));
#122983=CARTESIAN_POINT('Ctrl Pts',(3.126362908,3.784676613,6.81732021900001));
#122984=CARTESIAN_POINT('Ctrl Pts',(2.506244968,3.654941533,6.803031395));
#122985=CARTESIAN_POINT('Ctrl Pts',(2.779704616,3.702826767,6.702288531));
#122986=CARTESIAN_POINT('Ctrl Pts',(3.044195986,3.75,6.579921793));
#122987=CARTESIAN_POINT('Ctrl Pts',(3.14110391,3.767283967,6.53508741300001));
#122988=CARTESIAN_POINT('Ctrl Pts',(3.236649463,3.784676613,6.487418613));
#122989=CARTESIAN_POINT('',(3.12636290849546,3.78467661265307,6.81732021967232));
#122990=CARTESIAN_POINT('',(3.18150618989289,3.78467661221213,6.65236941389909));
#122991=CARTESIAN_POINT('',(2.59869933355453,3.6949325829309,7.03539350480189));
#122992=CARTESIAN_POINT('Ctrl Pts',(3.12636290647896,3.78467661270444,6.81732021922853));
#122993=CARTESIAN_POINT('Ctrl Pts',(3.05933018184786,3.77306479305799,6.84806083524092));
#122994=CARTESIAN_POINT('Ctrl Pts',(2.99194071024776,3.76150355535498,6.87776820981747));
#122995=CARTESIAN_POINT('Ctrl Pts',(2.92424190825284,3.74999999999723,6.90643245527431));
#122996=CARTESIAN_POINT('Ctrl Pts',(2.81701357788189,3.73177948525387,6.95183383669016));
#122997=CARTESIAN_POINT('Ctrl Pts',(2.70844557548394,3.71341418929348,6.99485597339471));
#122998=CARTESIAN_POINT('Ctrl Pts',(2.5986993398269,3.69493258474626,7.03539350208781));
#122999=CARTESIAN_POINT('Ctrl Pts',(2.51071781620878,3.65572482632389,6.8013819220982));
#123000=CARTESIAN_POINT('Ctrl Pts',(2.52532442071916,3.66259516218778,6.84033877095559));
#123001=CARTESIAN_POINT('Ctrl Pts',(2.53996885977681,3.66929201826815,6.87933999028188));
#123002=CARTESIAN_POINT('Ctrl Pts',(2.56929197403464,3.682349998848,6.95733017684901));
#123003=CARTESIAN_POINT('Ctrl Pts',(2.58398802850682,3.68871885427552,6.99636536148919));
#123004=CARTESIAN_POINT('Ctrl Pts',(2.59869932688208,3.69493258260825,7.03539350736838));
#123005=CARTESIAN_POINT('Ctrl Pts',(2.064855503,3.784676613,7.21015754));
#123006=CARTESIAN_POINT('Ctrl Pts',(2.455167015,3.720089779,7.09837955600001));
#123007=CARTESIAN_POINT('Ctrl Pts',(2.83113112,3.654947264,6.945120343));
#123008=CARTESIAN_POINT('Ctrl Pts',(1.766375162,3.784676613,7.03153033));
#123009=CARTESIAN_POINT('Ctrl Pts',(2.147016947,3.720089779,6.935910151));
#123010=CARTESIAN_POINT('Ctrl Pts',(2.51511208,3.654947264,6.799758174));
#123011=CARTESIAN_POINT('',(2.06485549874544,3.78467661255747,7.21015754196833));
#123012=CARTESIAN_POINT('Origin',(-0.0764201343107868,3.62502544448452,
-0.174496270778641));
#123013=CARTESIAN_POINT('',(1.915615324658,3.78467661169946,7.12084393710962));
#123014=CARTESIAN_POINT('Origin',(-1.23599047663348E-14,3.87542691999956,
3.963843142607E-13));
#123015=CARTESIAN_POINT('',(2.60243101765054,3.87435041278084,7.0340139887341));
#123016=CARTESIAN_POINT('Origin',(-0.0994150821283607,3.62514695328514,
-0.155797783113337));
#123017=CARTESIAN_POINT('Origin',(-0.0855418496423702,4.01774292338515,
-0.165239972260454));
#123018=CARTESIAN_POINT('Ctrl Pts',(0.774939815,3.654941533,7.459857122));
#123019=CARTESIAN_POINT('Ctrl Pts',(1.074801713,3.702826767,7.428707072));
#123020=CARTESIAN_POINT('Ctrl Pts',(1.371195932,3.75,7.373589473));
#123021=CARTESIAN_POINT('Ctrl Pts',(1.479792853,3.767283967,7.353394742));
#123022=CARTESIAN_POINT('Ctrl Pts',(1.587747952,3.784676613,7.330010671));
#123023=CARTESIAN_POINT('Ctrl Pts',(0.9851997,3.654941533,7.182748885));
#123024=CARTESIAN_POINT('Ctrl Pts',(1.273922751,3.702826767,7.14314707500001));
#123025=CARTESIAN_POINT('Ctrl Pts',(1.558535692,3.75,7.080499029));
#123026=CARTESIAN_POINT('Ctrl Pts',(1.662816028,3.767283967,7.057545191));
#123027=CARTESIAN_POINT('Ctrl Pts',(1.766375162,3.784676613,7.03153033));
#123028=CARTESIAN_POINT('',(1.58774795233273,3.78467661265383,7.33001067177046));
#123029=CARTESIAN_POINT('',(1.67706156174498,3.78467661221161,7.18077049939182));
#123030=CARTESIAN_POINT('',(1.02554154841774,3.694932582952,7.42955345417115));
#123031=CARTESIAN_POINT('Ctrl Pts',(1.58774795046899,3.78467661270495,7.3300106708948));
#123032=CARTESIAN_POINT('Ctrl Pts',(1.51567409001811,3.77306479305815,7.3456225344741));
#123033=CARTESIAN_POINT('Ctrl Pts',(1.44347393947909,3.76150355535514,7.3601486227396));
#123034=CARTESIAN_POINT('Ctrl Pts',(1.37119593248388,3.7500000000441,7.37358947262491));
#123035=CARTESIAN_POINT('Ctrl Pts',(1.25671458624729,3.73177948536409,7.39487847406491));
#123036=CARTESIAN_POINT('Ctrl Pts',(1.14143635549968,3.71341418929291,7.41355586531108));
#123037=CARTESIAN_POINT('Ctrl Pts',(1.02554155518139,3.69493258478233,7.42955345286027));
#123038=CARTESIAN_POINT('Ctrl Pts',(0.989922562716053,3.65572482627746,
7.18209950661361));
#123039=CARTESIAN_POINT('Ctrl Pts',(0.995813103393928,3.66259516373845,
7.22328556359935));
#123040=CARTESIAN_POINT('Ctrl Pts',(1.00173105597368,3.66929202150471,7.26452308866619));
#123041=CARTESIAN_POINT('Ctrl Pts',(1.01360302452885,3.68234999887928,7.34699349048117));
#123042=CARTESIAN_POINT('Ctrl Pts',(1.01956408260669,3.6887188543024,7.3882752714801));
#123043=CARTESIAN_POINT('Ctrl Pts',(1.02554154129235,3.69493258262675,7.42955345525194));
#123044=CARTESIAN_POINT('Ctrl Pts',(0.466609588,3.784676613,7.48547096));
#123045=CARTESIAN_POINT('Ctrl Pts',(0.871824797,3.720089779,7.460211721));
#123046=CARTESIAN_POINT('Ctrl Pts',(1.27194527,3.654947264,7.391356792));
#123047=CARTESIAN_POINT('Ctrl Pts',(0.213507122,3.784676613,7.246855505));
#123048=CARTESIAN_POINT('Ctrl Pts',(0.605805226,3.720089779,7.23529760400001));
#123049=CARTESIAN_POINT('Ctrl Pts',(0.994563149000001,3.654947264,7.181458358));
#123050=CARTESIAN_POINT('',(0.466609583418929,3.78467661255747,7.485470961005));
#123051=CARTESIAN_POINT('Origin',(-0.037121924407804,3.62502541058654,-0.186844580745509));
#123052=CARTESIAN_POINT('',(0.340058346887876,3.78467661169947,7.36616323287449));
#123053=CARTESIAN_POINT('Origin',(1.22352215164989E-13,3.87542692000033,
9.23306570088656E-13));
#123054=CARTESIAN_POINT('',(1.0294825429063,3.87435041278135,7.42900839215867));
#123055=CARTESIAN_POINT('Origin',(-0.0635989656444805,3.62514698225777,
-0.173527014489177));
#123056=CARTESIAN_POINT('Origin',(-0.0480202374533851,4.0177429109103,-0.179765932794114));
#123057=CARTESIAN_POINT('Origin',(-1.14342671615753E-13,3.87542691999933,
1.13884596197877E-12));
#123058=CARTESIAN_POINT('',(-0.0251083328437495,3.784676612654,7.49995797182608));
#123059=CARTESIAN_POINT('Ctrl Pts',(-0.0251083344734971,3.78467661270495,
7.4999579705691));
#123060=CARTESIAN_POINT('Ctrl Pts',(-0.0988532380978356,3.77306479305815,
7.49971108777196));
#123061=CARTESIAN_POINT('Ctrl Pts',(-0.172488069042823,3.76150355535486,
7.49837666610599));
#123062=CARTESIAN_POINT('Ctrl Pts',(-0.245965641750855,3.74999999995948,
7.49596564148352));
#123063=CARTESIAN_POINT('Ctrl Pts',(-0.362346987351099,3.73177948469136,
7.49214681183236));
#123064=CARTESIAN_POINT('Ctrl Pts',(-0.478945166289772,3.71341418839415,
7.48560612447644));
#123065=CARTESIAN_POINT('Ctrl Pts',(-0.595569421730545,3.69493258345309,
7.4763157408961));
#123066=CARTESIAN_POINT('',(-0.591603389574171,3.87435041291099,7.47663061978449));
#123067=CARTESIAN_POINT('Origin',(-0.0248088887967525,3.62514697597139,
-0.183141684594958));
#123068=CARTESIAN_POINT('Origin',(-0.00825320893698786,4.0177429119903,
-0.185885846195389));
#123069=CARTESIAN_POINT('Ctrl Pts',(-0.846826616,3.654941533,7.452038961));
#123070=CARTESIAN_POINT('Ctrl Pts',(-0.547278984,3.702826767,7.48607862600001));
#123071=CARTESIAN_POINT('Ctrl Pts',(-0.245965642,3.75,7.495965642));
#123072=CARTESIAN_POINT('Ctrl Pts',(-0.135566387,3.767283967,7.49958818));
#123073=CARTESIAN_POINT('Ctrl Pts',(-0.025108333,3.784676613,7.499957971));
#123074=CARTESIAN_POINT('Ctrl Pts',(-0.581912411,3.654941533,7.226609021));
#123075=CARTESIAN_POINT('Ctrl Pts',(-0.291426326,3.702826767,7.25));
#123076=CARTESIAN_POINT('Ctrl Pts',(0.,3.75,7.25));
#123077=CARTESIAN_POINT('Ctrl Pts',(0.106776717,3.767283967,7.25));
#123078=CARTESIAN_POINT('Ctrl Pts',(0.213507122,3.784676613,7.246855505));
#123079=CARTESIAN_POINT('',(0.094199399372222,3.78467661221161,7.37340673793775));
#123080=CARTESIAN_POINT('Ctrl Pts',(-0.037636821,1.973534152,7.499905564));
#123081=CARTESIAN_POINT('Ctrl Pts',(0.373348407,2.039276147,7.501968014));
#123082=CARTESIAN_POINT('Ctrl Pts',(0.782098092,2.104034486,7.459110039));
#123083=CARTESIAN_POINT('Ctrl Pts',(0.201401104,1.973534152,7.247202053));
#123084=CARTESIAN_POINT('Ctrl Pts',(0.598538503,2.039276147,7.23616553));
#123085=CARTESIAN_POINT('Ctrl Pts',(0.992091961000001,2.104034486,7.18180016));
#123086=CARTESIAN_POINT('',(0.206148885799383,1.97432008506241,7.24706856114906));
#123087=CARTESIAN_POINT('Origin',(0.0109862546629633,1.8750787904931,-0.193835066307506));
#123088=CARTESIAN_POINT('Ctrl Pts',(0.206148889272356,1.97432008582198,
7.24706856091956));
#123089=CARTESIAN_POINT('Ctrl Pts',(0.207389323391247,1.98121389469559,
7.28865544780864));
#123090=CARTESIAN_POINT('Ctrl Pts',(0.20865216717907,1.98793719438241,7.33029549705021));
#123091=CARTESIAN_POINT('Ctrl Pts',(0.211215736360714,2.00105345756954,
7.41357575940194));
#123092=CARTESIAN_POINT('Ctrl Pts',(0.212517943973008,2.00745398499083,
7.45526404173224));
#123093=CARTESIAN_POINT('Ctrl Pts',(0.213837435628797,2.01370168115021,
7.49695094993264));
#123094=CARTESIAN_POINT('Ctrl Pts',(1.24240846169613,2.10851071898521,7.39695738032139));
#123095=CARTESIAN_POINT('Ctrl Pts',(1.25618820682232,2.10627260249257,7.39459004978026));
#123096=CARTESIAN_POINT('Ctrl Pts',(1.26996795194848,2.104034486,7.39222271923915));
#123097=CARTESIAN_POINT('Ctrl Pts',(1.67129990201488,2.038849851,7.32327475439542));
#123098=CARTESIAN_POINT('Ctrl Pts',(2.06280841283434,1.973541827,7.21128260348006));
#123099=CARTESIAN_POINT('Ctrl Pts',(0.965316962563659,2.10851071898521,
7.18549885113338));
#123100=CARTESIAN_POINT('Ctrl Pts',(0.978704461781823,2.10627260249257,
7.18364950556676));
#123101=CARTESIAN_POINT('Ctrl Pts',(0.992091961,2.104034486,7.18180016));
#123102=CARTESIAN_POINT('Ctrl Pts',(1.381999838,2.038849851,7.12793839));
#123103=CARTESIAN_POINT('Ctrl Pts',(1.763784701,1.973541827,7.032180567));
#123104=CARTESIAN_POINT('',(1.75923475770139,1.97432008459303,7.03332020118504));
#123105=CARTESIAN_POINT('Origin',(-0.04140142794191,2.0178567362601,-0.195280406556874));
#123106=CARTESIAN_POINT('Ctrl Pts',(1.82046088137077,2.01370168116173,7.27570767517235));
#123107=CARTESIAN_POINT('Ctrl Pts',(1.81021078533883,2.00745398478552,7.23527903401856));
#123108=CARTESIAN_POINT('Ctrl Pts',(1.79997727388742,2.00105345715051,7.19484533535441));
#123109=CARTESIAN_POINT('Ctrl Pts',(1.77957084490069,1.98793719393146,7.11406321064706));
#123110=CARTESIAN_POINT('Ctrl Pts',(1.76938614485983,1.98121389346264,7.07366815198737));
#123111=CARTESIAN_POINT('Ctrl Pts',(1.75923476045435,1.97432008482154,7.03332020138535));
#123112=CARTESIAN_POINT('Ctrl Pts',(1.575501108,1.973534152,7.33265274399999));
#123113=CARTESIAN_POINT('Ctrl Pts',(1.977321095,2.039276147,7.246317299));
#123114=CARTESIAN_POINT('Ctrl Pts',(2.367301242,2.104034486,7.11659222000001));
#123115=CARTESIAN_POINT('Ctrl Pts',(1.754626674,1.973534152,7.034471212));
#123116=CARTESIAN_POINT('Ctrl Pts',(2.140106694,2.039276147,6.938319916));
#123117=CARTESIAN_POINT('Ctrl Pts',(2.512772145,2.104034486,6.80062321800001));
#123118=CARTESIAN_POINT('Origin',(-0.0309385540210372,1.87507850637468,
-0.191662857044855));
#123119=CARTESIAN_POINT('Ctrl Pts',(2.8034888261742,2.10851071909229,6.95693953369873));
#123120=CARTESIAN_POINT('Ctrl Pts',(2.81643750274181,2.10627260254611,6.95166531203499));
#123121=CARTESIAN_POINT('Ctrl Pts',(2.82938617930937,2.104034486,6.94639109037137));
#123122=CARTESIAN_POINT('Ctrl Pts',(3.20651343716099,2.038849851,6.79278058485507));
#123123=CARTESIAN_POINT('Ctrl Pts',(3.56479369392208,1.973541827,6.59924399066095));
#123124=CARTESIAN_POINT('Ctrl Pts',(2.48741823987845,2.10851071909229,6.80999126923477));
#123125=CARTESIAN_POINT('Ctrl Pts',(2.50009519243922,2.10627260254611,6.80530724361737));
#123126=CARTESIAN_POINT('Ctrl Pts',(2.512772145,2.104034486,6.800623218));
#123127=CARTESIAN_POINT('Ctrl Pts',(2.881985503,2.038849851,6.664202038));
#123128=CARTESIAN_POINT('Ctrl Pts',(3.234259347,1.973541827,6.48861052));
#123129=CARTESIAN_POINT('',(3.23006076639947,1.97432008459905,6.49070161271792));
#123130=CARTESIAN_POINT('Origin',(-0.0824129386066702,2.0178567697538,-0.181814627491717));
#123131=CARTESIAN_POINT('Ctrl Pts',(3.34196159965903,2.01370168113681,6.71426039576969));
#123132=CARTESIAN_POINT('Ctrl Pts',(3.32326018235616,2.00745398477792,6.67698042153999));
#123133=CARTESIAN_POINT('Ctrl Pts',(3.30457387463032,2.00105345714848,6.63969194278597));
#123134=CARTESIAN_POINT('Ctrl Pts',(3.26727876750594,1.98793719395234,6.56518523846705));
#123135=CARTESIAN_POINT('Ctrl Pts',(3.24864843637574,1.98121389347921,6.52792400329991));
#123136=CARTESIAN_POINT('Ctrl Pts',(3.23006076876782,1.97432008483358,6.49070161298074));
#123137=CARTESIAN_POINT('Ctrl Pts',(3.114970356,1.973534152,6.822533231));
#123138=CARTESIAN_POINT('Ctrl Pts',(3.488836447,2.039276147,6.651836841));
#123139=CARTESIAN_POINT('Ctrl Pts',(3.841812017,2.104034486,6.441310459));
#123140=CARTESIAN_POINT('Ctrl Pts',(3.22580785,1.973534152,6.492816316));
#123141=CARTESIAN_POINT('Ctrl Pts',(3.581605876,2.039276147,6.316046174));
#123142=CARTESIAN_POINT('Ctrl Pts',(3.915957895,2.104034486,6.101456692));
#123143=CARTESIAN_POINT('Origin',(-0.071416952844599,1.87507855779732,-0.180530784418701));
#123144=CARTESIAN_POINT('Ctrl Pts',(4.23348117064494,2.10851071892058,6.19162292591988));
#123145=CARTESIAN_POINT('Ctrl Pts',(4.24499331214195,2.10627260246026,6.18368843020217));
#123146=CARTESIAN_POINT('Ctrl Pts',(4.25650545363899,2.104034486,6.17575393448443));
#123147=CARTESIAN_POINT('Ctrl Pts',(4.59179396738482,2.038849851,5.94466354376879));
#123148=CARTESIAN_POINT('Ctrl Pts',(4.90009318391161,1.973541827,5.67863206376884));
#123149=CARTESIAN_POINT('Ctrl Pts',(3.89321060504381,2.10851071892058,6.11605606300682));
#123150=CARTESIAN_POINT('Ctrl Pts',(3.9045842500219,2.10627260246026,6.10875637750341));
#123151=CARTESIAN_POINT('Ctrl Pts',(3.915957895,2.104034486,6.101456692));
#123152=CARTESIAN_POINT('Ctrl Pts',(4.247212729,2.038849851,5.88885500499999));
#123153=CARTESIAN_POINT('Ctrl Pts',(4.55350362,1.973541827,5.64164025600001));
#123154=CARTESIAN_POINT('',(4.54985272407125,1.97432008460192,5.64458503122448));
#123155=CARTESIAN_POINT('Origin',(-0.11957089886817,2.01785677029382,-0.159847509292501));
#123156=CARTESIAN_POINT('Ctrl Pts',(4.70719590746652,2.0137016811724,5.83886176251772));
#123157=CARTESIAN_POINT('Ctrl Pts',(4.68091762642383,2.00745398479891,5.80647362523456));
#123158=CARTESIAN_POINT('Ctrl Pts',(4.65465227342763,2.00105345713783,5.7740739340661));
#123159=CARTESIAN_POINT('Ctrl Pts',(4.60221236624691,1.98793719392138,5.709326500652));
#123160=CARTESIAN_POINT('Ctrl Pts',(4.57600753795865,1.98121389346668,5.67694138305711));
#123161=CARTESIAN_POINT('Ctrl Pts',(4.54985272626207,1.97432008483703,5.64458503070716));
#123162=CARTESIAN_POINT('Ctrl Pts',(4.508787052,1.973534152,5.993399646));
#123163=CARTESIAN_POINT('Ctrl Pts',(4.837217683,2.039276147,5.746323886));
#123164=CARTESIAN_POINT('Ctrl Pts',(5.136683932,2.104034486,5.464840179));
#123165=CARTESIAN_POINT('Ctrl Pts',(4.546153837,1.973534152,5.647564545));
#123166=CARTESIAN_POINT('Ctrl Pts',(4.855633147,2.039276147,5.398441132));
#123167=CARTESIAN_POINT('Ctrl Pts',(5.136037807,2.104034486,5.11699283300001));
#123168=CARTESIAN_POINT('Origin',(-0.108556179717638,1.87507852096226,-0.160957689532432));
#123169=CARTESIAN_POINT('Ctrl Pts',(5.4655206391911,2.10851071889853,5.13679291131898));
#123170=CARTESIAN_POINT('Ctrl Pts',(5.47505795112589,2.10627260244923,5.12656914964515));
#123171=CARTESIAN_POINT('Ctrl Pts',(5.48459526306069,2.104034486,5.11634538797148));
#123172=CARTESIAN_POINT('Ctrl Pts',(5.76236731444896,2.038849851,4.81858064331117));
#123173=CARTESIAN_POINT('Ctrl Pts',(6.00626976343028,1.973541827,4.49249361300632));
#123174=CARTESIAN_POINT('Ctrl Pts',(5.11696076933579,2.10851071889853,5.13614087365377));
#123175=CARTESIAN_POINT('Ctrl Pts',(5.12649928816785,2.10627260244923,5.12656685332694));
#123176=CARTESIAN_POINT('Ctrl Pts',(5.136037807,2.104034486,5.116992833));
#123177=CARTESIAN_POINT('Ctrl Pts',(5.413845009,2.038849851,4.838151658));
#123178=CARTESIAN_POINT('Ctrl Pts',(5.659831125,1.973541827,4.530873164));
#123179=CARTESIAN_POINT('',(5.65689862469295,1.97432008458259,4.53453392705498));
#123180=CARTESIAN_POINT('Origin',(-0.15113806033607,2.01785671859312,-0.130406290041515));
#123181=CARTESIAN_POINT('Ctrl Pts',(5.85232696622083,2.01370168119811,4.690444443045));
#123182=CARTESIAN_POINT('Ctrl Pts',(5.81970056460916,2.00745398481113,4.66446257602344));
#123183=CARTESIAN_POINT('Ctrl Pts',(5.78708430510987,2.00105345714669,4.63846664610439));
#123184=CARTESIAN_POINT('Ctrl Pts',(5.72195162961054,1.98793719392437,4.58650600150808));
#123185=CARTESIAN_POINT('Ctrl Pts',(5.68939761284271,1.98121389349597,4.56051129344533));
#123186=CARTESIAN_POINT('Ctrl Pts',(5.65689862700698,1.97432008489497,4.53453392596363));
#123187=CARTESIAN_POINT('Ctrl Pts',(5.691777876,1.973534152,4.884021356));
#123188=CARTESIAN_POINT('Ctrl Pts',(5.959415997,2.039276147,4.57211921199999));
#123189=CARTESIAN_POINT('Ctrl Pts',(6.191370215,2.104034486,4.232840047));
#123190=CARTESIAN_POINT('Ctrl Pts',(5.653926723,1.973534152,4.538238933));
#123191=CARTESIAN_POINT('Ctrl Pts',(5.902616409,2.039276147,4.228410983));
#123192=CARTESIAN_POINT('Ctrl Pts',(6.115962299,2.104034486,3.893264076));
#123193=CARTESIAN_POINT('Origin',(-0.140619339003883,1.87507853779743,-0.133858214553792));
#123194=CARTESIAN_POINT('Ctrl Pts',(6.44199843682638,2.10851071890015,3.84177217007522));
#123195=CARTESIAN_POINT('Ctrl Pts',(6.44911496517792,2.10627260245004,3.82973719410629));
#123196=CARTESIAN_POINT('Ctrl Pts',(6.45623149352946,2.104034486,3.81770221813728));
#123197=CARTESIAN_POINT('Ctrl Pts',(6.6634987709102,2.038849851,3.46718626721084));
#123198=CARTESIAN_POINT('Ctrl Pts',(6.83159984383339,1.973541827,3.09629115331911));
#123199=CARTESIAN_POINT('Ctrl Pts',(6.10144753458863,2.10851071890015,3.91606544531126));
#123200=CARTESIAN_POINT('Ctrl Pts',(6.10870491679432,2.10627260245004,3.90466476065566));
#123201=CARTESIAN_POINT('Ctrl Pts',(6.115962299,2.104034486,3.893264076));
#123202=CARTESIAN_POINT('Ctrl Pts',(6.327331913,2.038849851,3.561221716));
#123203=CARTESIAN_POINT('Ctrl Pts',(6.501511218,1.973541827,3.208247479));
#123204=CARTESIAN_POINT('',(6.49943423274117,1.97432008456978,3.21245305639565));
#123205=CARTESIAN_POINT('Origin',(-0.175638016403146,2.01785677543793,-0.0948672503717496));
#123206=CARTESIAN_POINT('Ctrl Pts',(6.72380972081394,2.01370168119116,3.32270715395686));
#123207=CARTESIAN_POINT('Ctrl Pts',(6.6863607730789,2.00745398482567,3.30434644058282));
#123208=CARTESIAN_POINT('Ctrl Pts',(6.64891870713716,2.00105345717049,3.28596981283331));
#123209=CARTESIAN_POINT('Ctrl Pts',(6.57413879473958,1.98793719396562,3.24922557947126));
#123210=CARTESIAN_POINT('Ctrl Pts',(6.53675777860832,1.98121389349064,3.23083676460714));
#123211=CARTESIAN_POINT('Ctrl Pts',(6.49943423450967,1.9743200848467,3.21245305497854));
#123212=CARTESIAN_POINT('Ctrl Pts',(6.608627494,1.973534152,3.546271655));
#123213=CARTESIAN_POINT('Ctrl Pts',(6.802958642,2.039276147,3.184127325));
#123214=CARTESIAN_POINT('Ctrl Pts',(6.956554908,2.104034486,2.802917018));
#123215=CARTESIAN_POINT('Ctrl Pts',(6.49732827900001,1.973534152,3.216710312));
#123216=CARTESIAN_POINT('Ctrl Pts',(6.67359988800001,2.039276147,2.860665037));
#123217=CARTESIAN_POINT('Ctrl Pts',(6.809911191,2.104034486,2.487490617));
#123218=CARTESIAN_POINT('Origin',(-0.166107150153769,1.87507854227463,-0.10049961351814));
#123219=CARTESIAN_POINT('Ctrl Pts',(7.11725554807123,2.10851071887221,2.36711443152886));
#123220=CARTESIAN_POINT('Ctrl Pts',(7.12161853182935,2.10627260243607,2.35383098346935));
#123221=CARTESIAN_POINT('Ctrl Pts',(7.12598151558734,2.104034486,2.34054753540986));
#123222=CARTESIAN_POINT('Ctrl Pts',(7.2530524307518,2.038849851,1.95367011503003));
#123223=CARTESIAN_POINT('Ctrl Pts',(7.33749190763721,1.973541827,1.55530956171743));
#123224=CARTESIAN_POINT('Ctrl Pts',(6.80063739414221,2.10851071887221,2.5128791480281));
#123225=CARTESIAN_POINT('Ctrl Pts',(6.80527429257119,2.10627260243607,2.50018488251402));
#123226=CARTESIAN_POINT('Ctrl Pts',(6.809911191,2.104034486,2.487490617));
#123227=CARTESIAN_POINT('Ctrl Pts',(6.944959809,2.038849851,2.117773005));
#123228=CARTESIAN_POINT('Ctrl Pts',(7.039187871,1.973541827,1.735607707));
#123229=CARTESIAN_POINT('',(7.03806351987006,1.97432008460083,1.74016145090013));
#123230=CARTESIAN_POINT('Origin',(-0.191925213452907,2.01785676680825,-0.0548922832922177));
#123231=CARTESIAN_POINT('Ctrl Pts',(7.28089460562994,2.01370168114298,1.7996037715632));
#123232=CARTESIAN_POINT('Ctrl Pts',(7.24037418281004,2.00745398477847,1.78972273822671));
#123233=CARTESIAN_POINT('Ctrl Pts',(7.19985705962638,2.0010534570977,1.77982468312593));
#123234=CARTESIAN_POINT('Ctrl Pts',(7.11892653610712,1.98793719390642,1.76001497998512));
#123235=CARTESIAN_POINT('Ctrl Pts',(7.07846641611887,1.98121389348972,1.75009189878342));
#123236=CARTESIAN_POINT('Ctrl Pts',(7.03806352196428,1.97432008490095,1.74016144855234));
#123237=CARTESIAN_POINT('Ctrl Pts',(7.216465034,1.973534152,2.042702233));
#123238=CARTESIAN_POINT('Ctrl Pts',(7.328402503,2.039276147,1.647249183));
#123239=CARTESIAN_POINT('Ctrl Pts',(7.39645882600001,2.104034486,1.241932705));
#123240=CARTESIAN_POINT('Ctrl Pts',(7.036921987,1.973534152,1.744771892));
#123241=CARTESIAN_POINT('Ctrl Pts',(7.132533254,2.039276147,1.359157572));
#123242=CARTESIAN_POINT('Ctrl Pts',(7.185436205,2.104034486,0.965404863));
#123243=CARTESIAN_POINT('Origin',(-0.183828099314221,1.87507853001457,-0.0624418681352172));
#123244=CARTESIAN_POINT('Ctrl Pts',(7.45971770060335,2.1085107188556,0.781773053483733));
#123245=CARTESIAN_POINT('Ctrl Pts',(7.46112313152621,2.10627260242776,0.767862252559916));
#123246=CARTESIAN_POINT('Ctrl Pts',(7.46252856244921,2.104034486,0.753951451636089));
#123247=CARTESIAN_POINT('Ctrl Pts',(7.50346142036284,2.038849851,0.348802519468778));
#123248=CARTESIAN_POINT('Ctrl Pts',(7.50029100568184,1.973541827,-0.0583965774922585));
#123249=CARTESIAN_POINT('Ctrl Pts',(7.18183700810203,2.1085107188556,0.992193416474425));
#123250=CARTESIAN_POINT('Ctrl Pts',(7.18363660655107,2.10627260242776,0.978799139737212));
#123251=CARTESIAN_POINT('Ctrl Pts',(7.185436205,2.104034486,0.965404863000001));
#123252=CARTESIAN_POINT('Ctrl Pts',(7.237849103,2.038849851,0.575299581));
#123253=CARTESIAN_POINT('Ctrl Pts',(7.247719923,1.973541827,0.181812848));
#123254=CARTESIAN_POINT('',(7.24760077907989,1.97432008459269,0.186501829852585));
#123255=CARTESIAN_POINT('Origin',(-0.199238328473579,2.01785675377979,-0.0123506811088942));
#123256=CARTESIAN_POINT('Ctrl Pts',(7.49753295086213,2.01370168117945,0.192352917068669));
#123257=CARTESIAN_POINT('Ctrl Pts',(7.45583574284584,2.00745398481533,0.191413589910291));
#123258=CARTESIAN_POINT('Ctrl Pts',(7.41413809829081,2.0010534571559,0.190456929640095));
#123259=CARTESIAN_POINT('Ctrl Pts',(7.33084118470819,1.98793719395886,0.18850803665614));
#123260=CARTESIAN_POINT('Ctrl Pts',(7.28919383066974,1.98121389353883,0.187514681429552));
#123261=CARTESIAN_POINT('Ctrl Pts',(7.24760078045297,1.97432008494145,0.186501827635298));
#123262=CARTESIAN_POINT('Ctrl Pts',(7.48686869,1.973534152,0.443618325));
#123263=CARTESIAN_POINT('Ctrl Pts',(7.511178407,2.039276147,0.033347501));
#123264=CARTESIAN_POINT('Ctrl Pts',(7.490512549,2.104034486,-0.377123002));
#123265=CARTESIAN_POINT('Ctrl Pts',(7.247477043,1.973534152,0.191249878));
#123266=CARTESIAN_POINT('Ctrl Pts',(7.257957291,2.039276147,-0.20590259));
#123267=CARTESIAN_POINT('Ctrl Pts',(7.224978208,2.104034486,-0.601822151));
#123268=CARTESIAN_POINT('Origin',(-0.192953490786607,1.87507854258771,-0.0214644009727091));
#123269=CARTESIAN_POINT('Ctrl Pts',(7.4533717437585,2.10851071889274,-0.840123164227433));
#123270=CARTESIAN_POINT('Ctrl Pts',(7.45175390547986,2.10627260244634,-0.854010864545254));
#123271=CARTESIAN_POINT('Ctrl Pts',(7.45013606720136,2.104034486,-0.867898564863071));
#123272=CARTESIAN_POINT('Ctrl Pts',(7.40301689346621,2.038849851,-1.27237469374659));
#123273=CARTESIAN_POINT('Ctrl Pts',(7.31238483253978,1.973541827,-1.6693721570991));
#123274=CARTESIAN_POINT('Ctrl Pts',(7.22722190550252,2.10851071889274,-0.574886177926066));
#123275=CARTESIAN_POINT('Ctrl Pts',(7.2261000567513,2.10627260244633,-0.588354164463037));
#123276=CARTESIAN_POINT('Ctrl Pts',(7.224978208,2.104034486,-0.601822151));
#123277=CARTESIAN_POINT('Ctrl Pts',(7.192304617,2.038849851,-0.994074210999999));
#123278=CARTESIAN_POINT('Ctrl Pts',(7.117356647,1.973541827,-1.380483378));
#123279=CARTESIAN_POINT('',(7.11824828114546,1.9743200846023,-1.37587840931435));
#123280=CARTESIAN_POINT('Origin',(-0.197235680099277,2.0178567977005,0.0307684671074535));
#123281=CARTESIAN_POINT('Ctrl Pts',(7.36359498822142,2.01370168115123,-1.42389214575026));
#123282=CARTESIAN_POINT('Ctrl Pts',(7.32267071009206,2.00745398477611,-1.41584584484626));
#123283=CARTESIAN_POINT('Ctrl Pts',(7.28174227990175,2.00105345716874,-1.40781637803124));
#123284=CARTESIAN_POINT('Ctrl Pts',(7.19997384729897,1.98793719396908,-1.39181333278929));
#123285=CARTESIAN_POINT('Ctrl Pts',(7.15908664290256,1.98121389351294,-1.38383051380209));
#123286=CARTESIAN_POINT('Ctrl Pts',(7.11824828113933,1.97432008488866,-1.37587841117222));
#123287=CARTESIAN_POINT('Ctrl Pts',(7.407194687,1.973534152,-1.176208683));
#123288=CARTESIAN_POINT('Ctrl Pts',(7.342739956,2.039276147,-1.582113474));
#123289=CARTESIAN_POINT('Ctrl Pts',(7.23431823,2.104034486,-1.978544855));
#123290=CARTESIAN_POINT('Ctrl Pts',(7.119148127,1.973534152,-1.371214768));
#123291=CARTESIAN_POINT('Ctrl Pts',(7.044007313,2.039276147,-1.761334976));
#123292=CARTESIAN_POINT('Ctrl Pts',(6.926688259,2.104034486,-2.140908629));
#123293=CARTESIAN_POINT('Origin',(-0.19305672921978,1.87507853802671,0.0205167763710182));
#123294=CARTESIAN_POINT('Ctrl Pts',(7.09851440741733,2.10851071884374,-2.42273615646732));
#123295=CARTESIAN_POINT('Ctrl Pts',(7.09394894829215,2.10627260242184,-2.43595138254796));
#123296=CARTESIAN_POINT('Ctrl Pts',(7.08938348916698,2.104034486,-2.44916660862854));
#123297=CARTESIAN_POINT('Ctrl Pts',(6.95641552388265,2.038849851,-2.83405708175071));
#123298=CARTESIAN_POINT('Ctrl Pts',(6.78255967079359,1.973541827,-3.20228974984045));
#123299=CARTESIAN_POINT('Ctrl Pts',(6.93466993796179,2.10851071884374,-2.1150847329012));
#123300=CARTESIAN_POINT('Ctrl Pts',(6.93067909848083,2.10627260242184,-2.12799668095063));
#123301=CARTESIAN_POINT('Ctrl Pts',(6.926688259,2.104034486,-2.140908629));
#123302=CARTESIAN_POINT('Ctrl Pts',(6.810455961,2.038849851,-2.516966198));
#123303=CARTESIAN_POINT('Ctrl Pts',(6.654193685,1.973541827,-2.878229735));
#123304=CARTESIAN_POINT('',(6.65605440469576,1.97432008458747,-2.87392410309619));
#123305=CARTESIAN_POINT('Origin',(-0.186009880413163,2.01785677534532,0.0724488708947763));
#123306=CARTESIAN_POINT('Ctrl Pts',(6.88534350778262,2.01370168114798,-2.97355759548525));
#123307=CARTESIAN_POINT('Ctrl Pts',(6.84710573362344,2.00745398479343,-2.95690190251033));
#123308=CARTESIAN_POINT('Ctrl Pts',(6.80886028528214,2.00105345714027,-2.94026175731253));
#123309=CARTESIAN_POINT('Ctrl Pts',(6.73244373526343,1.98793719394154,-2.90705505827984));
#123310=CARTESIAN_POINT('Ctrl Pts',(6.69422852120976,1.98121389346513,-2.89046933272022));
#123311=CARTESIAN_POINT('Ctrl Pts',(6.65605440477926,1.97432008481482,-2.8739241051104));
#123312=CARTESIAN_POINT('Ctrl Pts',(6.981168493,1.973534152,-2.741037481));
#123313=CARTESIAN_POINT('Ctrl Pts',(6.830963147,2.039276147,-3.123596581));
#123314=CARTESIAN_POINT('Ctrl Pts',(6.639855232,2.104034486,-3.487452151));
#123315=CARTESIAN_POINT('Ctrl Pts',(6.657935758,1.973534152,-2.869562936));
#123316=CARTESIAN_POINT('Ctrl Pts',(6.500687381,2.039276147,-3.234409296));
#123317=CARTESIAN_POINT('Ctrl Pts',(6.30451406700001,2.104034486,-3.579888599));
#123318=CARTESIAN_POINT('Origin',(-0.184132620718572,1.87507855398852,0.0615385729578144));
#123319=CARTESIAN_POINT('Ctrl Pts',(6.41173842758946,2.10851071904183,-3.89206469701236));
#123320=CARTESIAN_POINT('Ctrl Pts',(6.40443882310531,2.10627260252088,-3.90398952022805));
#123321=CARTESIAN_POINT('Ctrl Pts',(6.39713921862116,2.104034486,-3.9159143434438));
#123322=CARTESIAN_POINT('Ctrl Pts',(6.18453989704751,2.038849851,-4.26322210937211));
#123323=CARTESIAN_POINT('Ctrl Pts',(5.93558955777856,1.973541827,-4.5854718333146));
#123324=CARTESIAN_POINT('Ctrl Pts',(6.31786051367224,2.10851071904183,-3.55638427522397));
#123325=CARTESIAN_POINT('Ctrl Pts',(6.31118729033618,2.10627260252088,-3.56813643711199));
#123326=CARTESIAN_POINT('Ctrl Pts',(6.304514067,2.104034486,-3.579888599));
#123327=CARTESIAN_POINT('Ctrl Pts',(6.11015795399999,2.038849851,-3.922167643));
#123328=CARTESIAN_POINT('Ctrl Pts',(5.879888021,1.973541827,-4.241393269));
#123329=CARTESIAN_POINT('',(5.88263082204013,1.9743200845952,-4.23758830006517));
#123330=CARTESIAN_POINT('Origin',(-0.166086502365517,2.01785676854295,0.110741551565458));
#123331=CARTESIAN_POINT('Ctrl Pts',(6.08514101783681,2.01370168113767,-4.38418279590154));
#123332=CARTESIAN_POINT('Ctrl Pts',(6.05137770310302,2.0074539847697,-4.3596965126326));
#123333=CARTESIAN_POINT('Ctrl Pts',(6.01760355145,2.00105345713783,-4.33522376406238));
#123334=CARTESIAN_POINT('Ctrl Pts',(5.95011203634988,1.98793719393057,-4.28636611987748));
#123335=CARTESIAN_POINT('Ctrl Pts',(5.9163557133816,1.98121389345838,-4.26195301803478));
#123336=CARTESIAN_POINT('Ctrl Pts',(5.88263082133317,1.97432008481336,-4.23758830206259));
#123337=CARTESIAN_POINT('Ctrl Pts',(6.22871062,1.973534152,-4.177698412));
#123338=CARTESIAN_POINT('Ctrl Pts',(5.999778092,2.039276147,-4.519023783));
#123339=CARTESIAN_POINT('Ctrl Pts',(5.734919982,2.104034486,-4.83329006));
#123340=CARTESIAN_POINT('Ctrl Pts',(5.885405712,1.973534152,-4.23373353));
#123341=CARTESIAN_POINT('Ctrl Pts',(5.653402532,2.039276147,-4.556246232));
#123342=CARTESIAN_POINT('Ctrl Pts',(5.387547803,2.104034486,-4.85147695700001));
#123343=CARTESIAN_POINT('Origin',(-0.166598777824842,1.87507851971097,0.0996829389749004));
#123344=CARTESIAN_POINT('Ctrl Pts',(5.42515668504128,2.1085107190361,-5.17940461950462));
#123345=CARTESIAN_POINT('Ctrl Pts',(5.41546425676681,2.10627260251802,-5.18948144778066));
#123346=CARTESIAN_POINT('Ctrl Pts',(5.40577182849224,2.104034486,-5.19955827605677));
#123347=CARTESIAN_POINT('Ctrl Pts',(5.12348205749383,2.038849851,-5.49304360974979));
#123348=CARTESIAN_POINT('Ctrl Pts',(4.81107787356319,1.973541827,-5.75424235046432));
#123349=CARTESIAN_POINT('Ctrl Pts',(5.40563495191362,2.1085107190361,-4.83139124279361));
#123350=CARTESIAN_POINT('Ctrl Pts',(5.39659137745674,2.10627260251802,-4.84143409989687));
#123351=CARTESIAN_POINT('Ctrl Pts',(5.38754780300001,2.104034486,-4.851476957));
#123352=CARTESIAN_POINT('Ctrl Pts',(5.124155752,2.038849851,-5.143972888));
#123353=CARTESIAN_POINT('Ctrl Pts',(4.830645328,1.973541827,-5.406233968));
#123354=CARTESIAN_POINT('',(4.83414196006164,1.97432008459502,-5.40310757779746));
#123355=CARTESIAN_POINT('Origin',(-0.138397360010162,2.01785674122855,0.14385621189966));
#123356=CARTESIAN_POINT('Ctrl Pts',(5.00040409687359,2.01370168117331,-5.58980848170412));
#123357=CARTESIAN_POINT('Ctrl Pts',(4.9726939767263,2.00745398480132,-5.5586365595206));
#123358=CARTESIAN_POINT('Ctrl Pts',(4.94497036347981,2.00105345717066,-5.52747552602794));
#123359=CARTESIAN_POINT('Ctrl Pts',(4.88955971169157,1.98793719396736,-5.46525146592909));
#123360=CARTESIAN_POINT('Ctrl Pts',(4.86184068816398,1.98121389354149,-5.43415251759514));
#123361=CARTESIAN_POINT('Ctrl Pts',(4.83414195911806,1.9743200849399,-5.40310758066947));
#123362=CARTESIAN_POINT('Ctrl Pts',(5.18500516,1.973534152,-5.419014808));
#123363=CARTESIAN_POINT('Ctrl Pts',(4.88805008300001,2.039276147,-5.703146456));
#123364=CARTESIAN_POINT('Ctrl Pts',(4.561826248,2.104034486,-5.953128697));
#123365=CARTESIAN_POINT('Ctrl Pts',(4.837680637,1.973534152,-5.39993945));
#123366=CARTESIAN_POINT('Ctrl Pts',(4.541770865,2.039276147,-5.66503815800001));
#123367=CARTESIAN_POINT('Ctrl Pts',(4.218665792,2.104034486,-5.896215645));
#123368=CARTESIAN_POINT('Origin',(-0.14127475023858,1.87507852894051,0.133166015454209));
#123369=CARTESIAN_POINT('Ctrl Pts',(4.18490064535655,2.10851071908492,-6.22456133880191));
#123370=CARTESIAN_POINT('Ctrl Pts',(4.17326860033842,2.10627260254242,-6.23231899093966));
#123371=CARTESIAN_POINT('Ctrl Pts',(4.16163655532026,2.104034486,-6.24007664307739));
#123372=CARTESIAN_POINT('Ctrl Pts',(3.82285589111545,2.038849851,-6.46601649628373));
#123373=CARTESIAN_POINT('Ctrl Pts',(3.46160553536181,1.973541827,-6.65395088997058));
#123374=CARTESIAN_POINT('Ctrl Pts',(4.24064790846959,2.10851071908492,-5.88048772585869));
#123375=CARTESIAN_POINT('Ctrl Pts',(4.22965685023479,2.10627260254242,-5.88835168542928));
#123376=CARTESIAN_POINT('Ctrl Pts',(4.218665792,2.104034486,-5.89621564500001));
#123377=CARTESIAN_POINT('Ctrl Pts',(3.898553722,2.038849851,-6.125251678));
#123378=CARTESIAN_POINT('Ctrl Pts',(3.555527029,1.973541827,-6.31828517400001));
#123379=CARTESIAN_POINT('',(3.55961399279641,1.97432008460497,-6.31598355033228));
#123380=CARTESIAN_POINT('Origin',(-0.104236902038956,2.01785675819182,0.170244306810112));
#123381=CARTESIAN_POINT('Ctrl Pts',(3.68185383783361,2.0137016811815,-6.53406093560932));
#123382=CARTESIAN_POINT('Ctrl Pts',(3.66149260672337,2.00745398479605,-6.49766093882905));
#123383=CARTESIAN_POINT('Ctrl Pts',(3.64111585723233,2.00105345715233,-6.46126867554373));
#123384=CARTESIAN_POINT('Ctrl Pts',(3.60037700929709,1.987937193926,-6.38858772696064));
#123385=CARTESIAN_POINT('Ctrl Pts',(3.57999139574734,1.9812138934833,-6.35225708390207));
#123386=CARTESIAN_POINT('Ctrl Pts',(3.55961399137252,1.97432008486823,-6.31598355218539));
#123387=CARTESIAN_POINT('Ctrl Pts',(3.898854622,1.973534152,-6.406944095));
#123388=CARTESIAN_POINT('Ctrl Pts',(3.547762284,2.039276147,-6.620596339));
#123389=CARTESIAN_POINT('Ctrl Pts',(3.175426589,2.104034486,-6.794605653));
#123390=CARTESIAN_POINT('Ctrl Pts',(3.563750991,1.973534152,-6.313650202));
#123391=CARTESIAN_POINT('Ctrl Pts',(3.217771039,2.039276147,-6.508939196));
#123392=CARTESIAN_POINT('Ctrl Pts',(2.852523658,2.104034486,-6.66525384200001));
#123393=CARTESIAN_POINT('Origin',(-0.109345230970199,1.87507853275137,0.160422895055139));
#123394=CARTESIAN_POINT('Ctrl Pts',(2.74896330201779,2.10851071888029,-6.97866448860505));
#123395=CARTESIAN_POINT('Ctrl Pts',(2.73593554242207,2.10627260244012,-6.9837402250486));
#123396=CARTESIAN_POINT('Ctrl Pts',(2.72290778282633,2.104034486,-6.98881596149228));
#123397=CARTESIAN_POINT('Ctrl Pts',(2.34347723180894,2.038849851,-7.13664563715395));
#123398=CARTESIAN_POINT('Ctrl Pts',(1.95027237023958,1.973541827,-7.24252808156075));
#123399=CARTESIAN_POINT('Ctrl Pts',(2.87737288146855,2.1085107188803,-6.65461913855489));
#123400=CARTESIAN_POINT('Ctrl Pts',(2.8649482697343,2.10627260244012,-6.65993649027745));
#123401=CARTESIAN_POINT('Ctrl Pts',(2.852523658,2.104034486,-6.665253842));
#123402=CARTESIAN_POINT('Ctrl Pts',(2.490659652,2.038849851,-6.820120508));
#123403=CARTESIAN_POINT('Ctrl Pts',(2.114156238,1.973541827,-6.934900389));
#123404=CARTESIAN_POINT('',(2.11864243188274,1.97432008458627,-6.93353115165319));
#123405=CARTESIAN_POINT('Origin',(-0.0652023946488164,2.01785671755945,
0.188671929289841));
#123406=CARTESIAN_POINT('Ctrl Pts',(2.19114418540924,2.01370168115789,-7.17278796232453));
#123407=CARTESIAN_POINT('Ctrl Pts',(2.17908391196442,2.00745398478866,-7.13286191455669));
#123408=CARTESIAN_POINT('Ctrl Pts',(2.16700682047428,2.00105345714571,-7.09294008337231));
#123409=CARTESIAN_POINT('Ctrl Pts',(2.14284467989806,1.98793719393754,-7.01320072699691));
#123410=CARTESIAN_POINT('Ctrl Pts',(2.13074568506423,1.98121389346194,-6.97333716964254));
#123411=CARTESIAN_POINT('Ctrl Pts',(2.11864243027874,1.97432008481779,-6.93353115313861));
#123412=CARTESIAN_POINT('Ctrl Pts',(2.430397975,1.973534152,-7.095291797));
#123413=CARTESIAN_POINT('Ctrl Pts',(2.041585064,2.039276147,-7.228474496));
#123414=CARTESIAN_POINT('Ctrl Pts',(1.640547511,2.104034486,-7.31837440000001));
#123415=CARTESIAN_POINT('Ctrl Pts',(2.12318431,1.973534152,-6.932141688));
#123416=CARTESIAN_POINT('Ctrl Pts',(1.743311816,2.039276147,-7.04848947199999));
#123417=CARTESIAN_POINT('Ctrl Pts',(1.353000687,2.104034486,-7.12263217800001));
#123418=CARTESIAN_POINT('Origin',(-0.0723025749741271,1.87507854736493,
0.180178118841089));
#123419=CARTESIAN_POINT('Ctrl Pts',(1.18448749191198,2.10851071904162,-7.40645304119193));
#123420=CARTESIAN_POINT('Ctrl Pts',(1.17067318028706,2.10627260252078,-7.40860952663705));
#123421=CARTESIAN_POINT('Ctrl Pts',(1.15685886866217,2.104034486,-7.4107660120822));
#123422=CARTESIAN_POINT('Ctrl Pts',(0.754520182233737,2.038849851,-7.47357316055654));
#123423=CARTESIAN_POINT('Ctrl Pts',(0.347746635845483,1.973541827,-7.4924527102599));
#123424=CARTESIAN_POINT('Ctrl Pts',(1.37955509720262,2.10851071904162,-7.1175879563888));
#123425=CARTESIAN_POINT('Ctrl Pts',(1.36627789210132,2.10627260252078,-7.12011006719445));
#123426=CARTESIAN_POINT('Ctrl Pts',(1.353000687,2.104034486,-7.122632178));
#123427=CARTESIAN_POINT('Ctrl Pts',(0.966305106,2.038849851,-7.196088082));
#123428=CARTESIAN_POINT('Ctrl Pts',(0.57392985,1.973541827,-7.22724736900001));
#123429=CARTESIAN_POINT('',(0.578605504968936,1.974320084601,-7.22687454289004));
#123430=CARTESIAN_POINT('Origin',(-0.0231191456018464,2.01785675782624,
0.198277636829115));
#123431=CARTESIAN_POINT('Ctrl Pts',(0.597979066411303,2.01370168115889,
-7.47612339587755));
#123432=CARTESIAN_POINT('Ctrl Pts',(0.594783675462212,2.00745398478028,
-7.4345381945658));
#123433=CARTESIAN_POINT('Ctrl Pts',(0.591570953207994,2.00105345716446,
-7.3929534961251));
#123434=CARTESIAN_POINT('Ctrl Pts',(0.585115314289111,1.98793719394626,
-7.30988425562794));
#123435=CARTESIAN_POINT('Ctrl Pts',(0.581868673498223,1.98121389348095,
-7.26835175999199));
#123436=CARTESIAN_POINT('Ctrl Pts',(0.57860550267337,1.97432008484254,-7.22687454419911));
#123437=CARTESIAN_POINT('Ctrl Pts',(0.84829862,1.973534152,-7.45187154));
#123438=CARTESIAN_POINT('Ctrl Pts',(0.439945595,2.039276147,-7.498357219));
#123439=CARTESIAN_POINT('Ctrl Pts',(0.028958256,2.104034486,-7.499944094));
#123440=CARTESIAN_POINT('Ctrl Pts',(0.58333989,1.973534152,-7.226493934));
#123441=CARTESIAN_POINT('Ctrl Pts',(0.18733727,2.039276147,-7.258460213));
#123442=CARTESIAN_POINT('Ctrl Pts',(-0.209787092,2.104034486,-7.246964149));
#123443=CARTESIAN_POINT('Origin',(-0.0318792104160436,1.87507852637965,
0.191508478928001));
#123444=CARTESIAN_POINT('Ctrl Pts',(-0.435373639053406,2.10851071889989,
-7.48792408298776));
#123445=CARTESIAN_POINT('Ctrl Pts',(-0.449328559925206,2.10627260244991,
-7.48706048234279));
#123446=CARTESIAN_POINT('Ctrl Pts',(-0.463283480797019,2.104034486,-7.4861968816978));
#123447=CARTESIAN_POINT('Ctrl Pts',(-0.869717392453361,2.038849851,-7.46104470839085));
#123448=CARTESIAN_POINT('Ctrl Pts',(-1.27103934506489,1.973541827,-7.39203857617524));
#123449=CARTESIAN_POINT('Ctrl Pts',(-0.182769151482024,2.10851071889989,
-7.24774627167939));
#123450=CARTESIAN_POINT('Ctrl Pts',(-0.196278121741014,2.10627260244991,
-7.24735521033965));
#123451=CARTESIAN_POINT('Ctrl Pts',(-0.209787092,2.104034486,-7.246964149));
#123452=CARTESIAN_POINT('Ctrl Pts',(-0.603232793,2.038849851,-7.235574576));
#123453=CARTESIAN_POINT('Ctrl Pts',(-0.993132859,1.973541827,-7.18165629400001));
#123454=CARTESIAN_POINT('',(-0.988486371605164,1.97432008459582,-7.18229731209575));
#123455=CARTESIAN_POINT('Origin',(0.0200451930811343,2.01785676284002,0.198611868378687));
#123456=CARTESIAN_POINT('Ctrl Pts',(-1.02314688972635,2.01370168116698,
-7.42988360828839));
#123457=CARTESIAN_POINT('Ctrl Pts',(-1.01732798509792,2.00745398479636,
-7.38858373133107));
#123458=CARTESIAN_POINT('Ctrl Pts',(-1.01152611461238,2.00105345715369,
-7.34728061954436));
#123459=CARTESIAN_POINT('Ctrl Pts',(-0.999973392743274,1.98793719394499,
-7.26476572021039));
#123460=CARTESIAN_POINT('Ctrl Pts',(-0.99421586977725,1.9812138934727,-7.22350629936079));
#123461=CARTESIAN_POINT('Ctrl Pts',(-0.988486373856812,1.97432008483443,
-7.18229731246988));
#123462=CARTESIAN_POINT('Ctrl Pts',(-0.773466236,1.973534152,-7.460010052));
#123463=CARTESIAN_POINT('Ctrl Pts',(-1.182265241,2.039276147,-7.417625092));
#123464=CARTESIAN_POINT('Ctrl Pts',(-1.583985056,2.104034486,-7.330824738));
#123465=CARTESIAN_POINT('Ctrl Pts',(-0.983780854,1.973534152,-7.182943354));
#123466=CARTESIAN_POINT('Ctrl Pts',(-1.377396959,2.039276147,-7.129033422));
#123467=CARTESIAN_POINT('Ctrl Pts',(-1.76276546,2.104034486,-7.032436131));
#123468=CARTESIAN_POINT('Origin',(0.010034762528979,1.87507853927421,0.193884179309698));
#123469=CARTESIAN_POINT('Ctrl Pts',(-2.03487718223917,2.10851071886228,
-7.21926811592231));
#123470=CARTESIAN_POINT('Ctrl Pts',(-2.04832019608257,2.1062726024311,-7.21542481034134));
#123471=CARTESIAN_POINT('Ctrl Pts',(-2.0617632099259,2.104034486,-7.21158150476034));
#123472=CARTESIAN_POINT('Ctrl Pts',(-2.45328794854016,2.038849851,-7.09964609871615));
#123473=CARTESIAN_POINT('Ctrl Pts',(-2.83039293831185,1.973541827,-6.9459809348642));
#123474=CARTESIAN_POINT('Ctrl Pts',(-1.73654731743755,2.10851071886228,
-7.03900802662101));
#123475=CARTESIAN_POINT('Ctrl Pts',(-1.74965638871877,2.1062726024311,-7.03572207881043));
#123476=CARTESIAN_POINT('Ctrl Pts',(-1.76276546,2.104034486,-7.032436131));
#123477=CARTESIAN_POINT('Ctrl Pts',(-2.144564197,2.038849851,-6.936733644));
#123478=CARTESIAN_POINT('Ctrl Pts',(-2.51375778,1.973541827,-6.800258953));
#123479=CARTESIAN_POINT('',(-2.50935772461844,1.97432008459731,-6.80188384142906));
#123480=CARTESIAN_POINT('Origin',(0.0622722465869113,2.01785673676985,0.189659333559888));
#123481=CARTESIAN_POINT('Ctrl Pts',(-2.59643163413031,2.01370168117248,
-7.03623072135717));
#123482=CARTESIAN_POINT('Ctrl Pts',(-2.58187051952417,2.00745398481506,
-6.99714730511095));
#123483=CARTESIAN_POINT('Ctrl Pts',(-2.56732534538734,2.0010534571731,-6.95805706773284));
#123484=CARTESIAN_POINT('Ctrl Pts',(-2.53830445549343,1.98793719398528,
-6.87995481461199));
#123485=CARTESIAN_POINT('Ctrl Pts',(-2.52381198434064,1.98121389351532,
-6.84089771329464));
#123486=CARTESIAN_POINT('Ctrl Pts',(-2.50935772681519,1.97432008487983,
-6.80188384184303));
#123487=CARTESIAN_POINT('Ctrl Pts',(-2.35906467,1.973534152,-7.119326786));
#123488=CARTESIAN_POINT('Ctrl Pts',(-2.749194668,2.039276147,-6.990053061));
#123489=CARTESIAN_POINT('Ctrl Pts',(-3.122862986,2.104034486,-6.81892416500001));
#123490=CARTESIAN_POINT('Ctrl Pts',(-2.504901099,1.973534152,-6.80352632700001));
#123491=CARTESIAN_POINT('Ctrl Pts',(-2.877725636,2.039276147,-6.666260952));
#123492=CARTESIAN_POINT('Ctrl Pts',(-3.233318874,2.104034486,-6.489079215));
#123493=CARTESIAN_POINT('Origin',(0.0514794804254071,1.87507852070844,0.187194023090833));
#123494=CARTESIAN_POINT('Ctrl Pts',(-3.53923212928303,2.1085107188304,-6.61304719479122));
#123495=CARTESIAN_POINT('Ctrl Pts',(-3.5515346557452,2.10627260241517,-6.60640389301813));
#123496=CARTESIAN_POINT('Ctrl Pts',(-3.56383718220737,2.104034486,-6.59976059124501));
#123497=CARTESIAN_POINT('Ctrl Pts',(-3.92214548626936,2.038849851,-6.40627592782908));
#123498=CARTESIAN_POINT('Ctrl Pts',(-4.25740050355622,1.973541827,-6.17513694492405));
#123499=CARTESIAN_POINT('Ctrl Pts',(-3.20912646050364,2.10851071883041,
-6.50113358894312));
#123500=CARTESIAN_POINT('Ctrl Pts',(-3.22122266725182,2.10627260241517,
-6.4951064019715));
#123501=CARTESIAN_POINT('Ctrl Pts',(-3.233318874,2.104034486,-6.489079215));
#123502=CARTESIAN_POINT('Ctrl Pts',(-3.585618163,2.038849851,-6.313538756));
#123503=CARTESIAN_POINT('Ctrl Pts',(-3.91684218,1.973541827,-6.100889061));
#123504=CARTESIAN_POINT('',(-3.91289429922261,1.97432008459373,-6.10342184278226));
#123505=CARTESIAN_POINT('Origin',(0.10158756789478,2.01785674361773,0.171838632592149));
#123506=CARTESIAN_POINT('Ctrl Pts',(-4.04831012087656,2.01370168115928,
-6.31357150580349));
#123507=CARTESIAN_POINT('Ctrl Pts',(-4.02568765781778,2.00745398480099,
-6.27853204729133));
#123508=CARTESIAN_POINT('Ctrl Pts',(-4.00307929618702,2.00105345714537,
-6.24348250033079));
#123509=CARTESIAN_POINT('Ctrl Pts',(-3.95794722285307,1.98793719394509,
-6.1734448678984));
#123510=CARTESIAN_POINT('Ctrl Pts',(-3.93539745539647,1.98121389347014,
-6.13841635280565));
#123511=CARTESIAN_POINT('Ctrl Pts',(-3.91289430129604,1.97432008482122,
-6.10342184208376));
#123512=CARTESIAN_POINT('Ctrl Pts',(-3.834355862,1.973534152,-6.445751711));
#123513=CARTESIAN_POINT('Ctrl Pts',(-4.187574808,2.039276147,-6.235633917));
#123514=CARTESIAN_POINT('Ctrl Pts',(-4.515719315,2.104034486,-5.988178277));
#123515=CARTESIAN_POINT('Ctrl Pts',(-3.908894953,1.973534152,-6.10598397));
#123516=CARTESIAN_POINT('Ctrl Pts',(-4.243495061,2.039276147,-5.891781529));
#123517=CARTESIAN_POINT('Ctrl Pts',(-4.552685891,2.104034486,-5.64230016800001));
#123518=CARTESIAN_POINT('Origin',(0.0905172887651684,1.87507854014182,0.171751205712217));
#123519=CARTESIAN_POINT('Ctrl Pts',(-4.87809651566979,2.10851071879243,
-5.69760753822029));
#123520=CARTESIAN_POINT('Ctrl Pts',(-4.88868330231458,2.10627260239619,
-5.68847487366332));
#123521=CARTESIAN_POINT('Ctrl Pts',(-4.89927008895948,2.104034486,-5.67934220910619));
#123522=CARTESIAN_POINT('Ctrl Pts',(-5.20760786104499,2.038849851,-5.41335541469936));
#123523=CARTESIAN_POINT('Ctrl Pts',(-5.48533675284584,1.973541827,-5.11555041405222));
#123524=CARTESIAN_POINT('Ctrl Pts',(-4.53165041691484,2.10851071879244,
-5.65927337102369));
#123525=CARTESIAN_POINT('Ctrl Pts',(-4.54216815395742,2.10627260239619,
-5.65078676951184));
#123526=CARTESIAN_POINT('Ctrl Pts',(-4.552685891,2.104034486,-5.642300168));
#123527=CARTESIAN_POINT('Ctrl Pts',(-4.859012609,2.038849851,-5.395129814));
#123528=CARTESIAN_POINT('Ctrl Pts',(-5.136779394,1.973541827,-5.116248377));
#123529=CARTESIAN_POINT('',(-5.13346828566157,1.97432008459591,-5.11957062092842));
#123530=CARTESIAN_POINT('Origin',(0.136152707978381,2.01785677842596,0.145982787016607));
#123531=CARTESIAN_POINT('Ctrl Pts',(-5.31089412599479,2.01370168116644,
-5.29569670360671));
#123532=CARTESIAN_POINT('Ctrl Pts',(-5.28126811575688,2.00745398480778,
-5.26633960900817));
#123533=CARTESIAN_POINT('Ctrl Pts',(-5.2516537084966,2.0010534571446,-5.23696963039117));
#123534=CARTESIAN_POINT('Ctrl Pts',(-5.19252077725244,1.98793719395353,
-5.17827150052631));
#123535=CARTESIAN_POINT('Ctrl Pts',(-5.16296811547313,1.98121389348676,
-5.1489094660589));
#123536=CARTESIAN_POINT('Ctrl Pts',(-5.1334682871504,1.97432008485722,-5.11957062045771));
#123537=CARTESIAN_POINT('Ctrl Pts',(-5.130356836,1.973534152,-5.470780451));
#123538=CARTESIAN_POINT('Ctrl Pts',(-5.430148604,2.039276147,-5.189643461));
#123539=CARTESIAN_POINT('Ctrl Pts',(-5.69742562700001,2.104034486,-4.877431827));
#123540=CARTESIAN_POINT('Ctrl Pts',(-5.130113223,1.973534152,-5.122932589));
#123541=CARTESIAN_POINT('Ctrl Pts',(-5.41084337400001,2.039276147,-4.841808949));
#123542=CARTESIAN_POINT('Ctrl Pts',(-5.659174375,2.104034486,-4.531693435));
#123543=CARTESIAN_POINT('Origin',(0.125322351826307,1.87507854796951,0.148277099444511));
#123544=CARTESIAN_POINT('Ctrl Pts',(-5.98886652981042,2.10851071902134,
-4.51575408564252));
#123545=CARTESIAN_POINT('Ctrl Pts',(-5.99724255079195,2.10627260251063,
-4.50455909097158));
#123546=CARTESIAN_POINT('Ctrl Pts',(-6.00561857177351,2.104034486,-4.49336409630082));
#123547=CARTESIAN_POINT('Ctrl Pts',(-6.24956828030743,2.038849851,-4.16731241937841));
#123548=CARTESIAN_POINT('Ctrl Pts',(-6.45678475223118,1.973541827,-3.81676643166152));
#123549=CARTESIAN_POINT('Ctrl Pts',(-5.64227943465445,2.10851071902134,
-4.55279182017937));
#123550=CARTESIAN_POINT('Ctrl Pts',(-5.65072690482716,2.10627260251063,
-4.5422426275897));
#123551=CARTESIAN_POINT('Ctrl Pts',(-5.659174375,2.104034486,-4.531693435));
#123552=CARTESIAN_POINT('Ctrl Pts',(-5.905205025,2.038849851,-4.224450597));
#123553=CARTESIAN_POINT('Ctrl Pts',(-6.116526512,1.973541827,-3.892377606));
#123554=CARTESIAN_POINT('',(-6.11400699946281,1.97432008458578,-3.89633396849977));
#123555=CARTESIAN_POINT('Origin',(0.164351554709555,2.01785674952642,0.113301003398673));
#123556=CARTESIAN_POINT('Ctrl Pts',(-6.32514662409162,2.01370168115646,
-4.03020100952011));
#123557=CARTESIAN_POINT('Ctrl Pts',(-6.28990234594244,2.00745398478208,
-4.0078989838217));
#123558=CARTESIAN_POINT('Ctrl Pts',(-6.25466663006614,2.00105345714523,
-3.98558188120025));
#123559=CARTESIAN_POINT('Ctrl Pts',(-6.18429783112559,1.98793719392257,
-3.9409679131739));
#123560=CARTESIAN_POINT('Ctrl Pts',(-6.14912412478396,1.98121389345093,
-3.91864529551827));
#123561=CARTESIAN_POINT('Ctrl Pts',(-6.11400700156398,1.97432008480395,
-3.89633396700648));
#123562=CARTESIAN_POINT('Ctrl Pts',(-6.18646802600001,1.973534152,-4.240001576));
#123563=CARTESIAN_POINT('Ctrl Pts',(-6.418814686,2.039276147,-3.900991045));
#123564=CARTESIAN_POINT('Ctrl Pts',(-6.612726649,2.104034486,-3.538622086));
#123565=CARTESIAN_POINT('Ctrl Pts',(-6.111453101,1.973534152,-3.900338574));
#123566=CARTESIAN_POINT('Ctrl Pts',(-6.325186664,2.039276147,-3.565438765));
#123567=CARTESIAN_POINT('Ctrl Pts',(-6.50104615600001,2.104034486,-3.209189754));
#123568=CARTESIAN_POINT('Origin',(0.154267558917515,1.87507849351964,0.117869865208854));
#123569=CARTESIAN_POINT('Ctrl Pts',(-6.81960380217781,2.1085107190505,-3.12274899058748));
#123570=CARTESIAN_POINT('Ctrl Pts',(-6.82537740354237,2.10627260252522,
-3.11001513168578));
#123571=CARTESIAN_POINT('Ctrl Pts',(-6.83115100490693,2.104034486,-3.09728127278417));
#123572=CARTESIAN_POINT('Ctrl Pts',(-6.99930583212112,2.038849851,-2.72641052709678));
#123573=CARTESIAN_POINT('Ctrl Pts',(-7.12632067321807,1.973541827,-2.33951469307138));
#123574=CARTESIAN_POINT('Ctrl Pts',(-6.48908173904204,2.1085107190505,-3.23342678355775));
#123575=CARTESIAN_POINT('Ctrl Pts',(-6.49506394752096,2.10627260252522,
-3.22130826877888));
#123576=CARTESIAN_POINT('Ctrl Pts',(-6.501046156,2.104034486,-3.209189754));
#123577=CARTESIAN_POINT('Ctrl Pts',(-6.675276618,2.038849851,-2.856240766));
#123578=CARTESIAN_POINT('Ctrl Pts',(-6.810271649,1.973541827,-2.486503584));
#123579=CARTESIAN_POINT('',(-6.80866154187226,1.97432008459362,-2.49090906853672));
#123580=CARTESIAN_POINT('Origin',(0.184865071285617,2.01785679395891,0.0753211970401979));
#123581=CARTESIAN_POINT('Ctrl Pts',(-7.04364229597177,2.0137016811527,-2.57625759581218));
#123582=CARTESIAN_POINT('Ctrl Pts',(-7.00442773317143,2.00745398478086,
-2.56205345706551));
#123583=CARTESIAN_POINT('Ctrl Pts',(-6.96521829159588,2.00105345718054,
-2.54783275332503));
#123584=CARTESIAN_POINT('Ctrl Pts',(-6.8869039917953,1.98793719395232,-2.51938904670658));
#123585=CARTESIAN_POINT('Ctrl Pts',(-6.8477539241966,1.98121389345868,-2.50514962650101));
#123586=CARTESIAN_POINT('Ctrl Pts',(-6.80866154374563,1.97432008478381,
-2.49090906776778));
#123587=CARTESIAN_POINT('Ctrl Pts',(-6.953306846,1.973534152,-2.810964941));
#123588=CARTESIAN_POINT('Ctrl Pts',(-7.107344128,2.039276147,-2.429932623));
#123589=CARTESIAN_POINT('Ctrl Pts',(-7.21882392200001,2.104034486,-2.03435031));
#123590=CARTESIAN_POINT('Ctrl Pts',(-6.807028224,1.973534152,-2.495369062));
#123591=CARTESIAN_POINT('Ctrl Pts',(-6.943771255,2.039276147,-2.122352626));
#123592=CARTESIAN_POINT('Ctrl Pts',(-7.038936244,2.104034486,-1.736627927));
#123593=CARTESIAN_POINT('Origin',(0.175999427533899,1.87507851689146,0.0819511757973274));
#123594=CARTESIAN_POINT('Ctrl Pts',(-7.33146397982346,2.10851071905646,
-1.58372762280809));
#123595=CARTESIAN_POINT('Ctrl Pts',(-7.33436519435819,2.10627260252819,
-1.57005032079825));
#123596=CARTESIAN_POINT('Ctrl Pts',(-7.33726640889282,2.104034486,-1.55637301878848));
#123597=CARTESIAN_POINT('Ctrl Pts',(-7.4217636225605,2.038849851,-1.1580247075818));
#123598=CARTESIAN_POINT('Ctrl Pts',(-7.46263775903092,1.973541827,-0.752869847803945));
#123599=CARTESIAN_POINT('Ctrl Pts',(-7.03246179338692,2.10851071905645,
-1.7628703042967));
#123600=CARTESIAN_POINT('Ctrl Pts',(-7.03569901869346,2.10627260252819,
-1.74974911564838));
#123601=CARTESIAN_POINT('Ctrl Pts',(-7.03893624400001,2.104034486,-1.736627927));
#123602=CARTESIAN_POINT('Ctrl Pts',(-7.13321969499999,2.038849851,-1.354476291));
#123603=CARTESIAN_POINT('Ctrl Pts',(-7.185576052,1.973541827,-0.964363417));
#123604=CARTESIAN_POINT('',(-7.1849506379579,1.97432008461106,-0.969012030082719));
#123605=CARTESIAN_POINT('Origin',(0.196735211445732,2.01785674944065,0.0338197687879882));
#123606=CARTESIAN_POINT('Ctrl Pts',(-7.43278508283959,2.01370168115849,
-1.00185123952923));
#123607=CARTESIAN_POINT('Ctrl Pts',(-7.39143386477347,2.00745398478806,
-0.996409157496566));
#123608=CARTESIAN_POINT('Ctrl Pts',(-7.35008408696195,2.00105345715456,
-0.990949796784439));
#123609=CARTESIAN_POINT('Ctrl Pts',(-7.26748617586181,1.98793719395952,
-0.980006347682499));
#123610=CARTESIAN_POINT('Ctrl Pts',(-7.22619036093368,1.98121389353513,
-0.97451594447279));
#123611=CARTESIAN_POINT('Ctrl Pts',(-7.18495063964874,1.97432008493794,
-0.969012028304344));
#123612=CARTESIAN_POINT('Ctrl Pts',(-7.395016767,1.973534152,-1.250490709));
#123613=CARTESIAN_POINT('Ctrl Pts',(-7.463542058,2.039276147,-0.845253253));
#123614=CARTESIAN_POINT('Ctrl Pts',(-7.487377012,2.104034486,-0.434954574));
#123615=CARTESIAN_POINT('Ctrl Pts',(-7.18431427300001,1.973534152,-0.973718867));
#123616=CARTESIAN_POINT('Ctrl Pts',(-7.237672821,2.039276147,-0.580027638));
#123617=CARTESIAN_POINT('Ctrl Pts',(-7.247693496,2.104034486,-0.182863309));
#123618=CARTESIAN_POINT('Origin',(0.189501763679538,1.87507855285121,0.0422005216901355));
#123619=CARTESIAN_POINT('Ctrl Pts',(-7.50051305040893,2.10851071891129,
0.029347089545044));
#123620=CARTESIAN_POINT('Ctrl Pts',(-7.50040622050944,2.10627260245561,
0.043328298730679));
#123621=CARTESIAN_POINT('Ctrl Pts',(-7.50029939060997,2.104034486,0.0573095079163131));
#123622=CARTESIAN_POINT('Ctrl Pts',(-7.4971879939768,2.038849851,0.464509059725814));
#123623=CARTESIAN_POINT('Ctrl Pts',(-7.45001019763226,1.973541827,0.868978355344865));
#123624=CARTESIAN_POINT('Ctrl Pts',(-7.24701174985858,2.10851071891129,
-0.209883968783856));
#123625=CARTESIAN_POINT('Ctrl Pts',(-7.24735262292936,2.10627260245561,
-0.196373638891925));
#123626=CARTESIAN_POINT('Ctrl Pts',(-7.247693496,2.104034486,-0.182863309));
#123627=CARTESIAN_POINT('Ctrl Pts',(-7.257621347,2.038849851,0.21062199));
#123628=CARTESIAN_POINT('Ctrl Pts',(-7.224890905,1.973541827,0.60286931));
#123629=CARTESIAN_POINT('',(-7.22527942719973,1.97432008458926,0.598194933891309));
#123630=CARTESIAN_POINT('Origin',(0.199405651581389,2.01785674870612,-0.00926317386782061));
#123631=CARTESIAN_POINT('Ctrl Pts',(-7.47437909993499,2.01370168117242,
0.619400567375759));
#123632=CARTESIAN_POINT('Ctrl Pts',(-7.43282476363654,2.00745398479686,
0.615826126927519));
#123633=CARTESIAN_POINT('Ctrl Pts',(-7.39126811926572,2.00105345711966,
0.612268870771427));
#123634=CARTESIAN_POINT('Ctrl Pts',(-7.30824878339747,1.98793719390629,
0.605200358586722));
#123635=CARTESIAN_POINT('Ctrl Pts',(-7.26673816734005,1.98121389347822,
0.601685019581431));
#123636=CARTESIAN_POINT('Ctrl Pts',(-7.22527942859502,1.97432008487502,
0.598194936057672));
#123637=CARTESIAN_POINT('Ctrl Pts',(-7.49094392300001,1.973534152,0.368455079));
#123638=CARTESIAN_POINT('Ctrl Pts',(-7.470753056,2.039276147,0.77894922));
#123639=CARTESIAN_POINT('Ctrl Pts',(-7.405828674,2.104034486,1.184779155));
#123640=CARTESIAN_POINT('Ctrl Pts',(-7.22566977100001,1.973534152,0.593461341));
#123641=CARTESIAN_POINT('Ctrl Pts',(-7.193148849,2.039276147,0.989418798));
#123642=CARTESIAN_POINT('Ctrl Pts',(-7.11755665600001,2.104034486,1.379451795));
#123643=CARTESIAN_POINT('Origin',(0.194143031294935,1.8750785217705,0.000476651582254073));
#123644=CARTESIAN_POINT('Ctrl Pts',(-7.31884646687648,2.10851071898058,
1.6410495620188));
#123645=CARTESIAN_POINT('Ctrl Pts',(-7.31573658785984,2.10627260249025,
1.65468093326815));
#123646=CARTESIAN_POINT('Ctrl Pts',(-7.3126267088431,2.104034486,1.6683123045175));
#123647=CARTESIAN_POINT('Ctrl Pts',(-7.22205218804354,2.038849851,2.06532289950042));
#123648=CARTESIAN_POINT('Ctrl Pts',(-7.08902844015126,1.973541827,2.45019409568082));
#123649=CARTESIAN_POINT('Ctrl Pts',(-7.12269949194147,2.10851071898057,
1.35291630753869));
#123650=CARTESIAN_POINT('Ctrl Pts',(-7.12012807397073,2.10627260249025,
1.36618405126933));
#123651=CARTESIAN_POINT('Ctrl Pts',(-7.117556656,2.104034486,1.379451795));
#123652=CARTESIAN_POINT('Ctrl Pts',(-7.042664691,2.038849851,1.765871821));
#123653=CARTESIAN_POINT('Ctrl Pts',(-6.92637789,1.973541827,2.141912539));
#123654=CARTESIAN_POINT('',(-6.92776218145332,1.97432008456834,2.13743096775303));
#123655=CARTESIAN_POINT('Origin',(0.192752513283734,2.01785674458455,-0.0519129632658388));
#123656=CARTESIAN_POINT('Ctrl Pts',(-7.16647945765253,2.01370168118037,
2.21168989111538));
#123657=CARTESIAN_POINT('Ctrl Pts',(-7.12666503765107,2.00745398480427,
2.19926606514373));
#123658=CARTESIAN_POINT('Ctrl Pts',(-7.08684466969444,2.00105345716807,
2.18685852563209));
#123659=CARTESIAN_POINT('Ctrl Pts',(-7.00728580085381,1.98793719394073,
2.16210856820885));
#123660=CARTESIAN_POINT('Ctrl Pts',(-6.96750137361793,1.9812138934618,2.14975186042709));
#123661=CARTESIAN_POINT('Ctrl Pts',(-6.92776218168722,1.97432008480815,
2.13743096977317));
#123662=CARTESIAN_POINT('Ctrl Pts',(-7.236602866,1.973534152,1.970172316));
#123663=CARTESIAN_POINT('Ctrl Pts',(-7.128639944,2.039276147,2.366728893));
#123664=CARTESIAN_POINT('Ctrl Pts',(-6.977992019,2.104034486,2.749113927));
#123665=CARTESIAN_POINT('Ctrl Pts',(-6.929160981,1.973534152,2.132891956));
#123666=CARTESIAN_POINT('Ctrl Pts',(-6.812281231,2.039276147,2.512601111));
#123667=CARTESIAN_POINT('Ctrl Pts',(-6.654610777,2.104034486,2.877265266));
#123668=CARTESIAN_POINT('Origin',(0.189706688252155,1.87507854824575,-0.0412695740778762));
#123669=CARTESIAN_POINT('Ctrl Pts',(-6.79495875646654,2.10851071886654,
3.17601838304026));
#123670=CARTESIAN_POINT('Ctrl Pts',(-6.78899124297289,2.10627260243327,
3.18866252798723));
#123671=CARTESIAN_POINT('Ctrl Pts',(-6.78302372947934,2.104034486,3.20130667293425));
#123672=CARTESIAN_POINT('Ctrl Pts',(-6.6092212484499,2.038849851,3.56956453521749));
#123673=CARTESIAN_POINT('Ctrl Pts',(-6.39657159139358,1.973541827,3.91684148375803));
#123674=CARTESIAN_POINT('Ctrl Pts',(-6.66533772140354,2.10851071886654,
2.85245572181685));
#123675=CARTESIAN_POINT('Ctrl Pts',(-6.65997424920171,2.10627260243327,
2.86486049390841));
#123676=CARTESIAN_POINT('Ctrl Pts',(-6.654610777,2.104034486,2.877265266));
#123677=CARTESIAN_POINT('Ctrl Pts',(-6.49840086199999,2.038849851,3.238551448));
#123678=CARTESIAN_POINT('Ctrl Pts',(-6.303995142,1.973541827,3.580802319));
#123679=CARTESIAN_POINT('',(-6.30631047548681,1.97432008458569,3.57672310566895));
#123680=CARTESIAN_POINT('Origin',(0.177086448535698,2.01785677518475,-0.0921354177511241));
#123681=CARTESIAN_POINT('Ctrl Pts',(-6.52348320097802,2.01370168114992,
3.70056305449002));
#123682=CARTESIAN_POINT('Ctrl Pts',(-6.48727037534077,2.00745398478357,
3.67987076733538));
#123683=CARTESIAN_POINT('Ctrl Pts',(-6.45104823951118,2.00105345713091,
3.65919310715007));
#123684=CARTESIAN_POINT('Ctrl Pts',(-6.37866992196166,1.98793719393924,
3.61791898507919));
#123685=CARTESIAN_POINT('Ctrl Pts',(-6.34247195938141,1.98121389348754,
3.59729869452439));
#123686=CARTESIAN_POINT('Ctrl Pts',(-6.30631047486903,1.97432008487082,
3.57672310798306));
#123687=CARTESIAN_POINT('Ctrl Pts',(-6.643886303,1.973534152,3.479766486));
#123688=CARTESIAN_POINT('Ctrl Pts',(-6.453199552,2.039276147,3.843842954));
#123689=CARTESIAN_POINT('Ctrl Pts',(-6.223872212,2.104034486,4.184903187));
#123690=CARTESIAN_POINT('Ctrl Pts',(-6.308652325,1.973534152,3.572590914));
#123691=CARTESIAN_POINT('Ctrl Pts',(-6.112878915,2.039276147,3.918296989));
#123692=CARTESIAN_POINT('Ctrl Pts',(-5.880502694,2.104034486,4.240541011));
#123693=CARTESIAN_POINT('Origin',(0.176399700379388,1.87507855895761,-0.0810860420883436));
#123694=CARTESIAN_POINT('Ctrl Pts',(-5.95334632705935,2.10851071891587,
4.56248011285926));
#123695=CARTESIAN_POINT('Ctrl Pts',(-5.94480021321551,2.1062726024579,4.57354580585008));
#123696=CARTESIAN_POINT('Ctrl Pts',(-5.93625409937179,2.104034486,4.58461149884087));
#123697=CARTESIAN_POINT('Ctrl Pts',(-5.68735046899805,2.038849851,4.90689730129712));
#123698=CARTESIAN_POINT('Ctrl Pts',(-5.40501816371079,1.973541827,5.20034171741082));
#123699=CARTESIAN_POINT('Ctrl Pts',(-5.89631216717291,2.10851071891587,
4.21861747586753));
#123700=CARTESIAN_POINT('Ctrl Pts',(-5.88840743058648,2.1062726024579,4.2295792434338));
#123701=CARTESIAN_POINT('Ctrl Pts',(-5.880502694,2.104034486,4.240541011));
#123702=CARTESIAN_POINT('Ctrl Pts',(-5.650279031,2.038849851,4.559800009));
#123703=CARTESIAN_POINT('Ctrl Pts',(-5.386844588,1.973541827,4.852257761));
#123704=CARTESIAN_POINT('',(-5.3899827002885,1.97432008460163,4.84877164614663));
#123705=CARTESIAN_POINT('Origin',(0.153139825866802,2.01785673863234,-0.128049668616968));
#123706=CARTESIAN_POINT('Ctrl Pts',(-5.57545611982729,2.0137016811512,5.01640200221225));
#123707=CARTESIAN_POINT('Ctrl Pts',(-5.5445381600034,2.00745398477771,4.98840880214805));
#123708=CARTESIAN_POINT('Ctrl Pts',(-5.51360796327672,2.00105345711284,
4.96042788561598));
#123709=CARTESIAN_POINT('Ctrl Pts',(-5.45179452686102,1.98793719392029,
4.90455953070735));
#123710=CARTESIAN_POINT('Ctrl Pts',(-5.4208756055621,1.98121389347575,4.87663983909214));
#123711=CARTESIAN_POINT('Ctrl Pts',(-5.3899826994675,1.97432008486875,4.84877164802182));
#123712=CARTESIAN_POINT('Ctrl Pts',(-5.740508999,1.973534152,4.826650643));
#123713=CARTESIAN_POINT('Ctrl Pts',(-5.476014721,2.039276147,5.14122319));
#123714=CARTESIAN_POINT('Ctrl Pts',(-5.17873105800001,2.104034486,5.42501102500001));
#123715=CARTESIAN_POINT('Ctrl Pts',(-5.393158098,1.973534152,4.845239491));
#123716=CARTESIAN_POINT('Ctrl Pts',(-5.127645174,2.039276147,5.140777654));
#123717=CARTESIAN_POINT('Ctrl Pts',(-4.831428841,2.104034486,5.405533772));
#123718=CARTESIAN_POINT('Origin',(0.154844449314781,1.87507851562995,-0.117110982067028));
#123719=CARTESIAN_POINT('Ctrl Pts',(-4.83336204015693,2.10851071895189,
5.73560534432582));
#123720=CARTESIAN_POINT('Ctrl Pts',(-4.82263693273945,2.10627260247597,
5.744575165774));
#123721=CARTESIAN_POINT('Ctrl Pts',(-4.81191182532195,2.104034486,5.75354498722217));
#123722=CARTESIAN_POINT('Ctrl Pts',(-4.49954550307968,2.038849851,6.01478900351599));
#123723=CARTESIAN_POINT('Ctrl Pts',(-4.16073209479057,1.973541827,6.24067975220858));
#123724=CARTESIAN_POINT('Ctrl Pts',(-4.85158160963388,2.10851071895189,
5.38752136625703));
#123725=CARTESIAN_POINT('Ctrl Pts',(-4.84150522531699,2.10627260247597,
5.39652756912856));
#123726=CARTESIAN_POINT('Ctrl Pts',(-4.83142884100001,2.104034486,5.405533772));
#123727=CARTESIAN_POINT('Ctrl Pts',(-4.537956432,2.038849851,5.667837389));
#123728=CARTESIAN_POINT('Ctrl Pts',(-4.217811169,1.973541827,5.896827024));
#123729=CARTESIAN_POINT('',(-4.22162532483266,1.9743200846106,5.89409701316203));
#123730=CARTESIAN_POINT('Origin',(0.122032535617409,2.01785676375151,-0.157976378280066));
#123731=CARTESIAN_POINT('Ctrl Pts',(-4.36672690769356,2.01370168112843,
6.09767956762301));
#123732=CARTESIAN_POINT('Ctrl Pts',(-4.34254950320055,2.00745398476853,
6.06369438560014));
#123733=CARTESIAN_POINT('Ctrl Pts',(-4.31835750742411,2.00105345714589,
6.02971856953371));
#123734=CARTESIAN_POINT('Ctrl Pts',(-4.26999927977852,1.98793719394933,
5.96186832408102));
#123735=CARTESIAN_POINT('Ctrl Pts',(-4.24580513408982,1.98121389347898,
5.92795472514188));
#123736=CARTESIAN_POINT('Ctrl Pts',(-4.22162532432222,1.97432008483649,
5.8940970152098));
#123737=CARTESIAN_POINT('Ctrl Pts',(-4.568711876,1.973534152,5.94784598));
#123738=CARTESIAN_POINT('Ctrl Pts',(-4.242777527,2.039276147,6.198205544));
#123739=CARTESIAN_POINT('Ctrl Pts',(-3.891438196,2.104034486,6.411451378));
#123740=CARTESIAN_POINT('Ctrl Pts',(-4.225485793,1.973534152,5.891330055));
#123741=CARTESIAN_POINT('Ctrl Pts',(-3.902648444,2.039276147,6.122881269));
#123742=CARTESIAN_POINT('Ctrl Pts',(-3.556442745,2.104034486,6.317769781));
#123743=CARTESIAN_POINT('Origin',(0.126048906359134,1.87507854154913,-0.147660019429458));
#123744=CARTESIAN_POINT('Ctrl Pts',(-3.48737511637751,2.10851071898316,
6.64054004366626));
#123745=CARTESIAN_POINT('Ctrl Pts',(-3.4749725094299,2.10627260249161,6.64699457467313));
#123746=CARTESIAN_POINT('Ctrl Pts',(-3.46256990248223,2.104034486,6.65344910567988));
#123747=CARTESIAN_POINT('Ctrl Pts',(-3.10134678922284,2.038849851,6.84143585675025));
#123748=CARTESIAN_POINT('Ctrl Pts',(-2.72189481628282,1.973541827,6.98921053722634));
#123749=CARTESIAN_POINT('Ctrl Pts',(-3.57999648804651,2.10851071898316,
6.30451074476264));
#123750=CARTESIAN_POINT('Ctrl Pts',(-3.56821961652325,2.10627260249161,
6.31114026288136));
#123751=CARTESIAN_POINT('Ctrl Pts',(-3.556442745,2.104034486,6.317769781));
#123752=CARTESIAN_POINT('Ctrl Pts',(-3.213444034,2.038849851,6.510852992));
#123753=CARTESIAN_POINT('Ctrl Pts',(-2.851557586,1.973541827,6.665667208));
#123754=CARTESIAN_POINT('',(-2.85586944075241,1.97432008458678,6.66382095471484));
#123755=CARTESIAN_POINT('Origin',(0.0852192425560599,2.01785676144799,-0.180516398354523));
#123756=CARTESIAN_POINT('Ctrl Pts',(-2.95381439782471,2.01370168116074,
6.89383641350064));
#123757=CARTESIAN_POINT('Ctrl Pts',(-2.93750805711261,2.00745398478963,
6.8554483588014));
#123758=CARTESIAN_POINT('Ctrl Pts',(-2.92118545276571,2.00105345712332,
6.81706631419646));
#123759=CARTESIAN_POINT('Ctrl Pts',(-2.8885436106362,1.98793719391023,6.74040678021258));
#123760=CARTESIAN_POINT('Ctrl Pts',(-2.87220553189679,1.98121389345132,
6.70208503629584));
#123761=CARTESIAN_POINT('Ctrl Pts',(-2.85586943938469,1.97432008482102,
6.66382095653845));
#123762=CARTESIAN_POINT('Ctrl Pts',(-3.183286862,1.973534152,6.790926649));
#123763=CARTESIAN_POINT('Ctrl Pts',(-2.811152772,2.039276147,6.965366696));
#123764=CARTESIAN_POINT('Ctrl Pts',(-2.422186008,2.104034486,7.098099389));
#123765=CARTESIAN_POINT('Ctrl Pts',(-2.860234467,1.973534152,6.661948573));
#123766=CARTESIAN_POINT('Ctrl Pts',(-2.495168211,2.039276147,6.818685762));
#123767=CARTESIAN_POINT('Ctrl Pts',(-2.115161339,2.104034486,6.93459389700001));
#123768=CARTESIAN_POINT('Origin',(0.0913593601730348,1.87507851176375,-0.171304427570849));
#123769=CARTESIAN_POINT('Ctrl Pts',(-1.97832240692608,2.10851071887184,
7.23497047157778));
#123770=CARTESIAN_POINT('Ctrl Pts',(-1.96482223300216,2.10627260243589,
7.23860790526074));
#123771=CARTESIAN_POINT('Ctrl Pts',(-1.95132205907823,2.104034486,7.24224533894379));
#123772=CARTESIAN_POINT('Ctrl Pts',(-1.55813254688159,2.038849851,7.34818477228274));
#123773=CARTESIAN_POINT('Ctrl Pts',(-1.15578476260228,1.973541827,7.41093360613812));
#123774=CARTESIAN_POINT('Ctrl Pts',(-2.14101470886305,2.10851071887184,
6.92670820836453));
#123775=CARTESIAN_POINT('Ctrl Pts',(-2.12808802393157,2.10627260243589,
6.93065105268227));
#123776=CARTESIAN_POINT('Ctrl Pts',(-2.115161339,2.104034486,6.93459389700001));
#123777=CARTESIAN_POINT('Ctrl Pts',(-1.738674564,2.038849851,7.049428346));
#123778=CARTESIAN_POINT('Ctrl Pts',(-1.35196834,1.973541827,7.122828203));
#123779=CARTESIAN_POINT('',(-1.35657627667434,1.97432008457408,7.12195203495116));
#123780=CARTESIAN_POINT('Origin',(0.0444211629499514,2.01785670642679,-0.194615624344407));
#123781=CARTESIAN_POINT('Ctrl Pts',(-1.40278481009805,2.01370168113039,
7.36764513055357));
#123782=CARTESIAN_POINT('Ctrl Pts',(-1.39511199963778,2.00745398477036,
7.32664918607161));
#123783=CARTESIAN_POINT('Ctrl Pts',(-1.38742201379162,2.0010534571221,7.28565561499032));
#123784=CARTESIAN_POINT('Ctrl Pts',(-1.37202285368925,1.98793719394712,
7.20377130722825));
#123785=CARTESIAN_POINT('Ctrl Pts',(-1.36430479237323,1.98121389349783,
7.16283330034612));
#123786=CARTESIAN_POINT('Ctrl Pts',(-1.35657627478824,1.97432008488557,
7.12195203641865));
#123787=CARTESIAN_POINT('Ctrl Pts',(-1.649014893,1.973534152,7.31647113600001));
#123788=CARTESIAN_POINT('Ctrl Pts',(-1.248081637,2.039276147,7.406835042));
#123789=CARTESIAN_POINT('Ctrl Pts',(-0.839675095000001,2.104034486,7.452848163));
#123790=CARTESIAN_POINT('Ctrl Pts',(-1.361241758,1.973534152,7.12106178));
#123791=CARTESIAN_POINT('Ctrl Pts',(-0.971016684,2.039276147,7.195656087));
#123792=CARTESIAN_POINT('Ctrl Pts',(-0.574977339,2.104034486,7.227164109));
#123793=CARTESIAN_POINT('Origin',(0.05239802991064,1.87507856101189,-0.186939026512341));
#123794=CARTESIAN_POINT('Ctrl Pts',(-0.376765541919947,2.10851071897258,
7.49110172164174));
#123795=CARTESIAN_POINT('Ctrl Pts',(-0.362799053543135,2.10627260248626,
7.4917519758376));
#123796=CARTESIAN_POINT('Ctrl Pts',(-0.348832565166325,2.104034486,7.49240223003331));
#123797=CARTESIAN_POINT('Ctrl Pts',(0.0579382408491217,2.038849851,7.51134073598938));
#123798=CARTESIAN_POINT('Ctrl Pts',(0.464368502441386,1.973541827,7.48612965584813));
#123799=CARTESIAN_POINT('Ctrl Pts',(-0.601921461974099,2.10851071897258,
7.22502049361022));
#123800=CARTESIAN_POINT('Ctrl Pts',(-0.588449400487053,2.10627260248626,
7.22609230130511));
#123801=CARTESIAN_POINT('Ctrl Pts',(-0.574977339,2.104034486,7.227164109));
#123802=CARTESIAN_POINT('Ctrl Pts',(-0.182606604,2.038849851,7.258380265));
#123803=CARTESIAN_POINT('Ctrl Pts',(0.210837442,1.973541827,7.246933667));
#123804=CARTESIAN_POINT('Origin',(0.00154614941171419,2.01785680179854,
-0.199616151906485));
#123805=CARTESIAN_POINT('Ctrl Pts',(-1.35704670638058,3.78339966801642,
7.12186672777107));
#123806=CARTESIAN_POINT('Ctrl Pts',(-1.35319549019029,3.78403814050821,
7.12259624888554));
#123807=CARTESIAN_POINT('Ctrl Pts',(-1.349344274,3.784676613,7.12332577));
#123808=CARTESIAN_POINT('Ctrl Pts',(-0.962175844,3.848863192,7.196665601));
#123809=CARTESIAN_POINT('Ctrl Pts',(-0.569339312,3.914045302,7.227610445));
#123810=CARTESIAN_POINT('Ctrl Pts',(-1.16146771926858,3.78339966801642,
7.40952484987452));
#123811=CARTESIAN_POINT('Ctrl Pts',(-1.15746109563429,3.78403814050821,
7.41014846343727));
#123812=CARTESIAN_POINT('Ctrl Pts',(-1.153454472,3.784676613,7.410772077));
#123813=CARTESIAN_POINT('Ctrl Pts',(-0.750662703,3.848863192,7.473464866));
#123814=CARTESIAN_POINT('Ctrl Pts',(-0.343448839,3.914045302,7.492132066));
#123815=CARTESIAN_POINT('',(-0.574036075380877,3.91326598488409,7.2272389368462));
#123816=CARTESIAN_POINT('Ctrl Pts',(-0.574036076308431,3.91326598386019,
7.22723893873903));
#123817=CARTESIAN_POINT('Ctrl Pts',(-0.576049247025033,3.90857186132774,
7.2558036048112));
#123818=CARTESIAN_POINT('Ctrl Pts',(-0.57805430305433,3.90396299771727,
7.28438297799801));
#123819=CARTESIAN_POINT('Ctrl Pts',(-0.580051625069697,3.89943471856325,
7.31297553246098));
#123820=CARTESIAN_POINT('Ctrl Pts',(-0.581955575986403,3.89511812805851,
7.34023143804963));
#123821=CARTESIAN_POINT('Ctrl Pts',(-0.583844230084641,3.89087604513709,
7.36750030135324));
#123822=CARTESIAN_POINT('Ctrl Pts',(-0.585765722797521,3.88669712984843,
7.39477643667835));
#123823=CARTESIAN_POINT('Ctrl Pts',(-0.587687262853223,3.88251811159729,
7.42205324404827));
#123824=CARTESIAN_POINT('Ctrl Pts',(-0.589633671771024,3.87840354548757,
7.44933825566685));
#123825=CARTESIAN_POINT('Ctrl Pts',(-0.59160338941931,3.87435041354706,
7.47663061988905));
#123826=CARTESIAN_POINT('Origin',(-0.00201954687480965,4.01777100458333,
-0.19381601599339));
#123827=CARTESIAN_POINT('Ctrl Pts',(-2.118772315,3.914032935,6.933491464));
#123828=CARTESIAN_POINT('Ctrl Pts',(-2.056341304,3.90342418,6.952569456));
#123829=CARTESIAN_POINT('Ctrl Pts',(-1.993576877,3.892857143,6.970520155));
#123830=CARTESIAN_POINT('Ctrl Pts',(-1.674952964,3.839213527,7.061646965));
#123831=CARTESIAN_POINT('Ctrl Pts',(-1.349344274,3.784676613,7.12332577));
#123832=CARTESIAN_POINT('Ctrl Pts',(-1.34543222082607,3.78402137462933,
7.12406681522476));
#123833=CARTESIAN_POINT('Ctrl Pts',(-1.34152016765215,3.78336613625867,
7.12480786044952));
#123834=CARTESIAN_POINT('Ctrl Pts',(-2.42588209,3.914032935,7.096837048));
#123835=CARTESIAN_POINT('Ctrl Pts',(-2.361980272,3.90342418,7.118680339));
#123836=CARTESIAN_POINT('Ctrl Pts',(-2.297695481,3.892857143,7.139369403));
#123837=CARTESIAN_POINT('Ctrl Pts',(-1.971353434,3.839213527,7.244397537));
#123838=CARTESIAN_POINT('Ctrl Pts',(-1.636790581,3.784676613,7.319215572));
#123839=CARTESIAN_POINT('Ctrl Pts',(-1.6327709472766,3.78402137462933,7.32011447961603));
#123840=CARTESIAN_POINT('Ctrl Pts',(-1.6287513135532,3.78336613625867,7.32101338723207));
#123841=CARTESIAN_POINT('',(-2.11425816854035,3.91326598495297,6.93486931335475));
#123842=CARTESIAN_POINT('Ctrl Pts',(-2.1142581686341,3.91326598528019,6.93486931384458));
#123843=CARTESIAN_POINT('Ctrl Pts',(-2.07409799250755,3.90644394825061,
6.9471130886998));
#123844=CARTESIAN_POINT('Ctrl Pts',(-2.03386770757442,3.89964051877146,
6.95899693099171));
#123845=CARTESIAN_POINT('Ctrl Pts',(-1.99357687675307,3.89285714287914,
6.97052015546677));
#123846=CARTESIAN_POINT('Ctrl Pts',(-1.85161574205348,3.86895652430184,
7.01112120550672));
#123847=CARTESIAN_POINT('Ctrl Pts',(-1.7079233848003,3.84480664668525,7.04752157904651));
#123848=CARTESIAN_POINT('Ctrl Pts',(-1.56288052588263,3.82047224755234,
7.07954126122991));
#123849=CARTESIAN_POINT('Ctrl Pts',(-1.49200829878732,3.80858174101899,
7.09518702417306));
#123850=CARTESIAN_POINT('Ctrl Pts',(-1.42081403974305,3.79664724067556,
7.109787527585));
#123851=CARTESIAN_POINT('Ctrl Pts',(-1.34934427548489,3.78467661296572,
7.12332577119014));
#123852=CARTESIAN_POINT('Ctrl Pts',(-2.18502660812532,3.87435041326576,
7.17465390925577));
#123853=CARTESIAN_POINT('Ctrl Pts',(-2.17685404271359,3.87860220111518,
7.14713740763035));
#123854=CARTESIAN_POINT('Ctrl Pts',(-2.1687082656535,3.88292159126619,7.11962328841485));
#123855=CARTESIAN_POINT('Ctrl Pts',(-2.16059124855501,3.8873120745959,7.0921121225464));
#123856=CARTESIAN_POINT('Ctrl Pts',(-2.15285368017845,3.89149731463637,
7.06588702970225));
#123857=CARTESIAN_POINT('Ctrl Pts',(-2.14514798794445,3.8957461849516,7.03966258355752));
#123858=CARTESIAN_POINT('Ctrl Pts',(-2.13742892265818,3.90006996195599,
7.01345452121582));
#123859=CARTESIAN_POINT('Ctrl Pts',(-2.12970964348895,3.90439385876533,
6.98724573269059));
#123860=CARTESIAN_POINT('Ctrl Pts',(-2.12198607104547,3.90879118062969,
6.96105020924954));
#123861=CARTESIAN_POINT('Ctrl Pts',(-2.1142581719554,3.91326598407097,6.93486931282839));
#123862=CARTESIAN_POINT('Ctrl Pts',(-2.85631053383156,3.78339966801642,
6.66363651409478));
#123863=CARTESIAN_POINT('Ctrl Pts',(-2.85270618241578,3.78403814050821,
6.66517687704739));
#123864=CARTESIAN_POINT('Ctrl Pts',(-2.849101831,3.784676613,6.66671724));
#123865=CARTESIAN_POINT('Ctrl Pts',(-2.48675108,3.848863192,6.82157219400001));
#123866=CARTESIAN_POINT('Ctrl Pts',(-2.109751075,3.914045302,6.936241807));
#123867=CARTESIAN_POINT('Ctrl Pts',(-2.72714206803972,3.78339966801642,
6.98661305006529));
#123868=CARTESIAN_POINT('Ctrl Pts',(-2.72336317551986,3.78403814050821,
6.98808338953264));
#123869=CARTESIAN_POINT('Ctrl Pts',(-2.719584283,3.784676613,6.989553729));
#123870=CARTESIAN_POINT('Ctrl Pts',(-2.339686658,3.848863192,7.137369119));
#123871=CARTESIAN_POINT('Ctrl Pts',(-1.946006124,3.914045302,7.243138834));
#123872=CARTESIAN_POINT('Origin',(0.0396917695066523,4.01777116282268,-0.189717473787636));
#123873=CARTESIAN_POINT('Ctrl Pts',(-3.559732308,3.914032935,6.315916869));
#123874=CARTESIAN_POINT('Ctrl Pts',(-3.502862104,3.90342418,6.347969651));
#123875=CARTESIAN_POINT('Ctrl Pts',(-3.445423944,3.892857143,6.378993169));
#123876=CARTESIAN_POINT('Ctrl Pts',(-3.153838851,3.839213527,6.536484208));
#123877=CARTESIAN_POINT('Ctrl Pts',(-2.849101831,3.784676613,6.66671724));
#123878=CARTESIAN_POINT('Ctrl Pts',(-2.84544054227241,3.78402137462933,
6.66828193578925));
#123879=CARTESIAN_POINT('Ctrl Pts',(-2.84177925354481,3.78336613625867,
6.66984663157849));
#123880=CARTESIAN_POINT('Ctrl Pts',(-3.894776499,3.914032935,6.409424001));
#123881=CARTESIAN_POINT('Ctrl Pts',(-3.837064332,3.90342418,6.44449361));
#123882=CARTESIAN_POINT('Ctrl Pts',(-3.778730021,3.892857143,6.478518305));
#123883=CARTESIAN_POINT('Ctrl Pts',(-3.482595614,3.839213527,6.651244833));
#123884=CARTESIAN_POINT('Ctrl Pts',(-3.17193832,3.784676613,6.796234788));
#123885=CARTESIAN_POINT('Ctrl Pts',(-3.16820590163919,3.78402137462933,
6.79797678209003));
#123886=CARTESIAN_POINT('Ctrl Pts',(-3.16447348327838,3.78336613625867,
6.79971877618007));
#123887=CARTESIAN_POINT('',(-3.55561989781354,3.9132659848605,6.31823291263059));
#123888=CARTESIAN_POINT('Ctrl Pts',(-3.55561990133067,3.9132659850464,6.31823290990407));
#123889=CARTESIAN_POINT('Ctrl Pts',(-3.500785581,3.903042157,6.349091223));
#123890=CARTESIAN_POINT('Ctrl Pts',(-3.445423944,3.892857143,6.378993169));
#123891=CARTESIAN_POINT('Ctrl Pts',(-3.153838851037,3.83921352752391,6.5364842076699));
#123892=CARTESIAN_POINT('Ctrl Pts',(-2.84910183343416,3.7846766127594,6.66671724052467));
#123893=CARTESIAN_POINT('Ctrl Pts',(-3.67628040946578,3.87435041322476,
6.53719835604485));
#123894=CARTESIAN_POINT('Ctrl Pts',(-3.66238367936974,3.87860220111933,
6.51208203505423));
#123895=CARTESIAN_POINT('Ctrl Pts',(-3.64851362369141,3.88292159127308,
6.48696228194705));
#123896=CARTESIAN_POINT('Ctrl Pts',(-3.63467229045904,3.8873120746017,6.46183923059982));
#123897=CARTESIAN_POINT('Ctrl Pts',(-3.62147800234562,3.89149731463765,
6.43789061436477));
#123898=CARTESIAN_POINT('Ctrl Pts',(-3.60831498411576,3.89574618495018,
6.41393577729978));
#123899=CARTESIAN_POINT('Ctrl Pts',(-3.59514242756216,3.90006996193851,
6.38999981577969));
#123900=CARTESIAN_POINT('Ctrl Pts',(-3.58196950601821,3.90439385873175,
6.3660631910326));
#123901=CARTESIAN_POINT('Ctrl Pts',(-3.56879524322248,3.90879118056604,
6.34214044413692));
#123902=CARTESIAN_POINT('Ctrl Pts',(-3.55561990060165,3.91326598374165,
6.31823291137695));
#123903=CARTESIAN_POINT('Ctrl Pts',(-4.22201645637774,3.78339966801642,
5.893822062747));
#123904=CARTESIAN_POINT('Ctrl Pts',(-4.21882750518887,3.78403814050821,
5.8961012418735));
#123905=CARTESIAN_POINT('Ctrl Pts',(-4.215638554,3.784676613,5.898380421));
#123906=CARTESIAN_POINT('Ctrl Pts',(-3.895048599,3.848863192,6.127509652));
#123907=CARTESIAN_POINT('Ctrl Pts',(-3.551513221,3.914045302,6.320542211));
#123908=CARTESIAN_POINT('Ctrl Pts',(-4.16529828519659,3.78339966801642,
6.23701498812772));
#123909=CARTESIAN_POINT('Ctrl Pts',(-4.16192382059829,3.78403814050821,
6.23926330206386));
#123910=CARTESIAN_POINT('Ctrl Pts',(-4.158549356,3.784676613,6.241511616));
#123911=CARTESIAN_POINT('Ctrl Pts',(-3.819309465,3.848863192,6.467537924));
#123912=CARTESIAN_POINT('Ctrl Pts',(-3.457570326,3.914045302,6.65546448));
#123913=CARTESIAN_POINT('Origin',(0.0795475392719219,4.01777120008797,-0.176749585716738));
#123914=CARTESIAN_POINT('Ctrl Pts',(-4.834243174,3.914032935,5.403017021));
#123915=CARTESIAN_POINT('Ctrl Pts',(-4.785592964,3.90342418,5.446545839));
#123916=CARTESIAN_POINT('Ctrl Pts',(-4.736166816,3.892857143,5.489191552));
#123917=CARTESIAN_POINT('Ctrl Pts',(-4.485254739,3.839213527,5.705682713));
#123918=CARTESIAN_POINT('Ctrl Pts',(-4.215638554,3.784676613,5.898380421));
#123919=CARTESIAN_POINT('Ctrl Pts',(-4.21239922751805,3.78402137462933,
5.90069560392768));
#123920=CARTESIAN_POINT('Ctrl Pts',(-4.20915990103609,3.78336613625867,
5.90301078685534));
#123921=CARTESIAN_POINT('Ctrl Pts',(-5.181555488,3.914032935,5.422313411));
#123922=CARTESIAN_POINT('Ctrl Pts',(-5.13273152800001,3.90342418,5.468969522));
#123923=CARTESIAN_POINT('Ctrl Pts',(-5.083075345,3.892857143,5.514738891));
#123924=CARTESIAN_POINT('Ctrl Pts',(-4.830995493,3.839213527,5.747087313));
#123925=CARTESIAN_POINT('Ctrl Pts',(-4.558769749,3.784676613,5.955469618));
#123926=CARTESIAN_POINT('Ctrl Pts',(-4.5554990697505,3.78402137462933,5.95797324484628));
#123927=CARTESIAN_POINT('Ctrl Pts',(-4.552228390501,3.78336613625867,5.96047687169255));
#123928=CARTESIAN_POINT('',(-4.83072479043724,3.91326598487081,5.40616296424982));
#123929=CARTESIAN_POINT('Ctrl Pts',(-4.83072479322977,3.9132659850464,5.40616296074057));
#123930=CARTESIAN_POINT('Ctrl Pts',(-4.783806095,3.903042157,5.448087581));
#123931=CARTESIAN_POINT('Ctrl Pts',(-4.736166816,3.892857143,5.489191552));
#123932=CARTESIAN_POINT('Ctrl Pts',(-4.48525473952604,3.83921352756829,
5.70568271291834));
#123933=CARTESIAN_POINT('Ctrl Pts',(-4.21563855621441,3.78467661274867,
5.89838042096646));
#123934=CARTESIAN_POINT('Ctrl Pts',(-4.99563542474069,3.87435041323828,
5.59407067341434));
#123935=CARTESIAN_POINT('Ctrl Pts',(-4.97666432598813,3.87860220109873,
5.57252894419364));
#123936=CARTESIAN_POINT('Ctrl Pts',(-4.95771854011772,3.88292159124263,
5.55097812899301));
#123937=CARTESIAN_POINT('Ctrl Pts',(-4.93880009614804,3.88731207456726,
5.52941791819073));
#123938=CARTESIAN_POINT('Ctrl Pts',(-4.92076603853602,3.89149731460856,
5.50886558923815));
#123939=CARTESIAN_POINT('Ctrl Pts',(-4.90276118250714,3.89574618491636,
5.48830046273151));
#123940=CARTESIAN_POINT('Ctrl Pts',(-4.88475106888788,3.90006996189442,
5.46775582088404));
#123941=CARTESIAN_POINT('Ctrl Pts',(-4.86674045623729,3.90439385867739,
5.44721060977753));
#123942=CARTESIAN_POINT('Ctrl Pts',(-4.84873151701053,3.90879118050781,
5.42667924040515));
#123943=CARTESIAN_POINT('Ctrl Pts',(-4.83072479286557,3.91326598389372,
5.4061629624153));
#123944=CARTESIAN_POINT('Ctrl Pts',(-5.39030558027708,3.78339966801642,
4.84841904112145));
#123945=CARTESIAN_POINT('Ctrl Pts',(-5.38768114113854,3.78403814050821,
4.85133046456072));
#123946=CARTESIAN_POINT('Ctrl Pts',(-5.385056702,3.784676613,4.854241888));
#123947=CARTESIAN_POINT('Ctrl Pts',(-5.121217974,3.848863192,5.14693157));
#123948=CARTESIAN_POINT('Ctrl Pts',(-4.827210557,3.914045302,5.409301086));
#123949=CARTESIAN_POINT('Ctrl Pts',(-5.40868978391049,3.78339966801642,
5.19578103749289));
#123950=CARTESIAN_POINT('Ctrl Pts',(-5.40587753345524,3.78403814050821,
5.19870219724644));
#123951=CARTESIAN_POINT('Ctrl Pts',(-5.40306528300001,3.784676613,5.201623357));
#123952=CARTESIAN_POINT('Ctrl Pts',(-5.120345607,3.848863192,5.495291845));
#123953=CARTESIAN_POINT('Ctrl Pts',(-4.807462382,3.914045302,5.756588004));
#123954=CARTESIAN_POINT('Origin',(0.115683568884218,4.01777114530414,-0.155516752860486));
#123955=CARTESIAN_POINT('Ctrl Pts',(-5.88271020300001,3.914032935,4.237478103));
#123956=CARTESIAN_POINT('Ctrl Pts',(-5.844554817,3.90342418,4.290447598));
#123957=CARTESIAN_POINT('Ctrl Pts',(-5.805451792,3.892857143,4.342721438));
#123958=CARTESIAN_POINT('Ctrl Pts',(-5.6069451,3.839213527,4.608089836));
#123959=CARTESIAN_POINT('Ctrl Pts',(-5.385056702,3.784676613,4.854241888));
#123960=CARTESIAN_POINT('Ctrl Pts',(-5.38239080505588,3.78402137462933,
4.85719930266942));
#123961=CARTESIAN_POINT('Ctrl Pts',(-5.37972490811174,3.78336613625867,
4.86015671733883));
#123962=CARTESIAN_POINT('Ctrl Pts',(-6.22605070100001,3.914032935,4.181661472));
#123963=CARTESIAN_POINT('Ctrl Pts',(-6.188397903,3.90342418,4.237722498));
#123964=CARTESIAN_POINT('Ctrl Pts',(-6.149741715,3.892857143,4.293096416));
#123965=CARTESIAN_POINT('Ctrl Pts',(-5.953503393,3.839213527,4.574202378));
#123966=CARTESIAN_POINT('Ctrl Pts',(-5.732438171,3.784676613,4.836233308));
#123967=CARTESIAN_POINT('Ctrl Pts',(-5.72978216417362,3.78402137462933,
4.83938150079354));
#123968=CARTESIAN_POINT('Ctrl Pts',(-5.72712615734723,3.78336613625867,
4.84252969358708));
#123969=CARTESIAN_POINT('',(-5.87995036158964,3.91326598496052,4.24130684423531));
#123970=CARTESIAN_POINT('Ctrl Pts',(-5.87995036176124,3.91326598532877,
4.24130684443286));
#123971=CARTESIAN_POINT('Ctrl Pts',(-5.85538874095779,3.90644394830579,
4.27535793159474));
#123972=CARTESIAN_POINT('Ctrl Pts',(-5.8305534848299,3.89964051880999,4.30916490723401));
#123973=CARTESIAN_POINT('Ctrl Pts',(-5.80545179213163,3.89285714291852,
4.34272143834066));
#123974=CARTESIAN_POINT('Ctrl Pts',(-5.71700827329339,3.86895653713759,
4.46095480768064));
#123975=CARTESIAN_POINT('Ctrl Pts',(-5.62464440301594,3.84480667252569,
4.57689174154322));
#123976=CARTESIAN_POINT('Ctrl Pts',(-5.52855433006173,3.82047228658325,
4.69015852906592));
#123977=CARTESIAN_POINT('Ctrl Pts',(-5.48160180434346,3.80858176712922,
4.74550411878901));
#123978=CARTESIAN_POINT('Ctrl Pts',(-5.43376034511521,3.79664725376609,
4.80021246869245));
#123979=CARTESIAN_POINT('Ctrl Pts',(-5.38505670397552,3.78467661297329,
4.85424188801248));
#123980=CARTESIAN_POINT('Ctrl Pts',(-6.08140007972271,3.87435041321968,
4.38937046350253));
#123981=CARTESIAN_POINT('Ctrl Pts',(-6.05824167964873,3.87860220110466,
4.37241059342075));
#123982=CARTESIAN_POINT('Ctrl Pts',(-6.03510604752354,3.88292159125114,
4.35543640811372));
#123983=CARTESIAN_POINT('Ctrl Pts',(-6.01199509829652,3.88731207457891,
4.33844716915637));
#123984=CARTESIAN_POINT('Ctrl Pts',(-5.98996452384717,3.89149731460825,
4.32225213147051));
#123985=CARTESIAN_POINT('Ctrl Pts',(-5.96795971712769,3.89574618491864,
4.30603831801684));
#123986=CARTESIAN_POINT('Ctrl Pts',(-5.94595417929557,3.90006996191496,
4.2898456405848));
#123987=CARTESIAN_POINT('Ctrl Pts',(-5.92394803172508,3.90439385871625,
4.27365251447949));
#123988=CARTESIAN_POINT('Ctrl Pts',(-5.90194649400798,3.90879118057332,
4.25747254677785));
#123989=CARTESIAN_POINT('Ctrl Pts',(-5.87995036393221,3.91326598396042,
4.24130684150133));
#123990=CARTESIAN_POINT('Ctrl Pts',(-6.30655000747555,3.78339966801642,
3.57630933537954));
#123991=CARTESIAN_POINT('Ctrl Pts',(-6.30461279623777,3.78403814050821,
3.57971686818977));
#123992=CARTESIAN_POINT('Ctrl Pts',(-6.302675585,3.784676613,3.583124401));
#123993=CARTESIAN_POINT('Ctrl Pts',(-6.107924889,3.848863192,3.925688688));
#123994=CARTESIAN_POINT('Ctrl Pts',(-5.87719289300001,3.914045302,4.245127054));
#123995=CARTESIAN_POINT('Ctrl Pts',(-6.39917695920962,3.78339966801642,
3.91159814126253));
#123996=CARTESIAN_POINT('Ctrl Pts',(-6.39705842060482,3.78403814050821,
3.91505555663127));
#123997=CARTESIAN_POINT('Ctrl Pts',(-6.394939882,3.784676613,3.918512972));
#123998=CARTESIAN_POINT('Ctrl Pts',(-6.181960079,3.848863192,4.266092026));
#123999=CARTESIAN_POINT('Ctrl Pts',(-5.93256284,3.914045302,4.588539871));
#124000=CARTESIAN_POINT('Origin',(0.146410461703627,4.01777117749663,-0.127012326547644));
#124001=CARTESIAN_POINT('Ctrl Pts',(-6.65610824,3.914032935,2.873799418));
#124002=CARTESIAN_POINT('Ctrl Pts',(-6.630231782,3.90342418,2.933732796));
#124003=CARTESIAN_POINT('Ctrl Pts',(-6.603280295,3.892857143,2.993190497));
#124004=CARTESIAN_POINT('Ctrl Pts',(-6.46646094,3.839213527,3.2950278));
#124005=CARTESIAN_POINT('Ctrl Pts',(-6.30267558499999,3.784676613,3.583124401));
#124006=CARTESIAN_POINT('Ctrl Pts',(-6.30070777198533,3.78402137462933,
3.58658576200464));
#124007=CARTESIAN_POINT('Ctrl Pts',(-6.29873995897067,3.78336613625867,
3.59004712300929));
#124008=CARTESIAN_POINT('Ctrl Pts',(-6.979422703,3.914032935,2.745479691));
#124009=CARTESIAN_POINT('Ctrl Pts',(-6.95470167,3.90342418,2.808324279));
#124010=CARTESIAN_POINT('Ctrl Pts',(-6.928852998,3.892857143,2.870713524));
#124011=CARTESIAN_POINT('Ctrl Pts',(-6.797632091,3.839213527,3.187432823));
#124012=CARTESIAN_POINT('Ctrl Pts',(-6.638064156,3.784676613,3.490860104));
#124013=CARTESIAN_POINT('Ctrl Pts',(-6.63614701353499,3.78402137462933,
3.49450565675749));
#124014=CARTESIAN_POINT('Ctrl Pts',(-6.63422987106999,3.78336613625867,
3.49815120951497));
#124015=CARTESIAN_POINT('',(-6.65423598880558,3.91326598476628,2.87813192909408));
#124016=CARTESIAN_POINT('Ctrl Pts',(-6.6542359888712,3.91326598544311,2.8781319292423));
#124017=CARTESIAN_POINT('Ctrl Pts',(-6.63756858305185,3.90644394855885,
2.91666694270274));
#124018=CARTESIAN_POINT('Ctrl Pts',(-6.62058146189084,3.8996405190235,2.95502237632601));
#124019=CARTESIAN_POINT('Ctrl Pts',(-6.60328029523313,3.8928571430914,2.9931904964857));
#124020=CARTESIAN_POINT('Ctrl Pts',(-6.5423212091965,3.86895653485097,3.12767239143726));
#124021=CARTESIAN_POINT('Ctrl Pts',(-6.47703976156619,3.84480666772173,
3.26075429956098));
#124022=CARTESIAN_POINT('Ctrl Pts',(-6.40754522474049,3.82047227927594,
3.39202951081633));
#124023=CARTESIAN_POINT('Ctrl Pts',(-6.37358809548747,3.80858176224409,
3.45617454321643));
#124024=CARTESIAN_POINT('Ctrl Pts',(-6.33862582826106,3.79664725133354,
3.51988832868173));
#124025=CARTESIAN_POINT('Ctrl Pts',(-6.30267558687012,3.78467661302513,
3.58312440037351));
#124026=CARTESIAN_POINT('Ctrl Pts',(-6.88280522651749,3.87435041325227,
2.97942816881733));
#124027=CARTESIAN_POINT('Ctrl Pts',(-6.8565423860806,3.87860220116035,2.96784318262581));
#124028=CARTESIAN_POINT('Ctrl Pts',(-6.83029870404635,3.88292159130352,
2.95623932143671));
#124029=CARTESIAN_POINT('Ctrl Pts',(-6.80407589172509,3.88731207462835,
2.94461545246392));
#124030=CARTESIAN_POINT('Ctrl Pts',(-6.77907892536439,3.89149731466413,
2.933534968108));
#124031=CARTESIAN_POINT('Ctrl Pts',(-6.75410308807489,3.89574618496796,
2.92243060758178));
#124032=CARTESIAN_POINT('Ctrl Pts',(-6.72913108036634,3.90006996195947,
2.91134704614054));
#124033=CARTESIAN_POINT('Ctrl Pts',(-6.70415838072343,3.90439385875593,
2.90026317759156));
#124034=CARTESIAN_POINT('Ctrl Pts',(-6.6791930118057,3.90879118061045,2.88919116886928));
#124035=CARTESIAN_POINT('Ctrl Pts',(-6.65423599044422,3.91326598379351,
2.87813192527154));
#124036=CARTESIAN_POINT('Ctrl Pts',(-6.92790716496715,3.78339966801642,
2.13697537852514));
#124037=CARTESIAN_POINT('Ctrl Pts',(-6.92674776348357,3.78403814050821,
2.14071968826257));
#124038=CARTESIAN_POINT('Ctrl Pts',(-6.92558836200001,3.784676613,2.144463998));
#124039=CARTESIAN_POINT('Ctrl Pts',(-6.809032025,3.848863192,2.520884965));
#124040=CARTESIAN_POINT('Ctrl Pts',(-6.65236422,3.914045302,2.882455599));
#124041=CARTESIAN_POINT('Ctrl Pts',(-7.09044573248517,3.78339966801642,
2.44451326180714));
#124042=CARTESIAN_POINT('Ctrl Pts',(-7.08911996624259,3.78403814050821,
2.44834526790357));
#124043=CARTESIAN_POINT('Ctrl Pts',(-7.0877942,3.784676613,2.452177274));
#124044=CARTESIAN_POINT('Ctrl Pts',(-6.954512969,3.848863192,2.837414485));
#124045=CARTESIAN_POINT('Ctrl Pts',(-6.780263254,3.914045302,3.205936713));
#124046=CARTESIAN_POINT('Origin',(0.170291314417856,4.01777096736017,-0.0925688634418695));
#124047=CARTESIAN_POINT('Ctrl Pts',(-7.118274054,3.914032935,1.375745066));
#124048=CARTESIAN_POINT('Ctrl Pts',(-7.105886478,3.90342418,1.439839908));
#124049=CARTESIAN_POINT('Ctrl Pts',(-7.09234675,3.892857143,1.503701295));
#124050=CARTESIAN_POINT('Ctrl Pts',(-7.02361225300001,3.839213527,1.827893927));
#124051=CARTESIAN_POINT('Ctrl Pts',(-6.925588362,3.784676613,2.144463998));
#124052=CARTESIAN_POINT('Ctrl Pts',(-6.92441064566231,3.78402137462933,
2.14826745592069));
#124053=CARTESIAN_POINT('Ctrl Pts',(-6.92323292932462,3.78336613625867,
2.15207091384138));
#124054=CARTESIAN_POINT('Ctrl Pts',(-7.406444656,3.914032935,1.180922331));
#124055=CARTESIAN_POINT('Ctrl Pts',(-7.395811316,3.90342418,1.247611939));
#124056=CARTESIAN_POINT('Ctrl Pts',(-7.383978815,3.892857143,1.314099258));
#124057=CARTESIAN_POINT('Ctrl Pts',(-7.323911067,3.839213527,1.651622452));
#124058=CARTESIAN_POINT('Ctrl Pts',(-7.233301638,3.784676613,1.982258161));
#124059=CARTESIAN_POINT('Ctrl Pts',(-7.23221300334376,3.78402137462933,
1.98623061171932));
#124060=CARTESIAN_POINT('Ctrl Pts',(-7.23112436868752,3.78336613625867,
1.99020306243863));
#124061=CARTESIAN_POINT('',(-7.11737693701566,3.91326598488478,1.38037876392498));
#124062=CARTESIAN_POINT('Ctrl Pts',(-7.11737693714267,3.9132659850464,1.38037875906925));
#124063=CARTESIAN_POINT('Ctrl Pts',(-7.105396986,3.903042157,1.442148645));
#124064=CARTESIAN_POINT('Ctrl Pts',(-7.09234675,3.892857143,1.503701295));
#124065=CARTESIAN_POINT('Ctrl Pts',(-7.02361225412372,3.83921352757512,
1.82789392608951));
#124066=CARTESIAN_POINT('Ctrl Pts',(-6.92558836366604,3.78467661276937,
2.14446399703795));
#124067=CARTESIAN_POINT('Ctrl Pts',(-7.36237804982059,3.87435041323098,
1.43017112466086));
#124068=CARTESIAN_POINT('Ctrl Pts',(-7.33423879050147,3.87860220114459,
1.42450272340496));
#124069=CARTESIAN_POINT('Ctrl Pts',(-7.30611418400067,3.8829215913066,1.4188117698809));
#124070=CARTESIAN_POINT('Ctrl Pts',(-7.27800565822947,3.88731207464986,
1.41309678996559));
#124071=CARTESIAN_POINT('Ctrl Pts',(-7.2512111305266,3.89149731469153,1.40764897000845));
#124072=CARTESIAN_POINT('Ctrl Pts',(-7.22443210526551,3.89574618499422,
1.40217328992509));
#124073=CARTESIAN_POINT('Ctrl Pts',(-7.19766129125643,3.9000699619737,1.39671709932097));
#124074=CARTESIAN_POINT('Ctrl Pts',(-7.17088973547094,3.90439385875811,
1.39126075753454));
#124075=CARTESIAN_POINT('Ctrl Pts',(-7.14412788854292,3.90879118059815,
1.38581442237808));
#124076=CARTESIAN_POINT('Ctrl Pts',(-7.11737693823209,3.91326598397551,
1.38037876113061));
#124077=CARTESIAN_POINT('Ctrl Pts',(-7.22532308280471,3.78339966801642,
0.597718829193276));
#124078=CARTESIAN_POINT('Ctrl Pts',(-7.22499570340235,3.78403814050821,
0.601624836096638));
#124079=CARTESIAN_POINT('Ctrl Pts',(-7.224668324,3.784676613,0.605530843000001));
#124080=CARTESIAN_POINT('Ctrl Pts',(-7.191756391,3.848863192,0.998207464));
#124081=CARTESIAN_POINT('Ctrl Pts',(-7.116478391,3.914045302,1.385003724));
#124082=CARTESIAN_POINT('Ctrl Pts',(-7.45017314305326,3.78339966801642,
0.863125660047407));
#124083=CARTESIAN_POINT('Ctrl Pts',(-7.44970214052664,3.78403814050821,
0.867153076523704));
#124084=CARTESIAN_POINT('Ctrl Pts',(-7.449231138,3.784676613,0.871180493));
#124085=CARTESIAN_POINT('Ctrl Pts',(-7.401880561,3.848863192,1.276062597));
#124086=CARTESIAN_POINT('Ctrl Pts',(-7.31092609300001,3.914045302,1.673427518));
#124087=CARTESIAN_POINT('Origin',(0.186209394296897,4.01777117271173,-0.0537970715760096));
#124088=CARTESIAN_POINT('Ctrl Pts',(-7.24759728500001,3.914032935,-0.186637596));
#124089=CARTESIAN_POINT('Ctrl Pts',(-7.24927782,3.90342418,-0.121378293));
#124090=CARTESIAN_POINT('Ctrl Pts',(-7.249782953,3.892857143,-0.056099309));
#124091=CARTESIAN_POINT('Ctrl Pts',(-7.25234726400001,3.839213527,0.275289764));
#124092=CARTESIAN_POINT('Ctrl Pts',(-7.224668324,3.784676613,0.605530843));
#124093=CARTESIAN_POINT('Ctrl Pts',(-7.22433577303191,3.78402137462933,
0.609498552403771));
#124094=CARTESIAN_POINT('Ctrl Pts',(-7.22400322206382,3.78336613625867,
0.613466261807543));
#124095=CARTESIAN_POINT('Ctrl Pts',(-7.487149489,3.914032935,-0.438853645));
#124096=CARTESIAN_POINT('Ctrl Pts',(-7.491101045,3.90342418,-0.37143735));
#124097=CARTESIAN_POINT('Ctrl Pts',(-7.49383799,3.892857143,-0.303960829));
#124098=CARTESIAN_POINT('Ctrl Pts',(-7.507732102,3.839213527,0.038584051));
#124099=CARTESIAN_POINT('Ctrl Pts',(-7.490317975,3.784676613,0.380968029));
#124100=CARTESIAN_POINT('Ctrl Pts',(-7.49010875149677,3.78402137462933,
0.385081630291895));
#124101=CARTESIAN_POINT('Ctrl Pts',(-7.48989952799356,3.78336613625867,
0.389195231583791));
#124102=CARTESIAN_POINT('',(-7.24771724987847,3.91326598491533,-0.181919377610948));
#124103=CARTESIAN_POINT('Ctrl Pts',(-7.24771724884897,3.9132659850464,-0.181919382176649));
#124104=CARTESIAN_POINT('Ctrl Pts',(-7.249296082,3.903042157,-0.119018306));
#124105=CARTESIAN_POINT('Ctrl Pts',(-7.249782953,3.892857143,-0.056099309));
#124106=CARTESIAN_POINT('Ctrl Pts',(-7.25234726369774,3.83921352753372,
0.275289763730124));
#124107=CARTESIAN_POINT('Ctrl Pts',(-7.22466832546219,3.78467661278774,
0.605530841650099));
#124108=CARTESIAN_POINT('Ctrl Pts',(-7.49769425876845,3.8743504132083,-0.185959131938337));
#124109=CARTESIAN_POINT('Ctrl Pts',(-7.46899434101961,3.87860220112769,
-0.185445900076303));
#124110=CARTESIAN_POINT('Ctrl Pts',(-7.44030388546657,3.88292159126831,
-0.184957843287825));
#124111=CARTESIAN_POINT('Ctrl Pts',(-7.41162396971045,3.88731207458993,
-0.18449670805495));
#124112=CARTESIAN_POINT('Ctrl Pts',(-7.38428476285018,3.89149731462924,
-0.184057129653488));
#124113=CARTESIAN_POINT('Ctrl Pts',(-7.3569547068799,3.89574618493294,-0.183648092579244));
#124114=CARTESIAN_POINT('Ctrl Pts',(-7.32963685985538,3.90006996193835,
-0.183221786705205));
#124115=CARTESIAN_POINT('Ctrl Pts',(-7.3023182558969,3.90439385874872,-0.182795469018913));
#124116=CARTESIAN_POINT('Ctrl Pts',(-7.27501128494097,3.90879118062685,
-0.182361465698886));
#124117=CARTESIAN_POINT('Ctrl Pts',(-7.24771725040738,3.913265984062,-0.181919380376777));
#124118=CARTESIAN_POINT('Ctrl Pts',(-7.18489092487628,3.78339966801642,
-0.969486389062758));
#124119=CARTESIAN_POINT('Ctrl Pts',(-7.18541087543814,3.78403814050821,
-0.965601325531379));
#124120=CARTESIAN_POINT('Ctrl Pts',(-7.18593082600001,3.784676613,-0.961716262));
#124121=CARTESIAN_POINT('Ctrl Pts',(-7.23820222100001,3.848863192,-0.571145109));
#124122=CARTESIAN_POINT('Ctrl Pts',(-7.24783394100001,3.914045302,-0.177209386));
#124123=CARTESIAN_POINT('Ctrl Pts',(-7.46153873851908,3.78339966801642,
-0.758620738679522));
#124124=CARTESIAN_POINT('Ctrl Pts',(-7.46194452325954,3.78403814050821,
-0.754586229339761));
#124125=CARTESIAN_POINT('Ctrl Pts',(-7.462350308,3.784676613,-0.750551720000001));
#124126=CARTESIAN_POINT('Ctrl Pts',(-7.503144445,3.848863192,-0.34495656));
#124127=CARTESIAN_POINT('Ctrl Pts',(-7.499738154,3.914045302,0.062670712));
#124128=CARTESIAN_POINT('Origin',(0.193420885555706,4.01777118640439,-0.0125098067846215));
#124129=CARTESIAN_POINT('Ctrl Pts',(-7.038030922,3.914032935,-1.740293292));
#124130=CARTESIAN_POINT('Ctrl Pts',(-7.053700988,3.90342418,-1.67692098));
#124131=CARTESIAN_POINT('Ctrl Pts',(-7.068227363,3.892857143,-1.613276771));
#124132=CARTESIAN_POINT('Ctrl Pts',(-7.141970577,3.839213527,-1.290186641));
#124133=CARTESIAN_POINT('Ctrl Pts',(-7.185930826,3.784676613,-0.961716262));
#124134=CARTESIAN_POINT('Ctrl Pts',(-7.18645899013354,3.78402137462933,
-0.957769826821296));
#124135=CARTESIAN_POINT('Ctrl Pts',(-7.18698715426708,3.78336613625867,
-0.953823391642592));
#124136=CARTESIAN_POINT('Ctrl Pts',(-7.21776353400001,3.914032935,-2.038109313));
#124137=CARTESIAN_POINT('Ctrl Pts',(-7.236115215,3.90342418,-1.97311864));
#124138=CARTESIAN_POINT('Ctrl Pts',(-7.253293629,3.892857143,-1.907808045));
#124139=CARTESIAN_POINT('Ctrl Pts',(-7.340499928,3.839213527,-1.576258498));
#124140=CARTESIAN_POINT('Ctrl Pts',(-7.397095368,3.784676613,-1.238135744));
#124141=CARTESIAN_POINT('Ctrl Pts',(-7.39777533870557,3.78402137462933,
-1.23407333954463));
#124142=CARTESIAN_POINT('Ctrl Pts',(-7.39845530941115,3.78336613625867,
-1.23001093508926));
#124143=CARTESIAN_POINT('',(-7.03916235933143,3.91326598489301,-1.73571117188066));
#124144=CARTESIAN_POINT('Ctrl Pts',(-7.03916235763906,3.91326598504639,
-1.73571117593494));
#124145=CARTESIAN_POINT('Ctrl Pts',(-7.05422615,3.903042157,-1.674620094));
#124146=CARTESIAN_POINT('Ctrl Pts',(-7.068227363,3.892857143,-1.613276771));
#124147=CARTESIAN_POINT('Ctrl Pts',(-7.14197057734831,3.83921352753312,
-1.29018664159581));
#124148=CARTESIAN_POINT('Ctrl Pts',(-7.18593082707106,3.78467661278557,
-0.96171626364151));
#124149=CARTESIAN_POINT('Ctrl Pts',(-7.28242661707377,3.87435041323117,
-1.79339414618054));
#124150=CARTESIAN_POINT('Ctrl Pts',(-7.25450801706575,3.87860220116321,
-1.78672327941277));
#124151=CARTESIAN_POINT('Ctrl Pts',(-7.22659324614468,3.88292159131356,
-1.78007903323408));
#124152=CARTESIAN_POINT('Ctrl Pts',(-7.19868298126388,3.88731207464196,
-1.77346334495166));
#124153=CARTESIAN_POINT('Ctrl Pts',(-7.17207744626437,3.8914973146731,-1.76715692231842));
#124154=CARTESIAN_POINT('Ctrl Pts',(-7.14547428273653,3.89574618497195,
-1.76088229411127));
#124155=CARTESIAN_POINT('Ctrl Pts',(-7.1188867549914,3.90006996196626,-1.75459342542347));
#124156=CARTESIAN_POINT('Ctrl Pts',(-7.09229849054837,3.90439385876552,
-1.74830438248117));
#124157=CARTESIAN_POINT('Ctrl Pts',(-7.06572323930961,3.90879118062557,
-1.74201033436876));
#124158=CARTESIAN_POINT('Ctrl Pts',(-7.03916235886328,3.91326598396044,
-1.73571117489821));
#124159=CARTESIAN_POINT('Ctrl Pts',(-6.80850125154208,3.78339966801642,
-2.49135950079383));
#124160=CARTESIAN_POINT('Ctrl Pts',(-6.80984421977104,3.78403814050821,
-2.48767704189692));
#124161=CARTESIAN_POINT('Ctrl Pts',(-6.811187188,3.784676613,-2.483994583));
#124162=CARTESIAN_POINT('Ctrl Pts',(-6.94619776,3.848863192,-2.113791572));
#124163=CARTESIAN_POINT('Ctrl Pts',(-7.040288831,3.914045302,-1.731136382));
#124164=CARTESIAN_POINT('Ctrl Pts',(-7.12401107506173,3.78339966801642,
-2.34489487403908));
#124165=CARTESIAN_POINT('Ctrl Pts',(-7.12527467303087,3.78403814050821,
-2.34104192101954));
#124166=CARTESIAN_POINT('Ctrl Pts',(-7.126538271,3.784676613,-2.337188968));
#124167=CARTESIAN_POINT('Ctrl Pts',(-7.253569634,3.848863192,-1.949845932));
#124168=CARTESIAN_POINT('Ctrl Pts',(-7.337870794,3.914045302,-1.551016507));
#124169=CARTESIAN_POINT('Origin',(0.191588194309098,4.01777119498489,0.0293624839387421));
#124170=CARTESIAN_POINT('Ctrl Pts',(-6.499374055,3.914032935,-3.212574807));
#124171=CARTESIAN_POINT('Ctrl Pts',(-6.528300937,3.90342418,-3.154052706));
#124172=CARTESIAN_POINT('Ctrl Pts',(-6.556169318,3.892857143,-3.095019205));
#124173=CARTESIAN_POINT('Ctrl Pts',(-6.697643284,3.839213527,-2.795335353));
#124174=CARTESIAN_POINT('Ctrl Pts',(-6.811187188,3.784676613,-2.483994583));
#124175=CARTESIAN_POINT('Ctrl Pts',(-6.81255137084789,3.78402137462933,
-2.48025395295892));
#124176=CARTESIAN_POINT('Ctrl Pts',(-6.81391555369579,3.78336613625867,
-2.47651332291784));
#124177=CARTESIAN_POINT('Ctrl Pts',(-6.610882977,3.914032935,-3.542065254));
#124178=CARTESIAN_POINT('Ctrl Pts',(-6.64277668,3.90342418,-3.482539096));
#124179=CARTESIAN_POINT('Ctrl Pts',(-6.673593319,3.892857143,-3.422448278));
#124180=CARTESIAN_POINT('Ctrl Pts',(-6.830034135,3.839213527,-3.117396951));
#124181=CARTESIAN_POINT('Ctrl Pts',(-6.957992803,3.784676613,-2.799345666));
#124182=CARTESIAN_POINT('Ctrl Pts',(-6.95953017325041,3.78402137462933,
-2.7955244119083));
#124183=CARTESIAN_POINT('Ctrl Pts',(-6.96106754350082,3.78336613625867,
-2.7917031578166));
#124184=CARTESIAN_POINT('',(-6.50146406065124,3.91326598485366,-3.20834304064166));
#124185=CARTESIAN_POINT('Ctrl Pts',(-6.50146405798387,3.91326598504639,
-3.20834304420609));
#124186=CARTESIAN_POINT('Ctrl Pts',(-6.529308444,3.903042157,-3.151918508));
#124187=CARTESIAN_POINT('Ctrl Pts',(-6.556169318,3.892857143,-3.095019205));
#124188=CARTESIAN_POINT('Ctrl Pts',(-6.69764328314188,3.83921352754265,
-2.79533535427979));
#124189=CARTESIAN_POINT('Ctrl Pts',(-6.81118718892826,3.78467661279769,
-2.48399458497579));
#124190=CARTESIAN_POINT('Ctrl Pts',(-6.72664080068503,3.874350413243,-3.31697204352362));
#124191=CARTESIAN_POINT('Ctrl Pts',(-6.70080896102677,3.87860220111571,
-3.3044554644234));
#124192=CARTESIAN_POINT('Ctrl Pts',(-6.67497513854352,3.88292159126161,
-3.29196570633432));
#124193=CARTESIAN_POINT('Ctrl Pts',(-6.64913957764185,3.88731207458674,
-3.27950480713943));
#124194=CARTESIAN_POINT('Ctrl Pts',(-6.62451175980179,3.89149731461202,
-3.26762642150409));
#124195=CARTESIAN_POINT('Ctrl Pts',(-6.59987942312048,3.89574618490558,
-3.25577959675733));
#124196=CARTESIAN_POINT('Ctrl Pts',(-6.57526541791268,3.90006996188385,
-3.24392222576582));
#124197=CARTESIAN_POINT('Ctrl Pts',(-6.55065073069009,3.90439385866708,
-3.23206452622549));
#124198=CARTESIAN_POINT('Ctrl Pts',(-6.52604982838253,3.90879118050865,
-3.22020473601112));
#124199=CARTESIAN_POINT('Ctrl Pts',(-6.50146405949151,3.91326598380885,
-3.20834304338909));
#124200=CARTESIAN_POINT('Ctrl Pts',(-6.1137536276454,3.78339966801642,-3.8967394111811));
#124201=CARTESIAN_POINT('Ctrl Pts',(-6.11585681782271,3.78403814050821,
-3.89343174459055));
#124202=CARTESIAN_POINT('Ctrl Pts',(-6.117960008,3.784676613,-3.890124078));
#124203=CARTESIAN_POINT('Ctrl Pts',(-6.329396811,3.848863192,-3.557599489));
#124204=CARTESIAN_POINT('Ctrl Pts',(-6.503547641,3.914045302,-3.204117364));
#124205=CARTESIAN_POINT('Ctrl Pts',(-6.45337257147076,3.78339966801642,
-3.82152433181391));
#124206=CARTESIAN_POINT('Ctrl Pts',(-6.45543489823538,3.78403814050821,
-3.81803309490696));
#124207=CARTESIAN_POINT('Ctrl Pts',(-6.457497225,3.784676613,-3.814541858));
#124208=CARTESIAN_POINT('Ctrl Pts',(-6.664825969,3.848863192,-3.463562675));
#124209=CARTESIAN_POINT('Ctrl Pts',(-6.832892752,3.914045302,-3.092179918));
#124210=CARTESIAN_POINT('Origin',(0.180796726433546,4.01777118709131,0.0698617078634745));
#124211=CARTESIAN_POINT('Ctrl Pts',(-5.656813681,3.914032935,-4.53463989500001));
#124212=CARTESIAN_POINT('Ctrl Pts',(-5.697644791,3.90342418,-4.483704433));
#124213=CARTESIAN_POINT('Ctrl Pts',(-5.737552082,3.892857143,-4.43204198));
#124214=CARTESIAN_POINT('Ctrl Pts',(-5.940141634,3.839213527,-4.169777291));
#124215=CARTESIAN_POINT('Ctrl Pts',(-6.117960008,3.784676613,-3.890124078));
#124216=CARTESIAN_POINT('Ctrl Pts',(-6.12009642190956,3.78402137462933,
-3.88676416079535));
#124217=CARTESIAN_POINT('Ctrl Pts',(-6.12223283581911,3.78336613625867,
-3.8834042435907));
#124218=CARTESIAN_POINT('Ctrl Pts',(-5.69488488000001,3.914032935,-4.88039816));
#124219=CARTESIAN_POINT('Ctrl Pts',(-5.73882929,3.90342418,-4.82911989400001));
#124220=CARTESIAN_POINT('Ctrl Pts',(-5.781843203,3.892857143,-4.777058632));
#124221=CARTESIAN_POINT('Ctrl Pts',(-6.000203538,3.839213527,-4.512769388));
#124222=CARTESIAN_POINT('Ctrl Pts',(-6.193542228,3.784676613,-4.229661295));
#124223=CARTESIAN_POINT('Ctrl Pts',(-6.19586511206018,3.78402137462933,
-4.22625986884708));
#124224=CARTESIAN_POINT('Ctrl Pts',(-6.19818799612036,3.78336613625867,
-4.22285844269416));
#124225=CARTESIAN_POINT('',(-5.65976452842113,3.91326598494767,-4.53095635412661));
#124226=CARTESIAN_POINT('Ctrl Pts',(-5.65976452843428,3.91326598549518,
-4.53095635402317));
#124227=CARTESIAN_POINT('Ctrl Pts',(-5.68600352383997,3.90644394849667,
-4.49818037437931));
#124228=CARTESIAN_POINT('Ctrl Pts',(-5.71193410056366,3.89964051894245,
-4.46520603921559));
#124229=CARTESIAN_POINT('Ctrl Pts',(-5.73755208191494,3.89285714302252,
-4.43204198011011));
#124230=CARTESIAN_POINT('Ctrl Pts',(-5.82781467713491,3.86895654227978,
-4.31519147509118));
#124231=CARTESIAN_POINT('Ctrl Pts',(-5.91481573894974,3.84480668268621,
-4.19517787889522));
#124232=CARTESIAN_POINT('Ctrl Pts',(-5.99824711819163,3.82047230181262,
-4.07228824113556));
#124233=CARTESIAN_POINT('Ctrl Pts',(-6.03901424766822,3.80858177735024,
-4.01224059695898));
#124234=CARTESIAN_POINT('Ctrl Pts',(-6.07892954915294,3.79664725893554,
-3.95150690003611));
#124235=CARTESIAN_POINT('Ctrl Pts',(-6.11796000820442,3.78467661307154,
-3.89012408033314));
#124236=CARTESIAN_POINT('Ctrl Pts',(-5.85632473635433,3.87435041325547,
-4.68545201425032));
#124237=CARTESIAN_POINT('Ctrl Pts',(-5.83378752536501,3.87860220116027,
-4.66767498378072));
#124238=CARTESIAN_POINT('Ctrl Pts',(-5.81124261200345,3.88292159132248,
-4.64992372110351));
#124239=CARTESIAN_POINT('Ctrl Pts',(-5.78868979708449,3.88731207466434,
-4.63220026889469));
#124240=CARTESIAN_POINT('Ctrl Pts',(-5.76719126574319,3.8914973146917,-4.61530534051627));
#124241=CARTESIAN_POINT('Ctrl Pts',(-5.74568153657525,3.89574618498683,
-4.59844026372362));
#124242=CARTESIAN_POINT('Ctrl Pts',(-5.72419197744197,3.9000699619644,-4.58156882796319));
#124243=CARTESIAN_POINT('Ctrl Pts',(-5.70270182286743,3.90439385874691,
-4.56469692472231));
#124244=CARTESIAN_POINT('Ctrl Pts',(-5.68122558035583,3.90879118058365,
-4.54782594303456));
#124245=CARTESIAN_POINT('Ctrl Pts',(-5.65976452598906,3.91326598372246,
-4.53095635732969));
#124246=CARTESIAN_POINT('Ctrl Pts',(-5.13313367838099,3.78339966801642,
-5.11991211792546));
#124247=CARTESIAN_POINT('Ctrl Pts',(-5.13589874769049,3.78403814050821,
-5.11713390646273));
#124248=CARTESIAN_POINT('Ctrl Pts',(-5.13866381700001,3.784676613,-5.114355695));
#124249=CARTESIAN_POINT('Ctrl Pts',(-5.416640303,3.848863192,-4.835058009));
#124250=CARTESIAN_POINT('Ctrl Pts',(-5.662707791,3.914045302,-4.52727738));
#124251=CARTESIAN_POINT('Ctrl Pts',(-5.48098153912164,3.78339966801642,
-5.11946355990375));
#124252=CARTESIAN_POINT('Ctrl Pts',(-5.48374616256082,3.78403814050821,
-5.11649728545188));
#124253=CARTESIAN_POINT('Ctrl Pts',(-5.486510786,3.784676613,-5.113531011));
#124254=CARTESIAN_POINT('Ctrl Pts',(-5.76444244800001,3.848863192,-4.815327076));
#124255=CARTESIAN_POINT('Ctrl Pts',(-6.008416238,3.914045302,-4.488756433));
#124256=CARTESIAN_POINT('Origin',(0.161551797490415,4.01777118461528,0.107094516475824));
#124257=CARTESIAN_POINT('Ctrl Pts',(-4.549746986,3.914032935,-5.644670262));
#124258=CARTESIAN_POINT('Ctrl Pts',(-4.600573106,3.90342418,-5.603703124));
#124259=CARTESIAN_POINT('Ctrl Pts',(-4.650653287,3.892857143,-5.561827398));
#124260=CARTESIAN_POINT('Ctrl Pts',(-4.904885564,3.839213527,-5.349245077));
#124261=CARTESIAN_POINT('Ctrl Pts',(-5.138663817,3.784676613,-5.114355695));
#124262=CARTESIAN_POINT('Ctrl Pts',(-5.14147256561369,3.78402137462933,
-5.11153359663286));
#124263=CARTESIAN_POINT('Ctrl Pts',(-5.14428131422739,3.78336613625867,
-5.10871149826573));
#124264=CARTESIAN_POINT('Ctrl Pts',(-4.512600295,3.914032935,-5.99052907300001));
#124265=CARTESIAN_POINT('Ctrl Pts',(-4.566540621,3.90342418,-5.949896413));
#124266=CARTESIAN_POINT('Ctrl Pts',(-4.619740525,3.892857143,-5.908299035));
#124267=CARTESIAN_POINT('Ctrl Pts',(-4.889810092,3.839213527,-5.697129743));
#124268=CARTESIAN_POINT('Ctrl Pts',(-5.139488502,3.784676613,-5.462202664));
#124269=CARTESIAN_POINT('Ctrl Pts',(-5.14248828439617,3.78402137462933,
-5.45938011271906));
#124270=CARTESIAN_POINT('Ctrl Pts',(-5.14548806679234,3.78336613625867,
-5.45655756143813));
#124271=CARTESIAN_POINT('',(-4.55342069631209,3.91326598487342,-5.64170718412929));
#124272=CARTESIAN_POINT('Ctrl Pts',(-4.55342069208161,3.91326598504639,
-5.64170718634669));
#124273=CARTESIAN_POINT('Ctrl Pts',(-4.602383621,3.903042157,-5.602189219));
#124274=CARTESIAN_POINT('Ctrl Pts',(-4.650653287,3.892857143,-5.561827398));
#124275=CARTESIAN_POINT('Ctrl Pts',(-4.90488556315104,3.83921352756483,
-5.34924507770047));
#124276=CARTESIAN_POINT('Ctrl Pts',(-5.13866381694183,3.78467661279893,
-5.114355697307));
#124277=CARTESIAN_POINT('Ctrl Pts',(-4.71217343650642,3.87435041320727,
-5.83484545654915));
#124278=CARTESIAN_POINT('Ctrl Pts',(-4.69398466915291,3.87860220113085,
-5.81263920890565));
#124279=CARTESIAN_POINT('Ctrl Pts',(-4.6757828400969,3.8829215912813,-5.79045647096184));
#124280=CARTESIAN_POINT('Ctrl Pts',(-4.65756731577416,3.88731207461094,
-5.76829919469483));
#124281=CARTESIAN_POINT('Ctrl Pts',(-4.64020331825134,3.89149731464626,
-5.74717771153595));
#124282=CARTESIAN_POINT('Ctrl Pts',(-4.62282196747897,3.89574618494989,
-5.72608297484968));
#124283=CARTESIAN_POINT('Ctrl Pts',(-4.60546168216947,3.90006996193938,
-5.70498636382479));
#124284=CARTESIAN_POINT('Ctrl Pts',(-4.58810091583424,3.90439385873382,
-5.68388916824655));
#124285=CARTESIAN_POINT('Ctrl Pts',(-4.57075353820189,3.90879118058493,
-5.66279586335939));
#124286=CARTESIAN_POINT('Ctrl Pts',(-4.55342069426683,3.91326598388217,
-5.64170718630607));
#124287=CARTESIAN_POINT('Ctrl Pts',(-3.91249410326131,3.78339966801642,
-6.10368342451692));
#124288=CARTESIAN_POINT('Ctrl Pts',(-3.91579176013065,3.78403814050821,
-6.10156457425846));
#124289=CARTESIAN_POINT('Ctrl Pts',(-3.919089417,3.784676613,-6.09944572400001));
#124290=CARTESIAN_POINT('Ctrl Pts',(-4.250607714,3.848863192,-5.88643459));
#124291=CARTESIAN_POINT('Ctrl Pts',(-4.55708601800001,3.914045302,-5.63874693700001));
#124292=CARTESIAN_POINT('Ctrl Pts',(-4.25230590117908,3.78339966801642,
-6.17802236055207));
#124293=CARTESIAN_POINT('Ctrl Pts',(-4.25564355058954,3.78403814050821,
-6.17571974827603));
#124294=CARTESIAN_POINT('Ctrl Pts',(-4.2589812,3.784676613,-6.173417136));
#124295=CARTESIAN_POINT('Ctrl Pts',(-4.594520006,3.848863192,-5.941932136));
#124296=CARTESIAN_POINT('Ctrl Pts',(-4.90299285900001,3.914045302,-5.675443685));
#124297=CARTESIAN_POINT('Origin',(0.134752179725973,4.0177709926056,0.139318973597412));
#124298=CARTESIAN_POINT('Ctrl Pts',(-3.229939179,3.914032935,-6.49076212));
#124299=CARTESIAN_POINT('Ctrl Pts',(-3.288383736,3.90342418,-6.461678884));
#124300=CARTESIAN_POINT('Ctrl Pts',(-3.346295113,3.892857143,-6.431547949));
#124301=CARTESIAN_POINT('Ctrl Pts',(-3.640282496,3.839213527,-6.278588109));
#124302=CARTESIAN_POINT('Ctrl Pts',(-3.919089417,3.784676613,-6.09944572399999));
#124303=CARTESIAN_POINT('Ctrl Pts',(-3.92243916635777,3.78402137462933,
-6.09729340264818));
#124304=CARTESIAN_POINT('Ctrl Pts',(-3.92578891571553,3.78336613625867,
-6.09514108129637));
#124305=CARTESIAN_POINT('Ctrl Pts',(-3.119311536,3.914032935,-6.820549504));
#124306=CARTESIAN_POINT('Ctrl Pts',(-3.180725587,3.90342418,-6.792462389));
#124307=CARTESIAN_POINT('Ctrl Pts',(-3.241623914,3.892857143,-6.763273941));
#124308=CARTESIAN_POINT('Ctrl Pts',(-3.55077456,3.839213527,-6.615098643));
#124309=CARTESIAN_POINT('Ctrl Pts',(-3.845118005,3.784676613,-6.439337507));
#124310=CARTESIAN_POINT('Ctrl Pts',(-3.84865441924078,3.78402137462933,
-6.43722580995057));
#124311=CARTESIAN_POINT('Ctrl Pts',(-3.85219083348155,3.78336613625867,
-6.43511411290114));
#124312=CARTESIAN_POINT('',(-3.234163974001,3.91326598471179,-6.4886580577403));
#124313=CARTESIAN_POINT('Ctrl Pts',(-3.23416396978397,3.91326598504639,
-6.48865805903995));
#124314=CARTESIAN_POINT('Ctrl Pts',(-3.290477367,3.903042157,-6.460589581));
#124315=CARTESIAN_POINT('Ctrl Pts',(-3.346295113,3.892857143,-6.431547949));
#124316=CARTESIAN_POINT('Ctrl Pts',(-3.64028249503674,3.83921352754219,
-6.27858810986231));
#124317=CARTESIAN_POINT('Ctrl Pts',(-3.91908941581858,3.78467661181153,
-6.09944572483374));
#124318=CARTESIAN_POINT('Ctrl Pts',(-3.3476861436547,3.87435041322755,-6.71140801016537));
#124319=CARTESIAN_POINT('Ctrl Pts',(-3.33469630621779,3.87860220110384,
-6.68581088513763));
#124320=CARTESIAN_POINT('Ctrl Pts',(-3.32168865877955,3.88292159125227,
-6.66023391214072));
#124321=CARTESIAN_POINT('Ctrl Pts',(-3.30866216274858,3.8873120745777,-6.63467886147286));
#124322=CARTESIAN_POINT('Ctrl Pts',(-3.29624462038394,3.89149731461195,
-6.61031844071623));
#124323=CARTESIAN_POINT('Ctrl Pts',(-3.28380438072982,3.89574618490461,
-6.58598041070877));
#124324=CARTESIAN_POINT('Ctrl Pts',(-3.27138511704215,3.90006996189716,
-6.56164507859973));
#124325=CARTESIAN_POINT('Ctrl Pts',(-3.2589655092365,3.90439385869467,-6.53730907219747));
#124326=CARTESIAN_POINT('Ctrl Pts',(-3.24655814078464,3.90879118056004,
-6.51297974367115));
#124327=CARTESIAN_POINT('Ctrl Pts',(-3.23416397113967,3.91326598383281,
-6.48865805919438));
#124328=CARTESIAN_POINT('Ctrl Pts',(-2.50891065267966,3.78339966801642,
-6.80205327793971));
#124329=CARTESIAN_POINT('Ctrl Pts',(-2.51258670233983,3.78403814050821,
-6.80069286396985));
#124330=CARTESIAN_POINT('Ctrl Pts',(-2.516262752,3.784676613,-6.79933245));
#124331=CARTESIAN_POINT('Ctrl Pts',(-2.885821433,3.848863192,-6.662568032));
#124332=CARTESIAN_POINT('Ctrl Pts',(-3.238379968,3.914045302,-6.486554955));
#124333=CARTESIAN_POINT('Ctrl Pts',(-2.82479716579741,3.78339966801642,
-6.94770370202509));
#124334=CARTESIAN_POINT('Ctrl Pts',(-2.8285517763987,3.78403814050821,-6.94617241951255));
#124335=CARTESIAN_POINT('Ctrl Pts',(-2.832306387,3.784676613,-6.944641137));
#124336=CARTESIAN_POINT('Ctrl Pts',(-3.209762915,3.848863192,-6.790699053));
#124337=CARTESIAN_POINT('Ctrl Pts',(-3.568310983,3.914045302,-6.596753499));
#124338=CARTESIAN_POINT('Origin',(0.101652530173353,4.01777101481532,0.165030098550536));
#124339=CARTESIAN_POINT('Ctrl Pts',(-1.759103005,3.914032935,-7.033353156));
#124340=CARTESIAN_POINT('Ctrl Pts',(-1.822433198,3.90342418,-7.017513722));
#124341=CARTESIAN_POINT('Ctrl Pts',(-1.885467899,3.892857143,-7.000536465));
#124342=CARTESIAN_POINT('Ctrl Pts',(-2.205463864,3.839213527,-6.914351339));
#124343=CARTESIAN_POINT('Ctrl Pts',(-2.516262752,3.784676613,-6.79933245));
#124344=CARTESIAN_POINT('Ctrl Pts',(-2.51999687155391,3.78402137462933,
-6.79795054581994));
#124345=CARTESIAN_POINT('Ctrl Pts',(-2.52373099110783,3.78336613625867,
-6.79656864163989));
#124346=CARTESIAN_POINT('Ctrl Pts',(-1.580167237,3.914032935,-7.331648621));
#124347=CARTESIAN_POINT('Ctrl Pts',(-1.646183361,3.90342418,-7.317420373));
#124348=CARTESIAN_POINT('Ctrl Pts',(-1.711932572,3.892857143,-7.302005674));
#124349=CARTESIAN_POINT('Ctrl Pts',(-2.045708757,3.839213527,-7.223752884));
#124350=CARTESIAN_POINT('Ctrl Pts',(-2.370954065,3.784676613,-7.115376084));
#124351=CARTESIAN_POINT('Ctrl Pts',(-2.37486175229012,3.78402137462933,
-7.11407398176059));
#124352=CARTESIAN_POINT('Ctrl Pts',(-2.37876943958024,3.78336613625867,
-7.11277187952119));
#124353=CARTESIAN_POINT('',(-1.76368133860213,3.91326598469372,-7.03220649149698));
#124354=CARTESIAN_POINT('Ctrl Pts',(-1.76368133412727,3.91326598504639,
-7.03220649202675));
#124355=CARTESIAN_POINT('Ctrl Pts',(-1.824712048,3.903042157,-7.016899955));
#124356=CARTESIAN_POINT('Ctrl Pts',(-1.885467899,3.892857143,-7.000536465));
#124357=CARTESIAN_POINT('Ctrl Pts',(-2.2054638634848,3.83921352755012,-6.91435133898436));
#124358=CARTESIAN_POINT('Ctrl Pts',(-2.51626275037259,3.78467661195553,
-6.79933245013235));
#124359=CARTESIAN_POINT('Ctrl Pts',(-1.82666476776869,3.87435041321898,
-7.27415258436543));
#124360=CARTESIAN_POINT('Ctrl Pts',(-1.81948125070448,3.87860220108891,
-7.24636147483946));
#124361=CARTESIAN_POINT('Ctrl Pts',(-1.81227600790523,3.88292159123251,
-7.21858621756027));
#124362=CARTESIAN_POINT('Ctrl Pts',(-1.80504764454275,3.88731207455456,
-7.19082831818905));
#124363=CARTESIAN_POINT('Ctrl Pts',(-1.79815718774571,3.89149731457801,
-7.16436802603133));
#124364=CARTESIAN_POINT('Ctrl Pts',(-1.79123975117751,3.89574618489468,
-7.13792472184617));
#124365=CARTESIAN_POINT('Ctrl Pts',(-1.7843422201044,3.90006996189343,-7.11148856171909));
#124366=CARTESIAN_POINT('Ctrl Pts',(-1.77744449791178,3.9043938586971,-7.08505166908842));
#124367=CARTESIAN_POINT('Ctrl Pts',(-1.77055729322819,3.90879118054189,
-7.05862392934173));
#124368=CARTESIAN_POINT('Ctrl Pts',(-1.76368133504616,3.91326598374363,
-7.03220649222192));
#124369=CARTESIAN_POINT('Ctrl Pts',(-0.988013329107109,3.78339966801642,
-7.18236667945575));
#124370=CARTESIAN_POINT('Ctrl Pts',(-0.991895883553554,3.78403814050821,
-7.18182831322788));
#124371=CARTESIAN_POINT('Ctrl Pts',(-0.995778438,3.784676613,-7.181289947));
#124372=CARTESIAN_POINT('Ctrl Pts',(-1.386097349,3.848863192,-7.12716719800001));
#124373=CARTESIAN_POINT('Ctrl Pts',(-1.76825087,3.914045302,-7.031058872));
#124374=CARTESIAN_POINT('Ctrl Pts',(-1.26520405425852,3.78339966801642,
-7.39251814139622));
#124375=CARTESIAN_POINT('Ctrl Pts',(-1.26920006462926,3.78403814050821,
-7.39182978969811));
#124376=CARTESIAN_POINT('Ctrl Pts',(-1.273196075,3.784676613,-7.39114143800001));
#124377=CARTESIAN_POINT('Ctrl Pts',(-1.674920877,3.848863192,-7.321940429));
#124378=CARTESIAN_POINT('Ctrl Pts',(-2.066778852,3.914045302,-7.209606451));
#124379=CARTESIAN_POINT('Origin',(0.0637993348120211,4.01777099075444,0.183023921145155));
#124380=CARTESIAN_POINT('Ctrl Pts',(-0.206013131,3.914032935,-7.247072415));
#124381=CARTESIAN_POINT('Ctrl Pts',(-0.271267708,3.90342418,-7.245217418));
#124382=CARTESIAN_POINT('Ctrl Pts',(-0.336478302,3.892857143,-7.242187677));
#124383=CARTESIAN_POINT('Ctrl Pts',(-0.667520194,3.839213527,-7.226807185));
#124384=CARTESIAN_POINT('Ctrl Pts',(-0.995778438,3.784676613,-7.181289947));
#124385=CARTESIAN_POINT('Ctrl Pts',(-0.999722324464786,3.78402137462933,
-7.18074307629029));
#124386=CARTESIAN_POINT('Ctrl Pts',(-1.00366621092957,3.78336613625867,
-7.18019620558059));
#124387=CARTESIAN_POINT('Ctrl Pts',(0.032863927,3.914032935,-7.499927997));
#124388=CARTESIAN_POINT('Ctrl Pts',(-0.03466743,3.90342418,-7.500223913));
#124389=CARTESIAN_POINT('Ctrl Pts',(-0.102193166,3.892857143,-7.499303738));
#124390=CARTESIAN_POINT('Ctrl Pts',(-0.444987886,3.839213527,-7.494632467));
#124391=CARTESIAN_POINT('Ctrl Pts',(-0.785926947,3.784676613,-7.458707585));
#124392=CARTESIAN_POINT('Ctrl Pts',(-0.790023188214264,3.78402137462933,
-7.45827596246361));
#124393=CARTESIAN_POINT('Ctrl Pts',(-0.794119429428528,3.78336613625867,
-7.4578443399272));
#124394=CARTESIAN_POINT('',(-0.210730925048304,3.91326598495388,-7.24693676499616));
#124395=CARTESIAN_POINT('Ctrl Pts',(-0.210730925117643,3.91326598525536,
-7.24693676569531));
#124396=CARTESIAN_POINT('Ctrl Pts',(-0.341742803026686,3.89196925411006,
-7.24312712114134));
#124397=CARTESIAN_POINT('Ctrl Pts',(-0.472587783383507,3.87079710536095,
-7.23576926099415));
#124398=CARTESIAN_POINT('Ctrl Pts',(-0.668801818713384,3.83867883707161,
-7.21938563561741));
#124399=CARTESIAN_POINT('Ctrl Pts',(-0.734255518074978,3.82792484001174,
-7.21302242832566));
#124400=CARTESIAN_POINT('Ctrl Pts',(-0.8323440796812,3.81174904512853,-7.20213774459991));
#124401=CARTESIAN_POINT('Ctrl Pts',(-0.865052750424345,3.80634502469735,
-7.19828232153745));
#124402=CARTESIAN_POINT('Ctrl Pts',(-0.91408637592218,3.79822878950977,
-7.1921636313569));
#124403=CARTESIAN_POINT('Ctrl Pts',(-0.93043242491259,3.795520612997,-7.19006725232141));
#124404=CARTESIAN_POINT('Ctrl Pts',(-0.954943348359991,3.79145592368764,
-7.18683874599003));
#124405=CARTESIAN_POINT('Ctrl Pts',(-0.963113831538947,3.79010036834645,
-7.18574837480559));
#124406=CARTESIAN_POINT('Ctrl Pts',(-0.979077887758595,3.78745055926263,
-7.18359021558888));
#124407=CARTESIAN_POINT('Ctrl Pts',(-0.983007263997672,3.7867984191769,
-7.18306083599155));
#124408=CARTESIAN_POINT('Ctrl Pts',(-0.995778437250238,3.78467661296255,
-7.18128994825785));
#124409=CARTESIAN_POINT('Ctrl Pts',(-0.220230577341825,3.87435041326975,
-7.49676586842818));
#124410=CARTESIAN_POINT('Ctrl Pts',(-0.219189274043534,3.87860220113651,
-7.46808025586321));
#124411=CARTESIAN_POINT('Ctrl Pts',(-0.218123345138543,3.8829215912762,
-7.43940545450373));
#124412=CARTESIAN_POINT('Ctrl Pts',(-0.217031104751613,3.88731207459202,
-7.41074263500273));
#124413=CARTESIAN_POINT('Ctrl Pts',(-0.215989923663363,3.89149731462842,
-7.38341972517652));
#124414=CARTESIAN_POINT('Ctrl Pts',(-0.214918741528663,3.89574618493874,
-7.3561076063082));
#124415=CARTESIAN_POINT('Ctrl Pts',(-0.213865463789634,3.90006996194319,
-7.32880674356716));
#124416=CARTESIAN_POINT('Ctrl Pts',(-0.21281215686596,3.9043938587526,-7.30150512436279));
#124417=CARTESIAN_POINT('Ctrl Pts',(-0.211767154034762,3.90879118062038,
-7.27421470500944));
#124418=CARTESIAN_POINT('Ctrl Pts',(-0.210730921496787,3.91326598402241,
-7.24693676549611));
#124419=CARTESIAN_POINT('Ctrl Pts',(0.579082400613263,3.78339966801642,
-7.22684059819051));
#124420=CARTESIAN_POINT('Ctrl Pts',(0.575174885306631,3.78403814050821,
-7.22714945309525));
#124421=CARTESIAN_POINT('Ctrl Pts',(0.57126737,3.784676613,-7.22745830800001));
#124422=CARTESIAN_POINT('Ctrl Pts',(0.178439107,3.848863192,-7.258507946));
#124423=CARTESIAN_POINT('Ctrl Pts',(-0.215440326,3.914045302,-7.246798291));
#124424=CARTESIAN_POINT('Ctrl Pts',(0.353548592258207,3.78339966801642,
-7.49166664761222));
#124425=CARTESIAN_POINT('Ctrl Pts',(0.349498031129104,3.78403814050821,
-7.49185341330611));
#124426=CARTESIAN_POINT('Ctrl Pts',(0.34544747,3.784676613,-7.492040179));
#124427=CARTESIAN_POINT('Ctrl Pts',(-0.0617614,3.848863192,-7.51081600900001));
#124428=CARTESIAN_POINT('Ctrl Pts',(-0.468606438,3.914045302,-7.485346218));
#124429=CARTESIAN_POINT('Origin',(0.0229630490407847,4.01777116662245,0.192459969041543));
#124430=CARTESIAN_POINT('Ctrl Pts',(1.356709689,3.914032935,-7.121926623));
#124431=CARTESIAN_POINT('Ctrl Pts',(1.292581958,3.90342418,-7.134142799));
#124432=CARTESIAN_POINT('Ctrl Pts',(1.228244647,3.892857143,-7.145202243));
#124433=CARTESIAN_POINT('Ctrl Pts',(0.901635979,3.839213527,-7.201345559));
#124434=CARTESIAN_POINT('Ctrl Pts',(0.57126737,3.784676613,-7.227458308));
#124435=CARTESIAN_POINT('Ctrl Pts',(0.567298128376246,3.78402137462933,
-7.22777204183371));
#124436=CARTESIAN_POINT('Ctrl Pts',(0.563328886752492,3.78336613625867,
-7.22808577566744));
#124437=CARTESIAN_POINT('Ctrl Pts',(1.64435841,3.914032935,-7.317519076));
#124438=CARTESIAN_POINT('Ctrl Pts',(1.578469512,3.90342418,-7.332325318));
#124439=CARTESIAN_POINT('Ctrl Pts',(1.51232468,3.892857143,-7.345942694));
#124440=CARTESIAN_POINT('Ctrl Pts',(1.176540125,3.839213527,-7.415071367));
#124441=CARTESIAN_POINT('Ctrl Pts',(0.835849241,3.784676613,-7.453278208));
#124442=CARTESIAN_POINT('Ctrl Pts',(0.831755981529315,3.78402137462933,
-7.453737247326));
#124443=CARTESIAN_POINT('Ctrl Pts',(0.82766272205863,3.78336613625867,-7.45419628665201));
#124444=CARTESIAN_POINT('',(1.35207303378698,3.91326598496294,-7.12280833054815));
#124445=CARTESIAN_POINT('Ctrl Pts',(1.35207303380376,3.91326598533785,-7.12280833096319));
#124446=CARTESIAN_POINT('Ctrl Pts',(1.22330513007813,3.8919692459027,-7.14725144316222));
#124447=CARTESIAN_POINT('Ctrl Pts',(1.09393752589995,3.87079709988476,-7.16819340483977));
#124448=CARTESIAN_POINT('Ctrl Pts',(0.898788929512348,3.83867884132354,
-7.19437302890363));
#124449=CARTESIAN_POINT('Ctrl Pts',(0.833497623644794,3.82792484808616,
-7.20222919913091));
#124450=CARTESIAN_POINT('Ctrl Pts',(0.735362384832814,3.81174904529717,
-7.21268513953307));
#124451=CARTESIAN_POINT('Ctrl Pts',(0.702589622489829,3.80634502484376,
-7.21595125144429));
#124452=CARTESIAN_POINT('Ctrl Pts',(0.653387038160116,3.7982287896232,-7.22051639285995));
#124453=CARTESIAN_POINT('Ctrl Pts',(0.63697249111092,3.79552061309923,-7.22198294333527));
#124454=CARTESIAN_POINT('Ctrl Pts',(0.612340585893026,3.79145592377342,
-7.22409904167042));
#124455=CARTESIAN_POINT('Ctrl Pts',(0.604126726459193,3.79010036842672,
-7.22479057511699));
#124456=CARTESIAN_POINT('Ctrl Pts',(0.588071960564506,3.78745055934405,
-7.22611467263649));
#124457=CARTESIAN_POINT('Ctrl Pts',(0.584120650273446,3.78679841930492,
-7.22644236935304));
#124458=CARTESIAN_POINT('Ctrl Pts',(0.571267371024303,3.78467661302323,
-7.227458308743));
#124459=CARTESIAN_POINT('Ctrl Pts',(1.39650135047031,3.8743504132196,-7.36883871285757));
#124460=CARTESIAN_POINT('Ctrl Pts',(1.39135174990272,3.87860220112565,-7.34059990434166));
#124461=CARTESIAN_POINT('Ctrl Pts',(1.3862285232922,3.8829215912896,-7.31236636061691));
#124462=CARTESIAN_POINT('Ctrl Pts',(1.38113356873396,3.88731207463253,-7.28413886241582));
#124463=CARTESIAN_POINT('Ctrl Pts',(1.37627678961713,3.89149731467127,-7.2572309239414));
#124464=CARTESIAN_POINT('Ctrl Pts',(1.37145162997354,3.89574618496625,-7.23032707475948));
#124465=CARTESIAN_POINT('Ctrl Pts',(1.36661140419777,3.90006996195997,-7.20343806747132));
#124466=CARTESIAN_POINT('Ctrl Pts',(1.36177104430707,3.90439385875865,-7.17654831513167));
#124467=CARTESIAN_POINT('Ctrl Pts',(1.35692498200478,3.9087911806267,-7.14967128594964));
#124468=CARTESIAN_POINT('Ctrl Pts',(1.35207303748469,3.91326598396996,-7.12280833022491));
#124469=CARTESIAN_POINT('Ctrl Pts',(2.11910088016766,3.78339966801642,-6.93339548231832));
#124470=CARTESIAN_POINT('Ctrl Pts',(2.11535111508383,3.78403814050821,-6.93453711665916));
#124471=CARTESIAN_POINT('Ctrl Pts',(2.11160135,3.784676613,-6.935678751));
#124472=CARTESIAN_POINT('Ctrl Pts',(1.734631949,3.848863192,-7.05044893100001));
#124473=CARTESIAN_POINT('Ctrl Pts',(1.347443968,3.914045302,-7.123685476));
#124474=CARTESIAN_POINT('Ctrl Pts',(1.95576969930549,3.78339966801642,-7.24051314774188));
#124475=CARTESIAN_POINT('Ctrl Pts',(1.95185398715275,3.78403814050821,-7.24156629787095));
#124476=CARTESIAN_POINT('Ctrl Pts',(1.947938275,3.784676613,-7.242619448));
#124477=CARTESIAN_POINT('Ctrl Pts',(1.554285971,3.848863192,-7.34849418));
#124478=CARTESIAN_POINT('Ctrl Pts',(1.151477492,3.914045302,-7.41107951600001));
#124479=CARTESIAN_POINT('Origin',(-0.0189470914091824,4.01777118429656,
0.192897026293775));
#124480=CARTESIAN_POINT('Ctrl Pts',(2.855994272,3.914032935,-6.663767457));
#124481=CARTESIAN_POINT('Ctrl Pts',(2.795991928,3.90342418,-6.689483593));
#124482=CARTESIAN_POINT('Ctrl Pts',(2.735536241,3.892857143,-6.714115092));
#124483=CARTESIAN_POINT('Ctrl Pts',(2.428632656,3.839213527,-6.839157018));
#124484=CARTESIAN_POINT('Ctrl Pts',(2.11160135,3.784676613,-6.935678751));
#124485=CARTESIAN_POINT('Ctrl Pts',(2.10779235053235,3.78402137462933,-6.93683841953322));
#124486=CARTESIAN_POINT('Ctrl Pts',(2.10398335106471,3.78336613625867,-6.93799808806644));
#124487=CARTESIAN_POINT('Ctrl Pts',(3.178964521,3.914032935,-6.792951095));
#124488=CARTESIAN_POINT('Ctrl Pts',(3.117798973,3.90342418,-6.821575341));
#124489=CARTESIAN_POINT('Ctrl Pts',(3.056127904,3.892857143,-6.849093534));
#124490=CARTESIAN_POINT('Ctrl Pts',(2.743054426,3.839213527,-6.98878977));
#124491=CARTESIAN_POINT('Ctrl Pts',(2.418542048,3.784676613,-7.099341826));
#124492=CARTESIAN_POINT('Ctrl Pts',(2.41464316655942,3.78402137462933,-7.10067006303679));
#124493=CARTESIAN_POINT('Ctrl Pts',(2.41074428511883,3.78336613625867,-7.10199830007358));
#124494=CARTESIAN_POINT('',(2.85165556048068,3.91326598476041,-6.66562529465688));
#124495=CARTESIAN_POINT('Ctrl Pts',(2.85165556055619,3.9132659853381,-6.66562529507203));
#124496=CARTESIAN_POINT('Ctrl Pts',(2.73115277808001,3.89196925540924,-6.71717821224725));
#124497=CARTESIAN_POINT('Ctrl Pts',(2.60931161017231,3.87079710731511,-6.7654407793461));
#124498=CARTESIAN_POINT('Ctrl Pts',(2.4243532403872,3.83867883409976,-6.8329595489516));
#124499=CARTESIAN_POINT('Ctrl Pts',(2.36227721360391,3.82792483428054,-6.85466775799881));
#124500=CARTESIAN_POINT('Ctrl Pts',(2.26868411913098,3.81174904513295,-6.88597539349721));
#124501=CARTESIAN_POINT('Ctrl Pts',(2.23737968355868,3.80634502473174,-6.89621032060966));
#124502=CARTESIAN_POINT('Ctrl Pts',(2.19030879911846,3.79822878957728,-6.91124583270203));
#124503=CARTESIAN_POINT('Ctrl Pts',(2.174593280194,3.79552061307862,-6.91620673842056));
#124504=CARTESIAN_POINT('Ctrl Pts',(2.15099215400452,3.79145592378738,-6.92356849502875));
#124505=CARTESIAN_POINT('Ctrl Pts',(2.14311898935416,3.79010036845298,-6.92600959777435));
#124506=CARTESIAN_POINT('Ctrl Pts',(2.12772421691881,3.78745055939456,-6.93075403869919));
#124507=CARTESIAN_POINT('Ctrl Pts',(2.12393573115497,3.78679841935278,-6.93192348897099));
#124508=CARTESIAN_POINT('Ctrl Pts',(2.11160135139247,3.78467661307689,-6.93567875136807));
#124509=CARTESIAN_POINT('Ctrl Pts',(2.94793442687894,3.8743504132592,-6.89635284857505));
#124510=CARTESIAN_POINT('Ctrl Pts',(2.93683471205565,3.87860220112973,-6.86988125968828));
#124511=CARTESIAN_POINT('Ctrl Pts',(2.92576188631293,3.88292159126709,-6.84340914287658));
#124512=CARTESIAN_POINT('Ctrl Pts',(2.91471797125888,3.88731207458112,-6.8169368525907));
#124513=CARTESIAN_POINT('Ctrl Pts',(2.90419032953263,3.89149731460779,-6.79170207068235));
#124514=CARTESIAN_POINT('Ctrl Pts',(2.89369444699761,3.8957461849108,-6.76646448526374));
#124515=CARTESIAN_POINT('Ctrl Pts',(2.8831870411466,3.90006996191208,-6.74124463351251));
#124516=CARTESIAN_POINT('Ctrl Pts',(2.87267934415219,3.9043938587183,-6.71602408295953));
#124517=CARTESIAN_POINT('Ctrl Pts',(2.86216881324473,3.90879118058129,-6.6908171839199));
#124518=CARTESIAN_POINT('Ctrl Pts',(2.85165556371442,3.9132659838416,-6.66562529299552));
#124519=CARTESIAN_POINT('Ctrl Pts',(3.56003255805081,3.78339966801642,-6.31575249957073));
#124520=CARTESIAN_POINT('Ctrl Pts',(3.5566158780254,3.78403814050821,-6.31767353178537));
#124521=CARTESIAN_POINT('Ctrl Pts',(3.553199198,3.784676613,-6.319594564));
#124522=CARTESIAN_POINT('Ctrl Pts',(3.209715328,3.848863192,-6.512718759));
#124523=CARTESIAN_POINT('Ctrl Pts',(2.847323279,3.914045302,-6.667477045));
#124524=CARTESIAN_POINT('Ctrl Pts',(3.46654118966067,3.78339966801642,-6.65080130115457));
#124525=CARTESIAN_POINT('Ctrl Pts',(3.46294342083033,3.78403814050821,-6.65267159157729));
#124526=CARTESIAN_POINT('Ctrl Pts',(3.459345652,3.784676613,-6.654541882));
#124527=CARTESIAN_POINT('Ctrl Pts',(3.097656658,3.848863192,-6.84256493));
#124528=CARTESIAN_POINT('Ctrl Pts',(2.717719614,3.914045302,-6.990278972));
#124529=CARTESIAN_POINT('Origin',(-0.0599712116260304,4.0177709640612,0.184313895487016));
#124530=CARTESIAN_POINT('Ctrl Pts',(4.221735737,3.914032935,-5.894017931));
#124531=CARTESIAN_POINT('Ctrl Pts',(4.168664423,3.90342418,-5.93203156800001));
#124532=CARTESIAN_POINT('Ctrl Pts',(4.114917201,3.892857143,-5.969083383));
#124533=CARTESIAN_POINT('Ctrl Pts',(3.842069169,3.839213527,-6.157177096));
#124534=CARTESIAN_POINT('Ctrl Pts',(3.553199198,3.784676613,-6.319594564));
#124535=CARTESIAN_POINT('Ctrl Pts',(3.54972854527601,3.78402137462933,-6.32154594242049));
#124536=CARTESIAN_POINT('Ctrl Pts',(3.54625789255202,3.78336613625867,-6.32349732084099));
#124537=CARTESIAN_POINT('Ctrl Pts',(4.564925784,3.914032935,-5.950752271));
#124538=CARTESIAN_POINT('Ctrl Pts',(4.51134362,3.90342418,-5.991856083));
#124539=CARTESIAN_POINT('Ctrl Pts',(4.457029984,3.892857143,-6.031988372));
#124540=CARTESIAN_POINT('Ctrl Pts',(4.181306552,3.839213527,-6.235720132));
#124541=CARTESIAN_POINT('Ctrl Pts',(3.888146516,3.784676613,-6.41344811100001));
#124542=CARTESIAN_POINT('Ctrl Pts',(3.88462431992685,3.78402137462933,-6.41558343885118));
#124543=CARTESIAN_POINT('Ctrl Pts',(3.88110212385369,3.78336613625867,-6.41771876670236));
#124544=CARTESIAN_POINT('',(4.21789784165354,3.91326598485098,-5.89676502733377));
#124545=CARTESIAN_POINT('Ctrl Pts',(4.21789784484407,3.9132659850464,-5.89676502406029));
#124546=CARTESIAN_POINT('Ctrl Pts',(4.166721337,3.903042157,-5.93337107700001));
#124547=CARTESIAN_POINT('Ctrl Pts',(4.114917201,3.892857143,-5.969083383));
#124548=CARTESIAN_POINT('Ctrl Pts',(3.8420691693967,3.83921352754342,-6.15717709595602));
#124549=CARTESIAN_POINT('Ctrl Pts',(3.55319919982665,3.78467661280563,-6.3195945646125));
#124550=CARTESIAN_POINT('Ctrl Pts',(4.36152536588842,3.87435041321657,-6.10140118971835));
#124551=CARTESIAN_POINT('Ctrl Pts',(4.34499454697019,3.87860220111063,-6.07793460252609));
#124552=CARTESIAN_POINT('Ctrl Pts',(4.32848987505951,3.88292159125983,-6.05446171928498));
#124553=CARTESIAN_POINT('Ctrl Pts',(4.31201340060561,3.88731207458989,-6.03098245170927));
#124554=CARTESIAN_POINT('Ctrl Pts',(4.29630715704654,3.89149731462512,-6.00860077678455));
#124555=CARTESIAN_POINT('Ctrl Pts',(4.28063132748528,3.8957461849378,-5.98620953662333));
#124556=CARTESIAN_POINT('Ctrl Pts',(4.26494805633297,3.90006996192755,-5.963838092623));
#124557=CARTESIAN_POINT('Ctrl Pts',(4.24926435062234,3.90439385872224,-5.94146602874582));
#124558=CARTESIAN_POINT('Ctrl Pts',(4.23358081196648,3.90879118056435,-5.91910790639487));
#124559=CARTESIAN_POINT('Ctrl Pts',(4.21789784426514,3.91326598386267,-5.89676502585713));
#124560=CARTESIAN_POINT('Ctrl Pts',(4.83450107061284,3.78339966801642,-5.40279194947145));
#124561=CARTESIAN_POINT('Ctrl Pts',(4.83157723580641,3.78403814050821,-5.40540255423573));
#124562=CARTESIAN_POINT('Ctrl Pts',(4.828653401,3.784676613,-5.40801315900001));
#124563=CARTESIAN_POINT('Ctrl Pts',(4.534715986,3.848863192,-5.670461097));
#124564=CARTESIAN_POINT('Ctrl Pts',(4.214064918,3.914045302,-5.899504798));
#124565=CARTESIAN_POINT('Ctrl Pts',(4.81522106667948,3.78339966801642,-5.75010537695528));
#124566=CARTESIAN_POINT('Ctrl Pts',(4.81210946883974,3.78403814050821,-5.75270535497764));
#124567=CARTESIAN_POINT('Ctrl Pts',(4.808997871,3.784676613,-5.755305333));
#124568=CARTESIAN_POINT('Ctrl Pts',(4.496184362,3.848863192,-6.016684949));
#124569=CARTESIAN_POINT('Ctrl Pts',(4.156884187,3.914045302,-6.242620752));
#124570=CARTESIAN_POINT('Origin',(-0.0981910086943499,4.0177709938306,0.167112529190243));
#124571=CARTESIAN_POINT('Ctrl Pts',(5.39007353,3.914032935,-4.848670677));
#124572=CARTESIAN_POINT('Ctrl Pts',(5.346414803,3.90342418,-4.89720434));
#124573=CARTESIAN_POINT('Ctrl Pts',(5.301889206,3.892857143,-4.944943968));
#124574=CARTESIAN_POINT('Ctrl Pts',(5.075854798,3.839213527,-5.187294417));
#124575=CARTESIAN_POINT('Ctrl Pts',(4.828653401,3.784676613,-5.408013159));
#124576=CARTESIAN_POINT('Ctrl Pts',(4.82568337888624,3.78402137462933,-5.41066500301309));
#124577=CARTESIAN_POINT('Ctrl Pts',(4.82271335677248,3.78336613625867,-5.41331684702618));
#124578=CARTESIAN_POINT('Ctrl Pts',(5.737436191,3.914032935,-4.830302884));
#124579=CARTESIAN_POINT('Ctrl Pts',(5.693942853,3.90342418,-4.881964294));
#124580=CARTESIAN_POINT('Ctrl Pts',(5.649526295,3.892857143,-4.932834139));
#124581=CARTESIAN_POINT('Ctrl Pts',(5.42404543,3.839213527,-5.19107515));
#124582=CARTESIAN_POINT('Ctrl Pts',(5.175945575,3.784676613,-5.42766869));
#124583=CARTESIAN_POINT('Ctrl Pts',(5.17296475828653,3.78402137462933,-5.43051126311771));
#124584=CARTESIAN_POINT('Ctrl Pts',(5.16998394157306,3.78336613625867,-5.43335383623542));
#124585=CARTESIAN_POINT('',(5.38691590799243,3.9132659848901,-4.85217858241229));
#124586=CARTESIAN_POINT('Ctrl Pts',(5.38691591059486,3.91326598504639,-4.85217857849253));
#124587=CARTESIAN_POINT('Ctrl Pts',(5.3448051,3.903042157,-4.898930239));
#124588=CARTESIAN_POINT('Ctrl Pts',(5.301889206,3.892857143,-4.944943968));
#124589=CARTESIAN_POINT('Ctrl Pts',(5.07585479797788,3.83921352754011,-5.18729441661446));
#124590=CARTESIAN_POINT('Ctrl Pts',(4.82865340218875,3.78467661181152,-5.40801315812267));
#124591=CARTESIAN_POINT('Ctrl Pts',(5.57117622601867,3.87435041325356,-5.02115479276776));
#124592=CARTESIAN_POINT('Ctrl Pts',(5.54998726589277,3.87860220115474,-5.00179047883341));
#124593=CARTESIAN_POINT('Ctrl Pts',(5.52882248806047,3.88292159129895,-4.98241439514008));
#124594=CARTESIAN_POINT('Ctrl Pts',(5.50768387603071,3.88731207461873,-4.96302601472333));
#124595=CARTESIAN_POINT('Ctrl Pts',(5.48753343726377,3.89149731465094,-4.94454398894852));
#124596=CARTESIAN_POINT('Ctrl Pts',(5.46741064524587,3.89574618494883,-4.92604608339457));
#124597=CARTESIAN_POINT('Ctrl Pts',(5.44728484119411,3.90006996193012,-4.90756911091528));
#124598=CARTESIAN_POINT('Ctrl Pts',(5.42715847948854,3.90439385871635,-4.88909162646865));
#124599=CARTESIAN_POINT('Ctrl Pts',(5.40703527793493,3.90879118055703,-4.87062772170752));
#124600=CARTESIAN_POINT('Ctrl Pts',(5.3869159104284,3.91326598389117,-4.85217858048639));
#124601=CARTESIAN_POINT('Ctrl Pts',(5.88291368665964,3.78339966801642,-4.23720285334885));
#124602=CARTESIAN_POINT('Ctrl Pts',(5.88061941232982,3.78403814050821,-4.24038096167442));
#124603=CARTESIAN_POINT('Ctrl Pts',(5.878325138,3.784676613,-4.24355907));
#124604=CARTESIAN_POINT('Ctrl Pts',(5.64767836400001,3.848863192,-4.563058976));
#124605=CARTESIAN_POINT('Ctrl Pts',(5.383761566,3.914045302,-4.855678264));
#124606=CARTESIAN_POINT('Ctrl Pts',(5.93874655798517,3.78339966801642,-4.58054091591451));
#124607=CARTESIAN_POINT('Ctrl Pts',(5.93626662599258,3.78403814050821,-4.58374900945725));
#124608=CARTESIAN_POINT('Ctrl Pts',(5.933786694,3.784676613,-4.586957103));
#124609=CARTESIAN_POINT('Ctrl Pts',(5.684475482,3.848863192,-4.909471467));
#124610=CARTESIAN_POINT('Ctrl Pts',(5.401677476,3.914045302,-5.203064524));
#124611=CARTESIAN_POINT('Origin',(-0.131819659600271,4.01777116439499,0.142097461283107));
#124612=CARTESIAN_POINT('Ctrl Pts',(6.306377476,3.914032935,-3.576604972));
#124613=CARTESIAN_POINT('Ctrl Pts',(6.274172769,3.90342418,-3.633389281));
#124614=CARTESIAN_POINT('Ctrl Pts',(6.240950764,3.892857143,-3.68958447));
#124615=CARTESIAN_POINT('Ctrl Pts',(6.072299097,3.839213527,-3.974859616));
#124616=CARTESIAN_POINT('Ctrl Pts',(5.878325138,3.784676613,-4.24355907));
#124617=CARTESIAN_POINT('Ctrl Pts',(5.87599462144663,3.78402137462933,-4.24678738233974));
#124618=CARTESIAN_POINT('Ctrl Pts',(5.87366410489327,3.78336613625867,-4.25001569467947));
#124619=CARTESIAN_POINT('Ctrl Pts',(6.641670459,3.914032935,-3.483993903));
#124620=CARTESIAN_POINT('Ctrl Pts',(6.610299646,3.90342418,-3.54379728));
#124621=CARTESIAN_POINT('Ctrl Pts',(6.577857036,3.892857143,-3.603026063));
#124622=CARTESIAN_POINT('Ctrl Pts',(6.41316197200001,3.839213527,-3.903701264));
#124623=CARTESIAN_POINT('Ctrl Pts',(6.221723171,3.784676613,-4.188097513));
#124624=CARTESIAN_POINT('Ctrl Pts',(6.21942311331706,3.78402137462933,-4.19151441581224));
#124625=CARTESIAN_POINT('Ctrl Pts',(6.21712305563413,3.78336613625867,-4.1949313186245));
#124626=CARTESIAN_POINT('',(6.30404777322913,3.91326598495116,-3.58070966019294));
#124627=CARTESIAN_POINT('Ctrl Pts',(6.30404777308629,3.91326598539557,-3.58070966019485));
#124628=CARTESIAN_POINT('Ctrl Pts',(6.28331170433608,3.90644394844782,-3.61721671670234));
#124629=CARTESIAN_POINT('Ctrl Pts',(6.26227721073114,3.89964051892997,-3.65351067815672));
#124630=CARTESIAN_POINT('Ctrl Pts',(6.24095076432879,3.89285714298821,-3.68958446996868));
#124631=CARTESIAN_POINT('Ctrl Pts',(6.16580889148348,3.86895650882096,-3.81668732776632));
#124632=CARTESIAN_POINT('Ctrl Pts',(6.08652135128144,3.84480661539908,-3.94193107106089));
#124633=CARTESIAN_POINT('Ctrl Pts',(6.00324074906257,3.82047220032148,-4.06492318798607));
#124634=CARTESIAN_POINT('Ctrl Pts',(5.96254746592548,3.8085817094227,-4.12502065251343));
#124635=CARTESIAN_POINT('Ctrl Pts',(5.92090156723483,3.79664722485402,-4.18458072582146));
#124636=CARTESIAN_POINT('Ctrl Pts',(5.87832513995717,3.78467661302156,-4.24355906959005));
#124637=CARTESIAN_POINT('Ctrl Pts',(6.52032507810972,3.87435041328379,-3.70612477820758));
#124638=CARTESIAN_POINT('Ctrl Pts',(6.49546874906344,3.87860220115049,-3.69176819098134));
#124639=CARTESIAN_POINT('Ctrl Pts',(6.47063350665611,3.88292159130609,-3.67739491099258));
#124640=CARTESIAN_POINT('Ctrl Pts',(6.44582117486303,3.88731207464001,-3.6630039969133));
#124641=CARTESIAN_POINT('Ctrl Pts',(6.42216875293301,3.89149731467131,-3.64928581941188));
#124642=CARTESIAN_POINT('Ctrl Pts',(6.39853991765918,3.89574618498043,-3.63554619022822));
#124643=CARTESIAN_POINT('Ctrl Pts',(6.37491264077159,3.9000699619687,-3.6218276521987));
#124644=CARTESIAN_POINT('Ctrl Pts',(6.35128470921004,3.9043938587619,-3.60810873405048));
#124645=CARTESIAN_POINT('Ctrl Pts',(6.32766278316446,3.90879118060183,-3.59440239872993));
#124646=CARTESIAN_POINT('Ctrl Pts',(6.30404777520749,3.91326598385711,-3.58070965616348));
#124647=CARTESIAN_POINT('Ctrl Pts',(6.6562477962472,3.78339966801642,-2.87348685982246));
#124648=CARTESIAN_POINT('Ctrl Pts',(6.6546903601236,3.78403814050821,-2.87708386691123));
#124649=CARTESIAN_POINT('Ctrl Pts',(6.653132924,3.784676613,-2.880680874));
#124650=CARTESIAN_POINT('Ctrl Pts',(6.496561579,3.848863192,-3.242293289));
#124651=CARTESIAN_POINT('Ctrl Pts',(6.301719506,3.914045302,-3.58480561));
#124652=CARTESIAN_POINT('Ctrl Pts',(6.78458286054716,3.78339966801642,-3.19679545366646));
#124653=CARTESIAN_POINT('Ctrl Pts',(6.78285055327358,3.78403814050821,-3.20046165583323));
#124654=CARTESIAN_POINT('Ctrl Pts',(6.781118246,3.784676613,-3.204127858));
#124655=CARTESIAN_POINT('Ctrl Pts',(6.606966847,3.848863192,-3.572696556));
#124656=CARTESIAN_POINT('Ctrl Pts',(6.39389433,3.914045302,-3.920218782));
#124657=CARTESIAN_POINT('Origin',(-0.1592844565639,4.0177710357927,0.110437880897422));
#124658=CARTESIAN_POINT('Ctrl Pts',(6.927802221,3.914032935,-2.137301193));
#124659=CARTESIAN_POINT('Ctrl Pts',(6.90855739,3.90342418,-2.199680976));
#124660=CARTESIAN_POINT('Ctrl Pts',(6.888192401,3.892857143,-2.261704102));
#124661=CARTESIAN_POINT('Ctrl Pts',(6.78480944,3.839213527,-2.576564797));
#124662=CARTESIAN_POINT('Ctrl Pts',(6.653132924,3.784676613,-2.880680874));
#124663=CARTESIAN_POINT('Ctrl Pts',(6.65155088535002,3.78402137462933,-2.88433470235535));
#124664=CARTESIAN_POINT('Ctrl Pts',(6.64996884670004,3.78336613625867,-2.8879885307107));
#124665=CARTESIAN_POINT('Ctrl Pts',(7.235347597,3.914032935,-1.97477724));
#124666=CARTESIAN_POINT('Ctrl Pts',(7.217566175,3.90342418,-2.039926244));
#124667=CARTESIAN_POINT('Ctrl Pts',(7.198614493,3.892857143,-2.104744493));
#124668=CARTESIAN_POINT('Ctrl Pts',(7.102406188,3.839213527,-2.433794646));
#124669=CARTESIAN_POINT('Ctrl Pts',(6.976579907,3.784676613,-2.752695552));
#124670=CARTESIAN_POINT('Ctrl Pts',(6.97506815649374,3.78402137462933,-2.75652701393514));
#124671=CARTESIAN_POINT('Ctrl Pts',(6.97355640598748,3.78336613625867,-2.76035847587028));
#124672=CARTESIAN_POINT('',(6.92640937136214,3.91326598485584,-2.14181073245289));
#124673=CARTESIAN_POINT('Ctrl Pts',(6.92640937187168,3.9132659850464,-2.14181072785087));
#124674=CARTESIAN_POINT('Ctrl Pts',(6.907821148,3.903042157,-2.201923256));
#124675=CARTESIAN_POINT('Ctrl Pts',(6.888192401,3.892857143,-2.261704102));
#124676=CARTESIAN_POINT('Ctrl Pts',(6.78480944057515,3.83921352756187,-2.57656479577017));
#124677=CARTESIAN_POINT('Ctrl Pts',(6.65313292409509,3.78467661195603,-2.88068087233164));
#124678=CARTESIAN_POINT('Ctrl Pts',(7.16459077630807,3.87435041327016,-2.21780048805586));
#124679=CARTESIAN_POINT('Ctrl Pts',(7.1372293325444,3.87860220113624,-2.20912292591441));
#124680=CARTESIAN_POINT('Ctrl Pts',(7.10988489401252,3.88292159127784,-2.20042452820071));
#124681=CARTESIAN_POINT('Ctrl Pts',(7.08255903964796,3.88731207459879,-2.19170398356326));
#124682=CARTESIAN_POINT('Ctrl Pts',(7.05651059551731,3.89149731462703,-2.18339110094494));
#124683=CARTESIAN_POINT('Ctrl Pts',(7.03048057511907,3.89574618493553,-2.17505219774218));
#124684=CARTESIAN_POINT('Ctrl Pts',(7.00445661063303,3.90006996193304,-2.16673355763766));
#124685=CARTESIAN_POINT('Ctrl Pts',(6.97843192506453,3.90439385873549,-2.15841468703692));
#124686=CARTESIAN_POINT('Ctrl Pts',(6.95241580953439,3.9087911805915,-2.15010681410914));
#124687=CARTESIAN_POINT('Ctrl Pts',(6.92640937246644,3.9132659839127,-2.1418107295464));
#124688=CARTESIAN_POINT('Ctrl Pts',(7.11834315687191,3.78339966801642,-1.37540981543085));
#124689=CARTESIAN_POINT('Ctrl Pts',(7.11759538293595,3.78403814050821,-1.37925752921543));
#124690=CARTESIAN_POINT('Ctrl Pts',(7.116847609,3.784676613,-1.383105243));
#124691=CARTESIAN_POINT('Ctrl Pts',(7.041672795,3.848863192,-1.769921571));
#124692=CARTESIAN_POINT('Ctrl Pts',(6.925016046,3.914045302,-2.146311431));
#124693=CARTESIAN_POINT('Ctrl Pts',(7.31317960960073,3.78339966801642,-1.66357138748205));
#124694=CARTESIAN_POINT('Ctrl Pts',(7.31227592780037,3.78403814050821,-1.66752427074103));
#124695=CARTESIAN_POINT('Ctrl Pts',(7.311372246,3.784676613,-1.671477154));
#124696=CARTESIAN_POINT('Ctrl Pts',(7.220523785,3.848863192,-2.068866324));
#124697=CARTESIAN_POINT('Ctrl Pts',(7.087139791,3.914045302,-2.454067967));
#124698=CARTESIAN_POINT('Origin',(-0.179301663651004,4.01777114362114,0.073614573874817));
#124699=CARTESIAN_POINT('Ctrl Pts',(7.225290633,3.914032935,-0.598059586000001));
#124700=CARTESIAN_POINT('Ctrl Pts',(7.219905545,3.90342418,-0.663118034));
#124701=CARTESIAN_POINT('Ctrl Pts',(7.213349817,3.892857143,-0.728068964));
#124702=CARTESIAN_POINT('Ctrl Pts',(7.180069635,3.839213527,-1.057792671));
#124703=CARTESIAN_POINT('Ctrl Pts',(7.116847609,3.784676613,-1.383105243));
#124704=CARTESIAN_POINT('Ctrl Pts',(7.11608802261588,3.78402137462933,-1.38701373843915));
#124705=CARTESIAN_POINT('Ctrl Pts',(7.11532843623176,3.78336613625867,-1.39092223387829));
#124706=CARTESIAN_POINT('Ctrl Pts',(7.490707924,3.914032935,-0.373222187));
#124707=CARTESIAN_POINT('Ctrl Pts',(7.487347331,3.90342418,-0.440670524));
#124708=CARTESIAN_POINT('Ctrl Pts',(7.482772737,3.892857143,-0.50804741));
#124709=CARTESIAN_POINT('Ctrl Pts',(7.459549785,3.839213527,-0.850086495));
#124710=CARTESIAN_POINT('Ctrl Pts',(7.40521952,3.784676613,-1.188580606));
#124711=CARTESIAN_POINT('Ctrl Pts',(7.40456676443124,3.78402137462933,-1.19264747215549));
#124712=CARTESIAN_POINT('Ctrl Pts',(7.40391400886248,3.78336613625867,-1.19671433831097));
#124713=CARTESIAN_POINT('',(7.22489976603046,3.91326598469533,-0.602763115539841));
#124714=CARTESIAN_POINT('Ctrl Pts',(7.22489976555627,3.91326598504641,-0.60276311152549));
#124715=CARTESIAN_POINT('Ctrl Pts',(7.21966854000001,3.903042157,-0.665466161));
#124716=CARTESIAN_POINT('Ctrl Pts',(7.213349817,3.892857143,-0.728068964));
#124717=CARTESIAN_POINT('Ctrl Pts',(7.18006963483772,3.83921352756005,-1.0577926705533));
#124718=CARTESIAN_POINT('Ctrl Pts',(7.11684761074545,3.78467661272573,-1.38310524181887));
#124719=CARTESIAN_POINT('Ctrl Pts',(7.47384817275591,3.87435041323356,-0.625774312184501));
#124720=CARTESIAN_POINT('Ctrl Pts',(7.44526100500474,3.87860220111994,-0.623181528288914));
#124721=CARTESIAN_POINT('Ctrl Pts',(7.41668596593887,3.88292159125359,-0.620564740192355));
#124722=CARTESIAN_POINT('Ctrl Pts',(7.38812431561052,3.88731207456684,-0.617922327910737));
#124723=CARTESIAN_POINT('Ctrl Pts',(7.36089784559792,3.89149731459655,-0.615403441294617));
#124724=CARTESIAN_POINT('Ctrl Pts',(7.33368377491932,3.89574618490019,-0.612855181841101));
#124725=CARTESIAN_POINT('Ctrl Pts',(7.30647997453019,3.900069961904,-0.610325409987334));
#124726=CARTESIAN_POINT('Ctrl Pts',(7.27927542036719,3.90439385871277,-0.607795568037624));
#124727=CARTESIAN_POINT('Ctrl Pts',(7.25208160005011,3.90879118058398,-0.60527462440069));
#124728=CARTESIAN_POINT('Ctrl Pts',(7.22489976652122,3.91326598385759,-0.602763113096661));
#124729=CARTESIAN_POINT('Ctrl Pts',(7.24759270333537,3.78339966801643,0.18697986331215));
#124730=CARTESIAN_POINT('Ctrl Pts',(7.24768955666769,3.78403814050821,0.183061357656075));
#124731=CARTESIAN_POINT('Ctrl Pts',(7.24778641,3.784676613,0.179142852));
#124732=CARTESIAN_POINT('Ctrl Pts',(7.257523218,3.848863192,-0.214790287));
#124733=CARTESIAN_POINT('Ctrl Pts',(7.224506533,3.914045302,-0.607458115));
#124734=CARTESIAN_POINT('Ctrl Pts',(7.49982020834237,3.78339966801643,-0.0525605731549361));
#124735=CARTESIAN_POINT('Ctrl Pts',(7.49978740717118,3.78403814050821,-0.056615305077468));
#124736=CARTESIAN_POINT('Ctrl Pts',(7.499754606,3.784676613,-0.060670037));
#124737=CARTESIAN_POINT('Ctrl Pts',(7.496457056,3.848863192,-0.468298203));
#124738=CARTESIAN_POINT('Ctrl Pts',(7.448998472,3.914045302,-0.873167661));
#124739=CARTESIAN_POINT('Origin',(-0.190934635113679,4.01777094613612,0.0333488982646781));
#124740=CARTESIAN_POINT('Ctrl Pts',(7.184932486,3.914032935,0.969146623));
#124741=CARTESIAN_POINT('Ctrl Pts',(7.193658941,3.90342418,0.90445157));
#124742=CARTESIAN_POINT('Ctrl Pts',(7.201219013,3.892857143,0.839609869));
#124743=CARTESIAN_POINT('Ctrl Pts',(7.239597753,3.839213527,0.510440663));
#124744=CARTESIAN_POINT('Ctrl Pts',(7.24778641,3.784676613,0.179142852));
#124745=CARTESIAN_POINT('Ctrl Pts',(7.24788479331283,3.78402137462933,0.175162446400145));
#124746=CARTESIAN_POINT('Ctrl Pts',(7.24798317662565,3.78336613625867,0.17118204080029));
#124747=CARTESIAN_POINT('Ctrl Pts',(7.395811073,3.914032935,1.24578432));
#124748=CARTESIAN_POINT('Ctrl Pts',(7.407028448,3.90342418,1.17919046));
#124749=CARTESIAN_POINT('Ctrl Pts',(7.417044844,3.892857143,1.112405405));
#124750=CARTESIAN_POINT('Ctrl Pts',(7.46789312400001,3.839213527,0.773370756));
#124751=CARTESIAN_POINT('Ctrl Pts',(7.487599299,3.784676613,0.431111049));
#124752=CARTESIAN_POINT('Ctrl Pts',(7.48783606050798,3.78402137462933,0.426998940772556));
#124753=CARTESIAN_POINT('Ctrl Pts',(7.48807282201595,3.78336613625867,0.422886832545111));
#124754=CARTESIAN_POINT('',(7.1855618765768,3.91326598494572,0.964469033495719));
#124755=CARTESIAN_POINT('Ctrl Pts',(7.18556187701648,3.91326598546387,0.964469033469786));
#124756=CARTESIAN_POINT('Ctrl Pts',(7.19114716531835,3.90644394851566,0.922857084753342));
#124757=CARTESIAN_POINT('Ctrl Pts',(7.19636592023783,3.89964051897578,0.881234180225402));
#124758=CARTESIAN_POINT('Ctrl Pts',(7.20121901293983,3.89285714308741,0.839609869539318));
#124759=CARTESIAN_POINT('Ctrl Pts',(7.21831844637703,3.8689565293465,0.692950366790978));
#124760=CARTESIAN_POINT('Ctrl Pts',(7.23099246243938,3.84480665659152,0.545262042106412));
#124761=CARTESIAN_POINT('Ctrl Pts',(7.23912501119572,3.82047226237412,0.396949723893768));
#124762=CARTESIAN_POINT('Ctrl Pts',(7.24309881727761,3.808581750969,0.324479898038566));
#124763=CARTESIAN_POINT('Ctrl Pts',(7.24598903370267,3.79664724571288,0.251861386589163));
#124764=CARTESIAN_POINT('Ctrl Pts',(7.2477864112848,3.78467661306747,0.179142853770467));
#124765=CARTESIAN_POINT('Ctrl Pts',(7.43363673495892,3.87435041323103,0.99551237504792));
#124766=CARTESIAN_POINT('Ctrl Pts',(7.40516054742332,3.87860220113494,0.991899144976729));
#124767=CARTESIAN_POINT('Ctrl Pts',(7.37669104475964,3.88292159128888,0.988311965239462));
#124768=CARTESIAN_POINT('Ctrl Pts',(7.3482291093774,3.88731207462033,0.984752688798702));
#124769=CARTESIAN_POINT('Ctrl Pts',(7.32109769297024,3.89149731465741,0.981359798964424));
#124770=CARTESIAN_POINT('Ctrl Pts',(7.2939720717114,3.89574618495298,0.977998260824981));
#124771=CARTESIAN_POINT('Ctrl Pts',(7.26686045491279,3.90006996194473,0.97462087514303));
#124772=CARTESIAN_POINT('Ctrl Pts',(7.23974808689462,3.90439385874143,0.97124339587912));
#124773=CARTESIAN_POINT('Ctrl Pts',(7.21264811464817,3.90879118060208,0.967859533782324));
#124774=CARTESIAN_POINT('Ctrl Pts',(7.18556187633381,3.91326598387345,0.964469036847748));
#124775=CARTESIAN_POINT('Ctrl Pts',(7.03795286930082,3.78339966801642,1.74062657215132));
#124776=CARTESIAN_POINT('Ctrl Pts',(7.03888982115041,3.78403814050821,1.73682049957566));
#124777=CARTESIAN_POINT('Ctrl Pts',(7.039826773,3.784676613,1.733014427));
#124778=CARTESIAN_POINT('Ctrl Pts',(7.134019921,3.848863192,1.350384351));
#124779=CARTESIAN_POINT('Ctrl Pts',(7.186187123,3.914045302,0.959799268000001));
#124780=CARTESIAN_POINT('Ctrl Pts',(7.33577754858687,3.78339966801642,1.56090791565573));
#124781=CARTESIAN_POINT('Ctrl Pts',(7.33661716179344,3.78403814050821,1.55694092982786));
#124782=CARTESIAN_POINT('Ctrl Pts',(7.337456775,3.784676613,1.552973944));
#124783=CARTESIAN_POINT('Ctrl Pts',(7.421864326,3.848863192,1.154167022));
#124784=CARTESIAN_POINT('Ctrl Pts',(7.462550264,3.914045302,0.748560994));
#124785=CARTESIAN_POINT('Origin',(-0.19363957425676,4.01777115777898,-0.00847600782555386));
#124786=CARTESIAN_POINT('Ctrl Pts',(6.808614881,3.914032935,2.491036613));
#124787=CARTESIAN_POINT('Ctrl Pts',(6.83104484,3.90342418,2.429730024));
#124788=CARTESIAN_POINT('Ctrl Pts',(6.852367211,3.892857143,2.368029478));
#124789=CARTESIAN_POINT('Ctrl Pts',(6.96061032600001,3.839213527,2.05480636));
#124790=CARTESIAN_POINT('Ctrl Pts',(7.039826773,3.784676613,1.733014427));
#124791=CARTESIAN_POINT('Ctrl Pts',(7.04077852570941,3.78402137462933,1.7291482305762));
#124792=CARTESIAN_POINT('Ctrl Pts',(7.04173027841881,3.78336613625867,1.7252820341524));
#124793=CARTESIAN_POINT('Ctrl Pts',(6.955094316,3.914032935,2.806539337));
#124794=CARTESIAN_POINT('Ctrl Pts',(6.980365147,3.90342418,2.743913808));
#124795=CARTESIAN_POINT('Ctrl Pts',(7.004504177,3.892857143,2.68084338));
#124796=CARTESIAN_POINT('Ctrl Pts',(7.127046081,3.839213527,2.36066605));
#124797=CARTESIAN_POINT('Ctrl Pts',(7.219867256,3.784676613,2.030644429));
#124798=CARTESIAN_POINT('Ctrl Pts',(7.22098246386582,3.78402137462933,2.02667935629295));
#124799=CARTESIAN_POINT('Ctrl Pts',(7.22209767173163,3.78336613625867,2.0227142835859));
#124800=CARTESIAN_POINT('',(6.81023510037854,3.9132659847791,2.48660368285477));
#124801=CARTESIAN_POINT('Ctrl Pts',(6.81023510083825,3.91326598538396,2.486603682918));
#124802=CARTESIAN_POINT('Ctrl Pts',(6.85518854064161,3.89196924655433,2.36348655994546));
#124803=CARTESIAN_POINT('Ctrl Pts',(6.89678398055128,3.87079709579665,2.23921118101377));
#124804=CARTESIAN_POINT('Ctrl Pts',(6.95419025090827,3.83867884087599,2.0508687836617));
#124805=CARTESIAN_POINT('Ctrl Pts',(6.97250588636221,3.82792484728307,1.9877085761306));
#124806=CARTESIAN_POINT('Ctrl Pts',(6.99870059935963,3.81174904528243,1.89255770731536));
#124807=CARTESIAN_POINT('Ctrl Pts',(7.00722572817433,3.80634502483808,1.86074507440694));
#124808=CARTESIAN_POINT('Ctrl Pts',(7.01969082320505,3.79822878962379,1.81292921698448));
#124809=CARTESIAN_POINT('Ctrl Pts',(7.02379363232968,3.79552061310379,1.79696816810188));
#124810=CARTESIAN_POINT('Ctrl Pts',(7.0298668531405,3.791455923782,1.77300309738959));
#124811=CARTESIAN_POINT('Ctrl Pts',(7.03187813128029,3.79010036843707,1.76500932072657));
#124812=CARTESIAN_POINT('Ctrl Pts',(7.03578215795174,3.78745055935128,1.74938026706327));
#124813=CARTESIAN_POINT('Ctrl Pts',(7.03674478870647,3.78679841926599,1.7455340244289));
#124814=CARTESIAN_POINT('Ctrl Pts',(7.03982677379995,3.78467661301969,1.73301442848594));
#124815=CARTESIAN_POINT('Ctrl Pts',(7.04583670530855,3.87435041328414,2.57025001046774));
#124816=CARTESIAN_POINT('Ctrl Pts',(7.01880301281211,3.87860220114356,2.56059971734375));
#124817=CARTESIAN_POINT('Ctrl Pts',(6.99177024888423,3.88292159129812,2.55097630231711));
#124818=CARTESIAN_POINT('Ctrl Pts',(6.96473887695021,3.88731207463272,2.54138176494956));
#124819=CARTESIAN_POINT('Ctrl Pts',(6.93897114900317,3.89149731467151,2.53223574641716));
#124820=CARTESIAN_POINT('Ctrl Pts',(6.91320234107663,3.89574618498536,2.52312159228064));
#124821=CARTESIAN_POINT('Ctrl Pts',(6.88745061690712,3.90006996197851,2.51399497175813));
#124822=CARTESIAN_POINT('Ctrl Pts',(6.86169817919848,3.90439385877662,2.50486809835155));
#124823=CARTESIAN_POINT('Ctrl Pts',(6.83595921954747,3.90879118062751,2.49573765613441));
#124824=CARTESIAN_POINT('Ctrl Pts',(6.81023509907772,3.91326598391623,2.48660368644794));
#124825=CARTESIAN_POINT('Ctrl Pts',(6.49922618194218,3.78339966801642,3.21288351652541));
#124826=CARTESIAN_POINT('Ctrl Pts',(6.50095942147108,3.78403814050821,3.20936784476271));
#124827=CARTESIAN_POINT('Ctrl Pts',(6.502692661,3.784676613,3.205852173));
#124828=CARTESIAN_POINT('Ctrl Pts',(6.676937781,3.848863192,2.852416518));
#124829=CARTESIAN_POINT('Ctrl Pts',(6.81184959,3.914045302,2.482177504));
#124830=CARTESIAN_POINT('Ctrl Pts',(6.8287220845867,3.78339966801642,3.10139008475842));
#124831=CARTESIAN_POINT('Ctrl Pts',(6.83039485279335,3.78403814050821,3.09769633687921));
#124832=CARTESIAN_POINT('Ctrl Pts',(6.832067621,3.784676613,3.094002589));
#124833=CARTESIAN_POINT('Ctrl Pts',(7.00023347,3.848863192,2.72266468));
#124834=CARTESIAN_POINT('Ctrl Pts',(7.127161499,3.914045302,2.33528777));
#124835=CARTESIAN_POINT('Origin',(-0.187290317839145,4.01777099682798,-0.0499046783036339));
#124836=CARTESIAN_POINT('Ctrl Pts',(6.113934011,3.914032935,3.896448499));
#124837=CARTESIAN_POINT('Ctrl Pts',(6.149018675,3.90342418,3.841397003));
#124838=CARTESIAN_POINT('Ctrl Pts',(6.183106334,3.892857143,3.785722661));
#124839=CARTESIAN_POINT('Ctrl Pts',(6.356152497,3.839213527,3.503091595));
#124840=CARTESIAN_POINT('Ctrl Pts',(6.502692661,3.784676613,3.205852173));
#124841=CARTESIAN_POINT('Ctrl Pts',(6.50445328020732,3.78402137462933,3.20228096479837));
#124842=CARTESIAN_POINT('Ctrl Pts',(6.50621389941464,3.78336613625867,3.19870975659674));
#124843=CARTESIAN_POINT('Ctrl Pts',(6.18916508000001,3.914032935,4.236063694));
#124844=CARTESIAN_POINT('Ctrl Pts',(6.22730773,3.90342418,4.180334797));
#124845=CARTESIAN_POINT('Ctrl Pts',(6.264440681,3.892857143,4.123928098));
#124846=CARTESIAN_POINT('Ctrl Pts',(6.452946284,3.839213527,3.837579223));
#124847=CARTESIAN_POINT('Ctrl Pts',(6.614542245,3.784676613,3.535227133));
#124848=CARTESIAN_POINT('Ctrl Pts',(6.61648375335509,3.78402137462933,3.53159449821582));
#124849=CARTESIAN_POINT('Ctrl Pts',(6.61842526171017,3.78336613625867,3.52796186343163));
#124850=CARTESIAN_POINT('',(6.11646929938807,3.91326598466575,3.89246750905316));
#124851=CARTESIAN_POINT('Ctrl Pts',(6.11646929645235,3.91326598504639,3.8924675123496));
#124852=CARTESIAN_POINT('Ctrl Pts',(6.150251023,3.903042157,3.839384247));
#124853=CARTESIAN_POINT('Ctrl Pts',(6.183106334,3.892857143,3.785722661));
#124854=CARTESIAN_POINT('Ctrl Pts',(6.35615249632147,3.83921352755049,3.50309159634728));
#124855=CARTESIAN_POINT('Ctrl Pts',(6.50269266136571,3.78467661279065,3.20585217521131));
#124856=CARTESIAN_POINT('Ctrl Pts',(6.32858118267264,3.87435041327332,4.02480561173716));
#124857=CARTESIAN_POINT('Ctrl Pts',(6.30425405066542,3.87860220115422,4.0095694921564));
#124858=CARTESIAN_POINT('Ctrl Pts',(6.2799220475138,3.88292159129824,3.99435982204413));
#124859=CARTESIAN_POINT('Ctrl Pts',(6.25558519594437,3.88731207462102,3.97917865369964));
#124860=CARTESIAN_POINT('Ctrl Pts',(6.23238602679852,3.89149731464463,3.96470716418707));
#124861=CARTESIAN_POINT('Ctrl Pts',(6.20917895297857,3.89574618493737,3.95026656197386));
#124862=CARTESIAN_POINT('Ctrl Pts',(6.18599124343745,3.90006996191926,3.93581745729566));
#124863=CARTESIAN_POINT('Ctrl Pts',(6.162802891402,3.90439385870609,3.92136795225589));
#124864=CARTESIAN_POINT('Ctrl Pts',(6.13962846950894,3.90879118055024,3.90691785921443));
#124865=CARTESIAN_POINT('Ctrl Pts',(6.1164692969636,3.91326598372466,3.89246751191928));
#124866=CARTESIAN_POINT('Ctrl Pts',(5.65660290128854,3.78339966801643,4.53490959909924));
#124867=CARTESIAN_POINT('Ctrl Pts',(5.65905138414427,3.78403814050821,4.53184871704962));
#124868=CARTESIAN_POINT('Ctrl Pts',(5.661499867,3.784676613,4.528787835));
#124869=CARTESIAN_POINT('Ctrl Pts',(5.907649451,3.848863192,4.221072859));
#124870=CARTESIAN_POINT('Ctrl Pts',(6.118997541,3.914045302,3.888491878));
#124871=CARTESIAN_POINT('Ctrl Pts',(6.00236316514701,3.78339966801643,4.49685470076832));
#124872=CARTESIAN_POINT('Ctrl Pts',(6.00479087157351,3.78403814050821,4.49360690638416));
#124873=CARTESIAN_POINT('Ctrl Pts',(6.007218578,3.784676613,4.490359112));
#124874=CARTESIAN_POINT('Ctrl Pts',(6.251279477,3.848863192,4.163853564));
#124875=CARTESIAN_POINT('Ctrl Pts',(6.458514584,3.914045302,3.812819084));
#124876=CARTESIAN_POINT('Origin',(-0.172183610538041,4.01777098821472,-0.0889998762653649));
#124877=CARTESIAN_POINT('Ctrl Pts',(5.133372382,3.914032935,5.119666785));
#124878=CARTESIAN_POINT('Ctrl Pts',(5.179471231,3.90342418,5.073444527));
#124879=CARTESIAN_POINT('Ctrl Pts',(5.224730277,3.892857143,5.026399659));
#124880=CARTESIAN_POINT('Ctrl Pts',(5.454488042,3.839213527,4.787576161));
#124881=CARTESIAN_POINT('Ctrl Pts',(5.661499867,3.784676613,4.528787835));
#124882=CARTESIAN_POINT('Ctrl Pts',(5.66398702809829,3.78402137462934,4.52567860074675));
#124883=CARTESIAN_POINT('Ctrl Pts',(5.66647418919657,3.78336613625867,4.5225693664935));
#124884=CARTESIAN_POINT('Ctrl Pts',(5.13383736200001,3.914032935,5.46751442));
#124885=CARTESIAN_POINT('Ctrl Pts',(5.18306832399999,3.90342418,5.421287976));
#124886=CARTESIAN_POINT('Ctrl Pts',(5.2314589,3.892857143,5.374182522));
#124887=CARTESIAN_POINT('Ctrl Pts',(5.477113891,3.839213527,5.135051457));
#124888=CARTESIAN_POINT('Ctrl Pts',(5.69992859,3.784676613,4.874506546));
#124889=CARTESIAN_POINT('Ctrl Pts',(5.70260561606593,3.78402137462934,4.87137620710754));
#124890=CARTESIAN_POINT('Ctrl Pts',(5.70528264213184,3.78336613625867,4.86824586821509));
#124891=CARTESIAN_POINT('',(5.13670419225033,3.91326598486893,5.11632387946452));
#124892=CARTESIAN_POINT('Ctrl Pts',(5.13670418872993,3.91326598504639,5.11632388223311));
#124893=CARTESIAN_POINT('Ctrl Pts',(5.18110745,3.903042157,5.071743746));
#124894=CARTESIAN_POINT('Ctrl Pts',(5.224730277,3.892857143,5.026399659));
#124895=CARTESIAN_POINT('Ctrl Pts',(5.45448804055648,3.83921352755582,4.78757616143772));
#124896=CARTESIAN_POINT('Ctrl Pts',(5.66149986570685,3.7846766119556,4.52878783597895));
#124897=CARTESIAN_POINT('Ctrl Pts',(5.31540823715458,3.87435041321081,5.2911657759504));
#124898=CARTESIAN_POINT('Ctrl Pts',(5.29492517538631,3.87860220111821,5.27105625408227));
#124899=CARTESIAN_POINT('Ctrl Pts',(5.2744316704039,3.88292159127204,5.25097151622122));
#124900=CARTESIAN_POINT('Ctrl Pts',(5.2539273033291,3.88731207460207,5.23091357150108));
#124901=CARTESIAN_POINT('Ctrl Pts',(5.23438146031949,3.89149731463373,5.21179328180058));
#124902=CARTESIAN_POINT('Ctrl Pts',(5.2148212576476,3.89574618494381,5.19270145794553));
#124903=CARTESIAN_POINT('Ctrl Pts',(5.19528179427941,3.90006996193226,5.17360549318181));
#124904=CARTESIAN_POINT('Ctrl Pts',(5.17574178950408,3.90439385872563,5.15450899929958));
#124905=CARTESIAN_POINT('Ctrl Pts',(5.15621551555658,3.90879118056291,5.13541492577162));
#124906=CARTESIAN_POINT('Ctrl Pts',(5.13670419026838,3.91326598375979,5.11632388192909));
#124907=CARTESIAN_POINT('Ctrl Pts',(4.54948315630955,3.78339966801642,5.64488834877326));
#124908=CARTESIAN_POINT('Ctrl Pts',(4.55253239415478,3.78403814050821,5.64242537988663));
#124909=CARTESIAN_POINT('Ctrl Pts',(4.555581632,3.784676613,5.639962411));
#124910=CARTESIAN_POINT('Ctrl Pts',(4.862125999,3.848863192,5.392356525));
#124911=CARTESIAN_POINT('Ctrl Pts',(5.140027969,3.914045302,5.112984694));
#124912=CARTESIAN_POINT('Ctrl Pts',(4.89534041542821,3.78339966801642,5.68205138827747));
#124913=CARTESIAN_POINT('Ctrl Pts',(4.8984095432141,3.78403814050821,5.67940141063874));
#124914=CARTESIAN_POINT('Ctrl Pts',(4.901478671,3.784676613,5.676751433));
#124915=CARTESIAN_POINT('Ctrl Pts',(5.210022603,3.848863192,5.410345282));
#124916=CARTESIAN_POINT('Ctrl Pts',(5.487874705,3.914045302,5.11206721600001));
#124917=CARTESIAN_POINT('Origin',(-0.149025773014475,4.01777117436562,-0.123933495488204));
#124918=CARTESIAN_POINT('Ctrl Pts',(3.912779966,3.914032935,6.103495141));
#124919=CARTESIAN_POINT('Ctrl Pts',(3.967737468,3.90342418,6.068263424));
#124920=CARTESIAN_POINT('Ctrl Pts',(4.022051639,3.892857143,6.032047796));
#124921=CARTESIAN_POINT('Ctrl Pts',(4.297777787,3.839213527,5.848198986));
#124922=CARTESIAN_POINT('Ctrl Pts',(4.555581632,3.784676613,5.639962411));
#124923=CARTESIAN_POINT('Ctrl Pts',(4.55867903812293,3.78402137462933,5.63746053503914));
#124924=CARTESIAN_POINT('Ctrl Pts',(4.56177644424584,3.78336613625867,5.63495865907829));
#124925=CARTESIAN_POINT('Ctrl Pts',(3.838457116,3.914032935,6.44331024900001));
#124926=CARTESIAN_POINT('Ctrl Pts',(3.896474404,3.90342418,6.408747755));
#124927=CARTESIAN_POINT('Ctrl Pts',(3.953859916,3.892857143,6.373146144));
#124928=CARTESIAN_POINT('Ctrl Pts',(4.24517774,3.839213527,6.192414392));
#124929=CARTESIAN_POINT('Ctrl Pts',(4.518792609,3.784676613,5.98585945));
#124930=CARTESIAN_POINT('Ctrl Pts',(4.52207997800942,3.78402137462933,5.9833777781612));
#124931=CARTESIAN_POINT('Ctrl Pts',(4.52536734701884,3.78336613625867,5.9808961063224));
#124932=CARTESIAN_POINT('',(3.91675250608448,3.91326598469296,6.10094663184978));
#124933=CARTESIAN_POINT('Ctrl Pts',(3.91675250213917,3.91326598504639,6.10094663341301));
#124934=CARTESIAN_POINT('Ctrl Pts',(3.969701051,3.903042157,6.06695414500001));
#124935=CARTESIAN_POINT('Ctrl Pts',(4.022051639,3.892857143,6.032047796));
#124936=CARTESIAN_POINT('Ctrl Pts',(4.29777778699874,3.83921352751727,5.84819898632377));
#124937=CARTESIAN_POINT('Ctrl Pts',(4.55558163184143,3.78467661273374,5.63996241260665));
#124938=CARTESIAN_POINT('Ctrl Pts',(4.05369271047263,3.87435041321389,6.31011690926935));
#124939=CARTESIAN_POINT('Ctrl Pts',(4.03801148411031,3.87860220114895,6.28607428389986));
#124940=CARTESIAN_POINT('Ctrl Pts',(4.02231473078001,3.88292159129884,6.2620536182469));
#124941=CARTESIAN_POINT('Ctrl Pts',(4.0066016095796,3.88731207462764,6.23805678428031));
#124942=CARTESIAN_POINT('Ctrl Pts',(3.99162303459158,3.89149731465319,6.21518173784877));
#124943=CARTESIAN_POINT('Ctrl Pts',(3.97662431624531,3.89574618493986,6.19233140489362));
#124944=CARTESIAN_POINT('Ctrl Pts',(3.96164674257626,3.90006996191702,6.16948148613298));
#124945=CARTESIAN_POINT('Ctrl Pts',(3.94666875390264,3.90439385869913,6.14663093423767));
#124946=CARTESIAN_POINT('Ctrl Pts',(3.93170365482692,3.90879118054072,6.12378569777082));
#124947=CARTESIAN_POINT('Ctrl Pts',(3.91675250287682,3.91326598379626,6.10094663327454));
#124948=CARTESIAN_POINT('Ctrl Pts',(3.22963463525794,3.78339966801642,6.49091839309238));
#124949=CARTESIAN_POINT('Ctrl Pts',(3.23314204912897,3.78403814050821,6.48916850304618));
#124950=CARTESIAN_POINT('Ctrl Pts',(3.236649463,3.784676613,6.487418613));
#124951=CARTESIAN_POINT('Ctrl Pts',(3.58925494,3.848863192,6.311499592));
#124952=CARTESIAN_POINT('Ctrl Pts',(3.9207164,3.914045302,6.098400028));
#124953=CARTESIAN_POINT('Ctrl Pts',(3.55941698871103,3.78339966801642,6.6015616687789));
#124954=CARTESIAN_POINT('Ctrl Pts',(3.56298402885552,3.78403814050821,6.59963341788945));
#124955=CARTESIAN_POINT('Ctrl Pts',(3.566551069,3.784676613,6.59770516700001));
#124956=CARTESIAN_POINT('Ctrl Pts',(3.925150863,3.848863192,6.403855268));
#124957=CARTESIAN_POINT('Ctrl Pts',(4.260627904,3.914045302,6.172280767));
#124958=CARTESIAN_POINT('Origin',(-0.118899507874863,4.0177710088603,-0.153072028990134));
#124959=CARTESIAN_POINT('Ctrl Pts',(2.509230308,3.914032935,6.801930848));
#124960=CARTESIAN_POINT('Ctrl Pts',(2.570476711,3.90342418,6.779337068));
#124961=CARTESIAN_POINT('Ctrl Pts',(2.631306337,3.892857143,6.755644082));
#124962=CARTESIAN_POINT('Ctrl Pts',(2.940108221,3.839213527,6.635366527));
#124963=CARTESIAN_POINT('Ctrl Pts',(3.236649463,3.784676613,6.487418613));
#124964=CARTESIAN_POINT('Ctrl Pts',(3.24021228285891,3.78402137462934,6.48564108026112));
#124965=CARTESIAN_POINT('Ctrl Pts',(3.24377510271782,3.78336613625867,6.48386354752224));
#124966=CARTESIAN_POINT('Ctrl Pts',(2.363594881,3.914032935,7.117824052));
#124967=CARTESIAN_POINT('Ctrl Pts',(2.427685672,3.90342418,7.096541612));
#124968=CARTESIAN_POINT('Ctrl Pts',(2.491382836,3.892857143,7.074108535));
#124969=CARTESIAN_POINT('Ctrl Pts',(2.814741796,3.839213527,6.960226912));
#124970=CARTESIAN_POINT('Ctrl Pts',(3.126362908,3.784676613,6.81732021899999));
#124971=CARTESIAN_POINT('Ctrl Pts',(3.13010690623377,3.78402137462934,6.81560325443765));
#124972=CARTESIAN_POINT('Ctrl Pts',(3.13385090446755,3.78336613625867,6.81388628987528));
#124973=CARTESIAN_POINT('',(2.51365782730426,3.91326598478301,6.80029589995261));
#124974=CARTESIAN_POINT('Ctrl Pts',(2.51365782739205,3.91326598534454,6.80029589992694));
#124975=CARTESIAN_POINT('Ctrl Pts',(2.55303868075648,3.90644394844332,6.78573918197759));
#124976=CARTESIAN_POINT('Ctrl Pts',(2.59225752687014,3.89964051893982,6.77085349511628));
#124977=CARTESIAN_POINT('Ctrl Pts',(2.63130633659125,3.89285714306086,6.75564408226938));
#124978=CARTESIAN_POINT('Ctrl Pts',(2.76889106306463,3.86895656917362,6.70205517870409));
#124979=CARTESIAN_POINT('Ctrl Pts',(2.90531186822816,3.84480673693962,6.64407447046975));
#124980=CARTESIAN_POINT('Ctrl Pts',(3.0401567232433,3.82047238378624,6.58178905128594));
#124981=CARTESIAN_POINT('Ctrl Pts',(3.10604627856664,3.80858183217285,6.55135438195659));
#124982=CARTESIAN_POINT('Ctrl Pts',(3.17155963440329,3.79664728639182,6.51989269544317));
#124983=CARTESIAN_POINT('Ctrl Pts',(3.23664946230039,3.78467661300963,6.48741861496226));
#124984=CARTESIAN_POINT('Ctrl Pts',(2.60243101783683,3.87435041322623,7.03401398873241));
#124985=CARTESIAN_POINT('Ctrl Pts',(2.59228486354879,3.87860220112027,7.00716246659475));
#124986=CARTESIAN_POINT('Ctrl Pts',(2.58211882471485,3.8829215912644,6.98032905281386));
#124987=CARTESIAN_POINT('Ctrl Pts',(2.57193167755894,3.88731207458757,6.95351539495929));
#124988=CARTESIAN_POINT('Ctrl Pts',(2.56222075215247,3.89149731461572,6.92795520354208));
#124989=CARTESIAN_POINT('Ctrl Pts',(2.55248484170893,3.89574618491529,6.90241481758498));
#124990=CARTESIAN_POINT('Ctrl Pts',(2.54276949248602,3.90006996190096,6.87687938164382));
#124991=CARTESIAN_POINT('Ctrl Pts',(2.5330538740663,3.90439385869159,6.85134323815647));
#124992=CARTESIAN_POINT('Ctrl Pts',(2.52334970118558,3.90879118054061,6.82581505672652));
#124993=CARTESIAN_POINT('Ctrl Pts',(2.5136578228534,3.91326598381907,6.80029590129335));
#124994=CARTESIAN_POINT('Ctrl Pts',(1.75877198777081,3.78339966801642,7.03344030656226));
#124995=CARTESIAN_POINT('Ctrl Pts',(1.76257357488541,3.78403814050821,7.03248531828113));
#124996=CARTESIAN_POINT('Ctrl Pts',(1.766375162,3.784676613,7.03153033));
#124997=CARTESIAN_POINT('Ctrl Pts',(2.148554308,3.848863192,6.93552395300001));
#124998=CARTESIAN_POINT('Ctrl Pts',(2.518076491,3.914045302,6.798660955));
#124999=CARTESIAN_POINT('Ctrl Pts',(2.05705917966293,3.78339966801642,7.21239026252005));
#125000=CARTESIAN_POINT('Ctrl Pts',(2.06095734133146,3.78403814050821,7.21127390126003));
#125001=CARTESIAN_POINT('Ctrl Pts',(2.064855503,3.784676613,7.21015754));
#125002=CARTESIAN_POINT('Ctrl Pts',(2.456743431,3.848863192,7.0979281));
#125003=CARTESIAN_POINT('Ctrl Pts',(2.834158878,3.914045302,6.94388532800001));
#125004=CARTESIAN_POINT('Origin',(-0.0832137526056376,4.017770990989,-0.175053254770167));
#125005=CARTESIAN_POINT('Ctrl Pts',(0.988351829,3.914032935,7.182315829));
#125006=CARTESIAN_POINT('Ctrl Pts',(1.053023321,3.90342418,7.173416445));
#125007=CARTESIAN_POINT('Ctrl Pts',(1.117524075,3.892857143,7.163353959));
#125008=CARTESIAN_POINT('Ctrl Pts',(1.444962461,3.839213527,7.112271703));
#125009=CARTESIAN_POINT('Ctrl Pts',(1.766375162,3.784676613,7.03153033));
#125010=CARTESIAN_POINT('Ctrl Pts',(1.77023680210883,3.78402137462933,7.03056025593805));
#125011=CARTESIAN_POINT('Ctrl Pts',(1.77409844221766,3.78336613625867,7.02959018187611));
#125012=CARTESIAN_POINT('Ctrl Pts',(0.778213576,3.914032935,7.45951631300001));
#125013=CARTESIAN_POINT('Ctrl Pts',(0.845381055,3.90342418,7.45250907));
#125014=CARTESIAN_POINT('Ctrl Pts',(0.912411464,3.892857143,7.444293474));
#125015=CARTESIAN_POINT('Ctrl Pts',(1.252691653,3.839213527,7.402586957));
#125016=CARTESIAN_POINT('Ctrl Pts',(1.587747952,3.784676613,7.330010671));
#125017=CARTESIAN_POINT('Ctrl Pts',(1.59177351427215,3.78402137462933,7.32913869706712));
#125018=CARTESIAN_POINT('Ctrl Pts',(1.59579907654429,3.78336613625867,7.32826672313425));
#125019=CARTESIAN_POINT('',(0.993027300813708,3.91326598477827,7.18167089038567));
#125020=CARTESIAN_POINT('Ctrl Pts',(0.993027300977299,3.91326598535293,
7.18167089088704));
#125021=CARTESIAN_POINT('Ctrl Pts',(1.03461671607111,3.9064439485324,7.17592022021272));
#125022=CARTESIAN_POINT('Ctrl Pts',(1.07611863008281,3.89964051902724,7.16981344487701));
#125023=CARTESIAN_POINT('Ctrl Pts',(1.11752407430451,3.89285714307317,7.16335395941058));
#125024=CARTESIAN_POINT('Ctrl Pts',(1.26341255565324,3.86895650694317,7.14059452521847));
#125025=CARTESIAN_POINT('Ctrl Pts',(1.40910843260399,3.84480661167109,7.1132957314019));
#125026=CARTESIAN_POINT('Ctrl Pts',(1.5541905854932,3.82047219473368,7.0814540622888));
#125027=CARTESIAN_POINT('Ctrl Pts',(1.62508185668359,3.80858170568305,7.06589531605229));
#125028=CARTESIAN_POINT('Ctrl Pts',(1.69582650333231,3.79664722298046,7.04925270345853));
#125029=CARTESIAN_POINT('Ctrl Pts',(1.76637516097775,3.78467661301146,7.03153033161224));
#125030=CARTESIAN_POINT('Ctrl Pts',(1.02948254308918,3.87435041323043,7.42900839219754));
#125031=CARTESIAN_POINT('Ctrl Pts',(1.02534588378698,3.87860220113284,7.40060352041932));
#125032=CARTESIAN_POINT('Ctrl Pts',(1.0211859121115,3.88292159128409,7.3722120590852));
#125033=CARTESIAN_POINT('Ctrl Pts',(1.01700107867272,3.88731207461403,7.34383535412217));
#125034=CARTESIAN_POINT('Ctrl Pts',(1.01301187494508,3.89149731465338,7.31678518381723));
#125035=CARTESIAN_POINT('Ctrl Pts',(1.00899401265604,3.89574618495283,7.28974898488849));
#125036=CARTESIAN_POINT('Ctrl Pts',(1.00499516686957,3.90006996195267,7.26272204028935));
#125037=CARTESIAN_POINT('Ctrl Pts',(1.00099621028148,3.90439385875746,7.23569434681681));
#125038=CARTESIAN_POINT('Ctrl Pts',(0.99700672008525,3.90879118062775,7.208676889702));
#125039=CARTESIAN_POINT('Ctrl Pts',(0.993027296840861,3.91326598383751,
7.18167089110787));
#125040=CARTESIAN_POINT('Ctrl Pts',(0.205671117258216,3.78339966801642,
7.24708636966053));
#125041=CARTESIAN_POINT('Ctrl Pts',(0.209589119629108,3.78403814050821,
7.24697093733027));
#125042=CARTESIAN_POINT('Ctrl Pts',(0.213507122,3.784676613,7.246855505));
#125043=CARTESIAN_POINT('Ctrl Pts',(0.607389665,3.848863192,7.235250923));
#125044=CARTESIAN_POINT('Ctrl Pts',(0.997694124,3.914045302,7.181024052));
#125045=CARTESIAN_POINT('Ctrl Pts',(0.458515569029854,3.78339966801642,
7.48597550365515));
#125046=CARTESIAN_POINT('Ctrl Pts',(0.462562578514927,3.78403814050821,
7.48572323182757));
#125047=CARTESIAN_POINT('Ctrl Pts',(0.466609588,3.784676613,7.48547096));
#125048=CARTESIAN_POINT('Ctrl Pts',(0.873461406,3.848863192,7.460109702));
#125049=CARTESIAN_POINT('Ctrl Pts',(1.275167733,3.914045302,7.39080153));
#125050=CARTESIAN_POINT('Origin',(-0.0436369827697361,4.01777097706205,
-0.18884908381595));
#125051=CARTESIAN_POINT('Ctrl Pts',(-0.578740883,3.914032935,7.226863704));
#125052=CARTESIAN_POINT('Ctrl Pts',(-0.51366827,3.90342418,7.232074841));
#125053=CARTESIAN_POINT('Ctrl Pts',(-0.448512371,3.892857143,7.236113367));
#125054=CARTESIAN_POINT('Ctrl Pts',(-0.117748137,3.839213527,7.25661495900001));
#125055=CARTESIAN_POINT('Ctrl Pts',(0.213507122,3.784676613,7.246855505));
#125056=CARTESIAN_POINT('Ctrl Pts',(0.217487016355248,3.78402137462933,
7.24673824921362));
#125057=CARTESIAN_POINT('Ctrl Pts',(0.221466910710496,3.78336613625867,
7.24662099342725));
#125058=CARTESIAN_POINT('Ctrl Pts',(-0.84355613,3.914032935,7.452409882));
#125059=CARTESIAN_POINT('Ctrl Pts',(-0.776452639,3.90342418,7.460005487));
#125060=CARTESIAN_POINT('Ctrl Pts',(-0.709223254,3.892857143,7.466391523));
#125061=CARTESIAN_POINT('Ctrl Pts',(-0.367932958,3.839213527,7.498810264));
#125062=CARTESIAN_POINT('Ctrl Pts',(-0.025108333,3.784676613,7.499957971));
#125063=CARTESIAN_POINT('Ctrl Pts',(-0.0209894375174155,3.78402137462933,
7.49997176022292));
#125064=CARTESIAN_POINT('Ctrl Pts',(-0.016870542034831,3.78336613625867,
7.49998554944585));
#125065=CARTESIAN_POINT('Ctrl Pts',(-0.574036075078507,3.91326598479031,
7.22723893284684));
#125066=CARTESIAN_POINT('Ctrl Pts',(-0.443380136338622,3.89196922700598,
7.23761650894715));
#125067=CARTESIAN_POINT('Ctrl Pts',(-0.312506527981107,3.87079705839004,
7.24444860561573));
#125068=CARTESIAN_POINT('Ctrl Pts',(-0.115671644510548,3.8386788420296,
7.24937548238318));
#125069=CARTESIAN_POINT('Ctrl Pts',(-0.0499136823355695,3.82792484954096,
7.2501263677632));
#125070=CARTESIAN_POINT('Ctrl Pts',(0.0487767784342727,3.81174904529917,
7.24991072932808));
#125071=CARTESIAN_POINT('Ctrl Pts',(0.0817105542309791,3.80634502485406,
7.24961433627786));
#125072=CARTESIAN_POINT('Ctrl Pts',(0.131118289538351,3.79822878963818,
7.24883298155762));
#125073=CARTESIAN_POINT('Ctrl Pts',(0.147595175806614,3.7955206131177,7.2485162103515));
#125074=CARTESIAN_POINT('Ctrl Pts',(0.172311478230664,3.79145592379503,
7.24795672663783));
#125075=CARTESIAN_POINT('Ctrl Pts',(0.180551955589269,3.79010036844976,
7.24775613187476));
#125076=CARTESIAN_POINT('Ctrl Pts',(0.196655767919899,3.78745055936495,
7.24733664196481));
#125077=CARTESIAN_POINT('Ctrl Pts',(0.200619346131265,3.78679841925717,
7.24723520591059));
#125078=CARTESIAN_POINT('Ctrl Pts',(0.213507120912194,3.78467661303892,
7.24685550591003));
#125079=CARTESIAN_POINT('Ctrl Pts',(0.178767433842035,1.96978752941321,
7.24784744327216));
#125080=CARTESIAN_POINT('Ctrl Pts',(0.192458160921018,1.97205380720657,
7.24745799913609));
#125081=CARTESIAN_POINT('Ctrl Pts',(0.206148888,1.974320085,7.247068555));
#125082=CARTESIAN_POINT('Ctrl Pts',(0.603261147,2.040055578,7.23577236600001));
#125083=CARTESIAN_POINT('Ctrl Pts',(0.99676151,2.104802836,7.181153563));
#125084=CARTESIAN_POINT('Ctrl Pts',(0.431246454094205,1.96978752941321,
7.48817152332989));
#125085=CARTESIAN_POINT('Ctrl Pts',(0.445389378432169,1.97205380720657,
7.48730340247219));
#125086=CARTESIAN_POINT('Ctrl Pts',(0.459532302770134,1.974320085,7.48643528161457));
#125087=CARTESIAN_POINT('Ctrl Pts',(0.869760963404042,2.040055578,7.46125462956701));
#125088=CARTESIAN_POINT('Ctrl Pts',(1.27478211834185,2.104802836,7.39140133707004));
#125089=CARTESIAN_POINT('',(0.459008938997241,1.97432008542257,7.48594087559712));
#125090=CARTESIAN_POINT('',(1.02461500783359,2.06488542555259,7.42968127597571));
#125091=CARTESIAN_POINT('Origin',(0.0043556889311553,1.87505116433469,-0.188905834260398));
#125092=CARTESIAN_POINT('Ctrl Pts',(0.992091959997776,2.10403448596886,
7.18180016033055));
#125093=CARTESIAN_POINT('Ctrl Pts',(0.997458679234665,2.09719849231725,
7.22306246022236));
#125094=CARTESIAN_POINT('Ctrl Pts',(1.00285674280479,2.09052285934313,7.26437149725571));
#125095=CARTESIAN_POINT('Ctrl Pts',(1.01369768214475,2.07748305174204,7.34698583760116));
#125096=CARTESIAN_POINT('Ctrl Pts',(1.01914634417815,2.07111192519156,7.38833520691057));
#125097=CARTESIAN_POINT('Ctrl Pts',(1.02461500444344,2.06488542585939,7.42968127647032));
#125098=CARTESIAN_POINT('',(0.332578908769879,1.97432008626233,7.366504715349));
#125099=CARTESIAN_POINT('Origin',(-2.01526078810743E-13,2.06597317200011,
-1.06425285251177E-12));
#125100=CARTESIAN_POINT('',(1.02305817476535,1.88359401259106,7.42989582457252));
#125101=CARTESIAN_POINT('Origin',(-0.00472924854615489,2.01784565612039,
-0.191489621333766));
#125102=CARTESIAN_POINT('',(1.5803045683921,1.97432008362733,7.33161902003294));
#125103=CARTESIAN_POINT('Origin',(-0.024888475172779,1.87500215864661,-0.190931453900025));
#125104=CARTESIAN_POINT('Origin',(-0.0338263713808067,2.01785750447293,
-0.190074353583174));
#125105=CARTESIAN_POINT('Ctrl Pts',(0.987449852,2.104810499,7.182439891));
#125106=CARTESIAN_POINT('Ctrl Pts',(1.377390219,2.039629277,7.128830454));
#125107=CARTESIAN_POINT('Ctrl Pts',(1.759234759,1.974320085,7.033320202));
#125108=CARTESIAN_POINT('Ctrl Pts',(0.77727679,2.104810499,7.459613984));
#125109=CARTESIAN_POINT('Ctrl Pts',(1.182265159,2.039629277,7.41741501));
#125110=CARTESIAN_POINT('Ctrl Pts',(1.580304579,1.974320085,7.331619019));
#125111=CARTESIAN_POINT('',(1.66976965661296,1.97432008293108,7.18246961337972));
#125112=CARTESIAN_POINT('Ctrl Pts',(1.73266090573731,1.96978752936799,7.03996708358226));
#125113=CARTESIAN_POINT('Ctrl Pts',(1.74594783236865,1.97205380718396,7.0366436427912));
#125114=CARTESIAN_POINT('Ctrl Pts',(1.759234759,1.974320085,7.033320202));
#125115=CARTESIAN_POINT('Ctrl Pts',(2.144634407,2.040055578,6.936920715));
#125116=CARTESIAN_POINT('Ctrl Pts',(2.517193523,2.104802836,6.798987922));
#125117=CARTESIAN_POINT('Ctrl Pts',(2.03089967991489,1.96978752936799,7.22039699500751));
#125118=CARTESIAN_POINT('Ctrl Pts',(2.04452533034233,1.97205380718396,7.21650885961273));
#125119=CARTESIAN_POINT('Ctrl Pts',(2.05815098076969,1.974320085,7.21262072421792));
#125120=CARTESIAN_POINT('Ctrl Pts',(2.45337562708394,2.040055578,7.09984174574467));
#125121=CARTESIAN_POINT('Ctrl Pts',(2.83391121931717,2.104802836,6.94455400749346));
#125122=CARTESIAN_POINT('',(2.05753356652339,1.97432008541403,7.21225038508608));
#125123=CARTESIAN_POINT('',(2.59782193263601,2.06488542558443,7.03571751704224));
#125124=CARTESIAN_POINT('Origin',(-0.0363552949333781,1.87505115563869,
-0.185425571201403));
#125125=CARTESIAN_POINT('Ctrl Pts',(2.51277214423581,2.10403448587199,6.80062321814657));
#125126=CARTESIAN_POINT('Ctrl Pts',(2.52688364672442,2.09719845370066,6.83976736318672));
#125127=CARTESIAN_POINT('Ctrl Pts',(2.54103581863248,2.09052278112002,6.87895044282818));
#125128=CARTESIAN_POINT('Ctrl Pts',(2.56938277355433,2.07748305176976,6.95730235436121));
#125129=CARTESIAN_POINT('Ctrl Pts',(2.58359294085558,2.07111192522839,6.99651369714983));
#125130=CARTESIAN_POINT('Ctrl Pts',(2.59782192948137,2.06488542591375,7.03571751823952));
#125131=CARTESIAN_POINT('',(1.90838416002563,1.97432008626233,7.12278529450258));
#125132=CARTESIAN_POINT('Origin',(4.74446870679657E-13,2.06597317200044,
1.06858966120171E-12));
#125133=CARTESIAN_POINT('',(2.59634761954241,1.88359401255043,7.03626172285193));
#125134=CARTESIAN_POINT('Origin',(-0.045783351768986,2.01784567000082,-0.185996229389547));
#125135=CARTESIAN_POINT('',(3.11943929387699,1.97432008362731,6.82049107327776));
#125136=CARTESIAN_POINT('Origin',(-0.0653511309221899,1.87500216096182,
-0.18111710065302));
#125137=CARTESIAN_POINT('Origin',(-0.0738959797718136,2.017857509494,-0.178359071339537));
#125138=CARTESIAN_POINT('Ctrl Pts',(2.508376089,2.104810499,6.802245908));
#125139=CARTESIAN_POINT('Ctrl Pts',(2.877675422,2.039629277,6.66606417800001));
#125140=CARTESIAN_POINT('Ctrl Pts',(3.230060768,1.974320085,6.490701613));
#125141=CARTESIAN_POINT('Ctrl Pts',(2.362700993,2.104810499,7.118120821));
#125142=CARTESIAN_POINT('Ctrl Pts',(2.749149426,2.039629277,6.989847907));
#125143=CARTESIAN_POINT('Ctrl Pts',(3.119439304,1.974320085,6.82049107000001));
#125144=CARTESIAN_POINT('',(3.17475002452162,1.97432008293108,6.65559634697524));
#125145=CARTESIAN_POINT('Ctrl Pts',(3.20553707944452,1.9697875293269,6.50290568719135));
#125146=CARTESIAN_POINT('Ctrl Pts',(3.21779892372226,1.97205380716342,6.49680365009561));
#125147=CARTESIAN_POINT('Ctrl Pts',(3.230060768,1.974320085,6.49070161300001));
#125148=CARTESIAN_POINT('Ctrl Pts',(3.585726947,2.040055578,6.313706361));
#125149=CARTESIAN_POINT('Ctrl Pts',(3.919924364,2.104802836,6.098909163));
#125150=CARTESIAN_POINT('Ctrl Pts',(3.5355902941514,1.9697875293269,6.61500472717748));
#125151=CARTESIAN_POINT('Ctrl Pts',(3.54806155038054,1.97205380716342,6.6082783821254));
#125152=CARTESIAN_POINT('Ctrl Pts',(3.56053280660969,1.974320085,6.60155203707342));
#125153=CARTESIAN_POINT('Ctrl Pts',(3.92227317370945,2.040055578,6.4064481530988));
#125154=CARTESIAN_POINT('Ctrl Pts',(4.26052978288015,2.104802836,6.17298705222455));
#125155=CARTESIAN_POINT('',(3.55985021522416,1.97432008541403,6.60132308208483));
#125156=CARTESIAN_POINT('',(4.04955759140998,2.06488542558083,6.31277142726971));
#125157=CARTESIAN_POINT('Origin',(-0.0753663103962776,1.87505112929091,
-0.17327508517603));
#125158=CARTESIAN_POINT('Ctrl Pts',(3.91595789455973,2.10403448589348,6.10145669238763));
#125159=CARTESIAN_POINT('Ctrl Pts',(3.93815431207447,2.09719845373132,6.13665211315745));
#125160=CARTESIAN_POINT('Ctrl Pts',(3.96039881815478,2.09052278109977,6.17187681586637));
#125161=CARTESIAN_POINT('Ctrl Pts',(4.00492638198642,2.07748305174562,6.24230314600544));
#125162=CARTESIAN_POINT('Ctrl Pts',(4.02723360302552,2.07111192522287,6.27754298342747));
#125163=CARTESIAN_POINT('Ctrl Pts',(4.04955758851027,2.06488542589252,6.31277142916232));
#125164=CARTESIAN_POINT('',(3.39495548913088,1.97432008626233,6.54601234906254));
#125165=CARTESIAN_POINT('Origin',(-5.68772459685896E-13,2.06597317199978,
-8.68229099726392E-13));
#125166=CARTESIAN_POINT('',(4.04823473517134,1.88359401261641,6.31361984319499));
#125167=CARTESIAN_POINT('Origin',(-0.0846965919862108,2.01784564054595,
-0.171805572819673));
#125168=CARTESIAN_POINT('',(4.51271250479587,1.97432008362732,5.99044454341028));
#125169=CARTESIAN_POINT('Origin',(-0.102758079614512,1.87500221011058,-0.162834088004034));
#125170=CARTESIAN_POINT('Origin',(-0.110510209683147,2.0178575028769,-0.158303586201035));
#125171=CARTESIAN_POINT('Ctrl Pts',(3.912013447,2.104810499,6.103986467));
#125172=CARTESIAN_POINT('Ctrl Pts',(4.243403721,2.039629277,5.89160015));
#125173=CARTESIAN_POINT('Ctrl Pts',(4.549852726,1.974320085,5.644585031));
#125174=CARTESIAN_POINT('Ctrl Pts',(3.837647923,2.104810499,6.443792239));
#125175=CARTESIAN_POINT('Ctrl Pts',(4.187486522,2.039629277,6.235443285));
#125176=CARTESIAN_POINT('Ctrl Pts',(4.512712514,1.974320085,5.990444538));
#125177=CARTESIAN_POINT('',(4.53128260996699,1.97432008293108,5.81751479231475));
#125178=CARTESIAN_POINT('Ctrl Pts',(4.52852590254689,1.9697875292444,5.66177564912586));
#125179=CARTESIAN_POINT('Ctrl Pts',(4.53918931427345,1.97205380712217,5.653180340063));
#125180=CARTESIAN_POINT('Ctrl Pts',(4.549852726,1.974320085,5.644585031));
#125181=CARTESIAN_POINT('Ctrl Pts',(4.859154879,2.040055578,5.395270115));
#125182=CARTESIAN_POINT('Ctrl Pts',(5.139363898,2.104802836,5.11365219));
#125183=CARTESIAN_POINT('Ctrl Pts',(4.87496063661739,1.9697875292444,5.70030219096034));
#125184=CARTESIAN_POINT('Ctrl Pts',(4.8856943566356,1.97205380712217,5.69105215250749));
#125185=CARTESIAN_POINT('Ctrl Pts',(4.89642807665381,1.974320085,5.68180211405464));
#125186=CARTESIAN_POINT('Ctrl Pts',(5.2077695869007,2.040055578,5.41349616449857));
#125187=CARTESIAN_POINT('Ctrl Pts',(5.48793070796859,2.104802836,5.1127780815485));
#125188=CARTESIAN_POINT('',(4.8957122252653,1.97432008541403,5.68172524887134));
#125189=CARTESIAN_POINT('',(5.3119404380159,2.06488542554777,5.29464716104061));
#125190=CARTESIAN_POINT('Origin',(-0.110853200776553,1.87505113429841,-0.153022349890662));
#125191=CARTESIAN_POINT('Ctrl Pts',(5.13603780673366,2.10403448590885,5.11699283318292));
#125192=CARTESIAN_POINT('Ctrl Pts',(5.16528125943058,2.09719845369597,5.14659383102125));
#125193=CARTESIAN_POINT('Ctrl Pts',(5.19457797081671,2.09052278110507,5.17621308819953));
#125194=CARTESIAN_POINT('Ctrl Pts',(5.25320408410194,2.07748305170339,5.23542077989614));
#125195=CARTESIAN_POINT('Ctrl Pts',(5.28256529802559,2.07111192517364,5.26504133632377));
#125196=CARTESIAN_POINT('Ctrl Pts',(5.31194043558567,2.06488542584355,5.2946471635141));
#125197=CARTESIAN_POINT('',(4.72278247355731,1.97432008626233,5.6631551419559));
#125198=CARTESIAN_POINT('Origin',(5.09575021068187E-13,2.06597317199967,
3.72965547335014E-13));
#125199=CARTESIAN_POINT('',(5.31083089400445,1.88359401261276,5.29576011612746));
#125200=CARTESIAN_POINT('Origin',(-0.119649861527216,2.01784567590668,-0.149581916488767));
#125201=CARTESIAN_POINT('',(5.69497629518068,1.97432008362732,4.88029148524348));
#125202=CARTESIAN_POINT('Origin',(-0.135360135114847,1.8750021533394,-0.136937159342184));
#125203=CARTESIAN_POINT('Origin',(-0.141957160544719,2.01785751579753,-0.130846144117192));
#125204=CARTESIAN_POINT('Ctrl Pts',(5.132729405,2.104810499,5.120311403));
#125205=CARTESIAN_POINT('Ctrl Pts',(5.410715178,2.039629277,4.841651446));
#125206=CARTESIAN_POINT('Ctrl Pts',(5.656898626,1.974320085,4.534533927));
#125207=CARTESIAN_POINT('Ctrl Pts',(5.133150701,2.104810499,5.468159094));
#125208=CARTESIAN_POINT('Ctrl Pts',(5.430021402,2.039629277,5.189476265));
#125209=CARTESIAN_POINT('Ctrl Pts',(5.69497630300001,1.974320085,4.880291478));
#125210=CARTESIAN_POINT('',(5.6759374563815,1.97432008293108,4.70741271228884));
#125211=CARTESIAN_POINT('Ctrl Pts',(5.63976588660991,1.96978752926671,4.55590727463079));
#125212=CARTESIAN_POINT('Ctrl Pts',(5.64833225630496,1.97205380713332,4.5452206008154));
#125213=CARTESIAN_POINT('Ctrl Pts',(5.656898626,1.974320085,4.534533927));
#125214=CARTESIAN_POINT('Ctrl Pts',(5.90537413,2.040055578,4.224557034));
#125215=CARTESIAN_POINT('Ctrl Pts',(6.118492488,2.104802836,3.889286524));
#125216=CARTESIAN_POINT('Ctrl Pts',(5.98638323718693,1.96978752926671,4.51905985893111));
#125217=CARTESIAN_POINT('Ctrl Pts',(5.99487752390771,1.97205380713332,4.50771864877803));
#125218=CARTESIAN_POINT('Ctrl Pts',(6.00337181062865,1.974320085,4.49637743862502));
#125219=CARTESIAN_POINT('Ctrl Pts',(6.24975648105858,2.040055578,4.16741511163491));
#125220=CARTESIAN_POINT('Ctrl Pts',(6.45872209265358,2.104802836,3.81350129129357));
#125221=CARTESIAN_POINT('',(6.00265617455652,1.97432008542257,4.49645625496983));
#125222=CARTESIAN_POINT('',(6.32594285336114,2.06488542554472,4.02895107831226));
#125223=CARTESIAN_POINT('Origin',(-0.141156925378861,1.87505112236032,-0.125614706819361));
#125224=CARTESIAN_POINT('Ctrl Pts',(6.1159622987499,2.10403448590706,3.89326407603806));
#125225=CARTESIAN_POINT('Ctrl Pts',(6.15088539536528,2.09719845368304,3.91588654113296));
#125226=CARTESIAN_POINT('Ctrl Pts',(6.1858644305456,2.09052278111875,3.9385153895049));
#125227=CARTESIAN_POINT('Ctrl Pts',(6.25584780147992,2.07748305171283,3.98373595689417));
#125228=CARTESIAN_POINT('Ctrl Pts',(6.29089011066474,2.07111192517319,4.00635220811398));
#125229=CARTESIAN_POINT('Ctrl Pts',(6.32594285153372,2.06488542584587,4.02895108122973));
#125230=CARTESIAN_POINT('',(5.82977739726162,1.97432008626233,4.51549509461754));
#125231=CARTESIAN_POINT('Origin',(1.48318857196017E-13,2.06597317199933,
4.31512464649231E-14));
#125232=CARTESIAN_POINT('',(6.32509850206447,1.8835940125713,4.03027653313335));
#125233=CARTESIAN_POINT('Origin',(-0.149007952235226,2.01784564257634,-0.120363418775087));
#125234=CARTESIAN_POINT('',(6.61094932292352,1.97432008362731,3.54194142174975));
#125235=CARTESIAN_POINT('Origin',(-0.161633041338647,1.87500220953601,-0.104637270587731));
#125236=CARTESIAN_POINT('Origin',(-0.166766339652466,2.01785753493042,-0.0972704506244883));
#125237=CARTESIAN_POINT('Ctrl Pts',(6.11344464,2.104810499,3.897216268));
#125238=CARTESIAN_POINT('Ctrl Pts',(6.325027606,2.039629277,3.565312503));
#125239=CARTESIAN_POINT('Ctrl Pts',(6.499434234,1.974320085,3.212453056));
#125240=CARTESIAN_POINT('Ctrl Pts',(6.188633058,2.104810499,4.236840907));
#125241=CARTESIAN_POINT('Ctrl Pts',(6.41865451600001,2.039629277,3.900855103));
#125242=CARTESIAN_POINT('Ctrl Pts',(6.610949329,1.974320085,3.541941413));
#125243=CARTESIAN_POINT('',(6.55519177567562,1.97432008293108,3.37719724580523));
#125244=CARTESIAN_POINT('Ctrl Pts',(6.48729668650738,1.969787529284,3.23700973907726));
#125245=CARTESIAN_POINT('Ctrl Pts',(6.49336546025369,1.97205380714197,3.22473139753864));
#125246=CARTESIAN_POINT('Ctrl Pts',(6.499434234,1.974320085,3.212453056));
#125247=CARTESIAN_POINT('Ctrl Pts',(6.67546465,2.040055578,2.856308362));
#125248=CARTESIAN_POINT('Ctrl Pts',(6.81152717,2.104802836,2.483062143));
#125249=CARTESIAN_POINT('Ctrl Pts',(6.81788921130267,1.969787529284,3.12651131127987));
#125250=CARTESIAN_POINT('Ctrl Pts',(6.82374688136015,1.97205380714197,3.11360923180562));
#125251=CARTESIAN_POINT('Ctrl Pts',(6.82960455141775,1.974320085,3.10070715233132));
#125252=CARTESIAN_POINT('Ctrl Pts',(6.99951170896415,2.040055578,2.72647036050727));
#125253=CARTESIAN_POINT('Ctrl Pts',(7.12751081015265,2.104802836,2.33590941933527));
#125254=CARTESIAN_POINT('',(6.82892258744442,1.97432008541403,3.10093796957677));
#125255=CARTESIAN_POINT('',(7.04415121165797,2.06488542558693,2.57486572117495));
#125256=CARTESIAN_POINT('Origin',(-0.164860089069191,1.87505114807512,-0.0923332809654503));
#125257=CARTESIAN_POINT('Ctrl Pts',(6.80991119064009,2.10403448596401,2.48749061800447));
#125258=CARTESIAN_POINT('Ctrl Pts',(6.84888096585377,2.09719845377735,2.50207674884828));
#125259=CARTESIAN_POINT('Ctrl Pts',(6.88790674456954,2.09052278115302,2.51665708882608));
#125260=CARTESIAN_POINT('Ctrl Pts',(6.96597502846516,2.07748305177085,2.54577606833292));
#125261=CARTESIAN_POINT('Ctrl Pts',(7.00505989342596,2.07111192523824,2.56033050351797));
#125262=CARTESIAN_POINT('Ctrl Pts',(7.0441512104955,2.06488542590153,2.57486572443612));
#125263=CARTESIAN_POINT('',(6.66417840968749,1.97432008626233,3.15669551549313));
#125264=CARTESIAN_POINT('Origin',(-4.06358974247567E-13,2.06597317199956,
-5.05238212378245E-14));
#125265=CARTESIAN_POINT('',(7.04361153473072,1.88359401255142,2.57634169805879));
#125266=CARTESIAN_POINT('Origin',(-0.171398987472374,2.01784567825094,-0.0855171611339606));
#125267=CARTESIAN_POINT('',(7.21780170794699,1.97432008362733,2.03797411287211));
#125268=CARTESIAN_POINT('Origin',(-0.180347906282772,1.87500217343594,-0.0674445279812566));
#125269=CARTESIAN_POINT('Origin',(-0.183777732123206,2.01785750426266,-0.0591464868456302));
#125270=CARTESIAN_POINT('Ctrl Pts',(6.808301998,2.104810499,2.491891632));
#125271=CARTESIAN_POINT('Ctrl Pts',(6.943588774,2.039629277,2.122263509));
#125272=CARTESIAN_POINT('Ctrl Pts',(7.038063521,1.974320085,1.74016145));
#125273=CARTESIAN_POINT('Ctrl Pts',(6.954741811,2.104810499,2.807412748));
#125274=CARTESIAN_POINT('Ctrl Pts',(7.10715847900001,2.039629277,2.429834291));
#125275=CARTESIAN_POINT('Ctrl Pts',(7.21780171200001,1.974320085,2.037974103));
#125276=CARTESIAN_POINT('',(7.12793261324207,1.97432008293108,1.88906778879299));
#125277=CARTESIAN_POINT('Ctrl Pts',(7.03148870360976,1.96978752929256,1.76675322528271));
#125278=CARTESIAN_POINT('Ctrl Pts',(7.03477611230488,1.97205380714625,1.75345733764136));
#125279=CARTESIAN_POINT('Ctrl Pts',(7.038063521,1.974320085,1.74016145));
#125280=CARTESIAN_POINT('Ctrl Pts',(7.133417862,2.040055578,1.354501886));
#125281=CARTESIAN_POINT('Ctrl Pts',(7.18606241200001,2.104802836,0.960732536));
#125282=CARTESIAN_POINT('Ctrl Pts',(7.33059826296775,1.96978752929256,1.58777056923608));
#125283=CARTESIAN_POINT('Ctrl Pts',(7.33354541825529,1.97205380714625,1.57391090731557));
#125284=CARTESIAN_POINT('Ctrl Pts',(7.33649257354279,1.974320085,1.56005124539505));
#125285=CARTESIAN_POINT('Ctrl Pts',(7.42197754858784,2.040055578,1.15803888505944));
#125286=CARTESIAN_POINT('Ctrl Pts',(7.46302504513293,2.104802836,0.749093018303043));
#125287=CARTESIAN_POINT('',(7.335876173956,1.97432008542257,1.56042326496528));
#125288=CARTESIAN_POINT('',(7.43298288878896,2.06488542554557,1.00038250462391));
#125289=CARTESIAN_POINT('Origin',(-0.180854772319673,1.87505114218545,-0.0547345597610988));
#125290=CARTESIAN_POINT('Ctrl Pts',(7.1854362047806,2.10403448594993,0.965404863426473));
#125291=CARTESIAN_POINT('Ctrl Pts',(7.22663047536372,2.09719845374919,0.971272628909129));
#125292=CARTESIAN_POINT('Ctrl Pts',(7.26787819505574,2.09052278113993,0.977122699762518));
#125293=CARTESIAN_POINT('Ctrl Pts',(7.35038100578259,2.07748305173631,0.988778520285952));
#125294=CARTESIAN_POINT('Ctrl Pts',(7.39168086172629,2.07111192518725,0.994590590199989));
#125295=CARTESIAN_POINT('Ctrl Pts',(7.43298288835397,2.06488542584543,1.00038250804817));
#125296=CARTESIAN_POINT('',(7.18696984626825,1.97432008626233,1.65029236204173));
#125297=CARTESIAN_POINT('Origin',(3.46077333457373E-13,2.06597317199922,
1.03731042852551E-13));
#125298=CARTESIAN_POINT('',(7.43277311984019,1.88359401261866,1.00193998853181));
#125299=CARTESIAN_POINT('Origin',(-0.18577510321681,2.01784564018602,-0.0466720355230915));
#125300=CARTESIAN_POINT('',(7.48715770716292,1.97432008362733,0.438713400513213));
#125301=CARTESIAN_POINT('Origin',(-0.19063011925592,1.87500216022345,-0.0270982572346022));
#125302=CARTESIAN_POINT('Origin',(-0.192195711059792,2.01785751467762,-0.0182568766687107));
#125303=CARTESIAN_POINT('Ctrl Pts',(7.184810722,2.104810499,0.970048913));
#125304=CARTESIAN_POINT('Ctrl Pts',(7.23747544800001,2.039629277,0.579979832));
#125305=CARTESIAN_POINT('Ctrl Pts',(7.24760078,1.974320085,0.186501829));
#125306=CARTESIAN_POINT('Ctrl Pts',(7.395654567,2.104810499,1.24671309));
#125307=CARTESIAN_POINT('Ctrl Pts',(7.463339611,2.039629277,0.845197129));
#125308=CARTESIAN_POINT('Ctrl Pts',(7.487157709,1.974320085,0.43871339));
#125309=CARTESIAN_POINT('',(7.36737924396087,1.97432008293108,0.312607622205938));
#125310=CARTESIAN_POINT('Ctrl Pts',(7.24689612384429,1.96978752930384,0.213885294717906));
#125311=CARTESIAN_POINT('Ctrl Pts',(7.24724845192216,1.97205380715189,0.200193561858956));
#125312=CARTESIAN_POINT('Ctrl Pts',(7.24760078,1.974320085,0.186501829));
#125313=CARTESIAN_POINT('Ctrl Pts',(7.257820383,2.040055578,-0.210639594));
#125314=CARTESIAN_POINT('Ctrl Pts',(7.224585363,2.104802836,-0.606519857));
#125315=CARTESIAN_POINT('Ctrl Pts',(7.50053668693796,1.96978752930384,-0.0252125596737303));
#125316=CARTESIAN_POINT('Ctrl Pts',(7.50043552174716,1.97205380715189,-0.0393817416357748));
#125317=CARTESIAN_POINT('Ctrl Pts',(7.50033435655642,1.974320085,-0.0535509235978196));
#125318=CARTESIAN_POINT('Ctrl Pts',(7.49739996627716,2.040055578,-0.464541201097412));
#125319=CARTESIAN_POINT('Ctrl Pts',(7.44957652221315,2.104802836,-0.872750138699384));
#125320=CARTESIAN_POINT('',(7.49981234051242,1.97432008541403,-0.0530550903464663));
#125321=CARTESIAN_POINT('',(7.47425654638148,2.06488542557781,-0.620877486031077));
#125322=CARTESIAN_POINT('Origin',(-0.188392808761042,1.87505115454289,-0.0145764631325766));
#125323=CARTESIAN_POINT('Ctrl Pts',(7.22497820783533,2.10403448606495,-0.601822150024921));
#125324=CARTESIAN_POINT('Ctrl Pts',(7.26647055856495,2.09719848953937,-0.604947103725027));
#125325=CARTESIAN_POINT('Ctrl Pts',(7.30801127704622,2.09052285362558,-0.608100825741811));
#125326=CARTESIAN_POINT('Ctrl Pts',(7.39109133589379,2.07748305180721,-0.614453212590015));
#125327=CARTESIAN_POINT('Ctrl Pts',(7.43267504747039,2.07111192523526,-0.617655273859918));
#125328=CARTESIAN_POINT('Ctrl Pts',(7.47425654669052,2.0648854259041,-0.620877482673569));
#125329=CARTESIAN_POINT('',(7.37370656042999,1.97432008626233,0.0667233722376788));
#125330=CARTESIAN_POINT('Origin',(-3.56919355182228E-13,2.06597317199989,
-5.50571415715295E-14));
#125331=CARTESIAN_POINT('',(7.47438649539287,1.88359401260575,-0.619311321310287));
#125332=CARTESIAN_POINT('Origin',(-0.191465076505951,2.01784564451317,-0.00564471672548951));
#125333=CARTESIAN_POINT('',(7.40642253346448,1.97432008362734,-1.1810610633371));
#125334=CARTESIAN_POINT('Origin',(-0.191998518223641,1.87500217719841,0.0145151198199273));
#125335=CARTESIAN_POINT('Origin',(-0.191626963176276,2.01785748769558,0.0234863549441309));
#125336=CARTESIAN_POINT('Ctrl Pts',(7.225365682,2.104810499,-0.597152216));
#125337=CARTESIAN_POINT('Ctrl Pts',(7.192945813,2.039629277,-0.989423057));
#125338=CARTESIAN_POINT('Ctrl Pts',(7.118248282,1.974320085,-1.375878411));
#125339=CARTESIAN_POINT('Ctrl Pts',(7.490754735,2.104810499,-0.372281487));
#125340=CARTESIAN_POINT('Ctrl Pts',(7.470543277,2.039629277,-0.778960512000001));
#125341=CARTESIAN_POINT('Ctrl Pts',(7.406422533,1.974320085,-1.181061074));
#125342=CARTESIAN_POINT('',(7.26233540970488,1.97432008293108,-1.27846972997522));
#125343=CARTESIAN_POINT('Ctrl Pts',(7.12344673600873,1.96978752934063,-1.34898367552147));
#125344=CARTESIAN_POINT('Ctrl Pts',(7.12084750900437,1.97205380717028,-1.36243104326073));
#125345=CARTESIAN_POINT('Ctrl Pts',(7.118248282,1.974320085,-1.375878411));
#125346=CARTESIAN_POINT('Ctrl Pts',(7.04285528900001,2.040055578,-1.7659318));
#125347=CARTESIAN_POINT('Ctrl Pts',(6.925294731,2.104802836,-2.145412056));
#125348=CARTESIAN_POINT('Ctrl Pts',(7.31975835219021,1.96978752934063,-1.63701677796964));
#125349=CARTESIAN_POINT('Ctrl Pts',(7.31661359694591,1.97205380717028,-1.65083294469777));
#125350=CARTESIAN_POINT('Ctrl Pts',(7.31346884170166,1.974320085,-1.66464911142589));
#125351=CARTESIAN_POINT('Ctrl Pts',(7.22225229550629,2.040055578,-2.06539985757794));
#125352=CARTESIAN_POINT('Ctrl Pts',(7.08779408177615,2.104802836,-2.45378447032773));
#125353=CARTESIAN_POINT('',(7.31306561959532,1.97432008541404,-1.66405265246183));
#125354=CARTESIAN_POINT('',(7.16604227551646,2.06488542558446,-2.21310593549342));
#125355=CARTESIAN_POINT('Origin',(-0.187121611163891,1.87505116918617,0.0262631604130306));
#125356=CARTESIAN_POINT('Ctrl Pts',(6.92668825952681,2.10403448598584,-2.14090862818555));
#125357=CARTESIAN_POINT('Ctrl Pts',(6.9665387449173,2.09719849370837,-2.15288014382144));
#125358=CARTESIAN_POINT('Ctrl Pts',(7.00643027970097,2.09052286216309,-2.16489015172776));
#125359=CARTESIAN_POINT('Ctrl Pts',(7.08620245038645,2.07748305175337,-2.18895379605831));
#125360=CARTESIAN_POINT('Ctrl Pts',(7.12612560916814,2.07111192523224,-2.20102026360126));
#125361=CARTESIAN_POINT('Ctrl Pts',(7.16604227657075,2.06488542588779,-2.21310593216758));
#125362=CARTESIAN_POINT('',(7.21565695159499,1.97432008626233,-1.51996552892817));
#125363=CARTESIAN_POINT('Origin',(-6.78276879106932E-13,2.06597317200044,
1.95915332568131E-13));
#125364=CARTESIAN_POINT('',(7.16650586494505,1.8835940125881,-2.21160432283929));
#125365=CARTESIAN_POINT('Origin',(-0.188202231489694,2.01784568714537,0.0356465962586838));
#125366=CARTESIAN_POINT('',(6.979371273744,1.97432008362733,-2.74561042469069));
#125367=CARTESIAN_POINT('Origin',(-0.184389231669062,1.87500215963995,0.0554497128324294));
#125368=CARTESIAN_POINT('Origin',(-0.182098181484285,2.01785749936806,0.0641314642319986));
#125369=CARTESIAN_POINT('Ctrl Pts',(6.928070572,2.104810499,-2.13643117));
#125370=CARTESIAN_POINT('Ctrl Pts',(6.812082027,2.039629277,-2.512561624));
#125371=CARTESIAN_POINT('Ctrl Pts',(6.656054405,1.974320085,-2.873924105));
#125372=CARTESIAN_POINT('Ctrl Pts',(7.235595536,2.104810499,-1.973868596));
#125373=CARTESIAN_POINT('Ctrl Pts',(7.128432642,2.039629277,-2.366694825));
#125374=CARTESIAN_POINT('Ctrl Pts',(6.979371271,1.974320085,-2.745610435));
#125375=CARTESIAN_POINT('',(6.81771284284578,1.97432008293108,-2.80976725824203));
#125376=CARTESIAN_POINT('Ctrl Pts',(6.66691289521506,1.96978752930778,-2.84877566723));
#125377=CARTESIAN_POINT('Ctrl Pts',(6.66148365010753,1.97205380715386,-2.86134988611501));
#125378=CARTESIAN_POINT('Ctrl Pts',(6.656054405,1.974320085,-2.873924105));
#125379=CARTESIAN_POINT('Ctrl Pts',(6.49857411,2.040055578,-3.238650998));
#125380=CARTESIAN_POINT('Ctrl Pts',(6.302185015,2.104802836,-3.583987171));
#125381=CARTESIAN_POINT('Ctrl Pts',(6.79671625280338,1.96978752930778,-3.1722759107947));
#125382=CARTESIAN_POINT('Ctrl Pts',(6.79067495268329,1.97205380715386,-3.18509303387333));
#125383=CARTESIAN_POINT('Ctrl Pts',(6.78463365256321,1.974320085,-3.19791015695202));
#125384=CARTESIAN_POINT('Ctrl Pts',(6.60940013367591,2.040055578,-3.56968271160877));
#125385=CARTESIAN_POINT('Ctrl Pts',(6.39459426724597,2.104802836,-3.92008256653065));
#125386=CARTESIAN_POINT('',(6.78436807859121,1.97432008541403,-3.19724096198437));
#125387=CARTESIAN_POINT('',(6.52275183234442,2.06488542557874,-3.70185201111922));
#125388=CARTESIAN_POINT('Origin',(-0.177101200238827,1.8750511420646,0.0658748586744901));
#125389=CARTESIAN_POINT('Ctrl Pts',(6.304514067401,2.10403448599765,-3.57988859824468));
#125390=CARTESIAN_POINT('Ctrl Pts',(6.3408593461888,2.09719849416704,-3.60014690175533));
#125391=CARTESIAN_POINT('Ctrl Pts',(6.37723643971121,2.09052286306901,-3.62045162178728));
#125392=CARTESIAN_POINT('Ctrl Pts',(6.44997061394838,2.07748305178323,-3.66110133296034));
#125393=CARTESIAN_POINT('Ctrl Pts',(6.48636645772073,2.07111192523635,-3.6814679922869));
#125394=CARTESIAN_POINT('Ctrl Pts',(6.52275183406528,2.06488542589603,-3.70185200814441));
#125395=CARTESIAN_POINT('',(6.72021124318542,1.97432008626233,-3.03558253094808));
#125396=CARTESIAN_POINT('Origin',(4.77482636762616E-13,2.06597317200011,
-2.85795692667179E-13));
#125397=CARTESIAN_POINT('',(6.52352738588618,1.88359401261646,-3.70048516261239));
#125398=CARTESIAN_POINT('Origin',(-0.176139373126123,2.01784567505773,0.075271214052744));
#125399=CARTESIAN_POINT('',(6.22597237088156,1.97432008362661,-4.18177809352906));
#125400=CARTESIAN_POINT('Origin',(-0.168158374947894,1.87500219531754,0.093791632467935));
#125401=CARTESIAN_POINT('Origin',(-0.164054535610359,2.01785749475703,0.101777878198789));
#125402=CARTESIAN_POINT('Ctrl Pts',(6.306826583,2.104810499,-3.575812977));
#125403=CARTESIAN_POINT('Ctrl Pts',(6.112692857,2.039629277,-3.918215602));
#125404=CARTESIAN_POINT('Ctrl Pts',(5.882630822,1.974320085,-4.237588302));
#125405=CARTESIAN_POINT('Ctrl Pts',(6.64210793300001,2.104810499,-3.483159803));
#125406=CARTESIAN_POINT('Ctrl Pts',(6.45300442,2.039629277,-3.843765118));
#125407=CARTESIAN_POINT('Ctrl Pts',(6.225972366,1.974320085,-4.181778103));
#125408=CARTESIAN_POINT('',(6.05430160126387,1.97432008293001,-4.2096831920532));
#125409=CARTESIAN_POINT('Ctrl Pts',(5.89864161766491,1.96978752925783,-4.21536207494712));
#125410=CARTESIAN_POINT('Ctrl Pts',(5.89063621983239,1.97205380712895,-4.22647518847359));
#125411=CARTESIAN_POINT('Ctrl Pts',(5.882630822,1.974320085,-4.237588302));
#125412=CARTESIAN_POINT('Ctrl Pts',(5.650426828,2.040055578,-4.559934474));
#125413=CARTESIAN_POINT('Ctrl Pts',(5.384392131,2.104802836,-4.85497903));
#125414=CARTESIAN_POINT('Ctrl Pts',(5.95586725441693,1.96978752925783,-4.55920294697488));
#125415=CARTESIAN_POINT('Ctrl Pts',(5.94721189386265,1.97205380712895,-4.57042171203193));
#125416=CARTESIAN_POINT('Ctrl Pts',(5.93855653330852,1.974320085,-4.58164047708885));
#125417=CARTESIAN_POINT('Ctrl Pts',(5.68749976732876,2.040055578,-4.90705116978796));
#125418=CARTESIAN_POINT('Ctrl Pts',(5.40239033188223,2.104802836,-5.2030819588303));
#125419=CARTESIAN_POINT('',(5.93844102545487,1.97432008541404,-4.58092983702517));
#125420=CARTESIAN_POINT('',(5.57446476273787,2.06488542557757,-5.01750360090843));
#125421=CARTESIAN_POINT('Origin',(-0.158799451568832,1.87505116138121,0.102406197804297));
#125422=CARTESIAN_POINT('Ctrl Pts',(5.38754780344266,2.10403448599945,-4.85147695703863));
#125423=CARTESIAN_POINT('Ctrl Pts',(5.41868842775781,2.09719849105826,-4.87907480555496));
#125424=CARTESIAN_POINT('Ctrl Pts',(5.44985014665898,2.09052285673973,-4.9067248264811));
#125425=CARTESIAN_POINT('Ctrl Pts',(5.51214531992537,2.07748305178984,-4.9620598403968));
#125426=CARTESIAN_POINT('Ctrl Pts',(5.54331201945759,2.07111192523415,-4.98977436912689));
#125427=CARTESIAN_POINT('Ctrl Pts',(5.57446476503845,2.06488542589882,-5.01750359839596));
#125428=CARTESIAN_POINT('',(5.91053592562699,1.97432008626236,-4.40925906729761));
#125429=CARTESIAN_POINT('Origin',(-1.21430643318376E-14,2.06597317200067,
5.03069808033274E-14));
#125430=CARTESIAN_POINT('',(5.57551601667315,1.88359401262239,-5.01633542971868));
#125431=CARTESIAN_POINT('Origin',(-0.155839863892731,2.01784566950499,0.11137583991492));
#125432=CARTESIAN_POINT('',(5.18145391881594,1.97432008362662,-5.42241046679518));
#125433=CARTESIAN_POINT('Origin',(-0.14406458720886,1.87500217976684,0.127748007483152));
#125434=CARTESIAN_POINT('Origin',(-0.138339389893165,2.01785750358587,0.134664849330288));
#125435=CARTESIAN_POINT('Ctrl Pts',(5.390682393,2.104810499,-4.847993744));
#125436=CARTESIAN_POINT('Ctrl Pts',(5.127480962,2.039629277,-5.140658173));
#125437=CARTESIAN_POINT('Ctrl Pts',(4.83414196,1.974320085,-5.403107579));
#125438=CARTESIAN_POINT('Ctrl Pts',(5.738042744,2.104810499,-4.829582328));
#125439=CARTESIAN_POINT('Ctrl Pts',(5.475840884,2.039629277,-5.141105227));
#125440=CARTESIAN_POINT('Ctrl Pts',(5.181453912,1.974320085,-5.422410475));
#125441=CARTESIAN_POINT('',(5.0077979453398,1.97432008293002,-5.41275901835897));
#125442=CARTESIAN_POINT('Ctrl Pts',(4.85455641397875,1.96978752925425,-5.38484283648086));
#125443=CARTESIAN_POINT('Ctrl Pts',(4.84434918698943,1.97205380712716,-5.39397520774036));
#125444=CARTESIAN_POINT('Ctrl Pts',(4.83414196,1.974320085,-5.403107579));
#125445=CARTESIAN_POINT('Ctrl Pts',(4.538071868,2.040055578,-5.668000483));
#125446=CARTESIAN_POINT('Ctrl Pts',(4.214831056,2.104802836,-5.898957465));
#125447=CARTESIAN_POINT('Ctrl Pts',(4.83652852359848,1.96978752925425,-5.73294672106691));
#125448=CARTESIAN_POINT('Ctrl Pts',(4.82566381768852,1.97205380712716,-5.74204255096055));
#125449=CARTESIAN_POINT('Ctrl Pts',(4.81479911177867,1.974320085,-5.75113838085421));
#125450=CARTESIAN_POINT('Ctrl Pts',(4.49965823349521,2.040055578,-6.01497136862089));
#125451=CARTESIAN_POINT('Ctrl Pts',(4.15757662825725,2.104802836,-6.24279102253975));
#125452=CARTESIAN_POINT('',(4.81483906876701,1.97432008542257,-5.75041952730824));
#125453=CARTESIAN_POINT('',(4.36552191631196,2.06488542557993,-6.09854229912174));
#125454=CARTESIAN_POINT('Origin',(-0.133072574609535,1.87505111885393,0.134149269772198));
#125455=CARTESIAN_POINT('Ctrl Pts',(4.21866579300695,2.10403448594715,-5.89621564465873));
#125456=CARTESIAN_POINT('Ctrl Pts',(4.24314564015502,2.09719849237975,-5.92986257791126));
#125457=CARTESIAN_POINT('Ctrl Pts',(4.26763487253668,2.09052285948726,-5.96356499754119));
#125458=CARTESIAN_POINT('Ctrl Pts',(4.31657823718754,2.0774830517774,-6.03099794484554));
#125459=CARTESIAN_POINT('Ctrl Pts',(4.34105847207769,2.07111192523094,-6.0647644424249));
#125460=CARTESIAN_POINT('Ctrl Pts',(4.3655219191016,2.06488542590188,-6.0985422971607));
#125461=CARTESIAN_POINT('',(4.82449051785214,1.97432008626236,-5.57676354993728));
#125462=CARTESIAN_POINT('Origin',(6.03250088770935E-13,2.06597317199933,
-7.52869988573934E-13));
#125463=CARTESIAN_POINT('',(4.36679971533024,1.88359401259344,-6.0976274274486));
#125464=CARTESIAN_POINT('Origin',(-0.128253981616274,2.01784565151063,0.142273006942648));
#125465=CARTESIAN_POINT('',(3.89465644041332,1.97432008362662,-6.40949695345443));
#125466=CARTESIAN_POINT('Origin',(-0.113234348416686,1.87500219878722,0.155730897896531));
#125467=CARTESIAN_POINT('Origin',(-0.106156210910903,2.01785750866169,0.161255456921047));
#125468=CARTESIAN_POINT('Ctrl Pts',(4.222475885,2.104810499,-5.893487711));
#125469=CARTESIAN_POINT('Ctrl Pts',(3.902513756,2.039629277,-6.122729281));
#125470=CARTESIAN_POINT('Ctrl Pts',(3.559613992,1.974320085,-6.315983552));
#125471=CARTESIAN_POINT('Ctrl Pts',(4.565673054,2.104810499,-5.950178952));
#125472=CARTESIAN_POINT('Ctrl Pts',(4.242633113,2.039629277,-6.198052969));
#125473=CARTESIAN_POINT('Ctrl Pts',(3.894656432,1.974320085,-6.40949696));
#125474=CARTESIAN_POINT('',(3.72713522297897,1.97432008293002,-6.3627402495688));
#125475=CARTESIAN_POINT('Ctrl Pts',(3.58347754718451,1.96978752924432,-6.30253433321539));
#125476=CARTESIAN_POINT('Ctrl Pts',(3.57154576959229,1.97205380712213,-6.30925894260769));
#125477=CARTESIAN_POINT('Ctrl Pts',(3.559613992,1.974320085,-6.315983552));
#125478=CARTESIAN_POINT('Ctrl Pts',(3.21352171,2.040055578,-6.511037088));
#125479=CARTESIAN_POINT('Ctrl Pts',(2.848189165,2.104802836,-6.667107205));
#125480=CARTESIAN_POINT('Ctrl Pts',(3.49103909375301,1.96978752924423,-6.63862427934538));
#125481=CARTESIAN_POINT('Ctrl Pts',(3.47847306406143,1.97205380712215,-6.64517186317271));
#125482=CARTESIAN_POINT('Ctrl Pts',(3.46590703436985,1.974320085,-6.65171944700002));
#125483=CARTESIAN_POINT('Ctrl Pts',(3.10141768163073,2.040055578,-6.84163819220421));
#125484=CARTESIAN_POINT('Ctrl Pts',(2.71835926323473,2.104802836,-6.9905941149948));
#125485=CARTESIAN_POINT('',(3.46610058947509,1.97432008542257,-6.65102598939106));
#125486=CARTESIAN_POINT('',(2.95245211747942,2.06488542557422,-6.89441993709166));
#125487=CARTESIAN_POINT('Origin',(-0.10112323409008,1.87505112184823,0.159619520245724));
#125488=CARTESIAN_POINT('Ctrl Pts',(2.85252365852959,2.10403448588764,-6.66525384212721));
#125489=CARTESIAN_POINT('Ctrl Pts',(2.8691981784706,2.097198453736,-6.70337678752731));
#125490=CARTESIAN_POINT('Ctrl Pts',(2.88586994821712,2.09052278108633,-6.74155596809501));
#125491=CARTESIAN_POINT('Ctrl Pts',(2.91917275381454,2.07748305174459,-6.81793328817871));
#125492=CARTESIAN_POINT('Ctrl Pts',(2.93582185562442,2.07111192521568,-6.85617287054979));
#125493=CARTESIAN_POINT('Ctrl Pts',(2.9524521206652,2.06488542588622,-6.89441993575723));
#125494=CARTESIAN_POINT('',(3.51285729480354,1.97432008626233,-6.48350476831375));
#125495=CARTESIAN_POINT('Origin',(2.97071395261028E-13,2.06597317199944,
-7.02996688639601E-13));
#125496=CARTESIAN_POINT('',(2.95389671194769,1.88359401259013,-6.8938011436048));
#125497=CARTESIAN_POINT('Origin',(-0.0946710014919422,2.01784568231715,
0.166517615899912));
#125498=CARTESIAN_POINT('',(2.42574915565128,1.97432008362663,-7.09688248541461));
#125499=CARTESIAN_POINT('Origin',(-0.0771095214129697,1.87500220161273,
0.176432218877178));
#125500=CARTESIAN_POINT('Origin',(-0.0690092930180509,2.01785749278518,
0.180306152982286));
#125501=CARTESIAN_POINT('Ctrl Pts',(2.856831098,2.104810499,-6.663408743));
#125502=CARTESIAN_POINT('Ctrl Pts',(2.495069344,2.039629277,-6.81850837300001));
#125503=CARTESIAN_POINT('Ctrl Pts',(2.118642431,1.974320085,-6.933531153));
#125504=CARTESIAN_POINT('Ctrl Pts',(3.179817567,2.104810499,-6.79255182100001));
#125505=CARTESIAN_POINT('Ctrl Pts',(2.811044533,2.039629277,-6.965186642));
#125506=CARTESIAN_POINT('Ctrl Pts',(2.425749146,1.974320085,-7.09688249));
#125507=CARTESIAN_POINT('',(2.27219580060485,1.97432008293002,-7.01520681757929));
#125508=CARTESIAN_POINT('Ctrl Pts',(2.14483925400811,1.96978752925302,-6.92552632842096));
#125509=CARTESIAN_POINT('Ctrl Pts',(2.13174084250406,1.97205380712647,-6.92952874071054));
#125510=CARTESIAN_POINT('Ctrl Pts',(2.118642431,1.974320085,-6.93353115299999));
#125511=CARTESIAN_POINT('Ctrl Pts',(1.738710849,2.040055578,-7.049624836));
#125512=CARTESIAN_POINT('Ctrl Pts',(1.348369115,2.104802836,-7.123510422));
#125513=CARTESIAN_POINT('Ctrl Pts',(1.9823125558243,1.96978752925301,-7.23388714288003));
#125514=CARTESIAN_POINT('Ctrl Pts',(1.9686327759748,1.97205380712648,-7.23758032291807));
#125515=CARTESIAN_POINT('Ctrl Pts',(1.95495299612523,1.974320085,-7.24127350295612));
#125516=CARTESIAN_POINT('Ctrl Pts',(1.55815828570982,2.040055578,-7.34839761751268));
#125517=CARTESIAN_POINT('Ctrl Pts',(1.1520344401105,2.104802836,-7.41152479726465));
#125518=CARTESIAN_POINT('',(1.9552910988738,1.97432008542256,-7.24063786665295));
#125519=CARTESIAN_POINT('',(1.40132893891287,2.06488542556653,-7.36792216172689));
#125520=CARTESIAN_POINT('Origin',(-0.0644455498001614,1.8750511310427,0.177626164917501));
#125521=CARTESIAN_POINT('Ctrl Pts',(1.35300068819368,2.10403448599822,-7.12263217760191));
#125522=CARTESIAN_POINT('Ctrl Pts',(1.36109001434623,2.09719849307877,-7.1634481242099));
#125523=CARTESIAN_POINT('Ctrl Pts',(1.36916456012967,2.09052286086466,-7.20431836909688));
#125524=CARTESIAN_POINT('Ctrl Pts',(1.38526999696438,2.07748305175325,-7.2860696486221));
#125525=CARTESIAN_POINT('Ctrl Pts',(1.39330947212822,2.07111192521438,-7.32699427557641));
#125526=CARTESIAN_POINT('Ctrl Pts',(1.40132894232119,2.06488542587175,-7.3679221611055));
#125527=CARTESIAN_POINT('',(2.03696676943691,1.97432008626233,-7.08708450836249));
#125528=CARTESIAN_POINT('Origin',(-3.10894972960218E-13,2.06597317200011,
1.45413195373756E-12));
#125529=CARTESIAN_POINT('',(1.40287278194287,1.88359401260661,-7.36762838021725));
#125530=CARTESIAN_POINT('Origin',(-0.056661288712726,2.01784569359405,0.182975980514766));
#125531=CARTESIAN_POINT('',(0.843416536409591,1.97432008362659,-7.45242568060032));
#125532=CARTESIAN_POINT('Origin',(-0.0373790373345705,1.87500222213718,
0.18888364590116));
#125533=CARTESIAN_POINT('Origin',(-0.0286353804236349,2.01785753439472,
0.190925474714267));
#125534=CARTESIAN_POINT('Ctrl Pts',(1.357604063,2.104810499,-7.121756188));
#125535=CARTESIAN_POINT('Ctrl Pts',(0.970958263,2.039629277,-7.19546159100001));
#125536=CARTESIAN_POINT('Ctrl Pts',(0.578605504,1.974320085,-7.22687454400001));
#125537=CARTESIAN_POINT('Ctrl Pts',(1.645277344,2.104810499,-7.317312516));
#125538=CARTESIAN_POINT('Ctrl Pts',(1.248014636,2.039629277,-7.40663593));
#125539=CARTESIAN_POINT('Ctrl Pts',(0.843416526,1.974320085,-7.452425683));
#125540=CARTESIAN_POINT('',(0.71101102766468,1.97432008293001,-7.33965011227314));
#125541=CARTESIAN_POINT('Ctrl Pts',(0.589148911429185,1.97256991806615,
-7.22603040681208));
#125542=CARTESIAN_POINT('Ctrl Pts',(0.583877207714593,1.97344500153307,
-7.22645247540605));
#125543=CARTESIAN_POINT('Ctrl Pts',(0.578605504,1.974320085,-7.226874544));
#125544=CARTESIAN_POINT('Ctrl Pts',(0.182599802,2.040055578,-7.258579962));
#125545=CARTESIAN_POINT('Ctrl Pts',(-0.214499177,2.104802836,-7.246826209));
#125546=CARTESIAN_POINT('Ctrl Pts',(0.363804157315899,1.97256991806615,
-7.4913823886135));
#125547=CARTESIAN_POINT('Ctrl Pts',(0.35833913061739,1.97344500153307,-7.49163979556223));
#125548=CARTESIAN_POINT('Ctrl Pts',(0.35287410391888,1.974320085,-7.49189720251094));
#125549=CARTESIAN_POINT('Ctrl Pts',(-0.0576538489707087,2.040055578,-7.51123338393259));
#125550=CARTESIAN_POINT('Ctrl Pts',(-0.467836611157437,2.104802836,-7.48559768636607));
#125551=CARTESIAN_POINT('Ctrl Pts',(-0.209787090640295,2.10403448593187,
-7.2469641490316));
#125552=CARTESIAN_POINT('Ctrl Pts',(-0.210661115512503,2.09719845377858,
-7.28856504641087));
#125553=CARTESIAN_POINT('Ctrl Pts',(-0.211561248998728,2.09052278112551,
-7.33021582666021));
#125554=CARTESIAN_POINT('Ctrl Pts',(-0.213406445786063,2.07748305177212,
-7.41351749012979));
#125555=CARTESIAN_POINT('Ctrl Pts',(-0.214352514273131,2.0711119252164,
-7.45521357168871));
#125556=CARTESIAN_POINT('Ctrl Pts',(-0.215318820520802,2.06488542588042,
-7.49690853500171));
#125557=CARTESIAN_POINT('',(0.465829941722541,1.97432008626233,-7.35928005451118));
#125558=CARTESIAN_POINT('Ctrl Pts',(-0.205103028,2.104810499,-7.247098229));
#125559=CARTESIAN_POINT('Ctrl Pts',(-0.598553747,2.039629277,-7.235963023));
#125560=CARTESIAN_POINT('Ctrl Pts',(-0.988486373,1.974320085,-7.18229731300001));
#125561=CARTESIAN_POINT('Ctrl Pts',(0.033805781,2.104810499,-7.49992381100001));
#125562=CARTESIAN_POINT('Ctrl Pts',(-0.373371039,2.039629277,-7.501759154));
#125563=CARTESIAN_POINT('Ctrl Pts',(-0.778353314,1.974320085,-7.459501734));
#125564=CARTESIAN_POINT('',(-0.883419830867674,1.97432008293002,-7.32089952502436));
#125565=CARTESIAN_POINT('Ctrl Pts',(-0.961349641748257,1.96978752924776,
-7.18603209141629));
#125566=CARTESIAN_POINT('Ctrl Pts',(-0.974918007374125,1.97205380712385,
-7.18416470220819));
#125567=CARTESIAN_POINT('Ctrl Pts',(-0.988486373000001,1.974320085,-7.182297313));
#125568=CARTESIAN_POINT('Ctrl Pts',(-1.38204941,2.040055578,-7.128131956));
#125569=CARTESIAN_POINT('Ctrl Pts',(-1.767337726,2.104802836,-7.031288457));
#125570=CARTESIAN_POINT('Ctrl Pts',(-1.23833222251996,1.96978752924775,
-7.3976495986289));
#125571=CARTESIAN_POINT('Ctrl Pts',(-1.25229838056131,1.97205380712385,
-7.39525744755006));
#125572=CARTESIAN_POINT('Ctrl Pts',(-1.2662645386027,1.974320085,-7.39286529647123));
#125573=CARTESIAN_POINT('Ctrl Pts',(-1.67136591378274,2.040055578,-7.32347873441183));
#125574=CARTESIAN_POINT('Ctrl Pts',(-2.06646034810132,2.104802836,-7.21024443357639));
#125575=CARTESIAN_POINT('',(-1.26569078805863,1.97432008542257,-7.39243037423573));
#125576=CARTESIAN_POINT('',(-1.82189851740587,2.0648854255639,-7.27534779711598));
#125577=CARTESIAN_POINT('Origin',(0.0160941115438731,1.87505115732695,0.188269130444804));
#125578=CARTESIAN_POINT('Ctrl Pts',(-1.76276545876383,2.10403448595781,
-7.0324361312964));
#125579=CARTESIAN_POINT('Ctrl Pts',(-1.77256201257561,2.09719845378385,
-7.07287653328555));
#125580=CARTESIAN_POINT('Ctrl Pts',(-1.78239478794987,2.09052278111519,
-7.11336003937026));
#125581=CARTESIAN_POINT('Ctrl Pts',(-1.80210424018197,2.07748305175972,
-7.19431749343474));
#125582=CARTESIAN_POINT('Ctrl Pts',(-1.81199161504939,2.07111192520572,
-7.23483536702823));
#125583=CARTESIAN_POINT('Ctrl Pts',(-1.82189851412105,2.06488542588051,
-7.27534779796791));
#125584=CARTESIAN_POINT('',(-1.12708857585293,1.97432008626233,-7.28736384418272));
#125585=CARTESIAN_POINT('Origin',(-1.65991352607531E-13,2.06597317199956,
-9.19403442267708E-14));
#125586=CARTESIAN_POINT('',(-1.82037400765965,1.88359401257266,-7.27572941129029));
#125587=CARTESIAN_POINT('Origin',(0.0254052287321954,2.01784566722006,0.189855907214538));
#125588=CARTESIAN_POINT('',(-2.36372820653794,1.97432008362663,-7.11777977619209));
#125589=CARTESIAN_POINT('Origin',(0.0453858973819207,1.87500220797284,0.18712122657347));
#125590=CARTESIAN_POINT('Origin',(0.0541787152175737,2.01785749269258,0.185302764171555));
#125591=CARTESIAN_POINT('Ctrl Pts',(-1.75821973,2.104810499,-7.033574012));
#125592=CARTESIAN_POINT('Ctrl Pts',(-2.14007805,2.039629277,-6.938118866));
#125593=CARTESIAN_POINT('Ctrl Pts',(-2.509357726,1.974320085,-6.801883842));
#125594=CARTESIAN_POINT('Ctrl Pts',(-1.579246502,2.104810499,-7.331847004));
#125595=CARTESIAN_POINT('Ctrl Pts',(-1.9772983,2.039629277,-7.246108457));
#125596=CARTESIAN_POINT('Ctrl Pts',(-2.363728217,1.974320085,-7.117779774));
#125597=CARTESIAN_POINT('',(-2.4365429594907,1.97432008293001,-6.95983181220429));
#125598=CARTESIAN_POINT('Ctrl Pts',(-2.48365830353901,1.96978752926819,
-6.81136489836744));
#125599=CARTESIAN_POINT('Ctrl Pts',(-2.49650801476954,1.97205380713406,
-6.80662437018367));
#125600=CARTESIAN_POINT('Ctrl Pts',(-2.509357726,1.974320085,-6.801883842));
#125601=CARTESIAN_POINT('Ctrl Pts',(-2.882075527,2.040055578,-6.664380422));
#125602=CARTESIAN_POINT('Ctrl Pts',(-3.237537527,2.104802836,-6.486975471));
#125603=CARTESIAN_POINT('Ctrl Pts',(-2.79965669405202,1.96978752926819,
-6.95849183810364));
#125604=CARTESIAN_POINT('Ctrl Pts',(-2.81278208925584,1.97205380713406,
-6.95315330308681));
#125605=CARTESIAN_POINT('Ctrl Pts',(-2.82590748445965,1.974320085,-6.94781476807013));
#125606=CARTESIAN_POINT('Ctrl Pts',(-3.20662175498896,2.040055578,-6.79296560482468));
#125607=CARTESIAN_POINT('Ctrl Pts',(-3.56813707398421,2.104802836,-6.59744503541926));
#125608=CARTESIAN_POINT('',(-2.8252536488491,1.97432008541403,-6.94751335411902));
#125609=CARTESIAN_POINT('',(-3.34328826125575,2.06488542556126,-6.71359988234816));
#125610=CARTESIAN_POINT('Origin',(0.0561901580705221,1.87505115267705,0.180407822666179));
#125611=CARTESIAN_POINT('Ctrl Pts',(-3.23331887272832,2.1040344859088,-6.48907921578793));
#125612=CARTESIAN_POINT('Ctrl Pts',(-3.25157987960098,2.09719845374874,
-6.52646817427314));
#125613=CARTESIAN_POINT('Ctrl Pts',(-3.26988552728305,2.09052278109752,
-6.56389144244372));
#125614=CARTESIAN_POINT('Ctrl Pts',(-3.30653764310171,2.07748305174118,
-6.63871920671912));
#125615=CARTESIAN_POINT('Ctrl Pts',(-3.32490400174457,2.07111192520323,
-6.67616430152468));
#125616=CARTESIAN_POINT('Ctrl Pts',(-3.34328825817631,2.06488542586829,
-6.71359988391151));
#125617=CARTESIAN_POINT('',(-2.66730568478596,1.97432008626233,-6.87469859929897));
#125618=CARTESIAN_POINT('Origin',(2.41126563160776E-13,2.06597317199933,
3.90312782094782E-13));
#125619=CARTESIAN_POINT('',(-3.34188142941272,1.88359401257845,-6.71430029892486));
#125620=CARTESIAN_POINT('Origin',(0.0656246953443929,2.01784563381219,0.179955857994889));
#125621=CARTESIAN_POINT('',(-3.83857780625906,1.97432008362732,-6.44323834739318));
#125622=CARTESIAN_POINT('Origin',(0.0845502529405523,1.87500220753361,0.172989665325833));
#125623=CARTESIAN_POINT('Origin',(0.0927466982508323,2.01785752670413,0.169323740462473));
#125624=CARTESIAN_POINT('Ctrl Pts',(-3.229124031,2.104810499,-6.491167691));
#125625=CARTESIAN_POINT('Ctrl Pts',(-3.581534681,2.039629277,-6.315855982));
#125626=CARTESIAN_POINT('Ctrl Pts',(-3.912894301,1.974320085,-6.103421843));
#125627=CARTESIAN_POINT('Ctrl Pts',(-3.118454975,2.104810499,-6.820941179));
#125628=CARTESIAN_POINT('Ctrl Pts',(-3.488769289,2.039629277,-6.651637782));
#125629=CARTESIAN_POINT('Ctrl Pts',(-3.838577816,1.974320085,-6.443238343));
#125630=CARTESIAN_POINT('',(-3.87573604768088,1.97432008293108,-6.27333009968417));
#125631=CARTESIAN_POINT('Ctrl Pts',(-3.88983386359933,1.96978752926216,
-6.11820585377211));
#125632=CARTESIAN_POINT('Ctrl Pts',(-3.90136408229967,1.97205380713105,
-6.11081384838606));
#125633=CARTESIAN_POINT('Ctrl Pts',(-3.912894301,1.974320085,-6.103421843));
#125634=CARTESIAN_POINT('Ctrl Pts',(-4.247338996,2.040055578,-5.889009866));
#125635=CARTESIAN_POINT('Ctrl Pts',(-4.556353671,2.104802836,-5.639338722));
#125636=CARTESIAN_POINT('Ctrl Pts',(-4.23007233002474,1.96978752926216,
-6.19396273380434));
#125637=CARTESIAN_POINT('Ctrl Pts',(-4.24174323357281,1.97205380713104,
-6.1859274387742));
#125638=CARTESIAN_POINT('Ctrl Pts',(-4.25341413712091,1.974320085,-6.17789214374396));
#125639=CARTESIAN_POINT('Ctrl Pts',(-4.59193952670449,2.040055578,-5.94482095355561));
#125640=CARTESIAN_POINT('Ctrl Pts',(-4.90297167475003,2.104802836,-5.67615643917303));
#125641=CARTESIAN_POINT('',(-4.25271079273639,1.97432008541403,-6.1777383320139));
#125642=CARTESIAN_POINT('',(-4.70834956143689,2.0648854255707,-5.83793149851878));
#125643=CARTESIAN_POINT('Origin',(0.093658769871397,1.87505117108866,0.164110696979646));
#125644=CARTESIAN_POINT('Ctrl Pts',(-4.55268589017149,2.10403448591427,
-5.64230016841548));
#125645=CARTESIAN_POINT('Ctrl Pts',(-4.57855748566152,2.09719845371626,
-5.67488941724997));
#125646=CARTESIAN_POINT('Ctrl Pts',(-4.60448005358777,2.0905227811132,-5.70750257679646));
#125647=CARTESIAN_POINT('Ctrl Pts',(-4.6563610206253,2.07748305174171,-5.77270178809585));
#125648=CARTESIAN_POINT('Ctrl Pts',(-4.68234757248036,2.07111192520591,
-5.80532321318402));
#125649=CARTESIAN_POINT('Ctrl Pts',(-4.70834955878,2.06488542588462,-5.83793150069733));
#125650=CARTESIAN_POINT('',(-4.08280254455632,1.97432008626233,-6.14058008928434));
#125651=CARTESIAN_POINT('Origin',(-2.09034178855205E-13,2.06597317199922,
-3.12250225675825E-13));
#125652=CARTESIAN_POINT('',(-4.70712619026902,1.88359401258214,-5.83891796682442));
#125653=CARTESIAN_POINT('Origin',(0.102775484829765,2.01784565942823,0.161641054547004));
#125654=CARTESIAN_POINT('',(-5.13393977442981,1.97432008362732,-5.46741825438345));
#125655=CARTESIAN_POINT('Origin',(0.119761026372398,1.87500217170092,0.150769287710907));
#125656=CARTESIAN_POINT('Origin',(0.126977900188805,2.01785750701945,0.14542721135377));
#125657=CARTESIAN_POINT('Ctrl Pts',(-4.549038082,2.104810499,-5.645241583));
#125658=CARTESIAN_POINT('Ctrl Pts',(-4.855522731,2.039629277,-5.398270692));
#125659=CARTESIAN_POINT('Ctrl Pts',(-5.133468287,1.974320085,-5.119570621));
#125660=CARTESIAN_POINT('Ctrl Pts',(-4.511847958,2.104810499,-5.991095726));
#125661=CARTESIAN_POINT('Ctrl Pts',(-4.83710930400001,2.039629277,-5.746143917));
#125662=CARTESIAN_POINT('Ctrl Pts',(-5.133939783,1.974320085,-5.467418248));
#125663=CARTESIAN_POINT('',(-5.13370402587073,1.97432008293108,-5.29349444335369));
#125664=CARTESIAN_POINT('Ctrl Pts',(-5.11412511472685,1.96978752917448,
-5.13896630254029));
#125665=CARTESIAN_POINT('Ctrl Pts',(-5.12379670086343,1.97205380708721,
-5.12926846177013));
#125666=CARTESIAN_POINT('Ctrl Pts',(-5.133468287,1.974320085,-5.119570621));
#125667=CARTESIAN_POINT('Ctrl Pts',(-5.41400161399999,2.040055578,-4.83827575400001));
#125668=CARTESIAN_POINT('Ctrl Pts',(-5.66211978200001,2.104802836,-4.528012762));
#125669=CARTESIAN_POINT('Ctrl Pts',(-5.46269448542457,1.96978752917448,
-5.1398108166444));
#125670=CARTESIAN_POINT('Ctrl Pts',(-5.47236517900318,1.97205380708721,
-5.12945448288212));
#125671=CARTESIAN_POINT('Ctrl Pts',(-5.48203587258168,1.974320085,-5.11909814911986));
#125672=CARTESIAN_POINT('Ctrl Pts',(-5.76254331010755,2.040055578,-4.81870308208225));
#125673=CARTESIAN_POINT('Ctrl Pts',(-6.00854877035677,2.104802836,-4.4894570760898));
#125674=CARTESIAN_POINT('',(-5.48131591003525,1.97432008542256,-5.1190991295705));
#125675=CARTESIAN_POINT('',(-5.85325366966401,2.06488542555512,-4.68928792635981));
#125676=CARTESIAN_POINT('Origin',(0.12674794337641,1.87505114974812,0.140139938977898));
#125677=CARTESIAN_POINT('Ctrl Pts',(-5.65917437480889,2.10403448600368,
-4.53169343556461));
#125678=CARTESIAN_POINT('Ctrl Pts',(-5.69144666801797,2.09719848852933,
-4.55795900408713));
#125679=CARTESIAN_POINT('Ctrl Pts',(-5.72377386052729,2.09052285163215,
-4.5842369499391));
#125680=CARTESIAN_POINT('Ctrl Pts',(-5.78845813227907,2.07748305175775,
-4.63675924955608));
#125681=CARTESIAN_POINT('Ctrl Pts',(-5.82084977523512,2.07111192519836,
-4.6630316634958));
#125682=CARTESIAN_POINT('Ctrl Pts',(-5.85325366755331,2.06488542586541,
-4.68928792903829));
#125683=CARTESIAN_POINT('',(-5.30739209512797,1.97432008626233,-5.11933487856937));
#125684=CARTESIAN_POINT('Origin',(-3.62557206479153E-13,2.06597317200011,
-2.83193607453214E-13));
#125685=CARTESIAN_POINT('',(-5.85227096105508,1.88359401263917,-4.69051432075498));
#125686=CARTESIAN_POINT('Origin',(0.135120953411509,2.01784566648913,0.135768498711389));
#125687=CARTESIAN_POINT('',(-6.18924442501226,1.97432008362733,-4.23594776103393));
#125688=CARTESIAN_POINT('Origin',(0.149372346640306,1.87500214029896,0.121499565369763));
#125689=CARTESIAN_POINT('Origin',(0.15527189438599,2.01785750689169,0.114730801693088));
#125690=CARTESIAN_POINT('Ctrl Pts',(-5.656244168,2.104810499,-4.535350253));
#125691=CARTESIAN_POINT('Ctrl Pts',(-5.902471935,2.039629277,-4.228268264));
#125692=CARTESIAN_POINT('Ctrl Pts',(-6.114007001,1.974320085,-3.896333968));
#125693=CARTESIAN_POINT('Ctrl Pts',(-5.694271946,2.104810499,-4.881113296));
#125694=CARTESIAN_POINT('Ctrl Pts',(-5.959271464,2.039629277,-4.571966749));
#125695=CARTESIAN_POINT('Ctrl Pts',(-6.189244432,1.974320085,-4.235947753));
#125696=CARTESIAN_POINT('',(-6.15162570948745,1.97432008293108,-4.06614087110922));
#125697=CARTESIAN_POINT('Ctrl Pts',(-6.0992855593784,1.96978752911656,-3.91943439982929));
#125698=CARTESIAN_POINT('Ctrl Pts',(-6.10664628018919,1.97205380705825,
-3.90788418391467));
#125699=CARTESIAN_POINT('Ctrl Pts',(-6.114007001,1.974320085,-3.896333968));
#125700=CARTESIAN_POINT('Ctrl Pts',(-6.327511533,2.040055578,-3.561309246));
#125701=CARTESIAN_POINT('Ctrl Pts',(-6.503131465,2.104802836,-3.204961958));
#125702=CARTESIAN_POINT('Ctrl Pts',(-6.43988711735395,1.96978752911656,
-3.84532705777992));
#125703=CARTESIAN_POINT('Ctrl Pts',(-6.44710540996376,1.97205380705825,
-3.83313393594917));
#125704=CARTESIAN_POINT('Ctrl Pts',(-6.45432370257357,1.974320085,-3.82094081411849));
#125705=CARTESIAN_POINT('Ctrl Pts',(-6.66369697254378,2.040055578,-3.4672680099197));
#125706=CARTESIAN_POINT('Ctrl Pts',(-6.83317280303885,2.104802836,-3.09283569069017));
#125707=CARTESIAN_POINT('',(-6.45362078060153,1.97432008541403,-3.82109654502115));
#125708=CARTESIAN_POINT('',(-6.72446614117549,2.06488542555435,-3.32137846279023));
#125709=CARTESIAN_POINT('Origin',(0.153910537074243,1.875051149797,0.10961646125067));
#125710=CARTESIAN_POINT('Ctrl Pts',(-6.5010461556297,2.10403448604283,-3.20918975482682));
#125711=CARTESIAN_POINT('Ctrl Pts',(-6.53821023998976,2.09719849249568,
-3.22790364918131));
#125712=CARTESIAN_POINT('Ctrl Pts',(-6.5754305981183,2.09052285962829,-3.24661782843558));
#125713=CARTESIAN_POINT('Ctrl Pts',(-6.64989337486342,2.07748305175858,
-3.28400700247734));
#125714=CARTESIAN_POINT('Ctrl Pts',(-6.68717551143973,2.07111192520455,
-3.30270193622378));
#125715=CARTESIAN_POINT('Ctrl Pts',(-6.72446613966908,2.06488542585766,
-3.32137846589913));
#125716=CARTESIAN_POINT('',(-6.28381388945082,1.97432008626233,-3.85871525909399));
#125717=CARTESIAN_POINT('Origin',(-7.48099499014998E-13,2.06597317199967,
-4.36282954208167E-13));
#125718=CARTESIAN_POINT('',(-6.7237700463037,1.88359401261698,-3.32278743789529));
#125719=CARTESIAN_POINT('Origin',(0.161148139917844,2.01784564836717,0.103547310673459));
#125720=CARTESIAN_POINT('',(-6.95514688390034,1.97432008362734,-2.80640905739787));
#125721=CARTESIAN_POINT('Origin',(0.171998886078484,1.87500216690848,0.0865483033650638));
#125722=CARTESIAN_POINT('Origin',(0.176305524741013,2.01785750020066,0.0786696112267905));
#125723=CARTESIAN_POINT('Ctrl Pts',(-6.498970563,2.104810499,-3.213390985));
#125724=CARTESIAN_POINT('Ctrl Pts',(-6.673428112,2.039629277,-2.860556712));
#125725=CARTESIAN_POINT('Ctrl Pts',(-6.808661543,1.974320085,-2.490909068));
#125726=CARTESIAN_POINT('Ctrl Pts',(-6.61043810600001,2.104810499,-3.542895433));
#125727=CARTESIAN_POINT('Ctrl Pts',(-6.802784713,2.039629277,-3.184009497));
#125728=CARTESIAN_POINT('Ctrl Pts',(-6.955146889,1.974320085,-2.806409048));
#125729=CARTESIAN_POINT('',(-6.88190421143207,1.97432008293108,-2.64865906986868));
#125730=CARTESIAN_POINT('Ctrl Pts',(-6.79925019074248,1.96978752924164,
-2.51663409861818));
#125731=CARTESIAN_POINT('Ctrl Pts',(-6.80395586687118,1.97205380712079,
-2.50377158330912));
#125732=CARTESIAN_POINT('Ctrl Pts',(-6.80866154300001,1.974320085,-2.490909068));
#125733=CARTESIAN_POINT('Ctrl Pts',(-6.945154046,2.040055578,-2.117819875));
#125734=CARTESIAN_POINT('Ctrl Pts',(-7.040063948,2.104802836,-1.732050695));
#125735=CARTESIAN_POINT('Ctrl Pts',(-7.11595778587165,1.96978752924164,
-2.37104007871296));
#125736=CARTESIAN_POINT('Ctrl Pts',(-7.12038615790618,1.97205380712079,
-2.35758030613505));
#125737=CARTESIAN_POINT('Ctrl Pts',(-7.12481452994075,1.974320085,-2.34412053355715));
#125738=CARTESIAN_POINT('Ctrl Pts',(-7.25326357034823,2.040055578,-1.9537073392189));
#125739=CARTESIAN_POINT('Ctrl Pts',(-7.3382852704879,2.104802836,-1.55159674539325));
#125740=CARTESIAN_POINT('',(-7.12416152133647,1.97432008542256,-2.34442372779283));
#125741=CARTESIAN_POINT('',(-7.28125004982754,2.06488542555286,-1.79816503360501));
#125742=CARTESIAN_POINT('Origin',(0.173876656861732,1.87505112352018,0.0739675246104965));
#125743=CARTESIAN_POINT('Ctrl Pts',(-7.03893624352271,2.10403448598341,
-1.73662792835122));
#125744=CARTESIAN_POINT('Ctrl Pts',(-7.07925461425185,2.09719845379898,
-1.74691518076445));
#125745=CARTESIAN_POINT('Ctrl Pts',(-7.11962803445628,2.09052278112076,
-1.75719062130498));
#125746=CARTESIAN_POINT('Ctrl Pts',(-7.20038699405701,2.07748305173764,
-1.77769823778878));
#125747=CARTESIAN_POINT('Ctrl Pts',(-7.24081635312325,2.07111192519368,
-1.78794153699519));
#125748=CARTESIAN_POINT('Ctrl Pts',(-7.2812500490213,2.06488542585132,-1.79816503697546));
#125749=CARTESIAN_POINT('',(-6.966411530463,1.97432008626233,-2.41766640231028));
#125750=CARTESIAN_POINT('Origin',(8.06646416329215E-14,2.06597317199956,
8.67361737988404E-15));
#125751=CARTESIAN_POINT('',(-7.2808731171701,1.88359401257591,-1.79969070725037));
#125752=CARTESIAN_POINT('Origin',(0.179640001142697,2.01784567761325,0.0664842918032968));
#125753=CARTESIAN_POINT('',(-7.39583440602958,1.97432008362734,-1.24564578622645));
#125754=CARTESIAN_POINT('Origin',(0.186582973207047,1.87500218005872,0.0475501875908102));
#125755=CARTESIAN_POINT('Origin',(0.189095318358905,2.0178574927992,0.0389299101556073));
#125756=CARTESIAN_POINT('Ctrl Pts',(-7.037812317,2.104810499,-1.741177127));
#125757=CARTESIAN_POINT('Ctrl Pts',(-7.132342206,2.039629277,-1.359088706));
#125758=CARTESIAN_POINT('Ctrl Pts',(-7.184950639,1.974320085,-0.969012029));
#125759=CARTESIAN_POINT('Ctrl Pts',(-7.217507527,2.104810499,-2.039015717));
#125760=CARTESIAN_POINT('Ctrl Pts',(-7.32820731,2.039629277,-1.6471715));
#125761=CARTESIAN_POINT('Ctrl Pts',(-7.39583440900001,1.974320085,-1.245645776));
#125762=CARTESIAN_POINT('',(-7.29039252209028,1.97432008293108,-1.10732891507316));
#125763=CARTESIAN_POINT('Ctrl Pts',(-7.18128944022013,1.96978752940308,
-0.996158784306705));
#125764=CARTESIAN_POINT('Ctrl Pts',(-7.18312003961001,1.97205380720151,
-0.982585406653354));
#125765=CARTESIAN_POINT('Ctrl Pts',(-7.18495063900001,1.974320085,-0.969012029));
#125766=CARTESIAN_POINT('Ctrl Pts',(-7.238048875,2.040055578,-0.5753036));
#125767=CARTESIAN_POINT('Ctrl Pts',(-7.247810865,2.104802836,-0.178150666));
#125768=CARTESIAN_POINT('Ctrl Pts',(-7.45929417670702,1.96978752940307,
-0.785885901131069));
#125769=CARTESIAN_POINT('Ctrl Pts',(-7.46072556256693,1.97205380720151,
-0.771788841946397));
#125770=CARTESIAN_POINT('Ctrl Pts',(-7.46215694842695,1.974320085,-0.757691782761731));
#125771=CARTESIAN_POINT('Ctrl Pts',(-7.50367562510637,2.040055578,-0.348793484426639));
#125772=CARTESIAN_POINT('Ctrl Pts',(-7.50026767388759,2.104802836,0.0621931387486895));
#125773=CARTESIAN_POINT('',(-7.4615843846223,1.97432008542257,-0.75812826601158));
#125774=CARTESIAN_POINT('',(-7.4975707984158,2.06488542435384,-0.190871407260673));
#125775=CARTESIAN_POINT('Origin',(0.185712462960369,1.8750511548578,0.0348598629889121));
#125776=CARTESIAN_POINT('Ctrl Pts',(-7.24769349606498,2.10403448591232,
-0.182863309195361));
#125777=CARTESIAN_POINT('Ctrl Pts',(-7.28928070105476,2.09719845372094,
-0.184242793533437));
#125778=CARTESIAN_POINT('Ctrl Pts',(-7.33091912871676,2.09052278112048,
-0.185598908102442));
#125779=CARTESIAN_POINT('Ctrl Pts',(-7.41419852012812,2.07748305174943,
-0.18826627887279));
#125780=CARTESIAN_POINT('Ctrl Pts',(-7.45588466985395,2.0711119252019,-0.189578978335218));
#125781=CARTESIAN_POINT('Ctrl Pts',(-7.49757079858528,2.06488542588253,
-0.190871409159069));
#125782=CARTESIAN_POINT('',(-7.32326751109381,1.97432008626233,-0.86357015218475));
#125783=CARTESIAN_POINT('Ctrl Pts',(-7.24757379,2.104810499,-0.187547762));
#125784=CARTESIAN_POINT('Ctrl Pts',(-7.25775590700001,2.039629277,0.205928776));
#125785=CARTESIAN_POINT('Ctrl Pts',(-7.225279428,1.974320085,0.598194935));
#125786=CARTESIAN_POINT('Ctrl Pts',(-7.487094318,2.104810499,-0.439793892));
#125787=CARTESIAN_POINT('Ctrl Pts',(-7.510971078,2.039629277,-0.033313594));
#125788=CARTESIAN_POINT('Ctrl Pts',(-7.490700931,1.974320085,0.373362509));
#125789=CARTESIAN_POINT('',(-7.4907009161437,1.97432008293385,0.373362508483209));
#125790=CARTESIAN_POINT('Origin',(0.193037880697701,2.01785620729277,-0.00263048357573647));
#125791=CARTESIAN_POINT('',(-7.35799018033779,1.97432008293106,0.485778709310116));
#125792=CARTESIAN_POINT('Origin',(1.67097238823466E-12,2.06597317199989,
6.95515693649451E-14));
#125793=CARTESIAN_POINT('',(-7.49753065369832,1.88359401161432,-0.19244243844303));
#125794=CARTESIAN_POINT('Origin',(0.189732461945215,2.01784566286124,0.0263126490594483));
#125795=CARTESIAN_POINT('Origin',(0.19243733327029,1.87500051292121,0.00632878849069943));
#125796=CARTESIAN_POINT('Ctrl Pts',(-7.22753957590222,1.96978752942611,
0.570895806364564));
#125797=CARTESIAN_POINT('Ctrl Pts',(-7.22640950195114,1.97205380721309,
0.584545370682287));
#125798=CARTESIAN_POINT('Ctrl Pts',(-7.225279428,1.974320085,0.598194935));
#125799=CARTESIAN_POINT('Ctrl Pts',(-7.192500583,2.040055578,0.994113231));
#125800=CARTESIAN_POINT('Ctrl Pts',(-7.116658202,2.104802836,1.38407949));
#125801=CARTESIAN_POINT('Ctrl Pts',(-7.45384226286143,1.96978752942612,
0.836015428168855));
#125802=CARTESIAN_POINT('Ctrl Pts',(-7.4522097326846,1.97205380721309,0.850090611511704));
#125803=CARTESIAN_POINT('Ctrl Pts',(-7.45057720250766,1.974320085,0.864165794854558));
#125804=CARTESIAN_POINT('Ctrl Pts',(-7.40322414780391,2.040055578,1.27242956615732));
#125805=CARTESIAN_POINT('Ctrl Pts',(-7.31154589716983,2.104802836,1.67307494163324));
#125806=CARTESIAN_POINT('',(-7.45011185591378,1.97432008542257,0.863616432006661));
#125807=CARTESIAN_POINT('',(-7.337695642267,1.97432008626236,0.730905678799971));
#125808=CARTESIAN_POINT('',(-7.36331346990707,2.06488542554735,1.4253471567595));
#125809=CARTESIAN_POINT('Origin',(0.188864511309988,1.87505115067447,-0.00587784889222384));
#125810=CARTESIAN_POINT('Ctrl Pts',(-7.11755665585574,2.10403448593754,
1.37945179480568));
#125811=CARTESIAN_POINT('Ctrl Pts',(-7.15846812337888,2.09719845374601,
1.38704458172499));
#125812=CARTESIAN_POINT('Ctrl Pts',(-7.19942459243104,2.09052278110782,
1.39467120347564));
#125813=CARTESIAN_POINT('Ctrl Pts',(-7.28133036377528,2.07748305171712,
1.40996880174503));
#125814=CARTESIAN_POINT('Ctrl Pts',(-7.3223241059206,2.07111192517997,1.41764808240219));
#125815=CARTESIAN_POINT('Ctrl Pts',(-7.36331347059013,2.06488542584423,
1.42534715336305));
#125816=CARTESIAN_POINT('Origin',(7.27282817303276E-13,2.06597317200033,
-1.77321265310004E-13));
#125817=CARTESIAN_POINT('',(-7.23531060460637,1.97432008362732,1.97491276746511));
#125818=CARTESIAN_POINT('Origin',(0.18796447481838,2.01785751978077,-0.0440672207483484));
#125819=CARTESIAN_POINT('',(-7.36361198950017,1.88359401260101,1.423804222735));
#125820=CARTESIAN_POINT('Origin',(0.190953218088885,2.01784568550177,-0.0150894238754196));
#125821=CARTESIAN_POINT('Origin',(0.189303689485433,1.87500217028609,-0.035188726902253));
#125822=CARTESIAN_POINT('Ctrl Pts',(-7.118446767,2.104810499,1.374851129));
#125823=CARTESIAN_POINT('Ctrl Pts',(-7.043805007,2.039629277,1.761317258));
#125824=CARTESIAN_POINT('Ctrl Pts',(-6.927762182,1.974320085,2.137430969));
#125825=CARTESIAN_POINT('Ctrl Pts',(-7.4065929,2.104810499,1.179992206));
#125826=CARTESIAN_POINT('Ctrl Pts',(-7.342530186,2.039629277,1.582102018));
#125827=CARTESIAN_POINT('Ctrl Pts',(-7.235310603,1.974320085,1.974912778));
#125828=CARTESIAN_POINT('',(-7.08153639604613,1.97432008293108,2.05617186128699));
#125829=CARTESIAN_POINT('Ctrl Pts',(-6.93583799508597,1.96978752918469,
2.11125594238362));
#125830=CARTESIAN_POINT('Ctrl Pts',(-6.93180008854293,1.97205380709238,
2.12434345569181));
#125831=CARTESIAN_POINT('Ctrl Pts',(-6.927762182,1.974320085,2.137430969));
#125832=CARTESIAN_POINT('Ctrl Pts',(-6.810638957,2.040055578,2.517046433));
#125833=CARTESIAN_POINT('Ctrl Pts',(-6.652738511,2.104802836,2.881591627));
#125834=CARTESIAN_POINT('Ctrl Pts',(-7.09985696869169,1.96978752918469,
2.41882560241395));
#125835=CARTESIAN_POINT('Ctrl Pts',(-7.09523685758261,1.97205380709238,
2.43222077080092));
#125836=CARTESIAN_POINT('Ctrl Pts',(-7.09061674647364,1.974320085,2.44561593918789));
#125837=CARTESIAN_POINT('Ctrl Pts',(-6.95660613795933,2.040055578,2.8341552241412));
#125838=CARTESIAN_POINT('Ctrl Pts',(-6.78094436032466,2.104802836,3.20572561953813));
#125839=CARTESIAN_POINT('',(-7.09028037660616,1.97432008541402,2.44497938066934));
#125840=CARTESIAN_POINT('',(-6.88475578729827,2.06488542555484,2.97491807055449));
#125841=CARTESIAN_POINT('Origin',(0.183185163030007,1.87505116189093,-0.0463406174919131));
#125842=CARTESIAN_POINT('Ctrl Pts',(-6.65461077690117,2.10403448600761,
2.87726526592325));
#125843=CARTESIAN_POINT('Ctrl Pts',(-6.69293353219664,2.0971984538097,2.89347529398928));
#125844=CARTESIAN_POINT('Ctrl Pts',(-6.73129296363881,2.09052278114379,
2.90972803985757));
#125845=CARTESIAN_POINT('Ctrl Pts',(-6.80799529212629,2.07748305175425,
2.94227530853572));
#125846=CARTESIAN_POINT('Ctrl Pts',(-6.84637980517642,2.0711119251996,2.95858749470928));
#125847=CARTESIAN_POINT('Ctrl Pts',(-6.88475578868484,2.06488542586237,
2.97491806741338));
#125848=CARTESIAN_POINT('',(-7.00902128040429,1.97432008626232,2.29120517214505));
#125849=CARTESIAN_POINT('Origin',(6.34475111338517E-13,2.06597317200078,
-3.15285991758785E-13));
#125850=CARTESIAN_POINT('',(-6.88537901244729,1.88359401260015,2.97347538228458));
#125851=CARTESIAN_POINT('Origin',(0.18324471553533,2.01784562527804,-0.0557858145456952));
#125852=CARTESIAN_POINT('',(-6.6416051968254,1.97432008362727,3.48411831007128));
#125853=CARTESIAN_POINT('Origin',(0.177313480385554,1.87500217804533,-0.0750607933144437));
#125854=CARTESIAN_POINT('Origin',(0.174096740851528,2.01785756261903,-0.0834437133487326));
#125855=CARTESIAN_POINT('Ctrl Pts',(-6.656469085,2.104810499,2.872963509));
#125856=CARTESIAN_POINT('Ctrl Pts',(-6.50049361399999,2.039629277,3.234348502));
#125857=CARTESIAN_POINT('Ctrl Pts',(-6.306310476,1.974320085,3.576723107));
#125858=CARTESIAN_POINT('Ctrl Pts',(-6.97976743,2.104810499,2.744603181));
#125859=CARTESIAN_POINT('Ctrl Pts',(-6.830760744,2.039629277,3.123540298));
#125860=CARTESIAN_POINT('Ctrl Pts',(-6.641605193,1.974320085,3.48411832));
#125861=CARTESIAN_POINT('',(-6.47395784058873,1.97432008293106,3.53042070233472));
#125862=CARTESIAN_POINT('Ctrl Pts',(-6.31982433767558,1.96978752932471,
3.55289609980211));
#125863=CARTESIAN_POINT('Ctrl Pts',(-6.31306740683774,1.97205380716239,
3.56480960340106));
#125864=CARTESIAN_POINT('Ctrl Pts',(-6.306310476,1.974320085,3.576723107));
#125865=CARTESIAN_POINT('Ctrl Pts',(-6.110319423,2.040055578,3.922285341));
#125866=CARTESIAN_POINT('Ctrl Pts',(-5.877744161,2.104802836,4.244363742));
#125867=CARTESIAN_POINT('Ctrl Pts',(-6.41389025301481,1.96978752932471,
3.88853418294504));
#125868=CARTESIAN_POINT('Ctrl Pts',(-6.40649859251036,1.97205380716239,
3.90062299204184));
#125869=CARTESIAN_POINT('Ctrl Pts',(-6.39910693200597,1.974320085,3.9127118011387));
#125870=CARTESIAN_POINT('Ctrl Pts',(-6.18470495565525,2.040055578,4.26335893388342));
#125871=CARTESIAN_POINT('Ctrl Pts',(-5.9332734024071,2.104802836,4.58848012970813));
#125872=CARTESIAN_POINT('',(-6.39891526755264,1.97432008541402,3.91201781545349));
#125873=CARTESIAN_POINT('',(-6.08427457567457,2.0648854255748,4.38538512164169));
#125874=CARTESIAN_POINT('Origin',(0.168940651985443,1.87505118558091,-0.0846366779811158));
#125875=CARTESIAN_POINT('Ctrl Pts',(-5.88050269401229,2.10403448603753,
4.24054101089173));
#125876=CARTESIAN_POINT('Ctrl Pts',(-5.91444480773726,2.09719845385691,
4.26461031715442));
#125877=CARTESIAN_POINT('Ctrl Pts',(-5.94841355701859,2.09052278120813,
4.28872922672933));
#125878=CARTESIAN_POINT('Ctrl Pts',(-6.01632592706529,2.07748305181364,
4.33700429176202));
#125879=CARTESIAN_POINT('Ctrl Pts',(-6.050306393732,2.07111192524561,4.36118664380401));
#125880=CARTESIAN_POINT('Ctrl Pts',(-6.08427457769155,2.06488542589445,
4.38538511889264));
#125881=CARTESIAN_POINT('',(-6.35261287342917,1.97432008626232,3.74437045883386));
#125882=CARTESIAN_POINT('Origin',(3.33934269125535E-14,2.06597317200022,
-1.17093834628434E-13));
#125883=CARTESIAN_POINT('',(-6.08519336544764,1.88359401258516,4.38411013764511));
#125884=CARTESIAN_POINT('Origin',(0.16696819574831,2.01784563268764,-0.0938737286868618));
#125885=CARTESIAN_POINT('',(-5.73734571087834,1.97432008362714,4.83041035311533));
#125886=CARTESIAN_POINT('Origin',(0.157031971549915,1.87500216085911,-0.111422941102539));
#125887=CARTESIAN_POINT('Origin',(0.152088705016516,2.01785751253689,-0.118918655078524));
#125888=CARTESIAN_POINT('Ctrl Pts',(-5.88324230700001,2.104810499,4.236739308));
#125889=CARTESIAN_POINT('Ctrl Pts',(-5.653226364,2.039629277,4.556145206));
#125890=CARTESIAN_POINT('Ctrl Pts',(-5.3899827,1.974320085,4.848771648));
#125891=CARTESIAN_POINT('Ctrl Pts',(-6.22657579300001,2.104810499,4.180879561));
#125892=CARTESIAN_POINT('Ctrl Pts',(-5.99959252,2.039629277,4.518925306));
#125893=CARTESIAN_POINT('Ctrl Pts',(-5.737345705,1.974320085,4.830410362));
#125894=CARTESIAN_POINT('',(-5.5636642108475,1.97432008293083,4.8395909954036));
#125895=CARTESIAN_POINT('Ctrl Pts',(-5.40830271781122,1.96978752917624,
4.82840678318885));
#125896=CARTESIAN_POINT('Ctrl Pts',(-5.39914270890567,1.97205380708815,
4.83858921559444));
#125897=CARTESIAN_POINT('Ctrl Pts',(-5.3899827,1.974320085,4.848771648));
#125898=CARTESIAN_POINT('Ctrl Pts',(-5.12428814500001,2.040055578,5.144122545));
#125899=CARTESIAN_POINT('Ctrl Pts',(-4.827913027,2.104802836,5.408674126));
#125900=CARTESIAN_POINT('Ctrl Pts',(-5.42801715832236,1.96978752917623,
5.17641922496828));
#125901=CARTESIAN_POINT('Ctrl Pts',(-5.41819957382225,1.97205380708815,
5.18663641624999));
#125902=CARTESIAN_POINT('Ctrl Pts',(-5.40838198932213,1.974320085,5.1968536075316));
#125903=CARTESIAN_POINT('Ctrl Pts',(-5.12361384424682,2.040055578,5.493212717974));
#125904=CARTESIAN_POINT('Ctrl Pts',(-4.80816917351054,2.104802836,5.7566824093551));
#125905=CARTESIAN_POINT('',(-5.40834399228508,1.97432008541403,5.19613464466293));
#125906=CARTESIAN_POINT('',(-4.99929944699896,2.0648854255675,5.59079643827862));
#125907=CARTESIAN_POINT('Origin',(0.146796408726788,1.87505116076644,-0.1189750306459));
#125908=CARTESIAN_POINT('Ctrl Pts',(-4.83142884124745,2.10403448603426,
5.40553377141309));
#125909=CARTESIAN_POINT('Ctrl Pts',(-4.85940321785624,2.09719845384183,
5.43633690176658));
#125910=CARTESIAN_POINT('Ctrl Pts',(-4.88739294396725,2.09052278119847,
5.46719420155808));
#125911=CARTESIAN_POINT('Ctrl Pts',(-4.94333984845768,2.07748305180029,
5.52893977444882));
#125912=CARTESIAN_POINT('Ctrl Pts',(-4.97132737977632,2.0711119252313,5.55986155241276));
#125913=CARTESIAN_POINT('Ctrl Pts',(-4.99929944955791,2.06488542588397,
5.59079643602845));
#125914=CARTESIAN_POINT('',(-5.39916334827033,1.97432008626232,5.02245314433436));
#125915=CARTESIAN_POINT('Origin',(-5.5424415057459E-13,2.065973171999,6.82180006927879E-13));
#125916=CARTESIAN_POINT('',(-5.00047084026875,1.88359401262509,5.58974877539356));
#125917=CARTESIAN_POINT('Origin',(0.14288452164617,2.01784567409964,-0.127572246574718));
#125918=CARTESIAN_POINT('',(-4.56481431668053,1.97432008362732,5.95083777557622));
#125919=CARTESIAN_POINT('Origin',(0.129407994727996,1.87500218148817,-0.142575166280723));
#125920=CARTESIAN_POINT('Origin',(0.12296869673353,2.01785750439565,-0.148832672745743));
#125921=CARTESIAN_POINT('Ctrl Pts',(-4.834921657,2.104810499,5.402409886));
#125922=CARTESIAN_POINT('Ctrl Pts',(-4.541620533,2.039629277,5.664901623));
#125923=CARTESIAN_POINT('Ctrl Pts',(-4.221625324,1.974320085,5.894097015));
#125924=CARTESIAN_POINT('Ctrl Pts',(-5.182236391,2.104810499,5.421662659));
#125925=CARTESIAN_POINT('Ctrl Pts',(-4.887890019,2.039629277,5.70301038900001));
#125926=CARTESIAN_POINT('Ctrl Pts',(-4.564814309,1.974320085,5.950837783));
#125927=CARTESIAN_POINT('',(-4.39321982671405,1.97432008293108,5.92246739142333));
#125928=CARTESIAN_POINT('Ctrl Pts',(-4.24389487418159,1.96978752913463,
5.87814653153815));
#125929=CARTESIAN_POINT('Ctrl Pts',(-4.23276009909078,1.97205380706735,
5.88612177326912));
#125930=CARTESIAN_POINT('Ctrl Pts',(-4.221625324,1.974320085,5.894097015));
#125931=CARTESIAN_POINT('Ctrl Pts',(-3.898650847,2.040055578,6.125426297));
#125932=CARTESIAN_POINT('Ctrl Pts',(-3.552334045,2.104802836,6.32008092));
#125933=CARTESIAN_POINT('Ctrl Pts',(-4.18833601474106,1.96978752913463,
6.22226065806384));
#125934=CARTESIAN_POINT('Ctrl Pts',(-4.17655156568981,1.97205380706735,
6.23012848670628));
#125935=CARTESIAN_POINT('Ctrl Pts',(-4.1647671166385,1.974320085,6.23799631534876));
#125936=CARTESIAN_POINT('Ctrl Pts',(-3.82294824395876,2.040055578,6.46620998111279));
#125937=CARTESIAN_POINT('Ctrl Pts',(-3.4582402984613,2.104802836,6.6557086175373));
#125938=CARTESIAN_POINT('',(-4.16488456114592,1.97432008542257,6.23728599583473));
#125939=CARTESIAN_POINT('',(-3.6805626329654,2.06488542554733,6.5347883272354));
#125940=CARTESIAN_POINT('Origin',(0.117788238628589,1.87505116461688,-0.147750294515482));
#125941=CARTESIAN_POINT('Ctrl Pts',(-3.55644274524795,2.10403448598181,
6.31776978077794));
#125942=CARTESIAN_POINT('Ctrl Pts',(-3.57714133401449,2.09719845378938,
6.35386641504643));
#125943=CARTESIAN_POINT('Ctrl Pts',(-3.59784326874741,2.09052278111202,
6.39001925219844));
#125944=CARTESIAN_POINT('Ctrl Pts',(-3.63920869287107,2.07748305173078,
6.46234817845479));
#125945=CARTESIAN_POINT('Ctrl Pts',(-3.65989462309973,2.07111192518344,
6.49856351423839));
#125946=CARTESIAN_POINT('Ctrl Pts',(-3.68056263598081,2.06488542584907,
6.53478832556683));
#125947=CARTESIAN_POINT('',(-4.19325494636506,1.97432008626232,6.06569150259979));
#125948=CARTESIAN_POINT('Origin',(-2.54787510534094E-13,2.06597317199889,
4.4799233767101E-13));
#125949=CARTESIAN_POINT('',(-3.68193185568052,1.88359401262617,6.53401697296669));
#125950=CARTESIAN_POINT('Origin',(0.112119777202641,2.01784565321898,-0.155305776233697));
#125951=CARTESIAN_POINT('',(-3.17883727810966,1.97432008362732,6.79301063840171));
#125952=CARTESIAN_POINT('Origin',(0.0957330760861524,1.87500219779642,-0.167060764696217));
#125953=CARTESIAN_POINT('Origin',(0.0880991938531066,2.01785752956562,-0.171787801691451));
#125954=CARTESIAN_POINT('Ctrl Pts',(-3.560525444,2.104810499,6.315469782));
#125955=CARTESIAN_POINT('Ctrl Pts',(-3.217653573,2.039629277,6.508773536));
#125956=CARTESIAN_POINT('Ctrl Pts',(-2.85586944,1.974320085,6.663820956));
#125957=CARTESIAN_POINT('Ctrl Pts',(-3.895581376,2.104810499,6.408934837));
#125958=CARTESIAN_POINT('Ctrl Pts',(-3.547635213,2.039629277,6.62042904400001));
#125959=CARTESIAN_POINT('Ctrl Pts',(-3.178837269,1.974320085,6.793010644));
#125960=CARTESIAN_POINT('',(-3.01735336610401,1.97432008293108,6.72841579479619));
#125961=CARTESIAN_POINT('Ctrl Pts',(-2.88104722229099,1.96978752923893,
6.65303068119339));
#125962=CARTESIAN_POINT('Ctrl Pts',(-2.86845833114553,1.9720538071195,6.65842581859663));
#125963=CARTESIAN_POINT('Ctrl Pts',(-2.85586944,1.974320085,6.663820956));
#125964=CARTESIAN_POINT('Ctrl Pts',(-2.49071697,2.040055578,6.82031192300001));
#125965=CARTESIAN_POINT('Ctrl Pts',(-2.110651872,2.104802836,6.935967753));
#125966=CARTESIAN_POINT('Ctrl Pts',(-2.7528129322015,1.96978752923893,6.97715609885582));
#125967=CARTESIAN_POINT('Ctrl Pts',(-2.73961264674685,1.9720538071195,6.98230667369879));
#125968=CARTESIAN_POINT('Ctrl Pts',(-2.72641236129213,1.974320085,6.9874572485419));
#125969=CARTESIAN_POINT('Ctrl Pts',(-2.34352583198828,2.040055578,7.13685445153059));
#125970=CARTESIAN_POINT('Ctrl Pts',(-1.94660795094088,2.104802836,7.24352128796493));
#125971=CARTESIAN_POINT('',(-2.72667975770036,1.97432008542256,6.98678878301995));
#125972=CARTESIAN_POINT('',(-2.18972680033077,2.06488542555802,7.17322077696606));
#125973=CARTESIAN_POINT('Origin',(0.0832725217709313,1.87505115884544,-0.169617116136719));
#125974=CARTESIAN_POINT('Ctrl Pts',(-2.11516133959159,2.10403448594589,
6.93459389664791));
#125975=CARTESIAN_POINT('Ctrl Pts',(-2.12761629754393,2.09719845375242,
6.97429619653596));
#125976=CARTESIAN_POINT('Ctrl Pts',(-2.14006244105225,2.09052278115065,
7.0140541040936));
#125977=CARTESIAN_POINT('Ctrl Pts',(-2.16491218327615,2.07748305176128,
7.09358436382901));
#125978=CARTESIAN_POINT('Ctrl Pts',(-2.17732926116173,2.07111192520406,
7.13339986879836));
#125979=CARTESIAN_POINT('Ctrl Pts',(-2.18972680358998,2.06488542587125,
7.17322077600033));
#125980=CARTESIAN_POINT('',(-2.79127460316217,1.97432008626232,6.82530486757097));
#125981=CARTESIAN_POINT('Origin',(-4.86481514794246E-13,2.06597317199956,
1.71217207078911E-12));
#125982=CARTESIAN_POINT('',(-2.19122982986192,1.88359401259214,7.17276179905091));
#125983=CARTESIAN_POINT('Origin',(0.0761123067457722,2.01784568248533,-0.17577716954979));
#125984=CARTESIAN_POINT('',(-1.6442213420479,1.97432008362732,7.31754987448154));
#125985=CARTESIAN_POINT('Origin',(0.0575818226720837,1.87500221280571,-0.183734943946949));
#125986=CARTESIAN_POINT('Origin',(0.0491101563790857,2.01785750222948,-0.186710084026774));
#125987=CARTESIAN_POINT('Ctrl Pts',(-2.119643019,2.104810499,6.93322533));
#125988=CARTESIAN_POINT('Ctrl Pts',(-1.743232708,2.039629277,7.048302433));
#125989=CARTESIAN_POINT('Ctrl Pts',(-1.356576276,1.974320085,7.121952036));
#125990=CARTESIAN_POINT('Ctrl Pts',(-2.426773305,2.104810499,7.096532345));
#125991=CARTESIAN_POINT('Ctrl Pts',(-2.041496927,2.039629277,7.228283796));
#125992=CARTESIAN_POINT('Ctrl Pts',(-1.644221332,1.974320085,7.317549878));
#125993=CARTESIAN_POINT('',(-1.50039881645138,1.97432008293108,7.21975095441237));
#125994=CARTESIAN_POINT('Ctrl Pts',(-1.38348500528046,1.96978752935668,
7.11682651089333));
#125995=CARTESIAN_POINT('Ctrl Pts',(-1.37003064064024,1.97205380717837,
7.11938927344667));
#125996=CARTESIAN_POINT('Ctrl Pts',(-1.356576276,1.974320085,7.121952036));
#125997=CARTESIAN_POINT('Ctrl Pts',(-0.966319934,2.040055578,7.196287344));
#125998=CARTESIAN_POINT('Ctrl Pts',(-0.570277963,2.104802836,7.227536444));
#125999=CARTESIAN_POINT('Ctrl Pts',(-1.18857137701003,1.96978752935668,
7.40580747507847));
#126000=CARTESIAN_POINT('Ctrl Pts',(-1.17457248592774,1.97205380717837,
7.40799996110077));
#126001=CARTESIAN_POINT('Ctrl Pts',(-1.1605735948454,1.974320085,7.41019244712308));
#126002=CARTESIAN_POINT('Ctrl Pts',(-0.75452275766884,2.040055578,7.47378754044986));
#126003=CARTESIAN_POINT('Ctrl Pts',(-0.343954378698039,2.104802836,7.49263495404393));
#126004=CARTESIAN_POINT('',(-1.16097844002199,1.97432008542257,7.40959709227556));
#126005=CARTESIAN_POINT('',(-0.59650177670354,2.0648854255752,7.47624139567281));
#126006=CARTESIAN_POINT('Origin',(0.0448629872232868,1.87505114104151,-0.183552688534319));
#126007=CARTESIAN_POINT('Ctrl Pts',(-0.574977340857676,2.10403448596467,
7.22716410902309));
#126008=CARTESIAN_POINT('Ctrl Pts',(-0.578606266727296,2.09719849327752,
7.26861539947383));
#126009=CARTESIAN_POINT('Ctrl Pts',(-0.582214628220441,2.09052286129755,
7.31011907167483));
#126010=CARTESIAN_POINT('Ctrl Pts',(-0.589386786364929,2.07748305174417,
7.39313242856107));
#126011=CARTESIAN_POINT('Ctrl Pts',(-0.592954403264341,2.07111192522242,
7.43468637364651));
#126012=CARTESIAN_POINT('Ctrl Pts',(-0.596501780179169,2.06488542587664,
7.47624139542128));
#126013=CARTESIAN_POINT('',(-1.25877736262437,1.97432008626232,7.2657745631791));
#126014=CARTESIAN_POINT('Origin',(4.55364912443912E-14,2.06597317199933,
-1.16486681411843E-12));
#126015=CARTESIAN_POINT('',(-0.598068333136003,1.8835940126128,7.47611625540618));
#126016=CARTESIAN_POINT('Origin',(0.0365459521448464,2.01784563964012,-0.188029636822713));
#126017=CARTESIAN_POINT('',(-0.0327234426157351,1.97432008362731,7.49992860974549));
#126018=CARTESIAN_POINT('Origin',(0.016738008922914,1.87500216842685,-0.191817838129081));
#126019=CARTESIAN_POINT('Origin',(0.00782484507779792,2.01785753732395,
-0.192902388630886));
#126020=CARTESIAN_POINT('Ctrl Pts',(-0.579648442,2.104810499,7.226790967));
#126021=CARTESIAN_POINT('Ctrl Pts',(-0.18730022,2.039629277,7.258260542));
#126022=CARTESIAN_POINT('Ctrl Pts',(0.206148888,1.974320085,7.247068555));
#126023=CARTESIAN_POINT('Ctrl Pts',(-0.844492011,2.104810499,7.452303888));
#126024=CARTESIAN_POINT('Ctrl Pts',(-0.439900514,2.039629277,7.49815203));
#126025=CARTESIAN_POINT('Ctrl Pts',(-0.032723432,1.974320085,7.499928611));
#126026=CARTESIAN_POINT('',(0.0867127152835091,1.97432008293108,7.37349858314955));
#126027=CARTESIAN_POINT('Ctrl Pts',(-1.641510318,3.783915088,7.318158503));
#126028=CARTESIAN_POINT('Ctrl Pts',(-1.24377052,3.848090541,7.407374114));
#126029=CARTESIAN_POINT('Ctrl Pts',(-0.838704438,3.913265985,7.452957458));
#126030=CARTESIAN_POINT('Ctrl Pts',(-0.834644171981073,3.91391928492389,
7.45341437234286));
#126031=CARTESIAN_POINT('Ctrl Pts',(-0.830583905962144,3.91457258484778,
7.45387128668572));
#126032=CARTESIAN_POINT('Ctrl Pts',(-1.353937744,3.783915088,7.122454113));
#126033=CARTESIAN_POINT('Ctrl Pts',(-0.966834423,3.848090541,7.196040237));
#126034=CARTESIAN_POINT('Ctrl Pts',(-0.574036077,3.913265985,7.227238932));
#126035=CARTESIAN_POINT('Ctrl Pts',(-0.570098779241866,3.91391928492389,
7.2275516587544));
#126036=CARTESIAN_POINT('Ctrl Pts',(-0.56616148148373,3.91457258484778,
7.22786438550881));
#126037=CARTESIAN_POINT('',(-0.838704432778282,3.9132659845887,7.45295745868655));
#126038=CARTESIAN_POINT('',(-0.706370249897001,3.91326598377978,7.34009819573167));
#126039=CARTESIAN_POINT('',(-1.39529141150652,3.82362522065936,7.36906791091339));
#126040=CARTESIAN_POINT('Origin',(0.00437564016434397,4.01780065316102,
-0.188625706529489));
#126041=CARTESIAN_POINT('Ctrl Pts',(-1.34934427444366,3.78467661296189,
7.12332577189278));
#126042=CARTESIAN_POINT('Ctrl Pts',(-1.35687852219608,3.79148857314734,
7.16424520945549));
#126043=CARTESIAN_POINT('Ctrl Pts',(-1.36448261962806,3.79813536725102,
7.20520610145691));
#126044=CARTESIAN_POINT('Ctrl Pts',(-1.37979916234012,3.81110763474039,
7.28710522003744));
#126045=CARTESIAN_POINT('Ctrl Pts',(-1.38752070317403,3.81744080403857,
7.32809204393903));
#126046=CARTESIAN_POINT('Ctrl Pts',(-1.39529141290873,3.82362522065907,
7.36906791064074));
#126047=CARTESIAN_POINT('Ctrl Pts',(-1.95071269,3.913265985,7.241872686));
#126048=CARTESIAN_POINT('Ctrl Pts',(-1.887862343,3.903042157,7.258802419));
#126049=CARTESIAN_POINT('Ctrl Pts',(-1.824727629,3.892857143,7.274638759));
#126050=CARTESIAN_POINT('Ctrl Pts',(-1.48981453,3.838828313,7.358646393));
#126051=CARTESIAN_POINT('Ctrl Pts',(-1.148599349,3.783894965,7.411526127));
#126052=CARTESIAN_POINT('Ctrl Pts',(-2.114258167,3.913265985,6.934869314));
#126053=CARTESIAN_POINT('Ctrl Pts',(-2.054072224,3.903042157,6.95321841600001));
#126054=CARTESIAN_POINT('Ctrl Pts',(-1.993576877,3.892857143,6.970520155));
#126055=CARTESIAN_POINT('Ctrl Pts',(-1.672664928,3.838828313,7.06230134600001));
#126056=CARTESIAN_POINT('Ctrl Pts',(-1.344677418,3.783894965,7.124208212));
#126057=CARTESIAN_POINT('',(-1.95071268475464,3.91326598587933,7.24187268671574));
#126058=CARTESIAN_POINT('Ctrl Pts',(-1.39529140955773,3.82362522012815,
7.36906791137212));
#126059=CARTESIAN_POINT('Ctrl Pts',(-1.53971171293186,3.8468929357324,7.34172274220185));
#126060=CARTESIAN_POINT('Ctrl Pts',(-1.68297367235439,3.86998912007469,
7.31019548872055));
#126061=CARTESIAN_POINT('Ctrl Pts',(-1.82472762875061,3.89285714276327,
7.27463875947624));
#126062=CARTESIAN_POINT('Ctrl Pts',(-1.86677632062748,3.89964051914521,
7.26409151275274));
#126063=CARTESIAN_POINT('Ctrl Pts',(-1.90877464357573,3.90644394874722,
7.25316936065063));
#126064=CARTESIAN_POINT('Ctrl Pts',(-1.95071268604322,3.91326598565651,
7.24187268712382));
#126065=CARTESIAN_POINT('',(-2.03248542073876,3.91326598631302,7.08837100222542));
#126066=CARTESIAN_POINT('Origin',(2.18954628733448E-13,4.00453392000067,
-1.05080874557295E-12));
#126067=CARTESIAN_POINT('',(-1.40235121259848,4.0034549417923,7.36772767361413));
#126068=CARTESIAN_POINT('Origin',(0.058873471497646,4.16057200915549,-0.175368207921701));
#126069=CARTESIAN_POINT('Origin',(0.0336955573596309,4.01785438784316,-0.189448533857115));
#126070=CARTESIAN_POINT('Ctrl Pts',(-3.17697582940556,3.783915088,6.79445025702659));
#126071=CARTESIAN_POINT('Ctrl Pts',(-2.80769942346504,3.848090541,6.96711797440197));
#126072=CARTESIAN_POINT('Ctrl Pts',(-2.42188459324435,3.913265985,7.09874670216657));
#126073=CARTESIAN_POINT('Ctrl Pts',(-2.40874325520729,3.91548594253982,
7.10323014207464));
#126074=CARTESIAN_POINT('Ctrl Pts',(-2.39560191717029,3.91770590007956,
7.10771358198274));
#126075=CARTESIAN_POINT('Ctrl Pts',(-2.853400528,3.783915088,6.6648785));
#126076=CARTESIAN_POINT('Ctrl Pts',(-2.491166309,3.848090541,6.819959994));
#126077=CARTESIAN_POINT('Ctrl Pts',(-2.114258167,3.913265985,6.934869314));
#126078=CARTESIAN_POINT('Ctrl Pts',(-2.10142020195832,3.91548594253982,
6.93878326986547));
#126079=CARTESIAN_POINT('Ctrl Pts',(-2.08858223691657,3.91770590007957,
6.94269722573092));
#126080=CARTESIAN_POINT('',(-2.42126153214055,3.91326598502339,7.09841479422943));
#126081=CARTESIAN_POINT('',(-2.26775984623204,3.91326598377978,7.01664205534898));
#126082=CARTESIAN_POINT('',(-2.94680204673062,3.82362522067675,6.89683678909558));
#126083=CARTESIAN_POINT('Origin',(0.0448223164287281,4.0178006398365,-0.183275168909287));
#126084=CARTESIAN_POINT('Ctrl Pts',(-2.84910183290045,3.78467661312367,
6.6667172412568));
#126085=CARTESIAN_POINT('Ctrl Pts',(-2.86525640352458,3.79148857330945,
6.7050603647789));
#126086=CARTESIAN_POINT('Ctrl Pts',(-2.88148810208281,3.7981353673104,6.74342895726899));
#126087=CARTESIAN_POINT('Ctrl Pts',(-2.9140524396325,3.81110763381503,6.8201207104001));
#126088=CARTESIAN_POINT('Ctrl Pts',(-2.93040440790468,3.8174408020963,6.85848937555338));
#126089=CARTESIAN_POINT('Ctrl Pts',(-2.94680204808744,3.82362522067661,
6.89683678851494));
#126090=CARTESIAN_POINT('Ctrl Pts',(-3.46189467,3.913265985,6.653216162));
#126091=CARTESIAN_POINT('Ctrl Pts',(-3.404153122,3.903042157,6.683261053));
#126092=CARTESIAN_POINT('Ctrl Pts',(-3.345898807,3.892857143,6.712299246));
#126093=CARTESIAN_POINT('Ctrl Pts',(-3.036874949,3.838828313,6.866339244));
#126094=CARTESIAN_POINT('Ctrl Pts',(-2.715004769,3.783894965,6.991333857));
#126095=CARTESIAN_POINT('Ctrl Pts',(-3.555619896,3.913265985,6.318232914));
#126096=CARTESIAN_POINT('Ctrl Pts',(-3.500785581,3.903042157,6.34909122300001));
#126097=CARTESIAN_POINT('Ctrl Pts',(-3.445423944,3.892857143,6.378993169));
#126098=CARTESIAN_POINT('Ctrl Pts',(-3.15174498,3.838828313,6.53761515));
#126099=CARTESIAN_POINT('Ctrl Pts',(-2.844733783,3.783894965,6.668582286));
#126100=CARTESIAN_POINT('',(-3.46189466553809,3.9132659854451,6.65321616350949));
#126101=CARTESIAN_POINT('Ctrl Pts',(-2.946802044864,3.82362522012809,6.89683678997819));
#126102=CARTESIAN_POINT('Ctrl Pts',(-3.0819674786481,3.84689293573234,6.83908483956707));
#126103=CARTESIAN_POINT('Ctrl Pts',(-3.2151026252374,3.86998912007487,6.77749758928962));
#126104=CARTESIAN_POINT('Ctrl Pts',(-3.34589880719272,3.89285714303369,
6.71229924590394));
#126105=CARTESIAN_POINT('Ctrl Pts',(-3.38469707799573,3.89964051918897,
6.69295936222793));
#126106=CARTESIAN_POINT('Ctrl Pts',(-3.42336556352837,3.90644394833732,
6.67326416630459));
#126107=CARTESIAN_POINT('Ctrl Pts',(-3.46189466668291,3.91326598441267,
6.653216163726));
#126108=CARTESIAN_POINT('',(-3.50875727589861,3.91326598631302,6.48572454184184));
#126109=CARTESIAN_POINT('Origin',(4.07009495551058E-13,4.00453392000044,
-9.09428782280841E-13));
#126110=CARTESIAN_POINT('',(-2.95340868202953,4.00345494158478,6.89401023776217));
#126111=CARTESIAN_POINT('Origin',(0.0951960599535917,4.16057204517788,-0.158612234165763));
#126112=CARTESIAN_POINT('Origin',(0.0736336047404013,4.0178542574278,-0.177775727115013));
#126113=CARTESIAN_POINT('Ctrl Pts',(-4.56330586299524,3.783915088,5.95264389353416));
#126114=CARTESIAN_POINT('Ctrl Pts',(-4.23978138941415,3.848090541,6.2006582472807));
#126115=CARTESIAN_POINT('Ctrl Pts',(-3.89128298043124,3.913265985,6.41214835224929));
#126116=CARTESIAN_POINT('Ctrl Pts',(-3.8794126874205,3.91548594238702,6.41935197054465));
#126117=CARTESIAN_POINT('Ctrl Pts',(-3.86754239440971,3.91770589977398,
6.42655558883999));
#126118=CARTESIAN_POINT('Ctrl Pts',(-4.219441475,3.783915088,5.895660577));
#126119=CARTESIAN_POINT('Ctrl Pts',(-3.899014027,3.848090541,6.124986001));
#126120=CARTESIAN_POINT('Ctrl Pts',(-3.555619896,3.913265985,6.318232914));
#126121=CARTESIAN_POINT('Ctrl Pts',(-3.54392346110081,3.91548594238702,
6.32481514629033));
#126122=CARTESIAN_POINT('Ctrl Pts',(-3.53222702620162,3.91770589977399,
6.33139737858057));
#126123=CARTESIAN_POINT('',(-3.89060313579128,3.91326598502339,6.41195814384659));
#126124=CARTESIAN_POINT('',(-3.72311151290693,3.91326598377978,6.36509553085646));
#126125=CARTESIAN_POINT('',(-4.36052349282626,3.82362522064783,6.10211724455119));
#126126=CARTESIAN_POINT('Origin',(0.0831729945559451,4.01780058964706,-0.169354587059151));
#126127=CARTESIAN_POINT('Ctrl Pts',(-4.21563855520111,3.78467661323922,
5.89838042225523));
#126128=CARTESIAN_POINT('Ctrl Pts',(-4.23965807938136,3.79148857344083,
5.9323543498312));
#126129=CARTESIAN_POINT('Ctrl Pts',(-4.2637584026862,3.79813536730393,5.96633656991507));
#126130=CARTESIAN_POINT('Ctrl Pts',(-4.31204787018211,3.81110763542439,
6.03423495106847));
#126131=CARTESIAN_POINT('Ctrl Pts',(-4.33626567407951,3.81744080533757,
6.06819139775185));
#126132=CARTESIAN_POINT('Ctrl Pts',(-4.36052349394067,3.82362522064755,
6.10211724370674));
#126133=CARTESIAN_POINT('Ctrl Pts',(-4.811202304,3.913265985,5.753462644));
#126134=CARTESIAN_POINT('Ctrl Pts',(-4.761269485,3.903042157,5.795217828));
#126135=CARTESIAN_POINT('Ctrl Pts',(-4.710619476,3.892857143,5.83610008));
#126136=CARTESIAN_POINT('Ctrl Pts',(-4.44193447,3.838828313,6.052969703));
#126137=CARTESIAN_POINT('Ctrl Pts',(-4.154459583,3.783894965,6.244234587));
#126138=CARTESIAN_POINT('Ctrl Pts',(-4.830724789,3.913265985,5.406162966));
#126139=CARTESIAN_POINT('Ctrl Pts',(-4.783806095,3.903042157,5.448087581));
#126140=CARTESIAN_POINT('Ctrl Pts',(-4.736166816,3.892857143,5.489191552));
#126141=CARTESIAN_POINT('Ctrl Pts',(-4.483452941,3.838828313,5.707237335));
#126142=CARTESIAN_POINT('Ctrl Pts',(-4.211773557,3.783894965,5.901140864));
#126143=CARTESIAN_POINT('',(-4.81120229945886,3.9132659858793,5.75346264667725));
#126144=CARTESIAN_POINT('Ctrl Pts',(-4.36052349132177,3.82362522012809,
6.1021172458116));
#126145=CARTESIAN_POINT('Ctrl Pts',(-4.48011387030856,3.84689293573233,
6.01665893095114));
#126146=CARTESIAN_POINT('Ctrl Pts',(-4.59689695300997,3.86998912007465,
5.92789143529639));
#126147=CARTESIAN_POINT('Ctrl Pts',(-4.71061947665133,3.89285714276327,
5.8361000802071));
#126148=CARTESIAN_POINT('Ctrl Pts',(-4.74435316195801,3.89964051914521,
5.80887187081367));
#126149=CARTESIAN_POINT('Ctrl Pts',(-4.7778837148795,3.90644394874722,5.78132455595175));
#126150=CARTESIAN_POINT('Ctrl Pts',(-4.81120230059236,3.91326598565651,
5.75346264633524));
#126151=CARTESIAN_POINT('',(-4.82096354039051,3.91326598631302,5.5798128102786));
#126152=CARTESIAN_POINT('Origin',(-7.63712010298789E-13,4.00453391999933,
1.09677891768634E-12));
#126153=CARTESIAN_POINT('',(-4.36636804460132,4.00345494180093,6.09793654434491));
#126154=CARTESIAN_POINT('Origin',(0.12706732881094,4.16057201538049,-0.134439565904996));
#126155=CARTESIAN_POINT('Origin',(0.110128494847791,4.01785439830898,-0.157790259172783));
#126156=CARTESIAN_POINT('Ctrl Pts',(-5.73626078558308,3.783915088,4.83249851653824));
#126157=CARTESIAN_POINT('Ctrl Pts',(-5.47361588965722,3.848090541,5.14426263175883));
#126158=CARTESIAN_POINT('Ctrl Pts',(-5.17872930030728,3.913265985,5.4257250712431));
#126159=CARTESIAN_POINT('Ctrl Pts',(-5.16868509190111,3.91548594265879,
5.43531203620788));
#126160=CARTESIAN_POINT('Ctrl Pts',(-5.15864088349497,3.91770590031752,
5.44489900117279));
#126161=CARTESIAN_POINT('Ctrl Pts',(-5.38818602700001,3.783915088,4.850768118));
#126162=CARTESIAN_POINT('Ctrl Pts',(-5.124548183,3.848090541,5.14361447));
#126163=CARTESIAN_POINT('Ctrl Pts',(-4.830724789,3.913265985,5.406162966));
#126164=CARTESIAN_POINT('Ctrl Pts',(-4.82071679436569,3.91548594265879,
5.41510569824279));
#126165=CARTESIAN_POINT('Ctrl Pts',(-4.81070879973142,3.91770590031752,
5.4240484304857));
#126166=CARTESIAN_POINT('',(-5.17802446096145,3.91326598502339,5.42568545648943));
#126167=CARTESIAN_POINT('',(-5.00437462239009,3.91326598377978,5.41592421368362));
#126168=CARTESIAN_POINT('',(-5.57035170717127,3.82362522068455,5.02206947957131));
#126169=CARTESIAN_POINT('Origin',(0.117634589582996,4.01780062259429,-0.14751536631502));
#126170=CARTESIAN_POINT('Ctrl Pts',(-5.38505670344997,3.78467661305223,
4.85424188932103));
#126171=CARTESIAN_POINT('Ctrl Pts',(-5.41581805460382,3.7914885732252,4.8822580373369));
#126172=CARTESIAN_POINT('Ctrl Pts',(-5.44666009944762,3.79813536727438,
4.91026491555166));
#126173=CARTESIAN_POINT('Ctrl Pts',(-5.50841686742267,3.81110766406195,
4.96619518564335));
#126174=CARTESIAN_POINT('Ctrl Pts',(-5.53936826028539,3.81744086358108,
4.99415177693172));
#126175=CARTESIAN_POINT('Ctrl Pts',(-5.57035170819594,3.8236252206782,5.02206947843552));
#126176=CARTESIAN_POINT('Ctrl Pts',(-5.935543465,3.913265985,4.584683607));
#126177=CARTESIAN_POINT('Ctrl Pts',(-5.895754178,3.903042157,4.636196659));
#126178=CARTESIAN_POINT('Ctrl Pts',(-5.855076814,3.892857143,4.687011361));
#126179=CARTESIAN_POINT('Ctrl Pts',(-5.639294072,3.838828313,4.956570027));
#126180=CARTESIAN_POINT('Ctrl Pts',(-5.399656485,3.783894965,5.205161847));
#126181=CARTESIAN_POINT('Ctrl Pts',(-5.879950361,3.913265985,4.241306845));
#126182=CARTESIAN_POINT('Ctrl Pts',(-5.843141152,3.903042157,4.292337419));
#126183=CARTESIAN_POINT('Ctrl Pts',(-5.805451792,3.892857143,4.342721438));
#126184=CARTESIAN_POINT('Ctrl Pts',(-5.605519625,3.838828313,4.609995445));
#126185=CARTESIAN_POINT('Ctrl Pts',(-5.381875481,3.783894965,4.85776865500001));
#126186=CARTESIAN_POINT('',(-5.93554346122029,3.91326598587964,4.58468361069559));
#126187=CARTESIAN_POINT('Ctrl Pts',(-5.57035170579324,3.82362522012809,
5.02206948117668));
#126188=CARTESIAN_POINT('Ctrl Pts',(-5.66877511654743,3.84689293573234,
4.91290073788479));
#126189=CARTESIAN_POINT('Ctrl Pts',(-5.76374548809422,3.86998912007465,
4.80110366621072));
#126190=CARTESIAN_POINT('Ctrl Pts',(-5.85507681427008,3.89285714276327,
4.68701136109109));
#126191=CARTESIAN_POINT('Ctrl Pts',(-5.88216856458662,3.89964051914521,
4.65316798694159));
#126192=CARTESIAN_POINT('Ctrl Pts',(-5.90899333344674,3.90644394874722,
4.61905663523193));
#126193=CARTESIAN_POINT('Ctrl Pts',(-5.93554346242304,3.91326598565651,
4.58468361020552));
#126194=CARTESIAN_POINT('',(-5.90774690816809,3.91326598631302,4.41299523246855));
#126195=CARTESIAN_POINT('Origin',(4.70543742858709E-13,4.00453392000044,
-5.54677831443584E-13));
#126196=CARTESIAN_POINT('',(-5.57516088947638,4.0034549415791,5.01673011568443));
#126197=CARTESIAN_POINT('Origin',(0.152997134137387,4.16057204596886,-0.10398076501913));
#126198=CARTESIAN_POINT('Origin',(0.14147395430415,4.01785425857555,-0.130426777184716));
#126199=CARTESIAN_POINT('Ctrl Pts',(-6.64099453019887,3.783915088,3.48639088072739));
#126200=CARTESIAN_POINT('Ctrl Pts',(-6.45151019389346,3.848090541,3.84732701283557));
#126201=CARTESIAN_POINT('Ctrl Pts',(-6.22402399486561,3.913265985,4.18560091662053));
#126202=CARTESIAN_POINT('Ctrl Pts',(-6.21627552944004,3.91548594241539,
4.19712295030455));
#126203=CARTESIAN_POINT('Ctrl Pts',(-6.20852706401435,3.91770589983073,
4.20864498398861));
#126204=CARTESIAN_POINT('Ctrl Pts',(-6.30498499000001,3.783915088,3.579059133));
#126205=CARTESIAN_POINT('Ctrl Pts',(-6.110464161,3.848090541,3.921733244));
#126206=CARTESIAN_POINT('Ctrl Pts',(-5.87995036100001,3.913265985,4.241306845));
#126207=CARTESIAN_POINT('Ctrl Pts',(-5.87209877168578,3.91548594241539,
4.25219192290301));
#126208=CARTESIAN_POINT('Ctrl Pts',(-5.86424718237167,3.91770589983073,
4.26307700080593));
#126209=CARTESIAN_POINT('',(-6.22332711995899,3.91326598459135,4.18571374571257));
#126210=CARTESIAN_POINT('',(-6.05163873763557,3.91326598377978,4.2135102992684));
#126211=CARTESIAN_POINT('',(-6.51971646641597,3.82362522066975,3.70719532745384));
#126212=CARTESIAN_POINT('Origin',(0.146596010521638,4.01780065125232,-0.118778704970577));
#126213=CARTESIAN_POINT('Ctrl Pts',(-6.30267558681799,3.78467661304239,
3.58312440139765));
#126214=CARTESIAN_POINT('Ctrl Pts',(-6.33874039805141,3.79148857322278,
3.60387276644293));
#126215=CARTESIAN_POINT('Ctrl Pts',(-6.3748820238234,3.79813536728634,3.6245947315682));
#126216=CARTESIAN_POINT('Ctrl Pts',(-6.44721814073559,3.81110763418867,
3.66594140820452));
#126217=CARTESIAN_POINT('Ctrl Pts',(-6.48345555858731,3.81744080288131,
3.68659064831504));
#126218=CARTESIAN_POINT('Ctrl Pts',(-6.51971646712109,3.82362522066945,
3.707195326179));
#126219=CARTESIAN_POINT('Ctrl Pts',(-6.78234521,3.913265985,3.201529861));
#126220=CARTESIAN_POINT('Ctrl Pts',(-6.754559958,3.903042157,3.260392086));
#126221=CARTESIAN_POINT('Ctrl Pts',(-6.725757268,3.892857143,3.3187632));
#126222=CARTESIAN_POINT('Ctrl Pts',(-6.572966551,3.838828313,3.628406645));
#126223=CARTESIAN_POINT('Ctrl Pts',(-6.39237145,3.783894965,3.922701524));
#126224=CARTESIAN_POINT('Ctrl Pts',(-6.654235988,3.913265985,2.878131931));
#126225=CARTESIAN_POINT('Ctrl Pts',(-6.629257423,3.903042157,2.935882329));
#126226=CARTESIAN_POINT('Ctrl Pts',(-6.603280295,3.892857143,2.993190497));
#126227=CARTESIAN_POINT('Ctrl Pts',(-6.465478441,3.838828313,3.297195292));
#126228=CARTESIAN_POINT('Ctrl Pts',(-6.30032689000001,3.783894965,3.587252582));
#126229=CARTESIAN_POINT('',(-6.78234520716211,3.91326598587963,3.20152986547135));
#126230=CARTESIAN_POINT('Ctrl Pts',(-6.51971646550344,3.82362522012805,
3.70719532928111));
#126231=CARTESIAN_POINT('Ctrl Pts',(-6.59237073886474,3.8468929357323,3.57942076650544));
#126232=CARTESIAN_POINT('Ctrl Pts',(-6.66108769022292,3.86998912007463,
3.44982162559431));
#126233=CARTESIAN_POINT('Ctrl Pts',(-6.72575726773051,3.89285714276327,
3.31876319968304));
#126234=CARTESIAN_POINT('Ctrl Pts',(-6.74494030295258,3.89964051914521,
3.27988713929576));
#126235=CARTESIAN_POINT('Ctrl Pts',(-6.76380499121347,3.90644394874722,
3.24080675989453));
#126236=CARTESIAN_POINT('Ctrl Pts',(-6.78234520833622,3.91326598565651,
3.20152986476135));
#126237=CARTESIAN_POINT('',(-6.71829059567161,3.91326598631302,3.03983090335604));
#126238=CARTESIAN_POINT('Origin',(3.38271077815477E-14,4.00453391999933,
3.20923843055709E-14));
#126239=CARTESIAN_POINT('',(-6.523265407003,4.00345494158755,3.70094696342879));
#126240=CARTESIAN_POINT('Origin',(0.171773019413894,4.16057204387436,-0.0686599350762412));
#126241=CARTESIAN_POINT('Origin',(0.166204606815189,4.01785424021442,-0.0969649222269142));
#126242=CARTESIAN_POINT('Ctrl Pts',(-7.234578469,3.783915088,1.977593076));
#126243=CARTESIAN_POINT('Ctrl Pts',(-7.127096857,3.848090541,2.370790323));
#126244=CARTESIAN_POINT('Ctrl Pts',(-6.977633919,3.913265985,2.750022709));
#126245=CARTESIAN_POINT('Ctrl Pts',(-6.97613574545446,3.91391928492389,
2.75382402547298));
#126246=CARTESIAN_POINT('Ctrl Pts',(-6.97463757190891,3.91457258484778,
2.75762534194596));
#126247=CARTESIAN_POINT('Ctrl Pts',(-6.926969862,3.783915088,2.13999732));
#126248=CARTESIAN_POINT('Ctrl Pts',(-6.810661627,3.848090541,2.516476129));
#126249=CARTESIAN_POINT('Ctrl Pts',(-6.654235988,3.913265985,2.878131931));
#126250=CARTESIAN_POINT('Ctrl Pts',(-6.65266802234021,3.91391928492389,
2.88175706484522));
#126251=CARTESIAN_POINT('Ctrl Pts',(-6.65110005668042,3.91457258484778,
2.88538219869044));
#126252=CARTESIAN_POINT('',(-6.9776339183878,3.91326598458878,2.75002271233773));
#126253=CARTESIAN_POINT('',(-6.81593495058514,3.91326598377978,2.81407732706006));
#126254=CARTESIAN_POINT('',(-7.16422653006704,3.82362522066782,2.21897684172014));
#126255=CARTESIAN_POINT('Origin',(0.168702890671167,4.01780065157927,-0.0844880162775102));
#126256=CARTESIAN_POINT('Ctrl Pts',(-6.92558836378585,3.78467661306916,
2.14446399830583));
#126257=CARTESIAN_POINT('Ctrl Pts',(-6.96527028494623,3.79148857322583,
2.15697440977198));
#126258=CARTESIAN_POINT('Ctrl Pts',(-7.00502154967839,3.798135367293,2.16944252569916));
#126259=CARTESIAN_POINT('Ctrl Pts',(-7.08455480235546,3.81110763428842,
2.19427241333284));
#126260=CARTESIAN_POINT('Ctrl Pts',(-7.12438398655221,3.81744080309546,
2.20664891226419));
#126261=CARTESIAN_POINT('Ctrl Pts',(-7.16422653047534,3.82362522066753,
2.21897684032714));
#126262=CARTESIAN_POINT('Ctrl Pts',(-7.312012032,3.913265985,1.668676136));
#126263=CARTESIAN_POINT('Ctrl Pts',(-7.297530022,3.903042157,1.732135204));
#126264=CARTESIAN_POINT('Ctrl Pts',(-7.281948786,3.892857143,1.79533336));
#126265=CARTESIAN_POINT('Ctrl Pts',(-7.19929442,3.838828313,2.130583001));
#126266=CARTESIAN_POINT('Ctrl Pts',(-7.086186231,3.783894965,2.456820037));
#126267=CARTESIAN_POINT('Ctrl Pts',(-7.117376937,3.913265985,1.380378766));
#126268=CARTESIAN_POINT('Ctrl Pts',(-7.105396986,3.903042157,1.442148645));
#126269=CARTESIAN_POINT('Ctrl Pts',(-7.09234675,3.892857143,1.503701295));
#126270=CARTESIAN_POINT('Ctrl Pts',(-7.023118672,3.838828313,1.830221952));
#126271=CARTESIAN_POINT('Ctrl Pts',(-6.924182015,3.783894965,2.149000565));
#126272=CARTESIAN_POINT('',(-7.31201203007925,3.91326598587931,1.66867614091864));
#126273=CARTESIAN_POINT('Ctrl Pts',(-7.16422652957999,3.82362522012809,
2.21897684369667));
#126274=CARTESIAN_POINT('Ctrl Pts',(-7.20771443234409,3.84689293573233,
2.07857105821795));
#126275=CARTESIAN_POINT('Ctrl Pts',(-7.24696483514426,3.86998912007465,
1.93722976007989));
#126276=CARTESIAN_POINT('Ctrl Pts',(-7.2819487862808,3.89285714276327,1.79533336012661));
#126277=CARTESIAN_POINT('Ctrl Pts',(-7.29232612896224,3.89964051914521,
1.75324241500064));
#126278=CARTESIAN_POINT('Ctrl Pts',(-7.30234864499589,3.90644394874722,
1.71102036257375));
#126279=CARTESIAN_POINT('Ctrl Pts',(-7.31201203089214,3.91326598565651,
1.66867613996504));
#126280=CARTESIAN_POINT('',(-7.21469448283075,3.91326598631302,1.52452745889956));
#126281=CARTESIAN_POINT('Origin',(1.29236898960272E-13,4.00453392000067,
-1.20888542232134E-13));
#126282=CARTESIAN_POINT('',(-7.16634928489015,4.00345494175446,2.21211164336112));
#126283=CARTESIAN_POINT('Origin',(0.182516852497029,4.16057202103997,-0.0301285563182022));
#126284=CARTESIAN_POINT('Origin',(0.183163364923503,4.0178544102177,-0.058968874271389));
#126285=CARTESIAN_POINT('Ctrl Pts',(-7.49110093225904,3.783915088,0.375681439532661));
#126286=CARTESIAN_POINT('Ctrl Pts',(-7.47068275464331,3.848090541,0.782820608964772));
#126287=CARTESIAN_POINT('Ctrl Pts',(-7.40625939708089,3.913265985,1.1853486654421));
#126288=CARTESIAN_POINT('Ctrl Pts',(-7.4040650565511,3.91548594253913,1.19905927696758));
#126289=CARTESIAN_POINT('Ctrl Pts',(-7.40187071602134,3.9177059000782,1.21276988849307));
#126290=CARTESIAN_POINT('Ctrl Pts',(-7.225057322,3.783915088,0.600871612));
#126291=CARTESIAN_POINT('Ctrl Pts',(-7.192400124,3.848090541,0.993551388));
#126292=CARTESIAN_POINT('Ctrl Pts',(-7.117376937,3.913265985,1.380378766));
#126293=CARTESIAN_POINT('Ctrl Pts',(-7.11482155295706,3.91548594253913,
1.39355459268297));
#126294=CARTESIAN_POINT('Ctrl Pts',(-7.11226616891413,3.91770590007819,
1.4067304193659));
#126295=CARTESIAN_POINT('',(-7.40567430623151,3.91326598459133,1.18574367653095));
#126296=CARTESIAN_POINT('',(-7.26152562067098,3.91326598377978,1.28306122602161));
#126297=CARTESIAN_POINT('',(-7.4737453237154,3.8236252207137,0.627001465451102));
#126298=CARTESIAN_POINT('Origin',(0.182920815903383,4.01780065137544,-0.0462465742457208));
#126299=CARTESIAN_POINT('Ctrl Pts',(-7.22466832584242,3.78467661301739,
0.605530843173444));
#126300=CARTESIAN_POINT('Ctrl Pts',(-7.26611187466958,3.79148857323157,
0.609218327966945));
#126301=CARTESIAN_POINT('Ctrl Pts',(-7.30761405303173,3.79813536726189,
0.612849599230928));
#126302=CARTESIAN_POINT('Ctrl Pts',(-7.39062574518316,3.81110766408171,
0.620001695735266));
#126303=CARTESIAN_POINT('Ctrl Pts',(-7.43218454272656,3.81744086362057,
0.623526759203508));
#126304=CARTESIAN_POINT('Ctrl Pts',(-7.4737453238487,3.82362522071367,0.627001463856704));
#126305=CARTESIAN_POINT('Ctrl Pts',(-7.499777297,3.913265985,0.05779697));
#126306=CARTESIAN_POINT('Ctrl Pts',(-7.499275692,3.903042157,0.122885604));
#126307=CARTESIAN_POINT('Ctrl Pts',(-7.497644473,3.892857143,0.187955727));
#126308=CARTESIAN_POINT('Ctrl Pts',(-7.488991283,3.838828313,0.533135664000001));
#126309=CARTESIAN_POINT('Ctrl Pts',(-7.44865882,3.783894965,0.876060377));
#126310=CARTESIAN_POINT('Ctrl Pts',(-7.24771725,3.913265985,-0.181919376));
#126311=CARTESIAN_POINT('Ctrl Pts',(-7.249296082,3.903042157,-0.119018306));
#126312=CARTESIAN_POINT('Ctrl Pts',(-7.249782953,3.892857143,-0.056099309));
#126313=CARTESIAN_POINT('Ctrl Pts',(-7.25236567800001,3.838828313,0.277669467));
#126314=CARTESIAN_POINT('Ctrl Pts',(-7.224270084,3.783894965,0.610263670000001));
#126315=CARTESIAN_POINT('',(-7.49977729625428,3.91326598544903,0.0577969751222766));
#126316=CARTESIAN_POINT('Ctrl Pts',(-7.47374532365293,3.82362522012805,
0.627001467668876));
#126317=CARTESIAN_POINT('Ctrl Pts',(-7.48603340995214,3.84689293573231,
0.48052967758556));
#126318=CARTESIAN_POINT('Ctrl Pts',(-7.49398195897382,3.86998912007412,
0.334055183764473));
#126319=CARTESIAN_POINT('Ctrl Pts',(-7.49764447287357,3.89285714292383,
0.187955727374184));
#126320=CARTESIAN_POINT('Ctrl Pts',(-7.49873088980851,3.89964051904629,
0.144618023667244));
#126321=CARTESIAN_POINT('Ctrl Pts',(-7.49944259184632,3.90644394833731,
0.101228554286914));
#126322=CARTESIAN_POINT('Ctrl Pts',(-7.49977729697119,3.91326598441267,
0.0577969737391663));
#126323=CARTESIAN_POINT('',(-7.37374727356795,3.91326598631302,-0.0620611949262858));
#126324=CARTESIAN_POINT('Origin',(-2.30067701001424E-12,4.00453392,1.76098149734169E-13));
#126325=CARTESIAN_POINT('',(-7.47434263494074,4.00345494159181,0.619840442693622));
#126326=CARTESIAN_POINT('Origin',(0.18472655890323,4.16057205720237,0.00981153923062972));
#126327=CARTESIAN_POINT('Origin',(0.191557339022314,4.01785420958081,-0.0182154483150819));
#126328=CARTESIAN_POINT('Ctrl Pts',(-7.39629537,3.783915088,-1.242905788));
#126329=CARTESIAN_POINT('Ctrl Pts',(-7.46384694,3.848090541,-0.840919274));
#126330=CARTESIAN_POINT('Ctrl Pts',(-7.487433596,3.913265985,-0.433979423));
#126331=CARTESIAN_POINT('Ctrl Pts',(-7.48767002186263,3.91391928492389,
-0.429900374859003));
#126332=CARTESIAN_POINT('Ctrl Pts',(-7.48790644772526,3.91457258484778,
-0.425821326718006));
#126333=CARTESIAN_POINT('Ctrl Pts',(-7.185309132,3.783915088,-0.966350186));
#126334=CARTESIAN_POINT('Ctrl Pts',(-7.237829985,3.848090541,-0.575830712));
#126335=CARTESIAN_POINT('Ctrl Pts',(-7.24771725000001,3.913265985,-0.181919376));
#126336=CARTESIAN_POINT('Ctrl Pts',(-7.24781635710346,3.91391928492389,
-0.177970921949899));
#126337=CARTESIAN_POINT('Ctrl Pts',(-7.24791546420693,3.91457258484778,
-0.174022467899798));
#126338=CARTESIAN_POINT('',(-7.48743359644336,3.9132659845887,-0.433979417791379));
#126339=CARTESIAN_POINT('',(-7.36757542331898,3.91326598377978,-0.307949391868539));
#126340=CARTESIAN_POINT('',(-7.43380009195768,3.82362522069477,-0.994291802622036));
#126341=CARTESIAN_POINT('Origin',(0.188585881119456,4.01780062346965,-0.00584277760883337));
#126342=CARTESIAN_POINT('Ctrl Pts',(-7.18593082774993,3.78467661310377,
-0.961716262313775));
#126343=CARTESIAN_POINT('Ctrl Pts',(-7.22719814967869,3.79148857331076,
-0.967024126778678));
#126344=CARTESIAN_POINT('Ctrl Pts',(-7.26851064564091,3.79813536726239,
-0.972399494037209));
#126345=CARTESIAN_POINT('Ctrl Pts',(-7.35111886069136,3.81110763282126,
-0.983259643223968));
#126346=CARTESIAN_POINT('Ctrl Pts',(-7.39246359533456,3.81744080007791,
-0.988750875908959));
#126347=CARTESIAN_POINT('Ctrl Pts',(-7.43380009175475,3.82362522069464,
-0.994291804132863));
#126348=CARTESIAN_POINT('Ctrl Pts',(-7.336861312,3.913265985,-1.555784718));
#126349=CARTESIAN_POINT('Ctrl Pts',(-7.350363566,3.903042157,-1.49210999));
#126350=CARTESIAN_POINT('Ctrl Pts',(-7.362758637,3.892857143,-1.428210506));
#126351=CARTESIAN_POINT('Ctrl Pts',(-7.428511236,3.838828313,-1.089240504));
#126352=CARTESIAN_POINT('Ctrl Pts',(-7.462840401,3.783894965,-0.745662894));
#126353=CARTESIAN_POINT('Ctrl Pts',(-7.03916236,3.913265985,-1.73571117));
#126354=CARTESIAN_POINT('Ctrl Pts',(-7.05422615,3.903042157,-1.674620094));
#126355=CARTESIAN_POINT('Ctrl Pts',(-7.068227363,3.892857143,-1.613276771));
#126356=CARTESIAN_POINT('Ctrl Pts',(-7.14250012700001,3.838828313,-1.287866533));
#126357=CARTESIAN_POINT('Ctrl Pts',(-7.186559314,3.783894965,-0.957008476));
#126358=CARTESIAN_POINT('',(-7.33686131228228,3.91326598544478,-1.55578471328563));
#126359=CARTESIAN_POINT('Ctrl Pts',(-7.43380009232047,3.82362522012808,
-0.994291800520328));
#126360=CARTESIAN_POINT('Ctrl Pts',(-7.41431378467035,3.84689293573234,
-1.13998073657581));
#126361=CARTESIAN_POINT('Ctrl Pts',(-7.39058881472474,3.86998912007434,
-1.28473944107708));
#126362=CARTESIAN_POINT('Ctrl Pts',(-7.36275863686772,3.89285714295372,
-1.42821050582817));
#126363=CARTESIAN_POINT('Ctrl Pts',(-7.3545033286935,3.89964051908512,-1.4707685459966));
#126364=CARTESIAN_POINT('Ctrl Pts',(-7.34587093849312,3.90644394833732,
-1.51329658840766));
#126365=CARTESIAN_POINT('Ctrl Pts',(-7.33686131277566,3.91326598441268,
-1.55578471434209));
#126366=CARTESIAN_POINT('',(-7.18801183780196,3.91326598631302,-1.6457479361297));
#126367=CARTESIAN_POINT('Origin',(7.64145691167784E-13,4.00453392000044,
-2.8162151430311E-14));
#126368=CARTESIAN_POINT('',(-7.43284403006748,4.00345494177907,-1.00141380955596));
#126369=CARTESIAN_POINT('Origin',(0.178298505928733,4.16057201474277,0.0492928937590242));
#126370=CARTESIAN_POINT('Origin',(0.190994943113921,4.01785441543893,0.0233895974095227));
#126371=CARTESIAN_POINT('Ctrl Pts',(-6.95648361438047,3.783915088,-2.80447239965452));
#126372=CARTESIAN_POINT('Ctrl Pts',(-7.10890587833995,3.848090541,-2.42638952729282));
#126373=CARTESIAN_POINT('Ctrl Pts',(-7.2194539668175,3.913265985,-2.03401429123132));
#126374=CARTESIAN_POINT('Ctrl Pts',(-7.22321937368872,3.91548594255921,
-2.020649497409));
#126375=CARTESIAN_POINT('Ctrl Pts',(-7.22698478055991,3.91770590011835,
-2.00728470358669));
#126376=CARTESIAN_POINT('Ctrl Pts',(-6.809583872,3.783915088,-2.488386523));
#126377=CARTESIAN_POINT('Ctrl Pts',(-6.94482696000001,3.848090541,-2.118287608));
#126378=CARTESIAN_POINT('Ctrl Pts',(-7.03916236,3.913265985,-1.73571117));
#126379=CARTESIAN_POINT('Ctrl Pts',(-7.04237554231957,3.91548594255921,
-1.7226801355584));
#126380=CARTESIAN_POINT('Ctrl Pts',(-7.04558872463913,3.91770590011835,
-1.70964910111681));
#126381=CARTESIAN_POINT('',(-7.21908881398541,3.91326598502339,-2.03341011308339));
#126382=CARTESIAN_POINT('',(-7.12912558795207,3.91326598377977,-1.88456063811549));
#126383=CARTESIAN_POINT('',(-7.04625863050199,3.82362522070109,-2.56909309101298));
#126384=CARTESIAN_POINT('Origin',(0.185432846277829,4.01780061998897,0.0348342047164549));
#126385=CARTESIAN_POINT('Ctrl Pts',(-6.81118718964651,3.78467661311381,
-2.4839945843682));
#126386=CARTESIAN_POINT('Ctrl Pts',(-6.85034867044299,3.79148857328906,
-2.49804960808278));
#126387=CARTESIAN_POINT('Ctrl Pts',(-6.88953975868089,3.79813536731663,
-2.51218026776745));
#126388=CARTESIAN_POINT('Ctrl Pts',(-6.96788202635751,3.81110763248485,
-2.54054483607025));
#126389=CARTESIAN_POINT('Ctrl Pts',(-7.00707968910712,3.81744079938323,
-2.55479558166922));
#126390=CARTESIAN_POINT('Ctrl Pts',(-7.04625862997314,3.82362522070093,
-2.56909309246075));
#126391=CARTESIAN_POINT('Ctrl Pts',(-6.830881846,3.913265985,-3.096619642));
#126392=CARTESIAN_POINT('Ctrl Pts',(-6.85775661,3.903042157,-3.037336179));
#126393=CARTESIAN_POINT('Ctrl Pts',(-6.883598391,3.892857143,-2.977595203));
#126394=CARTESIAN_POINT('Ctrl Pts',(-7.02068226100001,3.838828313,-2.660684997));
#126395=CARTESIAN_POINT('Ctrl Pts',(-7.128067859,3.783894965,-2.332519796));
#126396=CARTESIAN_POINT('Ctrl Pts',(-6.501464062,3.913265985,-3.208343039));
#126397=CARTESIAN_POINT('Ctrl Pts',(-6.52930844400001,3.903042157,-3.151918508));
#126398=CARTESIAN_POINT('Ctrl Pts',(-6.556169318,3.892857143,-3.095019205));
#126399=CARTESIAN_POINT('Ctrl Pts',(-6.698659207,3.838828313,-2.793183326));
#126400=CARTESIAN_POINT('Ctrl Pts',(-6.812813018,3.783894965,-2.479531969));
#126401=CARTESIAN_POINT('',(-6.83088184728228,3.9132659854451,-3.09661963745733));
#126402=CARTESIAN_POINT('Ctrl Pts',(-7.04625863131703,3.82362522012808,
-2.56909308901641));
#126403=CARTESIAN_POINT('Ctrl Pts',(-6.99590908811595,3.84689293573234,
-2.70718691856856));
#126404=CARTESIAN_POINT('Ctrl Pts',(-6.94161995248627,3.86998912007467,
-2.84346107764366));
#126405=CARTESIAN_POINT('Ctrl Pts',(-6.88359839099153,3.89285714300334,
-2.97759520301957));
#126406=CARTESIAN_POINT('Ctrl Pts',(-6.86638736695053,3.89964051914954,
-3.01738361288811));
#126407=CARTESIAN_POINT('Ctrl Pts',(-6.84881452494633,3.90644394833732,
-3.05706166447821));
#126408=CARTESIAN_POINT('Ctrl Pts',(-6.83088184754387,3.91326598441267,
-3.09661963859435));
#126409=CARTESIAN_POINT('',(-6.66617295745172,3.91326598631302,-3.15248133320107));
#126410=CARTESIAN_POINT('Origin',(1.23772520010945E-12,4.00453392000089,
3.67544536472586E-13));
#126411=CARTESIAN_POINT('',(-7.04379390009593,4.00345494159456,-2.57584306385732));
#126412=CARTESIAN_POINT('Origin',(0.163533465628372,4.16057204973995,0.0864693627536012));
#126413=CARTESIAN_POINT('Origin',(0.181501620989318,4.01785426451466,0.0639010988808864));
#126414=CARTESIAN_POINT('Ctrl Pts',(-6.19096622720938,3.783915088,-4.23434373834982));
#126415=CARTESIAN_POINT('Ctrl Pts',(-6.42110158485165,3.848090541,-3.89786651471394));
#126416=CARTESIAN_POINT('Ctrl Pts',(-6.6134141979455,3.913265985,-3.53842936551643));
#126417=CARTESIAN_POINT('Ctrl Pts',(-6.61996460689183,3.91548594241512,
-3.52618648513606));
#126418=CARTESIAN_POINT('Ctrl Pts',(-6.62651501583818,3.91770589983019,
-3.51394360475565));
#126419=CARTESIAN_POINT('Ctrl Pts',(-6.115450039,3.783915088,-3.894068671));
#126420=CARTESIAN_POINT('Ctrl Pts',(-6.327091546,3.848090541,-3.56169573));
#126421=CARTESIAN_POINT('Ctrl Pts',(-6.501464062,3.913265985,-3.208343039));
#126422=CARTESIAN_POINT('Ctrl Pts',(-6.50740340872524,3.91548594241512,
-3.19630740290158));
#126423=CARTESIAN_POINT('Ctrl Pts',(-6.51334275545048,3.91770589983019,
-3.18427176680309));
#126424=CARTESIAN_POINT('',(-6.61318746238803,3.91326598502339,-3.53776081555977));
#126425=CARTESIAN_POINT('',(-6.55732576399389,3.91326598377977,-3.37305192420777));
#126426=CARTESIAN_POINT('',(-6.32924194658555,3.82362522064777,-4.02376644191561));
#126427=CARTESIAN_POINT('Origin',(0.173609143530363,4.01780060722512,0.0738823615602285));
#126428=CARTESIAN_POINT('Ctrl Pts',(-6.11796000902615,3.78467661310375,
-3.89012407986765));
#126429=CARTESIAN_POINT('Ctrl Pts',(-6.15318450146292,3.79148857325392,
-3.91226906565243));
#126430=CARTESIAN_POINT('Ctrl Pts',(-6.18842164977781,3.79813536728931,
-3.9344942839077));
#126431=CARTESIAN_POINT('Ctrl Pts',(-6.25883479088989,3.81110763537301,
-3.97903698618127));
#126432=CARTESIAN_POINT('Ctrl Pts',(-6.29405256303366,3.81744080530427,
-4.00138090761849));
#126433=CARTESIAN_POINT('Ctrl Pts',(-6.32924194583481,3.82362522064763,
-4.02376644309495));
#126434=CARTESIAN_POINT('Ctrl Pts',(-6.005497937,3.913265985,-4.492660073));
#126435=CARTESIAN_POINT('Ctrl Pts',(-6.044488575,3.903042157,-4.440539904));
#126436=CARTESIAN_POINT('Ctrl Pts',(-6.082568734,3.892857143,-4.387750858));
#126437=CARTESIAN_POINT('Ctrl Pts',(-6.284573986,3.838828313,-4.107718817));
#126438=CARTESIAN_POINT('Ctrl Pts',(-6.459994786,3.783894965,-3.810310665));
#126439=CARTESIAN_POINT('Ctrl Pts',(-5.65976453,3.913265985,-4.530956353));
#126440=CARTESIAN_POINT('Ctrl Pts',(-5.69908753200001,3.903042157,-4.481836715));
#126441=CARTESIAN_POINT('Ctrl Pts',(-5.737552082,3.892857143,-4.43204198));
#126442=CARTESIAN_POINT('Ctrl Pts',(-5.941596428,3.838828313,-4.167893971));
#126443=CARTESIAN_POINT('Ctrl Pts',(-6.12050715700001,3.783894965,-3.886115303));
#126444=CARTESIAN_POINT('',(-6.00549793922011,3.9132659854451,-4.49266006884022));
#126445=CARTESIAN_POINT('Ctrl Pts',(-6.32924194769678,3.82362522012804,
-4.02376644030595));
#126446=CARTESIAN_POINT('Ctrl Pts',(-6.25038345750539,3.8468929357323,-4.14780804938589));
#126447=CARTESIAN_POINT('Ctrl Pts',(-6.16806865568598,3.86998912007458,
-4.2692256348332));
#126448=CARTESIAN_POINT('Ctrl Pts',(-6.08256873377003,3.89285714299345,
-4.38775085799873));
#126449=CARTESIAN_POINT('Ctrl Pts',(-6.05720676147809,3.89964051913671,
-4.42290917543916));
#126450=CARTESIAN_POINT('Ctrl Pts',(-6.03151515499193,3.90644394833732,
-4.45788193471822));
#126451=CARTESIAN_POINT('Ctrl Pts',(-6.00549793923989,3.91326598441267,
-4.49266007000586));
#126452=CARTESIAN_POINT('',(-5.83263123844007,3.91326598631302,-4.51180820661373));
#126453=CARTESIAN_POINT('Origin',(3.25260651745651E-14,4.00453392000067,
8.13151629364128E-14));
#126454=CARTESIAN_POINT('',(-6.32538379609172,4.00345494159109,-4.02982876001983));
#126455=CARTESIAN_POINT('Origin',(0.141121856785884,4.16057201893952,0.119602660310776));
#126456=CARTESIAN_POINT('Origin',(0.163521298014353,4.01785421895581,0.101424576841471));
#126457=CARTESIAN_POINT('Ctrl Pts',(-5.13596613941495,3.783915088,-5.46622186992519));
#126458=CARTESIAN_POINT('Ctrl Pts',(-5.43305371731725,3.848090541,-5.18708359570571));
#126459=CARTESIAN_POINT('Ctrl Pts',(-5.69813853003985,3.913265985,-4.87739141458904));
#126460=CARTESIAN_POINT('Ctrl Pts',(-5.70716765213171,3.91548594258725,
-4.86684290943145));
#126461=CARTESIAN_POINT('Ctrl Pts',(-5.71619677422368,3.91770590017445,
-4.85629440427387));
#126462=CARTESIAN_POINT('Ctrl Pts',(-5.135364559,3.783915088,-5.11766849700001));
#126463=CARTESIAN_POINT('Ctrl Pts',(-5.413508362,3.848090541,-4.838562918));
#126464=CARTESIAN_POINT('Ctrl Pts',(-5.65976453,3.913265985,-4.530956353));
#126465=CARTESIAN_POINT('Ctrl Pts',(-5.66815232477374,3.91548594258725,
-4.52047888655021));
#126466=CARTESIAN_POINT('Ctrl Pts',(-5.67654011954747,3.91770590017445,
-4.51000142010045));
#126467=CARTESIAN_POINT('',(-5.69806081408175,3.91326598502339,-4.87668975361084));
#126468=CARTESIAN_POINT('',(-5.67891267437233,3.91326598377977,-4.70382305061765));
#126469=CARTESIAN_POINT('',(-5.31627694370513,3.82362522068245,-5.29029294613879));
#126470=CARTESIAN_POINT('Origin',(0.153667820396709,4.01780065382243,0.10947592326954));
#126471=CARTESIAN_POINT('Ctrl Pts',(-5.13866381815813,3.78467661318519,
-5.11435569671692));
#126472=CARTESIAN_POINT('Ctrl Pts',(-5.16830426428969,3.79148857338208,
-5.14355516998409));
#126473=CARTESIAN_POINT('Ctrl Pts',(-5.19793982225928,3.79813536732747,
-5.1728357199823));
#126474=CARTESIAN_POINT('Ctrl Pts',(-5.25713137033582,3.81110763353346,
-5.23147377430861));
#126475=CARTESIAN_POINT('Ctrl Pts',(-5.28672247804631,3.81744080148512,
-5.26086607751029));
#126476=CARTESIAN_POINT('Ctrl Pts',(-5.31627694263694,3.82362522068214,
-5.290292947179));
#126477=CARTESIAN_POINT('Ctrl Pts',(-4.899303619,3.913265985,-5.678628712));
#126478=CARTESIAN_POINT('Ctrl Pts',(-4.948586973,3.903042157,-5.636108919));
#126479=CARTESIAN_POINT('Ctrl Pts',(-4.997124924,3.892857143,-5.59274016));
#126480=CARTESIAN_POINT('Ctrl Pts',(-5.254606016,3.838828313,-5.36268027));
#126481=CARTESIAN_POINT('Ctrl Pts',(-5.489859537,3.783894965,-5.109935642));
#126482=CARTESIAN_POINT('Ctrl Pts',(-4.553420698,3.913265985,-5.64170718300001));
#126483=CARTESIAN_POINT('Ctrl Pts',(-4.602383621,3.903042157,-5.602189219));
#126484=CARTESIAN_POINT('Ctrl Pts',(-4.650653287,3.892857143,-5.561827398));
#126485=CARTESIAN_POINT('Ctrl Pts',(-4.906711204,3.838828313,-5.347718525));
#126486=CARTESIAN_POINT('Ctrl Pts',(-5.142013183,3.783894965,-5.110988204));
#126487=CARTESIAN_POINT('',(-4.89930362251608,3.91326598587964,-5.67862870804665));
#126488=CARTESIAN_POINT('Ctrl Pts',(-5.31627694526545,3.82362522012808,
-5.29029294474692));
#126489=CARTESIAN_POINT('Ctrl Pts',(-5.21259684342557,3.84689293573233,
-5.39448228564937));
#126490=CARTESIAN_POINT('Ctrl Pts',(-5.10610532417885,3.86998912007464,
-5.49536594628879));
#126491=CARTESIAN_POINT('Ctrl Pts',(-4.9971249235474,3.89285714276326,-5.59274016010589));
#126492=CARTESIAN_POINT('Ctrl Pts',(-4.96479790140804,3.89964051914521,
-5.6216244213825));
#126493=CARTESIAN_POINT('Ctrl Pts',(-4.93218884071494,3.90644394874722,
-5.65025660069319));
#126494=CARTESIAN_POINT('Ctrl Pts',(-4.8993036221179,3.91326598565651,-5.67862870931902));
#126495=CARTESIAN_POINT('',(-4.72636216469744,3.91326598631302,-5.66016794232501));
#126496=CARTESIAN_POINT('Origin',(-3.02709246557953E-13,4.00453392,-1.45716771982052E-13));
#126497=CARTESIAN_POINT('',(-5.31120577464656,4.00345494159129,-5.29538414253212));
#126498=CARTESIAN_POINT('Origin',(0.112111455877779,4.16057203305905,0.147143430146888));
#126499=CARTESIAN_POINT('Origin',(0.137894918506129,4.01785427167017,0.134205497386245));
#126500=CARTESIAN_POINT('Ctrl Pts',(-3.84081398363233,3.783915088,-6.44250554227282));
#126501=CARTESIAN_POINT('Ctrl Pts',(-4.19096229675016,3.848090541,-6.23375841256356));
#126502=CARTESIAN_POINT('Ctrl Pts',(-4.51642423896958,3.913265985,-5.9882920620467));
#126503=CARTESIAN_POINT('Ctrl Pts',(-4.52750988138672,3.91548594245996,
-5.97993116992911));
#126504=CARTESIAN_POINT('Ctrl Pts',(-4.53859552380381,3.91770589991986,
-5.97157027781169));
#126505=CARTESIAN_POINT('Ctrl Pts',(-3.91515514,3.783915088,-6.101971831));
#126506=CARTESIAN_POINT('Ctrl Pts',(-4.246795545,3.848090541,-5.889184282));
#126507=CARTESIAN_POINT('Ctrl Pts',(-4.553420698,3.913265985,-5.641707183));
#126508=CARTESIAN_POINT('Ctrl Pts',(-4.56386473572397,3.91548594245996,
-5.63327780226433));
#126509=CARTESIAN_POINT('Ctrl Pts',(-4.57430877344792,3.91770589991986,
-5.62484842152856));
#126510=CARTESIAN_POINT('',(-4.51649917455088,3.91326598459136,-5.98759010069319));
#126511=CARTESIAN_POINT('',(-4.53495994002295,3.91326598377977,-5.81464863880259));
#126512=CARTESIAN_POINT('',(-4.05472873979337,3.82362522068753,-6.30945123164814));
#126513=CARTESIAN_POINT('Origin',(0.126541207839908,4.01780067271071,0.13995068839164));
#126514=CARTESIAN_POINT('Ctrl Pts',(-3.91908941737862,3.78467661291985,
-6.09944572486574));
#126515=CARTESIAN_POINT('Ctrl Pts',(-3.94175982073275,3.79148856047556,
-6.13433428550706));
#126516=CARTESIAN_POINT('Ctrl Pts',(-3.96440801632649,3.79813534156362,
-6.16930096846007));
#126517=CARTESIAN_POINT('Ctrl Pts',(-4.00961033894422,3.81110763314013,
-6.23929266744067));
#126518=CARTESIAN_POINT('Ctrl Pts',(-4.03219114569097,3.81744080085026,
-6.27435900682164));
#126519=CARTESIAN_POINT('Ctrl Pts',(-4.05472873852679,3.82362522068738,
-6.30945123246102));
#126520=CARTESIAN_POINT('Ctrl Pts',(-3.564023309,3.913265985,-6.599070984));
#126521=CARTESIAN_POINT('Ctrl Pts',(-3.621294945,3.903042157,-6.568139745));
#126522=CARTESIAN_POINT('Ctrl Pts',(-3.678021106,3.892857143,-6.536219148));
#126523=CARTESIAN_POINT('Ctrl Pts',(-3.978938509,3.838828313,-6.366888754));
#126524=CARTESIAN_POINT('Ctrl Pts',(-4.263024558,3.783894965,-6.170625707));
#126525=CARTESIAN_POINT('Ctrl Pts',(-3.234163976,3.913265985,-6.488658057));
#126526=CARTESIAN_POINT('Ctrl Pts',(-3.290477367,3.903042157,-6.460589581));
#126527=CARTESIAN_POINT('Ctrl Pts',(-3.346295113,3.892857143,-6.431547949));
#126528=CARTESIAN_POINT('Ctrl Pts',(-3.642393617,3.838828313,-6.277489706));
#126529=CARTESIAN_POINT('Ctrl Pts',(-3.923084388,3.783894965,-6.09687697800001));
#126530=CARTESIAN_POINT('',(-3.56402331315857,3.91326598544902,-6.59907098094449));
#126531=CARTESIAN_POINT('Ctrl Pts',(-4.05472874160685,3.82362522012805,
-6.30945123057785));
#126532=CARTESIAN_POINT('Ctrl Pts',(-3.93107499426224,3.8468929357323,-6.38891652569893));
#126533=CARTESIAN_POINT('Ctrl Pts',(-3.80538618257823,3.86998912007455,
-6.46454905386878));
#126534=CARTESIAN_POINT('Ctrl Pts',(-3.67802110594336,3.89285714298927,
-6.53621914792962));
#126535=CARTESIAN_POINT('Ctrl Pts',(-3.6402406092741,3.89964051913127,-6.55747875699982));
#126536=CARTESIAN_POINT('Ctrl Pts',(-3.60223885805458,3.90644394833732,
-6.578431547705));
#126537=CARTESIAN_POINT('Ctrl Pts',(-3.56402331229007,3.91326598441268,
-6.5990709822231));
#126538=CARTESIAN_POINT('',(-3.39909364966501,3.91326598631302,-6.54386451677826));
#126539=CARTESIAN_POINT('Origin',(-2.91216703529606E-13,4.00453391999933,
-5.03069808033274E-13));
#126540=CARTESIAN_POINT('',(-4.04868167575611,4.00345494161998,-6.313333246779));
#126541=CARTESIAN_POINT('Origin',(0.0778588908243844,4.16057202404688,0.167803995367347));
#126542=CARTESIAN_POINT('Origin',(0.105820797950587,4.01785426712178,0.160711179465115));
#126543=CARTESIAN_POINT('Ctrl Pts',(-2.36606963524325,3.783915088,-7.11754481581828));
#126544=CARTESIAN_POINT('Ctrl Pts',(-2.75290613681028,3.848090541,-6.98894961498189));
#126545=CARTESIAN_POINT('Ctrl Pts',(-3.12352696960768,3.913265985,-6.81918682763074));
#126546=CARTESIAN_POINT('Ctrl Pts',(-3.13615078042259,3.91548594243905,
-6.813404493986));
#126547=CARTESIAN_POINT('Ctrl Pts',(-3.14877459123754,3.91770589987804,
-6.80762216034113));
#126548=CARTESIAN_POINT('Ctrl Pts',(-2.511877418,3.783915088,-6.800953745));
#126549=CARTESIAN_POINT('Ctrl Pts',(-2.881507287,3.848090541,-6.664433933));
#126550=CARTESIAN_POINT('Ctrl Pts',(-3.234163976,3.913265985,-6.488658057));
#126551=CARTESIAN_POINT('Ctrl Pts',(-3.24617590552632,3.91548594243905,
-6.48267091000746));
#126552=CARTESIAN_POINT('Ctrl Pts',(-3.25818783505264,3.91770589987804,
-6.47668376301503));
#126553=CARTESIAN_POINT('',(-3.12375105627747,3.91326598502339,-6.81851738529729));
#126554=CARTESIAN_POINT('',(-3.17895751939195,3.91326598377977,-6.65358771970716));
#126555=CARTESIAN_POINT('',(-2.60358592652387,3.823625220675,-7.03358659017151));
#126556=CARTESIAN_POINT('Origin',(0.0934974573071612,4.01780061747444,0.163881283245135));
#126557=CARTESIAN_POINT('Ctrl Pts',(-2.51626275246637,3.78467661289495,
-6.79933245052332));
#126558=CARTESIAN_POINT('Ctrl Pts',(-2.53090315221161,3.79148857308155,
-6.8382788747793));
#126559=CARTESIAN_POINT('Ctrl Pts',(-2.54550507273525,3.7981353672037,-6.87729683093022));
#126560=CARTESIAN_POINT('Ctrl Pts',(-2.57460438787571,3.81110763385064,
-6.95536917604575));
#126561=CARTESIAN_POINT('Ctrl Pts',(-2.58911904323647,3.81744080227308,
-6.99446989459292));
#126562=CARTESIAN_POINT('Ctrl Pts',(-2.60358592513734,3.82362522067471,
-7.03358659066263));
#126563=CARTESIAN_POINT('Ctrl Pts',(-2.06209323,3.913265985,-7.210948031));
#126564=CARTESIAN_POINT('Ctrl Pts',(-2.124675189,3.903042157,-7.193051656));
#126565=CARTESIAN_POINT('Ctrl Pts',(-2.186937109,3.892857143,-7.174071792));
#126566=CARTESIAN_POINT('Ctrl Pts',(-2.51722026,3.838828313,-7.07338859600001));
#126567=CARTESIAN_POINT('Ctrl Pts',(-2.836855288,3.783894965,-6.942784173));
#126568=CARTESIAN_POINT('Ctrl Pts',(-1.763681341,3.913265985,-7.032206491));
#126569=CARTESIAN_POINT('Ctrl Pts',(-1.824712048,3.903042157,-7.016899955));
#126570=CARTESIAN_POINT('Ctrl Pts',(-1.885467899,3.892857143,-7.000536465));
#126571=CARTESIAN_POINT('Ctrl Pts',(-2.207761753,3.838828313,-6.913732444));
#126572=CARTESIAN_POINT('Ctrl Pts',(-2.520716527,3.783894965,-6.79768256));
#126573=CARTESIAN_POINT('',(-2.06209323492269,3.91326598587965,-7.21094802900807));
#126574=CARTESIAN_POINT('Ctrl Pts',(-2.6035859284959,3.82362522012808,-7.03358658956712));
#126575=CARTESIAN_POINT('Ctrl Pts',(-2.46574044770231,3.84689293573232,
-7.08461212960003));
#126576=CARTESIAN_POINT('Ctrl Pts',(-2.32673141273862,3.86998912007464,
-7.13145703192533));
#126577=CARTESIAN_POINT('Ctrl Pts',(-2.1869371088004,3.89285714276326,-7.17407179237508));
#126578=CARTESIAN_POINT('Ctrl Pts',(-2.14546971161537,3.89964051914521,
-7.18671267363943));
#126579=CARTESIAN_POINT('Ctrl Pts',(-2.10385218957373,3.90644394874722,
-7.19900634661474));
#126580=CARTESIAN_POINT('Ctrl Pts',(-2.0620932340453,3.91326598565651,-7.21094803019025));
#126581=CARTESIAN_POINT('',(-1.91288729329756,3.91326598631302,-7.12157725890554));
#126582=CARTESIAN_POINT('Origin',(-2.96637714392034E-13,4.00453391999933,
-4.55798593312906E-13));
#126583=CARTESIAN_POINT('',(-2.59684572075897,4.00345494161613,-7.03607790633473));
#126584=CARTESIAN_POINT('Origin',(0.0399656944168258,4.16057204697022,0.180618175150855));
#126585=CARTESIAN_POINT('Origin',(0.0687986019714082,4.01785423229436,0.179702194074176));
#126586=CARTESIAN_POINT('Ctrl Pts',(-0.781116749,3.783915088,-7.45921286900001));
#126587=CARTESIAN_POINT('Ctrl Pts',(-1.186522811,3.848090541,-7.41675940000001));
#126588=CARTESIAN_POINT('Ctrl Pts',(-1.5849398,3.913265985,-7.33061838));
#126589=CARTESIAN_POINT('Ctrl Pts',(-1.58893341742117,3.91391928492389,
-7.32975492716629));
#126590=CARTESIAN_POINT('Ctrl Pts',(-1.59292703484234,3.91457258484778,
-7.32889147433258));
#126591=CARTESIAN_POINT('Ctrl Pts',(-0.9911471,3.783915088,-7.18193062000001));
#126592=CARTESIAN_POINT('Ctrl Pts',(-1.381482952,3.848090541,-7.128062062));
#126593=CARTESIAN_POINT('Ctrl Pts',(-1.763681341,3.913265985,-7.032206491));
#126594=CARTESIAN_POINT('Ctrl Pts',(-1.76751238783483,3.91391928492389,
-7.03124566229834));
#126595=CARTESIAN_POINT('Ctrl Pts',(-1.77134343466967,3.91457258484778,
-7.03028483359667));
#126596=CARTESIAN_POINT('',(-1.58493980516177,3.91326598458871,-7.33061837899305));
#126597=CARTESIAN_POINT('',(-1.67431057793867,3.91326598377977,-7.18141243376571));
#126598=CARTESIAN_POINT('',(-1.03070232883522,3.82362522068708,-7.42883925714906));
#126599=CARTESIAN_POINT('Origin',(0.0560818424519852,4.01780061746597,0.180148661364434));
#126600=CARTESIAN_POINT('Ctrl Pts',(-0.995778437857862,3.78467661298457,
-7.18128994883607));
#126601=CARTESIAN_POINT('Ctrl Pts',(-1.00170422328431,3.79148857321378,
-7.22247308061018));
#126602=CARTESIAN_POINT('Ctrl Pts',(-1.00757705172603,3.79813536725245,
-7.26371779929363));
#126603=CARTESIAN_POINT('Ctrl Pts',(-1.01921279396379,3.81110763322192,
-7.34622034452923));
#126604=CARTESIAN_POINT('Ctrl Pts',(-1.02498260530706,3.81744080091515,
-7.3875271267582));
#126605=CARTESIAN_POINT('Ctrl Pts',(-1.03070232734514,3.82362522068701,
-7.42883925735537));
#126606=CARTESIAN_POINT('Ctrl Pts',(-0.463741963,3.913265985,-7.48564916299999));
#126607=CARTESIAN_POINT('Ctrl Pts',(-0.528707983,3.903042157,-7.481624466));
#126608=CARTESIAN_POINT('Ctrl Pts',(-0.593594363,3.892857143,-7.476472814));
#126609=CARTESIAN_POINT('Ctrl Pts',(-0.937799589,3.838828313,-7.449144649));
#126610=CARTESIAN_POINT('Ctrl Pts',(-1.278037818,3.783894965,-7.390305767));
#126611=CARTESIAN_POINT('Ctrl Pts',(-0.210730926,3.913265985,-7.246936765));
#126612=CARTESIAN_POINT('Ctrl Pts',(-0.273625222,3.903042157,-7.245107886));
#126613=CARTESIAN_POINT('Ctrl Pts',(-0.336478302,3.892857143,-7.242187677));
#126614=CARTESIAN_POINT('Ctrl Pts',(-0.669897403,3.838828313,-7.226696737));
#126615=CARTESIAN_POINT('Ctrl Pts',(-1.000482763,3.783894965,-7.18063606100001));
#126616=CARTESIAN_POINT('',(-0.463741967619782,3.9132659854451,-7.48564916201049));
#126617=CARTESIAN_POINT('Ctrl Pts',(-1.0307023309297,3.82362522012805,-7.42883925694053));
#126618=CARTESIAN_POINT('Ctrl Pts',(-0.885110617978232,3.8468929357323,
-7.44903914474112));
#126619=CARTESIAN_POINT('Ctrl Pts',(-0.739281267546468,3.86998912007422,
-7.46490600598539));
#126620=CARTESIAN_POINT('Ctrl Pts',(-0.593594363125153,3.89285714293964,
-7.47647281373311));
#126621=CARTESIAN_POINT('Ctrl Pts',(-0.550379035012223,3.89964051906683,
-7.47990389320791));
#126622=CARTESIAN_POINT('Ctrl Pts',(-0.507091730846385,3.90644394833732,
-7.48296361012156));
#126623=CARTESIAN_POINT('Ctrl Pts',(-0.463741966732096,3.91326598441267,
-7.48564916276879));
#126624=CARTESIAN_POINT('',(-0.337236452565506,3.91326598631302,-7.36629296363075));
#126625=CARTESIAN_POINT('Origin',(-1.8564251698383E-13,4.00453391999933,
-1.12800394025392E-12));
#126626=CARTESIAN_POINT('',(-1.02358414613794,4.00345494160212,-7.4298233824669));
#126627=CARTESIAN_POINT('Origin',(0.000203746966547652,4.16057200674162,
0.184986838640377));
#126628=CARTESIAN_POINT('Origin',(0.0285594814776714,4.01785425606131,0.190290541207166));
#126629=CARTESIAN_POINT('Ctrl Pts',(0.840655601,3.783915088,-7.452737629));
#126630=CARTESIAN_POINT('Ctrl Pts',(0.435601466,3.848090541,-7.498427017));
#126631=CARTESIAN_POINT('Ctrl Pts',(0.027981472,3.913265985,-7.499947802));
#126632=CARTESIAN_POINT('Ctrl Pts',(0.0238956063009955,3.91391928492389,
-7.49996304591187));
#126633=CARTESIAN_POINT('Ctrl Pts',(0.0198097406019911,3.91457258484778,
-7.49997828982376));
#126634=CARTESIAN_POINT('Ctrl Pts',(0.575928156,3.783915088,-7.227088401));
#126635=CARTESIAN_POINT('Ctrl Pts',(0.183137991,3.848090541,-7.25838993));
#126636=CARTESIAN_POINT('Ctrl Pts',(-0.210730926,3.913265985,-7.246936765));
#126637=CARTESIAN_POINT('Ctrl Pts',(-0.214678954854233,3.91391928492389,
-7.24682196176486));
#126638=CARTESIAN_POINT('Ctrl Pts',(-0.218626983708466,3.91457258484778,
-7.24670715852972));
#126639=CARTESIAN_POINT('',(0.0279814687166059,3.91326598458875,-7.49994780268229));
#126640=CARTESIAN_POINT('',(-0.091374734637584,3.91326598377977,-7.37344228340535));
#126641=CARTESIAN_POINT('',(0.590375764720165,3.82362522068314,-7.4767276570203));
#126642=CARTESIAN_POINT('Origin',(0.0160440437016413,4.01780066691501,0.187993198170781));
#126643=CARTESIAN_POINT('Ctrl Pts',(0.57126737071102,3.78467661311086,-7.22745830969002));
#126644=CARTESIAN_POINT('Ctrl Pts',(0.574333282887148,3.79148857330225,
-7.26895247153846));
#126645=CARTESIAN_POINT('Ctrl Pts',(0.577464153266443,3.79813536727869,
-7.31049539597131));
#126646=CARTESIAN_POINT('Ctrl Pts',(0.583836056796043,3.81110763340525,
-7.39357041946398));
#126647=CARTESIAN_POINT('Ctrl Pts',(0.587080877680916,3.81744080128018,
-7.43515181229454));
#126648=CARTESIAN_POINT('Ctrl Pts',(0.590375766210829,3.8236252206831,-7.47672765690217));
#126649=CARTESIAN_POINT('Ctrl Pts',(1.156293362,3.913265985,-7.410329659));
#126650=CARTESIAN_POINT('Ctrl Pts',(1.091981021,3.903042157,-7.42036483100001));
#126651=CARTESIAN_POINT('Ctrl Pts',(1.027504195,3.892857143,-7.429282275));
#126652=CARTESIAN_POINT('Ctrl Pts',(0.685471549,3.838828313,-7.476586977));
#126653=CARTESIAN_POINT('Ctrl Pts',(0.340539281,3.783894965,-7.492264878));
#126654=CARTESIAN_POINT('Ctrl Pts',(1.352073032,3.913265985,-7.122808331));
#126655=CARTESIAN_POINT('Ctrl Pts',(1.290256015,3.903042157,-7.134542624));
#126656=CARTESIAN_POINT('Ctrl Pts',(1.228244647,3.892857143,-7.145202243));
#126657=CARTESIAN_POINT('Ctrl Pts',(0.899290605,3.838828313,-7.201748723));
#126658=CARTESIAN_POINT('Ctrl Pts',(0.566532463,3.783894965,-7.227831));
#126659=CARTESIAN_POINT('',(1.15629335682361,3.91326598544904,-7.41032965909334));
#126660=CARTESIAN_POINT('Ctrl Pts',(0.590375762642652,3.82362522012806,
-7.47672765726934));
#126661=CARTESIAN_POINT('Ctrl Pts',(0.736906000733055,3.84689293573232,
-7.46515736797145));
#126662=CARTESIAN_POINT('Ctrl Pts',(0.882736847828371,3.86998912007489,
-7.44930427085053));
#126663=CARTESIAN_POINT('Ctrl Pts',(1.02750419524605,3.89285714303887,-7.42928227496597));
#126664=CARTESIAN_POINT('Ctrl Pts',(1.07044675420083,3.89964051919568,-7.42334311994632));
#126665=CARTESIAN_POINT('Ctrl Pts',(1.11337977344539,3.90644394833732,-7.41702581146743));
#126666=CARTESIAN_POINT('Ctrl Pts',(1.15629335830546,3.91326598441268,-7.41032965957648));
#126667=CARTESIAN_POINT('',(1.25418318904368,3.91326598631302,-7.26656899637323));
#126668=CARTESIAN_POINT('Origin',(-5.45048760899197E-14,4.00453391999978,
-4.81385764583564E-14));
#126669=CARTESIAN_POINT('',(0.597539085963977,4.00345494159452,-7.47615857508329));
#126670=CARTESIAN_POINT('Origin',(-0.039567714929107,4.1605720347916,0.180705713604262));
#126671=CARTESIAN_POINT('Origin',(-0.0130150327720951,4.01785424798534,
0.191980769929868));
#126672=CARTESIAN_POINT('Ctrl Pts',(2.42374296910668,3.783915088,-7.09811240703523));
#126673=CARTESIAN_POINT('Ctrl Pts',(2.03796261175096,3.848090541,-7.22984213651986));
#126674=CARTESIAN_POINT('Ctrl Pts',(1.64017787606862,3.913265985,-7.3189853293929));
#126675=CARTESIAN_POINT('Ctrl Pts',(1.6266288282028,3.91548594250772,-7.32202165853979));
#126676=CARTESIAN_POINT('Ctrl Pts',(1.61307978033704,3.91770590001538,-7.3250579876868));
#126677=CARTESIAN_POINT('Ctrl Pts',(2.116073651,3.783915088,-6.93431556100001));
#126678=CARTESIAN_POINT('Ctrl Pts',(1.739195605,3.848090541,-7.049323552));
#126679=CARTESIAN_POINT('Ctrl Pts',(1.352073032,3.913265985,-7.122808331));
#126680=CARTESIAN_POINT('Ctrl Pts',(1.33888715079087,3.91548594250772,-7.1253113148975));
#126681=CARTESIAN_POINT('Ctrl Pts',(1.32570126958175,3.91770590001538,-7.12781429879499));
#126682=CARTESIAN_POINT('',(1.6395943529807,3.91326598502339,-7.318588002526));
#126683=CARTESIAN_POINT('',(1.49583368902063,3.91326598377977,-7.22069816754942));
#126684=CARTESIAN_POINT('',(2.18384854246494,3.82362522068674,-7.1750125812294));
#126685=CARTESIAN_POINT('Origin',(-0.024743966257188,4.01780066281652,0.187046725071964));
#126686=CARTESIAN_POINT('Ctrl Pts',(2.11160135128517,3.7846766132022,-6.93567875271368));
#126687=CARTESIAN_POINT('Ctrl Pts',(2.1235156023276,3.791488573401,-6.97554372364169));
#126688=CARTESIAN_POINT('Ctrl Pts',(2.13550377534536,3.79813536735995,-7.01544235294169));
#126689=CARTESIAN_POINT('Ctrl Pts',(2.1595853812163,3.81110763330458,-7.09520535668598));
#126690=CARTESIAN_POINT('Ctrl Pts',(2.17169310987897,3.81744080099409,-7.13511705796493));
#126691=CARTESIAN_POINT('Ctrl Pts',(2.18384854390247,3.82362522068656,-7.17501258079074));
#126692=CARTESIAN_POINT('Ctrl Pts',(2.722261695,3.913265985,-6.988511377));
#126693=CARTESIAN_POINT('Ctrl Pts',(2.661610206,3.903042157,-7.012137184));
#126694=CARTESIAN_POINT('Ctrl Pts',(2.600557799,3.892857143,-7.034706755));
#126695=CARTESIAN_POINT('Ctrl Pts',(2.276690798,3.838828313,-7.154432408));
#126696=CARTESIAN_POINT('Ctrl Pts',(1.94319314,3.783894965,-7.243894009));
#126697=CARTESIAN_POINT('Ctrl Pts',(2.851655559,3.913265985,-6.665625295));
#126698=CARTESIAN_POINT('Ctrl Pts',(2.793806315,3.903042157,-6.690374079));
#126699=CARTESIAN_POINT('Ctrl Pts',(2.735536241,3.892857143,-6.714115092));
#126700=CARTESIAN_POINT('Ctrl Pts',(2.426428783,3.838828313,-6.840054943));
#126701=CARTESIAN_POINT('Ctrl Pts',(2.10705726,3.783894965,-6.937060595));
#126702=CARTESIAN_POINT('',(2.72226169039741,3.9132659854451,-6.98851137802784));
#126703=CARTESIAN_POINT('Ctrl Pts',(2.18384854047772,3.823625220128,-7.17501258191799));
#126704=CARTESIAN_POINT('Ctrl Pts',(2.32446571297695,3.84689293573225,-7.13221312998114));
#126705=CARTESIAN_POINT('Ctrl Pts',(2.46347916887734,3.86998912007484,-7.08538134813477));
#126706=CARTESIAN_POINT('Ctrl Pts',(2.60055779923158,3.89285714303828,-7.03470675491019));
#126707=CARTESIAN_POINT('Ctrl Pts',(2.6412196424011,3.89964051919493,-7.01967507308682));
#126708=CARTESIAN_POINT('Ctrl Pts',(2.68179087705118,3.90644394833732,-7.00427612982547));
#126709=CARTESIAN_POINT('Ctrl Pts',(2.72226169151576,3.91326598441267,-6.98851137835724));
#126710=CARTESIAN_POINT('',(2.7869586195249,3.91326598631302,-6.8270683390515));
#126711=CARTESIAN_POINT('Origin',(3.67436116255337E-13,4.00453392,-1.32055824608734E-12));
#126712=CARTESIAN_POINT('',(2.19072205418073,4.00345494162733,-7.17291690205873));
#126713=CARTESIAN_POINT('Origin',(-0.0774889773561682,4.16057201301482,
0.167974844056662));
#126714=CARTESIAN_POINT('Origin',(-0.0539810493423482,4.01785423855514,
0.184694845267614));
#126715=CARTESIAN_POINT('Ctrl Pts',(3.89296155423979,3.783915088,-6.41112939026784));
#126716=CARTESIAN_POINT('Ctrl Pts',(3.54451852593086,3.848090541,-6.62271072494345));
#126717=CARTESIAN_POINT('Ctrl Pts',(3.17519692666322,3.913265985,-6.79528175958383));
#126718=CARTESIAN_POINT('Ctrl Pts',(3.16261736907935,3.91548594249093,-6.80115974579389));
#126719=CARTESIAN_POINT('Ctrl Pts',(3.15003781149546,3.91770589998178,-6.80703773200397));
#126720=CARTESIAN_POINT('Ctrl Pts',(3.557273893,3.783915088,-6.317301833));
#126721=CARTESIAN_POINT('Ctrl Pts',(3.213930366,3.848090541,-6.51063864));
#126722=CARTESIAN_POINT('Ctrl Pts',(2.851655559,3.913265985,-6.665625295));
#126723=CARTESIAN_POINT('Ctrl Pts',(2.83931602401239,3.91548594249093,-6.67090433515139));
#126724=CARTESIAN_POINT('Ctrl Pts',(2.82697648902474,3.91770589998178,-6.67618337530266));
#126725=CARTESIAN_POINT('',(3.17454163251317,3.91326598502339,-6.79501916224925));
#126726=CARTESIAN_POINT('',(3.01309859252858,3.91326598377977,-6.73032223012104));
#126727=CARTESIAN_POINT('',(3.67520699077175,3.82362522066602,-6.53780189151137));
#126728=CARTESIAN_POINT('Origin',(-0.0643749718556375,4.01780061212694,
0.17735441925624));
#126729=CARTESIAN_POINT('Ctrl Pts',(3.55319919914492,3.78467661303912,-6.31959456555699));
#126730=CARTESIAN_POINT('Ctrl Pts',(3.57340469212595,3.7914885732178,-6.35596630351304));
#126731=CARTESIAN_POINT('Ctrl Pts',(3.59368961467049,3.79813536727529,-6.39235502254762));
#126732=CARTESIAN_POINT('Ctrl Pts',(3.63435489786552,3.81110763438811,-6.4650763843928));
#126733=CARTESIAN_POINT('Ctrl Pts',(3.65475939482177,3.81744080329316,-6.50145217583232));
#126734=CARTESIAN_POINT('Ctrl Pts',(3.67520699201307,3.82362522066573,-6.53780189076739));
#126735=CARTESIAN_POINT('Ctrl Pts',(4.160940096,3.913265985,-6.23991807));
#126736=CARTESIAN_POINT('Ctrl Pts',(4.106785456,3.903042157,-6.27602979600001));
#126737=CARTESIAN_POINT('Ctrl Pts',(4.052012211,3.892857143,-6.311196166));
#126738=CARTESIAN_POINT('Ctrl Pts',(3.761454517,3.838828313,-6.49774453));
#126739=CARTESIAN_POINT('Ctrl Pts',(3.454985449,3.783894965,-6.656806708));
#126740=CARTESIAN_POINT('Ctrl Pts',(4.21789784,3.913265985,-5.89676502900001));
#126741=CARTESIAN_POINT('Ctrl Pts',(4.166721337,3.903042157,-5.93337107700001));
#126742=CARTESIAN_POINT('Ctrl Pts',(4.114917201,3.892857143,-5.969083383));
#126743=CARTESIAN_POINT('Ctrl Pts',(3.840109849,3.838828313,-6.15852779600001));
#126744=CARTESIAN_POINT('Ctrl Pts',(3.549058402,3.783894965,-6.32192094700001));
#126745=CARTESIAN_POINT('',(4.16094009122337,3.91326598587964,-6.23991807225179));
#126746=CARTESIAN_POINT('Ctrl Pts',(3.67520698908242,3.82362522012807,-6.53780189263945));
#126747=CARTESIAN_POINT('Ctrl Pts',(3.80333599309538,3.84689293573232,-6.46577453255949));
#126748=CARTESIAN_POINT('Ctrl Pts',(3.92903194273447,3.86998912007464,-6.39015386811644));
#126749=CARTESIAN_POINT('Ctrl Pts',(4.05201221122165,3.89285714276326,-6.31119616555459));
#126750=CARTESIAN_POINT('Ctrl Pts',(4.08849203547497,3.89964051914521,-6.28777482204693));
#126751=CARTESIAN_POINT('Ctrl Pts',(4.12480441948583,3.90644394874722,-6.26401428120537));
#126752=CARTESIAN_POINT('Ctrl Pts',(4.16094009247477,3.91326598565652,-6.23991807212533));
#126753=CARTESIAN_POINT('',(4.18941896135557,3.91326598631303,-6.06834155408714));
#126754=CARTESIAN_POINT('Origin',(5.49039980146659E-13,4.00453391999933,
-7.86263415486488E-13));
#126755=CARTESIAN_POINT('',(3.68146929365972,4.00345494161081,-6.53427760673526));
#126756=CARTESIAN_POINT('Origin',(-0.111786908240756,4.1605720525608,0.147389746905117));
#126757=CARTESIAN_POINT('Origin',(-0.0924228179123909,4.01785422783766,
0.168772261566034));
#126758=CARTESIAN_POINT('Ctrl Pts',(5.18014958364216,3.783915088,-5.42436908871496));
#126759=CARTESIAN_POINT('Ctrl Pts',(4.88533669232189,3.848090541,-5.7059087207646));
#126760=CARTESIAN_POINT('Ctrl Pts',(4.56174729882825,3.913265985,-5.95383836687107));
#126761=CARTESIAN_POINT('Ctrl Pts',(4.5507254370256,3.91548594261029,-5.9622831625013));
#126762=CARTESIAN_POINT('Ctrl Pts',(4.53970357522298,3.91770590022054,-5.97072795813157));
#126763=CARTESIAN_POINT('Ctrl Pts',(4.832139962,3.783915088,-5.404898092));
#126764=CARTESIAN_POINT('Ctrl Pts',(4.538385314,3.848090541,-5.667523501));
#126765=CARTESIAN_POINT('Ctrl Pts',(4.21789784,3.913265985,-5.896765029));
#126766=CARTESIAN_POINT('Ctrl Pts',(4.20698163347736,3.91548594261029,-5.90457328381877));
#126767=CARTESIAN_POINT('Ctrl Pts',(4.1960654269548,3.91770590022053,-5.91238153863744));
#126768=CARTESIAN_POINT('',(4.56105087436595,3.91326598502339,-5.95372277775558));
#126769=CARTESIAN_POINT('',(4.38947435436249,3.91326598377977,-5.92524390554672));
#126770=CARTESIAN_POINT('',(4.99471684429243,3.82362522071687,-5.59489085202631));
#126771=CARTESIAN_POINT('Origin',(-0.100995931843701,4.017800660735,0.159369335230573));
#126772=CARTESIAN_POINT('Ctrl Pts',(4.82865340169588,3.78467661288032,-5.40801315977069));
#126773=CARTESIAN_POINT('Ctrl Pts',(4.8562052884917,3.79148855789405,-5.43919089353966));
#126774=CARTESIAN_POINT('Ctrl Pts',(4.88383838974289,3.79813533635186,-5.47036812749705));
#126775=CARTESIAN_POINT('Ctrl Pts',(4.93918600393071,3.81110763150659,-5.53264760509342));
#126776=CARTESIAN_POINT('Ctrl Pts',(4.96693316125902,3.81744079750135,-5.5637865717557));
#126777=CARTESIAN_POINT('Ctrl Pts',(4.99471684547528,3.82362522071682,-5.59489085096975));
#126778=CARTESIAN_POINT('Ctrl Pts',(5.405057563,3.913265985,-5.199553129));
#126779=CARTESIAN_POINT('Ctrl Pts',(5.359931982,3.903042157,-5.24646223));
#126780=CARTESIAN_POINT('Ctrl Pts',(5.313999035,3.892857143,-5.292581058));
#126781=CARTESIAN_POINT('Ctrl Pts',(5.070336803,3.838828313,-5.537229341));
#126782=CARTESIAN_POINT('Ctrl Pts',(4.805226477,3.783894965,-5.758454524));
#126783=CARTESIAN_POINT('Ctrl Pts',(5.386915907,3.913265985,-4.852178584));
#126784=CARTESIAN_POINT('Ctrl Pts',(5.3448051,3.903042157,-4.898930239));
#126785=CARTESIAN_POINT('Ctrl Pts',(5.301889206,3.892857143,-4.944943968));
#126786=CARTESIAN_POINT('Ctrl Pts',(5.074231646,3.838828313,-5.189034734));
#126787=CARTESIAN_POINT('Ctrl Pts',(4.825109518,3.783894965,-5.411175301));
#126788=CARTESIAN_POINT('',(5.40505755925474,3.9132659854451,-5.19955313187586));
#126789=CARTESIAN_POINT('Ctrl Pts',(4.9947168426979,3.82362522012808,-5.59489085356987));
#126790=CARTESIAN_POINT('Ctrl Pts',(5.10436650864171,3.84689293573234,-5.49700350466743));
#126791=CARTESIAN_POINT('Ctrl Pts',(5.21086754932514,3.86998912007495,-5.39612989562032));
#126792=CARTESIAN_POINT('Ctrl Pts',(5.31399903520763,3.89285714304604,-5.29258105779153));
#126793=CARTESIAN_POINT('Ctrl Pts',(5.34459108521124,3.899640519205,-5.26186520817721));
#126794=CARTESIAN_POINT('Ctrl Pts',(5.37494669178829,3.90644394833732,-5.23085408659784));
#126795=CARTESIAN_POINT('Ctrl Pts',(5.40505756040768,3.91326598441267,-5.19955313169478));
#126796=CARTESIAN_POINT('',(5.39598672949708,3.91326598631302,-5.02586586240818));
#126797=CARTESIAN_POINT('Origin',(1.03562991515815E-12,4.00453391999933,
-1.23989360445442E-12));
#126798=CARTESIAN_POINT('',(5.00007512100252,4.00345494156695,-5.59010275254307));
#126799=CARTESIAN_POINT('Origin',(-0.14085793492312,4.16057199345265,0.119913108511505));
#126800=CARTESIAN_POINT('Origin',(-0.126543208492973,4.01785425210612,0.144958433320892));
#126801=CARTESIAN_POINT('Ctrl Pts',(6.224422733,3.783915088,-4.184084325));
#126802=CARTESIAN_POINT('Ctrl Pts',(5.99701896,3.848090541,-4.5223799));
#126803=CARTESIAN_POINT('Ctrl Pts',(5.734290451,3.913265985,-4.834036928));
#126804=CARTESIAN_POINT('Ctrl Pts',(5.73165693591518,3.91391928492389,-4.83716088850072));
#126805=CARTESIAN_POINT('Ctrl Pts',(5.72902342083036,3.91457258484779,-4.84028484900144));
#126806=CARTESIAN_POINT('Ctrl Pts',(5.88106053800001,3.783915088,-4.239767323));
#126807=CARTESIAN_POINT('Ctrl Pts',(5.65063041,3.848090541,-4.559401263));
#126808=CARTESIAN_POINT('Ctrl Pts',(5.386915907,3.913265985,-4.852178584));
#126809=CARTESIAN_POINT('Ctrl Pts',(5.38427250859463,3.91391928492389,-4.85511329974243));
#126810=CARTESIAN_POINT('Ctrl Pts',(5.38162911018926,3.91457258484779,-4.85804801548486));
#126811=CARTESIAN_POINT('',(5.73429044772017,3.9132659845887,-4.83403693208736));
#126812=CARTESIAN_POINT('',(5.56060317398342,3.91326598377978,-4.84310776175977));
#126813=CARTESIAN_POINT('',(6.08067928922541,3.82362522067835,-4.39036893445263));
#126814=CARTESIAN_POINT('Origin',(-0.132894517210351,4.01780063623296,0.133932311186329));
#126815=CARTESIAN_POINT('Ctrl Pts',(5.87832513986311,3.78467661310213,-4.24355907047409));
#126816=CARTESIAN_POINT('Ctrl Pts',(5.91193524479655,3.79148857330863,-4.26808509992057));
#126817=CARTESIAN_POINT('Ctrl Pts',(5.94562456780292,3.79813536728978,-4.2925931888642));
#126818=CARTESIAN_POINT('Ctrl Pts',(6.01306644055515,3.81110766408669,-4.34151851229078));
#126819=CARTESIAN_POINT('Ctrl Pts',(6.04685903415429,3.81744086360286,-4.36596478657745));
#126820=CARTESIAN_POINT('Ctrl Pts',(6.08067929013269,3.82362522067827,-4.3903689331953));
#126821=CARTESIAN_POINT('Ctrl Pts',(6.396440546,3.913265985,-3.916062862));
#126822=CARTESIAN_POINT('Ctrl Pts',(6.362454046,3.903042157,-3.971575921));
#126823=CARTESIAN_POINT('Ctrl Pts',(6.327509171,3.892857143,-4.026490742));
#126824=CARTESIAN_POINT('Ctrl Pts',(6.142135775,3.838828313,-4.317799462));
#126825=CARTESIAN_POINT('Ctrl Pts',(5.930780456,3.783894965,-4.590843406));
#126826=CARTESIAN_POINT('Ctrl Pts',(6.304047773,3.913265985,-3.580709661));
#126827=CARTESIAN_POINT('Ctrl Pts',(6.272971717,3.903042157,-3.635420867));
#126828=CARTESIAN_POINT('Ctrl Pts',(6.240950764,3.892857143,-3.68958447));
#126829=CARTESIAN_POINT('Ctrl Pts',(6.07108801100001,3.838828313,-3.976908175));
#126830=CARTESIAN_POINT('Ctrl Pts',(5.875543876,3.783894965,-4.247409112));
#126831=CARTESIAN_POINT('',(6.39644054272282,3.91326598544903,-3.91606286599203));
#126832=CARTESIAN_POINT('Ctrl Pts',(6.08067928814615,3.82362522012804,-4.3903689362603));
#126833=CARTESIAN_POINT('Ctrl Pts',(6.16672251947261,3.8468929357323,-4.27119870229895));
#126834=CARTESIAN_POINT('Ctrl Pts',(6.24904878106583,3.86998912007446,-4.14978888647607));
#126835=CARTESIAN_POINT('Ctrl Pts',(6.3275091708798,3.89285714297538,-4.02649074199364));
#126836=CARTESIAN_POINT('Ctrl Pts',(6.35078299564904,3.89964051911324,-3.98991662566928));
#126837=CARTESIAN_POINT('Ctrl Pts',(6.37376243079214,3.90644394833732,-3.95310496831084));
#126838=CARTESIAN_POINT('Ctrl Pts',(6.39644054404758,3.91326598441267,-3.91606286518905));
#126839=CARTESIAN_POINT('',(6.35024415539581,3.91326598631302,-3.74838626845302));
#126840=CARTESIAN_POINT('Origin',(-1.17093834628434E-13,4.00453392000044,
1.46150452851046E-13));
#126841=CARTESIAN_POINT('',(6.08488299311143,4.00345494165009,-4.38454090602215));
#126842=CARTESIAN_POINT('Origin',(-0.163342471740709,4.16057201846061,0.0868292585406771));
#126843=CARTESIAN_POINT('Origin',(-0.154746379352955,4.01785422327006,0.114366264473377));
#126844=CARTESIAN_POINT('Ctrl Pts',(6.97900989537378,3.783915088,-2.74793569772871));
#126845=CARTESIAN_POINT('Ctrl Pts',(6.829660385282,3.848090541,-3.12724286712813));
#126846=CARTESIAN_POINT('Ctrl Pts',(6.64008156229168,3.913265985,-3.48812937990599));
#126847=CARTESIAN_POINT('Ctrl Pts',(6.63362426926477,3.91548594255344,-3.50042162819467));
#126848=CARTESIAN_POINT('Ctrl Pts',(6.62716697623774,3.91770590010688,-3.51271387648341));
#126849=CARTESIAN_POINT('Ctrl Pts',(6.654989258,3.783915088,-2.876389747));
#126850=CARTESIAN_POINT('Ctrl Pts',(6.498658307,3.848090541,-3.238086488));
#126851=CARTESIAN_POINT('Ctrl Pts',(6.304047773,3.913265985,-3.580709661));
#126852=CARTESIAN_POINT('Ctrl Pts',(6.29741909357082,3.91548594255344,-3.59237983697737));
#126853=CARTESIAN_POINT('Ctrl Pts',(6.2907904141416,3.91770590010688,-3.60405001295468));
#126854=CARTESIAN_POINT('',(6.63940096982187,3.91326598502339,-3.48831689502031));
#126855=CARTESIAN_POINT('',(6.47172436983887,3.91326598377977,-3.53451328120357));
#126856=CARTESIAN_POINT('',(6.88231592933023,3.82362522069825,-2.98055824466829));
#126857=CARTESIAN_POINT('Origin',(-0.15857890756012,4.01780063905968,0.102232605658803));
#126858=CARTESIAN_POINT('Ctrl Pts',(6.65313292416621,3.78467661285622,-2.88068087466204));
#126859=CARTESIAN_POINT('Ctrl Pts',(6.69122961500491,3.79148857305671,-2.89740831972643));
#126860=CARTESIAN_POINT('Ctrl Pts',(6.72939981611138,3.79813536720143,-2.91410121473867));
#126861=CARTESIAN_POINT('Ctrl Pts',(6.80578224859457,3.81110763252607,-2.94738460114917));
#126862=CARTESIAN_POINT('Ctrl Pts',(6.84403980611034,3.81744079956995,-2.96399483581662));
#126863=CARTESIAN_POINT('Ctrl Pts',(6.88231592994026,3.82362522069821,-2.9805582432586));
#126864=CARTESIAN_POINT('Ctrl Pts',(7.088733078,3.913265985,-2.449461849));
#126865=CARTESIAN_POINT('Ctrl Pts',(7.06747483,3.903042157,-2.510983136));
#126866=CARTESIAN_POINT('Ctrl Pts',(7.04515201,3.892857143,-2.572126194));
#126867=CARTESIAN_POINT('Ctrl Pts',(6.926735305,3.838828313,-2.896474078));
#126868=CARTESIAN_POINT('Ctrl Pts',(6.779017733,3.783894965,-3.208569553));
#126869=CARTESIAN_POINT('Ctrl Pts',(6.926409371,3.913265985,-2.141810735));
#126870=CARTESIAN_POINT('Ctrl Pts',(6.907821148,3.903042157,-2.201923256));
#126871=CARTESIAN_POINT('Ctrl Pts',(6.888192401,3.892857143,-2.261704102));
#126872=CARTESIAN_POINT('Ctrl Pts',(6.784067048,3.838828313,-2.578825809));
#126873=CARTESIAN_POINT('Ctrl Pts',(6.65124433100001,3.783894965,-2.885038794));
#126874=CARTESIAN_POINT('',(7.08873307580789,3.9132659854451,-2.44946185318189));
#126875=CARTESIAN_POINT('Ctrl Pts',(6.88231592855685,3.82362522012813,-2.9805582466734));
#126876=CARTESIAN_POINT('Ctrl Pts',(6.94072943918886,3.84689293573239,-2.84567739513467));
#126877=CARTESIAN_POINT('Ctrl Pts',(6.99503143687744,3.86998912007453,-2.70940836070635));
#126878=CARTESIAN_POINT('Ctrl Pts',(7.04515200990613,3.89285714297705,-2.57212619405164));
#126879=CARTESIAN_POINT('Ctrl Pts',(7.0600193517086,3.8996405191154,-2.53140397600461));
#126880=CARTESIAN_POINT('Ctrl Pts',(7.0745481222804,3.90644394833732,-2.49051305559514));
#126881=CARTESIAN_POINT('Ctrl Pts',(7.08873307677877,3.91326598441267,-2.44946185253423));
#126882=CARTESIAN_POINT('',(7.00757122198645,3.91326598631302,-2.29563629967278));
#126883=CARTESIAN_POINT('Origin',(-1.25247034965525E-12,4.00453392000044,
6.18862600054726E-13));
#126884=CARTESIAN_POINT('',(6.88516849880378,4.00345494158127,-2.9739628013933));
#126885=CARTESIAN_POINT('Origin',(-0.178189687407482,4.16057206045661,0.0496855948308278));
#126886=CARTESIAN_POINT('Origin',(-0.175713817176157,4.01785418818641,0.0784265254962754));
#126887=CARTESIAN_POINT('Ctrl Pts',(7.405984482,3.783915088,-1.183804818));
#126888=CARTESIAN_POINT('Ctrl Pts',(7.341645033,3.848090541,-1.586317932));
#126889=CARTESIAN_POINT('Ctrl Pts',(7.234060485,3.913265985,-1.979487028));
#126890=CARTESIAN_POINT('Ctrl Pts',(7.23298208840295,3.91391928492389,-1.98342804204961));
#126891=CARTESIAN_POINT('Ctrl Pts',(7.23190369180592,3.91457258484779,-1.98736905609922));
#126892=CARTESIAN_POINT('Ctrl Pts',(7.117738078,3.783915088,-1.378515382));
#126893=CARTESIAN_POINT('Ctrl Pts',(7.042816165,3.848090541,-1.765362388));
#126894=CARTESIAN_POINT('Ctrl Pts',(6.92640937100001,3.913265985,-2.141810735));
#126895=CARTESIAN_POINT('Ctrl Pts',(6.92524254274394,3.91391928492389,-2.14558414506598));
#126896=CARTESIAN_POINT('Ctrl Pts',(6.92407571448788,3.91457258484779,-2.14935755513196));
#126897=CARTESIAN_POINT('',(7.23406048375419,3.9132659845887,-1.97948703307904));
#126898=CARTESIAN_POINT('',(7.08023492586553,3.91326598377977,-2.06064888883387));
#126899=CARTESIAN_POINT('',(7.36214312522358,3.82362522066215,-1.43137996415906));
#126900=CARTESIAN_POINT('Origin',(-0.176848370913549,4.01780060574887,0.0657526788448023));
#126901=CARTESIAN_POINT('Ctrl Pts',(7.11684761097684,3.78467661312194,-1.38310524299807));
#126902=CARTESIAN_POINT('Ctrl Pts',(7.15764952855394,3.79148857330044,-1.39125194736918));
#126903=CARTESIAN_POINT('Ctrl Pts',(7.19851580975261,3.79813536730619,-1.39934910677069));
#126904=CARTESIAN_POINT('Ctrl Pts',(7.2802674200159,3.81110763459257,-1.41543438358567));
#126905=CARTESIAN_POINT('Ctrl Pts',(7.32120126067541,3.81744080367663,-1.42343203901384));
#126906=CARTESIAN_POINT('Ctrl Pts',(7.36214312549663,3.82362522066195,-1.43137996274802));
#126907=CARTESIAN_POINT('Ctrl Pts',(7.44956433,3.913265985,-0.868326722));
#126908=CARTESIAN_POINT('Ctrl Pts',(7.442028346,3.903042157,-0.93297957));
#126909=CARTESIAN_POINT('Ctrl Pts',(7.433371371,3.892857143,-0.997491884));
#126910=CARTESIAN_POINT('Ctrl Pts',(7.38744839000001,3.838828313,-1.339712786));
#126911=CARTESIAN_POINT('Ctrl Pts',(7.310275675,3.783894965,-1.676266553));
#126912=CARTESIAN_POINT('Ctrl Pts',(7.224899766,3.913265985,-0.602763118));
#126913=CARTESIAN_POINT('Ctrl Pts',(7.21966854,3.903042157,-0.665466161));
#126914=CARTESIAN_POINT('Ctrl Pts',(7.213349817,3.892857143,-0.728068964));
#126915=CARTESIAN_POINT('Ctrl Pts',(7.17983065,3.838828313,-1.060160415));
#126916=CARTESIAN_POINT('Ctrl Pts',(7.115939995,3.783894965,-1.387767269));
#126917=CARTESIAN_POINT('',(7.44956432875072,3.91326598544511,-0.868326726546466));
#126918=CARTESIAN_POINT('Ctrl Pts',(7.36214312491588,3.82362522012806,-1.43137996614573));
#126919=CARTESIAN_POINT('Ctrl Pts',(7.39019556395953,3.84689293573232,-1.28709537604623));
#126920=CARTESIAN_POINT('Ctrl Pts',(7.41393419676835,3.8699891200747,-1.14233891164205));
#126921=CARTESIAN_POINT('Ctrl Pts',(7.4333713710084,3.89285714300989,-0.997491883937365));
#126922=CARTESIAN_POINT('Ctrl Pts',(7.43913704965416,3.89964051915805,-0.954525689482439));
#126923=CARTESIAN_POINT('Ctrl Pts',(7.44453580649954,3.90644394833731,-0.911467520086951));
#126924=CARTESIAN_POINT('Ctrl Pts',(7.44956432956707,3.91326598441266,-0.868326725714184));
#126925=CARTESIAN_POINT('',(7.33723204719462,3.91326598631305,-0.735544928033871));
#126926=CARTESIAN_POINT('Origin',(-1.03649727689614E-13,4.00453392000044,
4.01154803819637E-14));
#126927=CARTESIAN_POINT('',(7.36351117796384,4.0034549415695,-1.42432549981701));
#126928=CARTESIAN_POINT('Origin',(-0.184704478685992,4.16057204671496,0.010218425212104));
#126929=CARTESIAN_POINT('Origin',(-0.188465182015064,4.01785424450927,0.0388197041150465));
#126930=CARTESIAN_POINT('Ctrl Pts',(7.48753937344939,3.783915088,0.436170706963458));
#126931=CARTESIAN_POINT('Ctrl Pts',(7.51124512463192,3.848090541,0.0292251070786374));
#126932=CARTESIAN_POINT('Ctrl Pts',(7.49070676901765,3.913265985,-0.37789263964191));
#126933=CARTESIAN_POINT('Ctrl Pts',(7.49039083490264,3.91426855534244,-0.384155185068383));
#126934=CARTESIAN_POINT('Ctrl Pts',(7.49007490078761,3.91527112568487,-0.390417730494854));
#126935=CARTESIAN_POINT('Ctrl Pts',(7.247669375,3.783915088,0.183816829));
#126936=CARTESIAN_POINT('Ctrl Pts',(7.257659767,3.848090541,-0.210091905));
#126937=CARTESIAN_POINT('Ctrl Pts',(7.224899766,3.913265985,-0.602763118));
#126938=CARTESIAN_POINT('Ctrl Pts',(7.22439583072308,3.91426855534243,-0.608803437609964));
#126939=CARTESIAN_POINT('Ctrl Pts',(7.22389189544616,3.91527112568487,-0.614843757219925));
#126940=CARTESIAN_POINT('',(7.35768156699201,3.91326598377978,-0.490430843621213));
#126941=CARTESIAN_POINT('Ctrl Pts',(7.24778641174106,3.7846766131314,0.179142852983126));
#126942=CARTESIAN_POINT('Ctrl Pts',(7.28938570379294,3.7914885733155,0.179957820111429));
#126943=CARTESIAN_POINT('Ctrl Pts',(7.3310372038869,3.79813536731177,0.180835010192609));
#126944=CARTESIAN_POINT('Ctrl Pts',(7.41433536513795,3.811107634472,0.182699977771355));
#126945=CARTESIAN_POINT('Ctrl Pts',(7.45603145391974,3.81744080342295,0.18368886879813));
#126946=CARTESIAN_POINT('Ctrl Pts',(7.49772469110044,3.82362522066469,0.184728053864386));
#126947=CARTESIAN_POINT('Ctrl Pts',(7.46206223300001,3.913265985,0.753410398));
#126948=CARTESIAN_POINT('Ctrl Pts',(7.468600888,3.903042157,0.688649083));
#126949=CARTESIAN_POINT('Ctrl Pts',(7.474014549,3.892857143,0.623784038));
#126950=CARTESIAN_POINT('Ctrl Pts',(7.502732599,3.838828313,0.279691987));
#126951=CARTESIAN_POINT('Ctrl Pts',(7.499713251,3.783894965,-0.065583193));
#126952=CARTESIAN_POINT('Ctrl Pts',(7.185561877,3.913265985,0.964469032));
#126953=CARTESIAN_POINT('Ctrl Pts',(7.19393225500001,3.903042157,0.902107393));
#126954=CARTESIAN_POINT('Ctrl Pts',(7.201219013,3.892857143,0.839609869));
#126955=CARTESIAN_POINT('Ctrl Pts',(7.23987335,3.838828313,0.508076902));
#126956=CARTESIAN_POINT('Ctrl Pts',(7.247902213,3.783894965,0.174394712));
#126957=CARTESIAN_POINT('',(7.32381205594047,3.91326598631302,0.858939706981007));
#126958=CARTESIAN_POINT('Ctrl Pts',(7.21892121262391,3.783915088,2.03590428179448));
#126959=CARTESIAN_POINT('Ctrl Pts',(7.32957202129409,3.848090541,1.64355800233434));
#126960=CARTESIAN_POINT('Ctrl Pts',(7.39704884754676,3.913265985,1.24153053636633));
#126961=CARTESIAN_POINT('Ctrl Pts',(7.3993471930232,3.91548594250557,1.22783697578976));
#126962=CARTESIAN_POINT('Ctrl Pts',(7.4016455384996,3.91770590001114,1.21414341521315));
#126963=CARTESIAN_POINT('Ctrl Pts',(7.038707708,3.783915088,1.73755397));
#126964=CARTESIAN_POINT('Ctrl Pts',(7.133143264,3.848090541,1.355002242));
#126965=CARTESIAN_POINT('Ctrl Pts',(7.185561877,3.913265985,0.964469032));
#126966=CARTESIAN_POINT('Ctrl Pts',(7.18734732081472,3.91548594250557,0.951166980222463));
#126967=CARTESIAN_POINT('Ctrl Pts',(7.18913276462937,3.91770590001114,0.937864928444939));
#126968=CARTESIAN_POINT('',(7.39662051189907,3.91326598502339,1.24096937987799));
#126969=CARTESIAN_POINT('',(7.29109119514221,3.91326598377978,1.10271920244776));
#126970=CARTESIAN_POINT('',(7.282720983891,3.82362522068904,1.79219839063914));
#126971=CARTESIAN_POINT('Origin',(-0.188112269141258,4.01780062535348,-0.0145812353583524));
#126972=CARTESIAN_POINT('Ctrl Pts',(7.03982677471336,3.78467661306702,1.73301442817107));
#126973=CARTESIAN_POINT('Ctrl Pts',(7.08027830455524,3.79148857324013,1.74275295989348));
#126974=CARTESIAN_POINT('Ctrl Pts',(7.12076744619297,3.79813536730068,1.75256348314844));
#126975=CARTESIAN_POINT('Ctrl Pts',(7.20171741464376,3.81110766407564,1.77229153622958));
#126976=CARTESIAN_POINT('Ctrl Pts',(7.24222629903117,3.81744086360407,1.78222078615965));
#126977=CARTESIAN_POINT('Ctrl Pts',(7.28272098352246,3.82362522068899,1.7921983921349));
#126978=CARTESIAN_POINT('Ctrl Pts',(7.1256424,3.913265985,2.339918885));
#126979=CARTESIAN_POINT('Ctrl Pts',(7.145949953,3.903042157,2.278077271));
#126980=CARTESIAN_POINT('Ctrl Pts',(7.165181113,3.892857143,2.215892511));
#126981=CARTESIAN_POINT('Ctrl Pts',(7.267197371,3.838828313,1.886018673));
#126982=CARTESIAN_POINT('Ctrl Pts',(7.338472571,3.783894965,1.548166765));
#126983=CARTESIAN_POINT('Ctrl Pts',(6.810235101,3.913265985,2.486603681));
#126984=CARTESIAN_POINT('Ctrl Pts',(6.831815693,3.903042157,2.427499407));
#126985=CARTESIAN_POINT('Ctrl Pts',(6.852367211,3.892857143,2.368029478));
#126986=CARTESIAN_POINT('Ctrl Pts',(6.96138761900001,3.838828313,2.052557107));
#126987=CARTESIAN_POINT('Ctrl Pts',(7.040960579,3.783894965,1.72840219));
#126988=CARTESIAN_POINT('',(7.12564240078609,3.91326598544483,2.33991888034567));
#126989=CARTESIAN_POINT('Ctrl Pts',(7.28272098452153,3.82362522012728,1.79219838860444));
#126990=CARTESIAN_POINT('Ctrl Pts',(7.24759716170778,3.84689293573178,1.93492644936675));
#126991=CARTESIAN_POINT('Ctrl Pts',(7.20836009960477,3.86998912007441,2.07627145146909));
#126992=CARTESIAN_POINT('Ctrl Pts',(7.16518111287426,3.89285714300848,2.21589251110512));
#126993=CARTESIAN_POINT('Ctrl Pts',(7.15237286416935,3.89964051915622,2.25730851876993));
#126994=CARTESIAN_POINT('Ctrl Pts',(7.139192987011,3.90644394833732,2.29865393432783));
#126995=CARTESIAN_POINT('Ctrl Pts',(7.1256424011666,3.91326598441267,2.33991888144739));
#126996=CARTESIAN_POINT('',(6.96793875314233,3.91326598631302,2.41326127537066));
#126997=CARTESIAN_POINT('Origin',(6.26235174827627E-13,4.00453392000022,
1.57751416096641E-13));
#126998=CARTESIAN_POINT('',(7.28100050215491,4.00345494179838,1.79917527897799));
#126999=CARTESIAN_POINT('Origin',(-0.171923644953278,4.16057201721044,-0.0682813678646113));
#127000=CARTESIAN_POINT('Origin',(-0.187346446645758,4.01785439732041,-0.0439026729701864));
#127001=CARTESIAN_POINT('Ctrl Pts',(6.61248760692043,3.783915088,3.54016064187857));
#127002=CARTESIAN_POINT('Ctrl Pts',(6.80489431323841,3.848090541,3.18077385319475));
#127003=CARTESIAN_POINT('Ctrl Pts',(6.95721758996345,3.913265985,2.80265108972526));
#127004=CARTESIAN_POINT('Ctrl Pts',(6.96240591211869,3.91548594249667,2.78977175339997));
#127005=CARTESIAN_POINT('Ctrl Pts',(6.967594234274,3.91770589999335,2.77689241707473));
#127006=CARTESIAN_POINT('Ctrl Pts',(6.50062389200001,3.783915088,3.210045018));
#127007=CARTESIAN_POINT('Ctrl Pts',(6.67508891,3.848090541,2.85673799));
#127008=CARTESIAN_POINT('Ctrl Pts',(6.81023510100001,3.913265985,2.486603681));
#127009=CARTESIAN_POINT('Ctrl Pts',(6.8148383500374,3.91548594249667,2.47399644146913));
#127010=CARTESIAN_POINT('Ctrl Pts',(6.81944159907491,3.91770589999335,2.46138920193821));
#127011=CARTESIAN_POINT('',(6.95691990064213,3.91326598502339,2.8020109732692));
#127012=CARTESIAN_POINT('',(6.88357750223904,3.91326598377977,2.64430732386983));
#127013=CARTESIAN_POINT('',(6.72718533731447,3.82362522065873,3.31586752406077));
#127014=CARTESIAN_POINT('Origin',(-0.180579847175079,4.01780064981072,-0.054678938592192));
#127015=CARTESIAN_POINT('Ctrl Pts',(6.50269266259973,3.78467661305534,3.20585217381019));
#127016=CARTESIAN_POINT('Ctrl Pts',(6.54010496184601,3.79148857326335,3.22405890755018));
#127017=CARTESIAN_POINT('Ctrl Pts',(6.57753851684415,3.79813536723926,3.24234403476636));
#127018=CARTESIAN_POINT('Ctrl Pts',(6.65235497190099,3.81110766404678,3.27901270766542));
#127019=CARTESIAN_POINT('Ctrl Pts',(6.68978228575723,3.81744086356219,3.29741803003803));
#127020=CARTESIAN_POINT('Ctrl Pts',(6.72718533666519,3.82362522064911,3.31586752538029));
#127021=CARTESIAN_POINT('Ctrl Pts',(6.456035448,3.913265985,3.817015365));
#127022=CARTESIAN_POINT('Ctrl Pts',(6.48916234,3.903042157,3.760985098));
#127023=CARTESIAN_POINT('Ctrl Pts',(6.521311771,3.892857143,3.704388314));
#127024=CARTESIAN_POINT('Ctrl Pts',(6.691856071,3.838828313,3.404157223));
#127025=CARTESIAN_POINT('Ctrl Pts',(6.83409306900001,3.783894965,3.089526165));
#127026=CARTESIAN_POINT('Ctrl Pts',(6.116469301,3.913265985,3.892467507));
#127027=CARTESIAN_POINT('Ctrl Pts',(6.15025102300001,3.903042157,3.839384247));
#127028=CARTESIAN_POINT('Ctrl Pts',(6.183106334,3.892857143,3.785722661));
#127029=CARTESIAN_POINT('Ctrl Pts',(6.35739514,3.838828313,3.501062024));
#127030=CARTESIAN_POINT('Ctrl Pts',(6.504791453,3.783894965,3.201591502));
#127031=CARTESIAN_POINT('',(6.45603544999917,3.91326598587966,3.81701536011091));
#127032=CARTESIAN_POINT('Ctrl Pts',(6.72718533822867,3.82362522012764,3.31586752225138));
#127033=CARTESIAN_POINT('Ctrl Pts',(6.66220037684142,3.84689293573204,3.44770809685697));
#127034=CARTESIAN_POINT('Ctrl Pts',(6.59349565802203,3.86998912007451,3.57731372301597));
#127035=CARTESIAN_POINT('Ctrl Pts',(6.52131177123793,3.89285714276323,3.70438831419086));
#127036=CARTESIAN_POINT('Ctrl Pts',(6.49989975501614,3.89964051914521,3.74208264361581));
#127037=CARTESIAN_POINT('Ctrl Pts',(6.47813997398258,3.90644394874722,3.77962814197985));
#127038=CARTESIAN_POINT('Ctrl Pts',(6.45603544995081,3.91326598565651,3.81701536137577));
#127039=CARTESIAN_POINT('',(6.28625237872063,3.91326598631302,3.85474142911706));
#127040=CARTESIAN_POINT('Origin',(6.58761240002192E-13,4.00453391999933,
3.91613824701764E-13));
#127041=CARTESIAN_POINT('',(6.72400525501397,4.00345494160178,3.32231144352664));
#127042=CARTESIAN_POINT('Origin',(-0.153225813809006,4.16057200299011,-0.103643539873452));
#127043=CARTESIAN_POINT('Origin',(-0.173528731529875,4.01785423819475,-0.0831502913203769));
#127044=CARTESIAN_POINT('Ctrl Pts',(5.69686142934184,3.783915088,4.87888302588861));
#127045=CARTESIAN_POINT('Ctrl Pts',(5.96202731116912,3.848090541,4.56926025475706));
#127046=CARTESIAN_POINT('Ctrl Pts',(6.19207457063733,3.913265985,4.23272279231243));
#127047=CARTESIAN_POINT('Ctrl Pts',(6.19991026931688,3.91548594250644,4.2212599035295));
#127048=CARTESIAN_POINT('Ctrl Pts',(6.20774596799649,3.91770590001281,4.20979701474663));
#127049=CARTESIAN_POINT('Ctrl Pts',(5.658578127,3.783915088,4.53243792899999));
#127050=CARTESIAN_POINT('Ctrl Pts',(5.904914818,3.848090541,4.224895844));
#127051=CARTESIAN_POINT('Ctrl Pts',(6.116469301,3.913265985,3.892467507));
#127052=CARTESIAN_POINT('Ctrl Pts',(6.12367511247948,3.91548594250644,3.88114458019227));
#127053=CARTESIAN_POINT('Ctrl Pts',(6.13088092395888,3.91770590001281,3.86982165338449));
#127054=CARTESIAN_POINT('',(6.19192144724153,3.91326598502339,4.23203364701685));
#127055=CARTESIAN_POINT('',(6.15419537620777,3.91326598377977,4.06225057412534));
#127056=CARTESIAN_POINT('',(5.8570939813402,3.82362522065945,4.68449037745577));
#127057=CARTESIAN_POINT('Origin',(-0.164603298449912,4.01780062929309,-0.0922196567071654));
#127058=CARTESIAN_POINT('Ctrl Pts',(5.66149986785939,3.78467661292693,4.52878783530389));
#127059=CARTESIAN_POINT('Ctrl Pts',(5.69412357866396,3.79148857310069,4.55461144403524));
#127060=CARTESIAN_POINT('Ctrl Pts',(5.72675119669208,3.79813536718563,4.58051618334602));
#127061=CARTESIAN_POINT('Ctrl Pts',(5.79193565618604,3.81110763458452,4.63241077165652));
#127062=CARTESIAN_POINT('Ctrl Pts',(5.82453117336164,3.81744080378591,4.65843141993921));
#127063=CARTESIAN_POINT('Ctrl Pts',(5.85709398044422,3.82362522065944,4.68449037857536));
#127064=CARTESIAN_POINT('Ctrl Pts',(5.48455145300001,3.913265985,5.115632449));
#127065=CARTESIAN_POINT('Ctrl Pts',(5.528948709,3.903042157,5.068033441));
#127066=CARTESIAN_POINT('Ctrl Pts',(5.57251314,3.892857143,5.019671036));
#127067=CARTESIAN_POINT('Ctrl Pts',(5.803611018,3.838828313,4.763121164));
#127068=CARTESIAN_POINT('Ctrl Pts',(6.010158971,3.783894965,4.486422756));
#127069=CARTESIAN_POINT('Ctrl Pts',(5.136704194,3.913265985,5.116323878));
#127070=CARTESIAN_POINT('Ctrl Pts',(5.18110745,3.903042157,5.071743746));
#127071=CARTESIAN_POINT('Ctrl Pts',(5.224730277,3.892857143,5.026399659));
#127072=CARTESIAN_POINT('Ctrl Pts',(5.45613793,3.838828313,4.785861171));
#127073=CARTESIAN_POINT('Ctrl Pts',(5.664465509,3.783894965,4.525077954));
#127074=CARTESIAN_POINT('',(5.48455145598281,3.91326598544904,5.11563244476761));
#127075=CARTESIAN_POINT('Ctrl Pts',(5.85709398265966,3.82362522012791,4.68449037594388));
#127076=CARTESIAN_POINT('Ctrl Pts',(5.76528650735208,3.84689293573221,4.79927874531267));
#127077=CARTESIAN_POINT('Ctrl Pts',(5.67032668828692,3.86998912007453,4.91108478021124));
#127078=CARTESIAN_POINT('Ctrl Pts',(5.57251313993674,3.89285714299297,5.01967103596844));
#127079=CARTESIAN_POINT('Ctrl Pts',(5.54349855809972,3.89964051913609,5.05188114233675));
#127080=CARTESIAN_POINT('Ctrl Pts',(5.51417633597186,3.90644394833732,5.08387113827877));
#127081=CARTESIAN_POINT('Ctrl Pts',(5.48455145555049,3.91326598441267,5.11563244626558));
#127082=CARTESIAN_POINT('',(5.31062782910159,3.91326598631302,5.11597815768528));
#127083=CARTESIAN_POINT('Origin',(8.0708009719821E-13,4.00453392000044,
6.55725473919233E-13));
#127084=CARTESIAN_POINT('',(5.85260299487725,4.00345494155467,4.69010001812929));
#127085=CARTESIAN_POINT('Origin',(-0.127363302147928,4.16057203396705,-0.134159530637787));
#127086=CARTESIAN_POINT('Origin',(-0.151596600062219,4.01785425931465,-0.118509602027252));
#127087=CARTESIAN_POINT('Ctrl Pts',(4.51485634319997,3.783915088,5.98947426037819));
#127088=CARTESIAN_POINT('Ctrl Pts',(4.84038253734848,3.848090541,5.74409312384617));
#127089=CARTESIAN_POINT('Ctrl Pts',(5.13739702623243,3.913265985,5.46487708158082));
#127090=CARTESIAN_POINT('Ctrl Pts',(5.14751371322919,3.91548594258288,5.45536663205805));
#127091=CARTESIAN_POINT('Ctrl Pts',(5.15763040022591,3.9177059001657,5.44585618253516));
#127092=CARTESIAN_POINT('Ctrl Pts',(4.551943538,3.783915088,5.64289908));
#127093=CARTESIAN_POINT('Ctrl Pts',(4.858633471,3.848090541,5.395502265));
#127094=CARTESIAN_POINT('Ctrl Pts',(5.136704194,3.913265985,5.11632387800001));
#127095=CARTESIAN_POINT('Ctrl Pts',(5.14617563250833,3.91548594258288,5.1068147110629));
#127096=CARTESIAN_POINT('Ctrl Pts',(5.15564707101679,3.9177059001657,5.09730554412581));
#127097=CARTESIAN_POINT('',(5.13739562869265,3.91326598502339,5.46417113114432));
#127098=CARTESIAN_POINT('',(5.13704991397976,3.91326598377977,5.29024750217892));
#127099=CARTESIAN_POINT('',(4.71313142014474,3.82362522063888,5.83407166691751));
#127100=CARTESIAN_POINT('Origin',(-0.140930620901902,4.01780066783773,-0.125448627999198));
#127101=CARTESIAN_POINT('Ctrl Pts',(4.55558163274279,3.784676613028,5.6399624125463));
#127102=CARTESIAN_POINT('Ctrl Pts',(4.58189130678319,3.7914885732022,5.67219541290958));
#127103=CARTESIAN_POINT('Ctrl Pts',(4.60818735596335,3.79813536726801,5.70450848694832));
#127104=CARTESIAN_POINT('Ctrl Pts',(4.66069215544137,3.81110766403254,5.76920268671428));
#127105=CARTESIAN_POINT('Ctrl Pts',(4.68693207139744,3.81744086356028,5.80162222601506));
#127106=CARTESIAN_POINT('Ctrl Pts',(4.7131314190678,3.8236252206388,5.83407166778703));
#127107=CARTESIAN_POINT('Ctrl Pts',(4.256615929,3.913265985,6.175048246));
#127108=CARTESIAN_POINT('Ctrl Pts',(4.310207581,3.903042157,6.138106173));
#127109=CARTESIAN_POINT('Ctrl Pts',(4.363149987,3.892857143,6.100239519));
#127110=CARTESIAN_POINT('Ctrl Pts',(4.643995564,3.838828313,5.899366853));
#127111=CARTESIAN_POINT('Ctrl Pts',(4.905196519,3.783894965,5.673539205));
#127112=CARTESIAN_POINT('Ctrl Pts',(3.916752508,3.913265985,6.100946631));
#127113=CARTESIAN_POINT('Ctrl Pts',(3.969701051,3.903042157,6.06695414500001));
#127114=CARTESIAN_POINT('Ctrl Pts',(4.022051639,3.892857143,6.032047796));
#127115=CARTESIAN_POINT('Ctrl Pts',(4.299757775,3.838828313,5.846878769));
#127116=CARTESIAN_POINT('Ctrl Pts',(4.559275454,3.783894965,5.636976791));
#127117=CARTESIAN_POINT('',(4.25661593240909,3.91326598544479,6.17504824276322));
#127118=CARTESIAN_POINT('Ctrl Pts',(4.71313142169647,3.82362522012804,5.83407166577598));
#127119=CARTESIAN_POINT('Ctrl Pts',(4.59879424790011,3.8468929357323,5.92644045331317));
#127120=CARTESIAN_POINT('Ctrl Pts',(4.48201954411058,3.86998912007458,6.015218971059));
#127121=CARTESIAN_POINT('Ctrl Pts',(4.36314998703682,3.89285714299292,6.10023951897366));
#127122=CARTESIAN_POINT('Ctrl Pts',(4.32788952948444,3.89964051913601,6.1254592935724));
#127123=CARTESIAN_POINT('Ctrl Pts',(4.29237594126452,3.90644394833732,6.15039797052489));
#127124=CARTESIAN_POINT('Ctrl Pts',(4.25661593207867,3.91326598441268,6.17504824387779));
#127125=CARTESIAN_POINT('',(4.08668422522062,3.91326598631302,6.1379974340254));
#127126=CARTESIAN_POINT('Origin',(-6.90419943438769E-13,4.00453391999933,
-8.03176969377262E-13));
#127127=CARTESIAN_POINT('',(4.70753952324103,4.00345494176913,5.83858472873869));
#127128=CARTESIAN_POINT('Origin',(-0.0955451242393152,4.1605720476159,-0.158402113833271));
#127129=CARTESIAN_POINT('Origin',(-0.122576384829521,4.01785438464529,-0.148327773608642));
#127130=CARTESIAN_POINT('Ctrl Pts',(3.12174159235361,3.783915088,6.82000433694904));
#127131=CARTESIAN_POINT('Ctrl Pts',(3.49240685596093,3.848090541,6.65033858412427));
#127132=CARTESIAN_POINT('Ctrl Pts',(3.84250050621632,3.913265985,6.44149979260178));
#127133=CARTESIAN_POINT('Ctrl Pts',(3.85442513550379,3.91548594245362,6.43438648115518));
#127134=CARTESIAN_POINT('Ctrl Pts',(3.8663497647913,3.91770589990719,6.42727316970848));
#127135=CARTESIAN_POINT('Ctrl Pts',(3.232465128,3.783915088,6.489504542));
#127136=CARTESIAN_POINT('Ctrl Pts',(3.585167823,3.848090541,6.313820997));
#127137=CARTESIAN_POINT('Ctrl Pts',(3.916752508,3.913265985,6.100946631));
#127138=CARTESIAN_POINT('Ctrl Pts',(3.92804669869196,3.91548594245362,6.09369586281981));
#127139=CARTESIAN_POINT('Ctrl Pts',(3.93934088938394,3.91770589990718,6.08644509463963));
#127140=CARTESIAN_POINT('',(3.84265089985369,3.91326598502339,6.44081004656437));
#127141=CARTESIAN_POINT('',(3.87970170699552,3.91326598377977,6.27087833698131));
#127142=CARTESIAN_POINT('',(3.34878807226981,3.82362522063631,6.71085824953841));
#127143=CARTESIAN_POINT('Origin',(-0.110667850082253,4.01780063234556,-0.152811367961587));
#127144=CARTESIAN_POINT('Ctrl Pts',(3.23664946349505,3.78467661316556,6.48741861484588));
#127145=CARTESIAN_POINT('Ctrl Pts',(3.25541488977027,3.79148857336469,6.52455382809183));
#127146=CARTESIAN_POINT('Ctrl Pts',(3.2741497958025,3.79813536728641,6.56176431297438));
#127147=CARTESIAN_POINT('Ctrl Pts',(3.31151964099757,3.81110763603767,6.63623281746942));
#127148=CARTESIAN_POINT('Ctrl Pts',(3.33017674893767,3.81744080660581,6.67353502924518));
#127149=CARTESIAN_POINT('Ctrl Pts',(3.34878807103834,3.82362522063603,6.71085825013198));
#127150=CARTESIAN_POINT('Ctrl Pts',(2.829645774,3.913265985,6.945725649));
#127151=CARTESIAN_POINT('Ctrl Pts',(2.889925936,3.903042157,6.92116788300001));
#127152=CARTESIAN_POINT('Ctrl Pts',(2.94977079,3.892857143,6.895567583));
#127153=CARTESIAN_POINT('Ctrl Pts',(3.267232039,3.838828313,6.759764705));
#127154=CARTESIAN_POINT('Ctrl Pts',(3.57087253,3.783894965,6.59536726600001));
#127155=CARTESIAN_POINT('Ctrl Pts',(2.513657828,3.913265985,6.80029590000001));
#127156=CARTESIAN_POINT('Ctrl Pts',(2.572675843,3.903042157,6.77848051100001));
#127157=CARTESIAN_POINT('Ctrl Pts',(2.631306337,3.892857143,6.755644082));
#127158=CARTESIAN_POINT('Ctrl Pts',(2.942325725,3.838828313,6.634502815));
#127159=CARTESIAN_POINT('Ctrl Pts',(3.240898745,3.783894965,6.48529685700001));
#127160=CARTESIAN_POINT('',(2.82964577863558,3.91326598587967,6.9457256464307));
#127161=CARTESIAN_POINT('Ctrl Pts',(3.34878807403057,3.82362522012801,6.71085824878091));
#127162=CARTESIAN_POINT('Ctrl Pts',(3.21726748079077,3.84689293573226,6.77648839291499));
#127163=CARTESIAN_POINT('Ctrl Pts',(3.08413814752668,3.8699891200746,6.83808820886709));
#127164=CARTESIAN_POINT('Ctrl Pts',(2.94977078968296,3.89285714276324,6.89556758275439));
#127165=CARTESIAN_POINT('Ctrl Pts',(2.90991319577925,3.89964051914521,6.91261777693104));
#127166=CARTESIAN_POINT('Ctrl Pts',(2.86986881736904,3.90644394874724,6.92933902946402));
#127167=CARTESIAN_POINT('Ctrl Pts',(2.82964577787071,3.91326598565656,6.9457256476036));
#127168=CARTESIAN_POINT('',(2.67165180852597,3.91326598631311,6.87301077157454));
#127169=CARTESIAN_POINT('Origin',(7.4723213727701E-13,4.00453391999956,
1.41163122857613E-12));
#127170=CARTESIAN_POINT('',(3.34235673590872,4.00345494162035,6.71406370599629));
#127171=CARTESIAN_POINT('Origin',(-0.0592595316714378,4.16057203004573,
-0.175238072865184));
#127172=CARTESIAN_POINT('Origin',(-0.0878244445791232,4.01785425743471,
-0.171210135190435));
#127173=CARTESIAN_POINT('Ctrl Pts',(1.583020583,3.783915088,7.331033067));
#127174=CARTESIAN_POINT('Ctrl Pts',(1.98146011,3.848090541,7.244996356));
#127175=CARTESIAN_POINT('Ctrl Pts',(2.368228079,3.913265985,7.11628384500001));
#127176=CARTESIAN_POINT('Ctrl Pts',(2.37210492999178,3.91391928492389,7.11499366777252));
#127177=CARTESIAN_POINT('Ctrl Pts',(2.37598178098357,3.91457258484778,7.11370349054503));
#127178=CARTESIAN_POINT('Ctrl Pts',(1.761840242,3.783915088,7.032667983));
#127179=CARTESIAN_POINT('Ctrl Pts',(2.144063713,3.848090541,6.936912476));
#127180=CARTESIAN_POINT('Ctrl Pts',(2.513657828,3.913265985,6.8002959));
#127181=CARTESIAN_POINT('Ctrl Pts',(2.51736253321383,3.91391928492389,6.79892649469601));
#127182=CARTESIAN_POINT('Ctrl Pts',(2.52106723842766,3.91457258484778,6.79755708939203));
#127183=CARTESIAN_POINT('',(2.36822808400883,3.9132659845887,7.11628384347087));
#127184=CARTESIAN_POINT('',(2.44094296070756,3.91326598377977,6.95828986997161));
#127185=CARTESIAN_POINT('',(1.82785911574402,3.82362522063531,7.27385255908872));
#127186=CARTESIAN_POINT('Origin',(-0.0752306557181101,4.01780064760607,
-0.173029325392347));
#127187=CARTESIAN_POINT('Ctrl Pts',(1.76637516223459,3.78467661302819,7.03153033179064));
#127188=CARTESIAN_POINT('Ctrl Pts',(1.77671889009897,3.79148857321477,7.07183135625115));
#127189=CARTESIAN_POINT('Ctrl Pts',(1.78701663017569,3.79813536722453,7.1121993322267));
#127190=CARTESIAN_POINT('Ctrl Pts',(1.80750430603842,3.81110766402319,7.19296039122642));
#127191=CARTESIAN_POINT('Ctrl Pts',(1.81770639741428,3.8174408635424,7.23340142297894));
#127192=CARTESIAN_POINT('Ctrl Pts',(1.82785911431772,3.82362522063523,7.27385255944672));
#127193=CARTESIAN_POINT('Ctrl Pts',(1.270364528,3.913265985,7.391628641));
#127194=CARTESIAN_POINT('Ctrl Pts',(1.334514567,3.903042157,7.380603475));
#127195=CARTESIAN_POINT('Ctrl Pts',(1.398463589,3.892857143,7.36846657));
#127196=CARTESIAN_POINT('Ctrl Pts',(1.737696375,3.838828313,7.304083473));
#127197=CARTESIAN_POINT('Ctrl Pts',(2.06957851,3.783894965,7.208803284));
#127198=CARTESIAN_POINT('Ctrl Pts',(0.993027301999999,3.913265985,7.18167089));
#127199=CARTESIAN_POINT('Ctrl Pts',(1.055355172,3.903042157,7.173052662));
#127200=CARTESIAN_POINT('Ctrl Pts',(1.117524075,3.892857143,7.163353959));
#127201=CARTESIAN_POINT('Ctrl Pts',(1.447313794,3.838828313,7.111904882));
#127202=CARTESIAN_POINT('Ctrl Pts',(1.770981213,3.783894965,7.03037165));
#127203=CARTESIAN_POINT('',(1.27036453248304,3.9132659854451,7.39162863951458));
#127204=CARTESIAN_POINT('Ctrl Pts',(1.8278591176894,3.82362522012808,7.27385255883624));
#127205=CARTESIAN_POINT('Ctrl Pts',(1.6853048618196,3.84689293573234,7.30967526699593));
#127206=CARTESIAN_POINT('Ctrl Pts',(1.54204587881209,3.86998912007467,7.34121604212135));
#127207=CARTESIAN_POINT('Ctrl Pts',(1.3984635889666,3.89285714300268,7.36846656999108));
#127208=CARTESIAN_POINT('Ctrl Pts',(1.35587255566562,3.89964051914869,7.37654993559321));
#127209=CARTESIAN_POINT('Ctrl Pts',(1.31316981756267,3.90644394833732,7.38427189684407));
#127210=CARTESIAN_POINT('Ctrl Pts',(1.27036453168524,3.91326598441267,7.39162864036663));
#127211=CARTESIAN_POINT('',(1.13169592297835,3.91326598631302,7.28664976426088));
#127212=CARTESIAN_POINT('Origin',(-2.03938428644523E-13,4.00453392000067,
-6.67868538251071E-13));
#127213=CARTESIAN_POINT('',(1.82088906321882,4.00345494158282,7.27560052616864));
#127214=CARTESIAN_POINT('Origin',(-0.0202030731523872,4.16057201776935,
-0.18388014126873));
#127215=CARTESIAN_POINT('Origin',(-0.0489661124333862,4.01785421495085,
-0.186087345027113));
#127216=CARTESIAN_POINT('Ctrl Pts',(-0.029944964,3.783915088,7.49994022));
#127217=CARTESIAN_POINT('Ctrl Pts',(0.377674617,3.848090541,7.50156772));
#127218=CARTESIAN_POINT('Ctrl Pts',(0.783069551000001,3.913265985,7.459008116));
#127219=CARTESIAN_POINT('Ctrl Pts',(0.787133113336888,3.91391928492389,
7.45858151075809));
#127220=CARTESIAN_POINT('Ctrl Pts',(0.791196675673776,3.91457258484778,
7.45815490551618));
#127221=CARTESIAN_POINT('Ctrl Pts',(0.208833664,3.783915088,7.246991686));
#127222=CARTESIAN_POINT('Ctrl Pts',(0.602705566,3.848090541,7.235641637));
#127223=CARTESIAN_POINT('Ctrl Pts',(0.993027302,3.913265985,7.18167089));
#127224=CARTESIAN_POINT('Ctrl Pts',(0.996939774931096,3.91391928492389,
7.18112990273941));
#127225=CARTESIAN_POINT('Ctrl Pts',(1.00085224786219,3.91457258484778,7.18058891547881));
#127226=CARTESIAN_POINT('',(0.783069554340072,3.91326598458875,7.45900811632261));
#127227=CARTESIAN_POINT('',(0.888048434082487,3.91326598377978,7.32033950208015));
#127228=CARTESIAN_POINT('',(0.22146149895969,3.82362522067689,7.49672960729196));
#127229=CARTESIAN_POINT('Origin',(-0.0362756098282808,4.01780061753748,
-0.185156279461053));
#127230=CARTESIAN_POINT('Ctrl Pts',(0.213507121533661,3.78467661307173,
7.2468555066897));
#127231=CARTESIAN_POINT('Ctrl Pts',(0.214945489938668,3.79148857326155,
7.28843791132082));
#127232=CARTESIAN_POINT('Ctrl Pts',(0.216324553099686,3.79813536727868,
7.33007581620001));
#127233=CARTESIAN_POINT('Ctrl Pts',(0.218971991994922,3.811107633564,7.41335277529608));
#127234=CARTESIAN_POINT('Ctrl Pts',(0.220241931798139,3.8174408015945,7.45504124418656));
#127235=CARTESIAN_POINT('Ctrl Pts',(0.22146149747299,3.82362522066709,7.49672960733691));
#127236=CARTESIAN_POINT('Ctrl Pts',(-0.348317552,3.913265985,7.491907293));
#127237=CARTESIAN_POINT('Ctrl Pts',(-0.28329722,3.903042157,7.49493025100001));
#127238=CARTESIAN_POINT('Ctrl Pts',(-0.218234215,3.892857143,7.496824249));
#127239=CARTESIAN_POINT('Ctrl Pts',(0.12690796,3.838828313,7.506871415));
#127240=CARTESIAN_POINT('Ctrl Pts',(0.4715133,3.783894965,7.485163673));
#127241=CARTESIAN_POINT('Ctrl Pts',(-0.574036077000001,3.913265985,7.227238932));
#127242=CARTESIAN_POINT('Ctrl Pts',(-0.511312734,3.903042157,7.232220843));
#127243=CARTESIAN_POINT('Ctrl Pts',(-0.448512371,3.892857143,7.236113367));
#127244=CARTESIAN_POINT('Ctrl Pts',(-0.115372922,3.838828313,7.256762181));
#127245=CARTESIAN_POINT('Ctrl Pts',(0.218254568,3.783894965,7.246714079));
#127246=CARTESIAN_POINT('',(-0.348317546752673,3.91326598587967,7.49190729243567));
#127247=CARTESIAN_POINT('Ctrl Pts',(0.221461498925141,3.82362522046317,
7.49672960726836));
#127248=CARTESIAN_POINT('Ctrl Pts',(0.0745392594698745,3.8468929359541,
7.50106984909109));
#127249=CARTESIAN_POINT('Ctrl Pts',(-0.0721507419137992,3.86998912018444,
7.50107677173588));
#127250=CARTESIAN_POINT('Ctrl Pts',(-0.218234214930474,3.89285714276327,
7.49682424946948));
#127251=CARTESIAN_POINT('Ctrl Pts',(-0.261567177774771,3.89964051909098,
7.49556281732005));
#127252=CARTESIAN_POINT('Ctrl Pts',(-0.304931542627311,3.90644394863843,
7.49392441705024));
#127253=CARTESIAN_POINT('Ctrl Pts',(-0.348317546838671,3.91326598549287,
7.49190729297715));
#127254=CARTESIAN_POINT('',(-0.461176806441806,3.91326598631302,7.35957311300495));
#127255=CARTESIAN_POINT('Origin',(1.13136496698862E-13,4.00453391999956,
7.10369263412503E-13));
#127256=CARTESIAN_POINT('',(0.214278640529085,4.00345494161128,7.49693835249986));
#127257=CARTESIAN_POINT('Origin',(0.0197980510491458,4.16057202135974,-0.183924310788655));
#127258=CARTESIAN_POINT('Origin',(-0.0078180414431836,4.01785424473155,
-0.192262944664429));
#127259=CARTESIAN_POINT('Ctrl Pts',(0.431320676484365,1.97885290483257,
7.48816481493075));
#127260=CARTESIAN_POINT('Ctrl Pts',(0.44542542366215,1.97658649491626,7.48729904127472));
#127261=CARTESIAN_POINT('Ctrl Pts',(0.459530170839939,1.974320085,7.4864332676187));
#127262=CARTESIAN_POINT('Ctrl Pts',(0.868621014284314,1.908585653,7.46132256760333));
#127263=CARTESIAN_POINT('Ctrl Pts',(1.27253989903237,1.843501847,7.39178552536167));
#127264=CARTESIAN_POINT('Ctrl Pts',(0.17884133945574,1.97885290483257,7.24784534091357));
#127265=CARTESIAN_POINT('Ctrl Pts',(0.192495113727867,1.97658649491626,
7.24745694795684));
#127266=CARTESIAN_POINT('Ctrl Pts',(0.206148888,1.974320085,7.247068555));
#127267=CARTESIAN_POINT('Ctrl Pts',(0.602159817,1.908585653,7.23580369500001));
#127268=CARTESIAN_POINT('Ctrl Pts',(0.994585354,1.843501847,7.181455282));
#127269=CARTESIAN_POINT('',(0.989922562761728,1.84427517322922,7.1820995058139));
#127270=CARTESIAN_POINT('Origin',(0.00165684739715746,2.01783539001702,
-0.19726511916484));
#127271=CARTESIAN_POINT('Ctrl Pts',(1.02305817352955,1.88359401258998,7.42989582473918));
#127272=CARTESIAN_POINT('Ctrl Pts',(1.01748970331488,1.8773452349313,7.38856271124362));
#127273=CARTESIAN_POINT('Ctrl Pts',(1.01194012110602,1.87094900374799,7.34722645205979));
#127274=CARTESIAN_POINT('Ctrl Pts',(1.00089520291886,1.85785292454026,7.26464059629853));
#127275=CARTESIAN_POINT('Ctrl Pts',(0.995393852709155,1.8511459533259,7.22334605434188));
#127276=CARTESIAN_POINT('Ctrl Pts',(0.989922562684033,1.84427517325669,
7.18209950581963));
#127277=CARTESIAN_POINT('Ctrl Pts',(0.775003908,1.843494248,7.459850464));
#127278=CARTESIAN_POINT('Ctrl Pts',(1.181144933,1.909007671,7.41765647000001));
#127279=CARTESIAN_POINT('Ctrl Pts',(1.580304579,1.974320085,7.331619019));
#127280=CARTESIAN_POINT('Ctrl Pts',(0.985261412,1.843494248,7.182740421));
#127281=CARTESIAN_POINT('Ctrl Pts',(1.376315572,1.909007671,7.129099254));
#127282=CARTESIAN_POINT('Ctrl Pts',(1.759234759,1.974320085,7.033320202));
#127283=CARTESIAN_POINT('Origin',(-0.0322702647863354,1.87500004439775,
-0.196842784057325));
#127284=CARTESIAN_POINT('Ctrl Pts',(2.0309707252744,1.97885290481358,7.22037448773906));
#127285=CARTESIAN_POINT('Ctrl Pts',(2.04455959549943,1.97658649490676,7.21649685167196));
#127286=CARTESIAN_POINT('Ctrl Pts',(2.05814846572453,1.974320085,7.21261921560488));
#127287=CARTESIAN_POINT('Ctrl Pts',(2.45227693432097,1.908585653,7.10015315039258));
#127288=CARTESIAN_POINT('Ctrl Pts',(2.83180401172431,1.843501847,6.94541122513066));
#127289=CARTESIAN_POINT('Ctrl Pts',(1.73273263193011,1.97885290481358,7.03994914282426));
#127290=CARTESIAN_POINT('Ctrl Pts',(1.74598369546509,1.97658649490676,7.03663467241213));
#127291=CARTESIAN_POINT('Ctrl Pts',(1.759234759,1.974320085,7.033320202));
#127292=CARTESIAN_POINT('Ctrl Pts',(2.14356556,1.908585653,6.937188064));
#127293=CARTESIAN_POINT('Ctrl Pts',(2.515133105,1.843501847,6.79975039700001));
#127294=CARTESIAN_POINT('',(2.51071781581557,1.84427517322324,6.80138192165602));
#127295=CARTESIAN_POINT('Origin',(-0.0407880620217305,2.01783544827035,
-0.193009651875682));
#127296=CARTESIAN_POINT('Ctrl Pts',(2.59634761838852,1.88359401254937,7.03626172327405));
#127297=CARTESIAN_POINT('Ctrl Pts',(2.58202393835256,1.8773452349134,6.997092011555));
#127298=CARTESIAN_POINT('Ctrl Pts',(2.56771802844592,1.87094900373487,6.95791516722647));
#127299=CARTESIAN_POINT('Ctrl Pts',(2.53917783475688,1.85785293292152,6.87963450385735));
#127300=CARTESIAN_POINT('Ctrl Pts',(2.52492798746053,1.85114595747494,6.84048800649519));
#127301=CARTESIAN_POINT('Ctrl Pts',(2.51071781591354,1.84427517330664,6.80138192161454));
#127302=CARTESIAN_POINT('Ctrl Pts',(2.360532086,1.843494248,7.118840374));
#127303=CARTESIAN_POINT('Ctrl Pts',(2.748107298,1.909007671,6.99032453800001));
#127304=CARTESIAN_POINT('Ctrl Pts',(3.119439304,1.974320085,6.82049107000001));
#127305=CARTESIAN_POINT('Ctrl Pts',(2.506303418,1.843494248,6.803009862));
#127306=CARTESIAN_POINT('Ctrl Pts',(2.876683684,1.909007671,6.666557711));
#127307=CARTESIAN_POINT('Ctrl Pts',(3.230060768,1.974320085,6.490701613));
#127308=CARTESIAN_POINT('Origin',(-0.0738311105701356,1.87500004546059,
-0.185303373844017));
#127309=CARTESIAN_POINT('Ctrl Pts',(3.53565484055987,1.9788529047602,6.61496747322476));
#127310=CARTESIAN_POINT('Ctrl Pts',(3.54809243330167,1.97658649488008,6.60825928880557));
#127311=CARTESIAN_POINT('Ctrl Pts',(3.56053002604348,1.974320085,6.60155110438651));
#127312=CARTESIAN_POINT('Ctrl Pts',(3.92126711138468,1.908585653,6.40698846308583));
#127313=CARTESIAN_POINT('Ctrl Pts',(4.25865611684382,1.843501847,6.17427721524676));
#127314=CARTESIAN_POINT('Ctrl Pts',(3.20560327250901,1.97885290476021,6.50287274661561));
#127315=CARTESIAN_POINT('Ctrl Pts',(3.21783202025451,1.97658649488008,6.4967871798078));
#127316=CARTESIAN_POINT('Ctrl Pts',(3.230060768,1.974320085,6.490701613));
#127317=CARTESIAN_POINT('Ctrl Pts',(3.584740561,1.908585653,6.31419723));
#127318=CARTESIAN_POINT('Ctrl Pts',(3.918076027,1.843501847,6.100096741));
#127319=CARTESIAN_POINT('',(3.91411469490178,1.84427517306064,6.10263927730789));
#127320=CARTESIAN_POINT('Origin',(-0.0813257725786604,2.01783541886837,
-0.179728872211489));
#127321=CARTESIAN_POINT('Ctrl Pts',(4.04823473411854,1.88359401261533,6.3136198438659));
#127322=CARTESIAN_POINT('Ctrl Pts',(4.02582560354359,1.87734523497682,6.27844506607643));
#127323=CARTESIAN_POINT('Ctrl Pts',(4.00343229437791,1.87094900381564,6.24325950250469));
#127324=CARTESIAN_POINT('Ctrl Pts',(3.95873129615144,1.85785292434757,6.17294424923507));
#127325=CARTESIAN_POINT('Ctrl Pts',(3.93639927824253,1.85114595331107,6.13777629603404));
#127326=CARTESIAN_POINT('Ctrl Pts',(3.91411469398354,1.84427517339915,6.10263927840607));
#127327=CARTESIAN_POINT('Ctrl Pts',(3.835684406,1.843494248,6.44496122100001));
#127328=CARTESIAN_POINT('Ctrl Pts',(4.18657122,1.909007671,6.236132799));
#127329=CARTESIAN_POINT('Ctrl Pts',(4.512712514,1.974320085,5.990444538));
#127330=CARTESIAN_POINT('Ctrl Pts',(3.910153461,1.843494248,6.105178123));
#127331=CARTESIAN_POINT('Ctrl Pts',(4.242541264,1.909007671,5.89229533900001));
#127332=CARTESIAN_POINT('Ctrl Pts',(4.549852726,1.974320085,5.644585031));
#127333=CARTESIAN_POINT('Origin',(-0.111939653748659,1.87500003546859,-0.16509948825185));
#127334=CARTESIAN_POINT('Ctrl Pts',(4.87501566615518,1.9788529047133,5.70025193191983));
#127335=CARTESIAN_POINT('Ctrl Pts',(4.88572041336524,1.97658649485662,5.69102686641532));
#127336=CARTESIAN_POINT('Ctrl Pts',(4.89642516057517,1.974320085,5.68180180091079));
#127337=CARTESIAN_POINT('Ctrl Pts',(5.20690319502679,1.908585653,5.41424011548591));
#127338=CARTESIAN_POINT('Ctrl Pts',(5.48637819364505,1.843501847,5.11444086518299));
#127339=CARTESIAN_POINT('Ctrl Pts',(4.52858346737681,1.9788529047133,5.66172924861175));
#127340=CARTESIAN_POINT('Ctrl Pts',(4.5392180966884,1.97658649485662,5.65315713980588));
#127341=CARTESIAN_POINT('Ctrl Pts',(4.549852726,1.974320085,5.644585031));
#127342=CARTESIAN_POINT('Ctrl Pts',(4.858297077,1.908585653,5.395961552));
#127343=CARTESIAN_POINT('Ctrl Pts',(5.137814068,1.843501847,5.115209341));
#127344=CARTESIAN_POINT('',(5.13449191936986,1.84427517322394,5.11854400394933));
#127345=CARTESIAN_POINT('Origin',(-0.118060676876202,2.01783543967816,-0.158044115063364));
#127346=CARTESIAN_POINT('Ctrl Pts',(5.31083089269158,1.88359401260886,5.29576011741492));
#127347=CARTESIAN_POINT('Ctrl Pts',(5.28138452430791,1.87734531701701,5.26622539498652));
#127348=CARTESIAN_POINT('Ctrl Pts',(5.25195069654588,1.87094904413585,5.23667614406208));
#127349=CARTESIAN_POINT('Ctrl Pts',(5.19317884859687,1.85785291265372,5.17761398118619));
#127350=CARTESIAN_POINT('Ctrl Pts',(5.16380889825467,1.85114594749935,5.14806898668561));
#127351=CARTESIAN_POINT('Ctrl Pts',(5.13449191955354,1.84427517329317,5.11854400434702));
#127352=CARTESIAN_POINT('Ctrl Pts',(5.131484387,1.843494248,5.469722844));
#127353=CARTESIAN_POINT('Ctrl Pts',(5.429275724,1.909007671,5.19034642200001));
#127354=CARTESIAN_POINT('Ctrl Pts',(5.694976303,1.974320085,4.880291478));
#127355=CARTESIAN_POINT('Ctrl Pts',(5.131169075,1.843494248,5.12187504));
#127356=CARTESIAN_POINT('Ctrl Pts',(5.410022329,1.909007671,4.842515785));
#127357=CARTESIAN_POINT('Ctrl Pts',(5.656898626,1.974320085,4.534533927));
#127358=CARTESIAN_POINT('Origin',(-0.144814243662199,1.87500002627446,-0.137175988992163));
#127359=CARTESIAN_POINT('Ctrl Pts',(5.98642617657734,1.97885290449943,4.51899894419897));
#127360=CARTESIAN_POINT('Ctrl Pts',(5.99489753597836,1.97658649474969,4.50768835193765));
#127361=CARTESIAN_POINT('Ctrl Pts',(6.00336889537952,1.974320085,4.49637775967633));
#127362=CARTESIAN_POINT('Ctrl Pts',(6.24907027333074,1.908585653,4.16832791874103));
#127363=CARTESIAN_POINT('Ctrl Pts',(6.45756332514675,1.843501847,3.81545894504712));
#127364=CARTESIAN_POINT('Ctrl Pts',(5.63981213161998,1.97885290449943,4.55584958327403));
#127365=CARTESIAN_POINT('Ctrl Pts',(5.64835537881002,1.97658649474969,4.54519175513701));
#127366=CARTESIAN_POINT('Ctrl Pts',(5.656898626,1.974320085,4.534533927));
#127367=CARTESIAN_POINT('Ctrl Pts',(5.904685021,1.908585653,4.225416708));
#127368=CARTESIAN_POINT('Ctrl Pts',(6.117313634,1.843501847,3.891140437));
#127369=CARTESIAN_POINT('',(6.11478600923873,1.84427517321823,3.89511130174437));
#127370=CARTESIAN_POINT('Origin',(-0.149275386552622,2.01783542593181,-0.128969635675294));
#127371=CARTESIAN_POINT('Ctrl Pts',(6.32509850137208,1.88359401257019,4.03027653421333));
#127372=CARTESIAN_POINT('Ctrl Pts',(6.28999101930453,1.87734523490686,4.00776212019143));
#127373=CARTESIAN_POINT('Ctrl Pts',(6.25489336773249,1.87094900375861,3.98523127410483));
#127374=CARTESIAN_POINT('Ctrl Pts',(6.18479924655972,1.85785292702313,3.94018434990008));
#127375=CARTESIAN_POINT('Ctrl Pts',(6.14976460795124,1.85114595460251,3.9176437458544));
#127376=CARTESIAN_POINT('Ctrl Pts',(6.11478600941527,1.8442751733602,3.89511130181847));
#127377=CARTESIAN_POINT('Ctrl Pts',(6.187341861,1.843494248,4.238726305));
#127378=CARTESIAN_POINT('Ctrl Pts',(6.41811333,1.909007671,3.901865214));
#127379=CARTESIAN_POINT('Ctrl Pts',(6.610949329,1.974320085,3.541941413));
#127380=CARTESIAN_POINT('Ctrl Pts',(6.112256925,1.843494248,3.899078773));
#127381=CARTESIAN_POINT('Ctrl Pts',(6.324536764,1.909007671,3.566305575));
#127382=CARTESIAN_POINT('Ctrl Pts',(6.49943423400001,1.974320085,3.212453056));
#127383=CARTESIAN_POINT('Origin',(-0.170917169116834,1.87500007773979,-0.102838001282375));
#127384=CARTESIAN_POINT('Ctrl Pts',(6.81791805171561,1.97885290458604,3.12644259057752));
#127385=CARTESIAN_POINT('Ctrl Pts',(6.8237599125367,1.976586494793,3.11357534157059));
#127386=CARTESIAN_POINT('Ctrl Pts',(6.82960177335764,1.974320085,3.10070809256374));
#127387=CARTESIAN_POINT('Ctrl Pts',(6.99903777035848,1.908585653,2.72750934118146));
#127388=CARTESIAN_POINT('Ctrl Pts',(7.12679997215744,1.843501847,2.33807040446541));
#127389=CARTESIAN_POINT('Ctrl Pts',(6.48732944815439,1.97885290458604,3.23694345578894));
#127390=CARTESIAN_POINT('Ctrl Pts',(6.49338184107711,1.976586494793,3.2246982558945));
#127391=CARTESIAN_POINT('Ctrl Pts',(6.499434234,1.974320085,3.212453056));
#127392=CARTESIAN_POINT('Ctrl Pts',(6.674976456,1.908585653,2.857296075));
#127393=CARTESIAN_POINT('Ctrl Pts',(6.810774414,1.843501847,2.485126131));
#127394=CARTESIAN_POINT('',(6.80915950174646,1.84427517325685,2.48954752345402));
#127395=CARTESIAN_POINT('Origin',(-0.173510263844014,2.01783543082771,-0.0938646918006689));
#127396=CARTESIAN_POINT('Ctrl Pts',(7.04361153430039,1.88359401255035,2.57634169922522));
#127397=CARTESIAN_POINT('Ctrl Pts',(7.00448491229141,1.87734523491764,2.5619007306039));
#127398=CARTESIAN_POINT('Ctrl Pts',(6.96536435829275,1.87094900376008,2.54744160075242));
#127399=CARTESIAN_POINT('Ctrl Pts',(6.88722512871215,1.85785290811974,2.51851597096455));
#127400=CARTESIAN_POINT('Ctrl Pts',(6.84816407707341,1.85114594533474,2.50403378766267));
#127401=CARTESIAN_POINT('Ctrl Pts',(6.80915950224257,1.84427517341445,2.48954752411438));
#127402=CARTESIAN_POINT('Ctrl Pts',(6.953886107,1.843494248,2.809531636));
#127403=CARTESIAN_POINT('Ctrl Pts',(7.10684709,1.909007671,2.430937126));
#127404=CARTESIAN_POINT('Ctrl Pts',(7.217801712,1.974320085,2.037974103));
#127405=CARTESIAN_POINT('Ctrl Pts',(6.807542435,1.843494248,2.493965916));
#127406=CARTESIAN_POINT('Ctrl Pts',(6.943322888,1.909007671,2.12333888));
#127407=CARTESIAN_POINT('Ctrl Pts',(7.038063521,1.974320085,1.74016145));
#127408=CARTESIAN_POINT('Origin',(-0.189028489599921,1.87500006543182,-0.0636916109352054));
#127409=CARTESIAN_POINT('Ctrl Pts',(7.33061165607248,1.97885290465309,1.58769725582771));
#127410=CARTESIAN_POINT('Ctrl Pts',(7.33355085931847,1.97658649482652,1.57387500833381));
#127411=CARTESIAN_POINT('Ctrl Pts',(7.33649006256462,1.974320085,1.56005276083997));
#127412=CARTESIAN_POINT('Ctrl Pts',(7.42173804095537,1.908585653,1.15915545738787));
#127413=CARTESIAN_POINT('Ctrl Pts',(7.4627953726707,1.843501847,0.751356289701777));
#127414=CARTESIAN_POINT('Ctrl Pts',(7.03150645023676,1.97885290465309,1.76668144932446));
#127415=CARTESIAN_POINT('Ctrl Pts',(7.03478498561844,1.97658649482652,1.75342144966226));
#127416=CARTESIAN_POINT('Ctrl Pts',(7.038063521,1.974320085,1.74016145));
#127417=CARTESIAN_POINT('Ctrl Pts',(7.133153411,1.908585653,1.355571454));
#127418=CARTESIAN_POINT('Ctrl Pts',(7.185770951,1.843501847,0.962910089));
#127419=CARTESIAN_POINT('',(7.18514426358531,1.84427517325349,0.967575271040671));
#127420=CARTESIAN_POINT('Origin',(-0.18963165884277,2.0178354651733,-0.0543705811767188));
#127421=CARTESIAN_POINT('Ctrl Pts',(7.43277311966718,1.88359401261756,1.00193998978874));
#127422=CARTESIAN_POINT('Ctrl Pts',(7.39145687490835,1.87734523496621,0.996247710126135));
#127423=CARTESIAN_POINT('Ctrl Pts',(7.35014265232055,1.87094900381072,0.990536389400879));
#127424=CARTESIAN_POINT('Ctrl Pts',(7.26761217221817,1.8578529165569,0.979084656609812));
#127425=CARTESIAN_POINT('Ctrl Pts',(7.2263510766818,1.85114594946581,0.973338026201722));
#127426=CARTESIAN_POINT('Ctrl Pts',(7.18514426386498,1.84427517338048,0.967575270475462));
#127427=CARTESIAN_POINT('Ctrl Pts',(7.395274366,1.843494248,1.24896639));
#127428=CARTESIAN_POINT('Ctrl Pts',(7.463272578,1.909007671,0.84634112));
#127429=CARTESIAN_POINT('Ctrl Pts',(7.487157709,1.974320085,0.43871339));
#127430=CARTESIAN_POINT('Ctrl Pts',(7.184514827,1.843494248,0.972237985));
#127431=CARTESIAN_POINT('Ctrl Pts',(7.23744695100001,1.909007671,0.58108722));
#127432=CARTESIAN_POINT('Ctrl Pts',(7.24760078,1.974320085,0.186501829));
#127433=CARTESIAN_POINT('Origin',(-0.198300997752738,1.8750000238648,-0.0215670094842346));
#127434=CARTESIAN_POINT('Ctrl Pts',(7.50053400668084,1.97885290461155,-0.025287038347163));
#127435=CARTESIAN_POINT('Ctrl Pts',(7.50043311836844,1.97658649480575,-0.0394179710704729));
#127436=CARTESIAN_POINT('Ctrl Pts',(7.50033223005592,1.974320085,-0.0535489037937829));
#127437=CARTESIAN_POINT('Ctrl Pts',(7.49740608849883,1.908585653,-0.463399246762781));
#127438=CARTESIAN_POINT('Ctrl Pts',(7.44983875707374,1.843501847,-0.870490409364686));
#127439=CARTESIAN_POINT('Ctrl Pts',(7.24689802587571,1.97885290461155,0.213811381676077));
#127440=CARTESIAN_POINT('Ctrl Pts',(7.24724940293787,1.97658649480575,0.200156605338041));
#127441=CARTESIAN_POINT('Ctrl Pts',(7.24760078,1.974320085,0.186501829));
#127442=CARTESIAN_POINT('Ctrl Pts',(7.25779204,1.908585653,-0.209538183));
#127443=CARTESIAN_POINT('Ctrl Pts',(7.224768825,1.843501847,-0.604330558));
#127444=CARTESIAN_POINT('',(7.22515966553458,1.84427517322513,-0.59963972759421));
#127445=CARTESIAN_POINT('Origin',(-0.196886367451559,2.01783541028853,-0.0123342117785667));
#127446=CARTESIAN_POINT('Ctrl Pts',(7.4743864954929,1.88359401260467,-0.61931132006069));
#127447=CARTESIAN_POINT('Ctrl Pts',(7.43281252968542,1.87734523494865,-0.615988746101347));
#127448=CARTESIAN_POINT('Ctrl Pts',(7.39123644540397,1.87094900377294,-0.61268520272327));
#127449=CARTESIAN_POINT('Ctrl Pts',(7.30817373059725,1.85785292164987,-0.606127589323485));
#127450=CARTESIAN_POINT('Ctrl Pts',(7.26664192341387,1.85114595192226,-0.60286994943654));
#127451=CARTESIAN_POINT('Ctrl Pts',(7.22515966555154,1.84427517329407,-0.599639727229753));
#127452=CARTESIAN_POINT('Ctrl Pts',(7.490867816,1.843494248,-0.369999136));
#127453=CARTESIAN_POINT('Ctrl Pts',(7.470723736,1.909007671,-0.777828857000001));
#127454=CARTESIAN_POINT('Ctrl Pts',(7.406422533,1.974320085,-1.181061074));
#127455=CARTESIAN_POINT('Ctrl Pts',(7.225547291,1.843494248,-0.594950714));
#127456=CARTESIAN_POINT('Ctrl Pts',(7.193156039,1.909007671,-0.988335434000001));
#127457=CARTESIAN_POINT('Ctrl Pts',(7.118248282,1.974320085,-1.375878411));
#127458=CARTESIAN_POINT('Origin',(-0.198301150915829,1.87500003685011,0.0215660772445789));
#127459=CARTESIAN_POINT('Ctrl Pts',(7.31973972432723,1.9788529048441,-1.63708893764741));
#127460=CARTESIAN_POINT('Ctrl Pts',(7.31660346173343,1.97658649492202,-1.65086780969589));
#127461=CARTESIAN_POINT('Ctrl Pts',(7.3134671991396,1.974320085,-1.66464668174432));
#127462=CARTESIAN_POINT('Ctrl Pts',(7.22250376035314,1.908585653,-2.06428591686262));
#127463=CARTESIAN_POINT('Ctrl Pts',(7.08853595973428,1.843501847,-2.45163394439753));
#127464=CARTESIAN_POINT('Ctrl Pts',(7.12343270472288,1.9788529048441,-1.34905626783604));
#127465=CARTESIAN_POINT('Ctrl Pts',(7.12084049336147,1.97658649492202,-1.36246733941802));
#127466=CARTESIAN_POINT('Ctrl Pts',(7.118248282,1.974320085,-1.375878411));
#127467=CARTESIAN_POINT('Ctrl Pts',(7.04306438000001,1.908585653,-1.764850046));
#127468=CARTESIAN_POINT('Ctrl Pts',(6.925944539,1.843501847,-2.14331338));
#127469=CARTESIAN_POINT('',(6.92733463110791,1.84427517321638,-2.138816237699));
#127470=CARTESIAN_POINT('Origin',(-0.194934900054559,2.01783545594361,0.0302789327713401));
#127471=CARTESIAN_POINT('Ctrl Pts',(7.16650586548861,1.88359401258645,-2.21160432106037));
#127472=CARTESIAN_POINT('Ctrl Pts',(7.12661813124974,1.87734523495188,-2.19942225327674));
#127473=CARTESIAN_POINT('Ctrl Pts',(7.08672423681744,1.87094900375853,-2.1872583156522));
#127474=CARTESIAN_POINT('Ctrl Pts',(7.00701309419383,1.85785290831506,-2.16299796235914));
#127475=CARTESIAN_POINT('Ctrl Pts',(6.96715261721269,1.85114594538467,-2.15088838650028));
#127476=CARTESIAN_POINT('Ctrl Pts',(6.92733463187897,1.84427517331601,-2.13881623722281));
#127477=CARTESIAN_POINT('Ctrl Pts',(7.236196612,1.843494248,-1.971663914));
#127478=CARTESIAN_POINT('Ctrl Pts',(7.128852155,1.909007671,-2.365628421));
#127479=CARTESIAN_POINT('Ctrl Pts',(6.979371271,1.974320085,-2.745610435));
#127480=CARTESIAN_POINT('Ctrl Pts',(6.928721193,1.843494248,-2.134320179));
#127481=CARTESIAN_POINT('Ctrl Pts',(6.812521145,1.909007671,-2.511544621));
#127482=CARTESIAN_POINT('Ctrl Pts',(6.656054405,1.974320085,-2.873924105));
#127483=CARTESIAN_POINT('Origin',(-0.189028709532146,1.87500002431909,0.0636906784464586));
#127484=CARTESIAN_POINT('Ctrl Pts',(6.79668254745504,1.97885290457719,-3.17234238059632));
#127485=CARTESIAN_POINT('Ctrl Pts',(6.79065755907535,1.97658649478857,-3.18512490576253));
#127486=CARTESIAN_POINT('Ctrl Pts',(6.78463257069555,1.974320085,-3.19790743092867));
#127487=CARTESIAN_POINT('Ctrl Pts',(6.60988518346303,1.908585653,-3.56864887210941));
#127488=CARTESIAN_POINT('Ctrl Pts',(6.39578110021144,1.843501847,-3.91814180098456));
#127489=CARTESIAN_POINT('Ctrl Pts',(6.66688358603411,1.97885290457719,-2.84884354773725));
#127490=CARTESIAN_POINT('Ctrl Pts',(6.6614689955171,1.97658649478857,-2.86138382636864));
#127491=CARTESIAN_POINT('Ctrl Pts',(6.656054405,1.974320085,-2.873924105));
#127492=CARTESIAN_POINT('Ctrl Pts',(6.49901085800001,1.908585653,-3.237639483));
#127493=CARTESIAN_POINT('Ctrl Pts',(6.303270783,1.843501847,-3.582077251));
#127494=CARTESIAN_POINT('',(6.30559512912612,1.8442751732378,-3.57798407743432));
#127495=CARTESIAN_POINT('Origin',(-0.183868084562621,2.01783547332994,0.0714761343217757));
#127496=CARTESIAN_POINT('Ctrl Pts',(6.52352738649043,1.8835940126154,-3.7004851615402));
#127497=CARTESIAN_POINT('Ctrl Pts',(6.48719098969058,1.87734523496561,-3.68001321990517));
#127498=CARTESIAN_POINT('Ctrl Pts',(6.45084467936221,1.87094900377755,-3.65955766037718));
#127499=CARTESIAN_POINT('Ctrl Pts',(6.37821249536725,1.8578529259649,-3.61872901632466));
#127500=CARTESIAN_POINT('Ctrl Pts',(6.34188708286931,1.85114595406991,-3.59833370212756));
#127501=CARTESIAN_POINT('Ctrl Pts',(6.30559512917684,1.84427517334982,-3.57798407768235));
#127502=CARTESIAN_POINT('Ctrl Pts',(6.64316889699999,1.843494248,-3.481135878));
#127503=CARTESIAN_POINT('Ctrl Pts',(6.45364337,1.909007671,-3.842813829));
#127504=CARTESIAN_POINT('Ctrl Pts',(6.225972366,1.974320085,-4.181778103));
#127505=CARTESIAN_POINT('Ctrl Pts',(6.307915794,1.843494248,-3.573891204));
#127506=CARTESIAN_POINT('Ctrl Pts',(6.113340333,1.909007671,-3.917316773));
#127507=CARTESIAN_POINT('Ctrl Pts',(5.882630822,1.974320085,-4.237588302));
#127508=CARTESIAN_POINT('Origin',(-0.170917924837104,1.87500005981962,0.102837358194177));
#127509=CARTESIAN_POINT('Ctrl Pts',(5.95582004877323,1.97885290483854,-4.55926061605723));
#127510=CARTESIAN_POINT('Ctrl Pts',(5.94718805576368,1.97658649491924,-4.57044909915949));
#127511=CARTESIAN_POINT('Ctrl Pts',(5.93855606275414,1.974320085,-4.58163758226185));
#127512=CARTESIAN_POINT('Ctrl Pts',(5.68819572295363,1.908585653,-4.90614577269425));
#127513=CARTESIAN_POINT('Ctrl Pts',(5.40396662443388,1.843501847,-5.20144170167195));
#127514=CARTESIAN_POINT('Ctrl Pts',(5.8985984021513,1.97885290483854,-4.21542206677501));
#127515=CARTESIAN_POINT('Ctrl Pts',(5.89061461207569,1.97658649491924,-4.2265051843875));
#127516=CARTESIAN_POINT('Ctrl Pts',(5.882630822,1.974320085,-4.237588302));
#127517=CARTESIAN_POINT('Ctrl Pts',(5.651070811,1.908585653,-4.559040496));
#127518=CARTESIAN_POINT('Ctrl Pts',(5.385863092,1.843501847,-4.85334717));
#127519=CARTESIAN_POINT('',(5.3890130067386,1.84427517318824,-4.84984935889788));
#127520=CARTESIAN_POINT('Origin',(-0.164204111051632,2.01783546428834,0.10933127938741));
#127521=CARTESIAN_POINT('Ctrl Pts',(5.57551601750762,1.88359401262131,-5.01633542878597));
#127522=CARTESIAN_POINT('Ctrl Pts',(5.54443000772672,1.87734523496005,-4.98853085853225));
#127523=CARTESIAN_POINT('Ctrl Pts',(5.51333079461951,1.87094900377837,-4.96074015636165));
#127524=CARTESIAN_POINT('Ctrl Pts',(5.45117360658552,1.85785291420127,-4.90525224101142));
#127525=CARTESIAN_POINT('Ctrl Pts',(5.42008188133855,1.85114594825435,-4.87752489447751));
#127526=CARTESIAN_POINT('Ctrl Pts',(5.38901300719691,1.84427517327111,-4.84984935883641));
#127527=CARTESIAN_POINT('Ctrl Pts',(5.739513988,1.843494248,-4.82783379800001));
#127528=CARTESIAN_POINT('Ctrl Pts',(5.476669394,1.909007671,-5.14031353300001));
#127529=CARTESIAN_POINT('Ctrl Pts',(5.181453912,1.974320085,-5.422410475));
#127530=CARTESIAN_POINT('Ctrl Pts',(5.392159262,1.843494248,-4.846351049));
#127531=CARTESIAN_POINT('Ctrl Pts',(5.12830652300001,1.909007671,-5.139919546));
#127532=CARTESIAN_POINT('Ctrl Pts',(4.83414196,1.974320085,-5.403107579));
#127533=CARTESIAN_POINT('Origin',(-0.144814768045344,1.87500001817188,0.137175170863457));
#127534=CARTESIAN_POINT('Ctrl Pts',(4.83647002372375,1.97885290468778,-5.73299289464033));
#127535=CARTESIAN_POINT('Ctrl Pts',(4.82563464912652,1.97658649484386,-5.74206417358371));
#127536=CARTESIAN_POINT('Ctrl Pts',(4.81479927452918,1.974320085,-5.75113545252697));
#127537=CARTESIAN_POINT('Ctrl Pts',(4.5005325515057,1.908585653,-6.01423674925969));
#127538=CARTESIAN_POINT('Ctrl Pts',(4.15946867633154,1.843501847,-6.24152796918688));
#127539=CARTESIAN_POINT('Ctrl Pts',(4.85450131171783,1.97885290468778,-5.38489213629658));
#127540=CARTESIAN_POINT('Ctrl Pts',(4.84432163585891,1.97658649484386,-5.39399985764828));
#127541=CARTESIAN_POINT('Ctrl Pts',(4.83414196,1.974320085,-5.403107579));
#127542=CARTESIAN_POINT('Ctrl Pts',(4.538892973,1.908585653,-5.667265843));
#127543=CARTESIAN_POINT('Ctrl Pts',(4.216618428,1.843501847,-5.89767997));
#127544=CARTESIAN_POINT('',(4.22044662604908,1.84427517322959,-5.8949410741957));
#127545=CARTESIAN_POINT('Origin',(-0.136862052139167,2.01783541418011,0.14207413403895));
#127546=CARTESIAN_POINT('Ctrl Pts',(4.36679971634735,1.88359401259236,-6.0976274267159));
#127547=CARTESIAN_POINT('Ctrl Pts',(4.34241764086487,1.87734523493682,-6.06379033863203));
#127548=CARTESIAN_POINT('Ctrl Pts',(4.31801968949418,1.87094900376049,-6.02996395608223));
#127549=CARTESIAN_POINT('Ctrl Pts',(4.26924399912386,1.85785292379131,-5.96241140879724));
#127550=CARTESIAN_POINT('Ctrl Pts',(4.24483972189638,1.85114595296674,-5.92864848400608));
#127551=CARTESIAN_POINT('Ctrl Pts',(4.22044662594175,1.84427517327394,-5.89494107440453));
#127552=CARTESIAN_POINT('Ctrl Pts',(4.567485784,1.843494248,-5.948787575));
#127553=CARTESIAN_POINT('Ctrl Pts',(4.243612444,1.909007671,-6.19745789));
#127554=CARTESIAN_POINT('Ctrl Pts',(3.894656432,1.974320085,-6.40949696000001));
#127555=CARTESIAN_POINT('Ctrl Pts',(4.224271357,1.843494248,-5.892200905));
#127556=CARTESIAN_POINT('Ctrl Pts',(3.903478799,1.909007671,-6.122185394));
#127557=CARTESIAN_POINT('Ctrl Pts',(3.559613992,1.974320085,-6.315983552));
#127558=CARTESIAN_POINT('Origin',(-0.111940529213434,1.87499999749396,0.165099073720274));
#127559=CARTESIAN_POINT('Ctrl Pts',(3.49097203493613,1.97885290457087,-6.63865679804626));
#127560=CARTESIAN_POINT('Ctrl Pts',(3.47843992888034,1.97658649478541,-6.64518671007442));
#127561=CARTESIAN_POINT('Ctrl Pts',(3.46590782282453,1.974320085,-6.65171662210265));
#127562=CARTESIAN_POINT('Ctrl Pts',(3.10242947983344,1.908585653,-6.84110869980463));
#127563=CARTESIAN_POINT('Ctrl Pts',(2.72047859428653,1.843501847,-6.98976732606163));
#127564=CARTESIAN_POINT('Ctrl Pts',(3.58341313450755,1.97885290457087,-6.30257063543203));
#127565=CARTESIAN_POINT('Ctrl Pts',(3.57151356325381,1.97658649478541,-6.30927709371597));
#127566=CARTESIAN_POINT('Ctrl Pts',(3.559613992,1.974320085,-6.315983552));
#127567=CARTESIAN_POINT('Ctrl Pts',(3.214481544,1.908585653,-6.510496137));
#127568=CARTESIAN_POINT('Ctrl Pts',(2.850209373,1.843501847,-6.66624381));
#127569=CARTESIAN_POINT('',(2.8545368520132,1.84427517323806,-6.66439189667409));
#127570=CARTESIAN_POINT('Origin',(-0.103120705606142,2.0178354347729,0.168174104005968));
#127571=CARTESIAN_POINT('Ctrl Pts',(2.95389671312413,1.88359401258902,-6.89380114309682));
#127572=CARTESIAN_POINT('Ctrl Pts',(2.93735865075846,1.87734523494571,-6.85551372191643));
#127573=CARTESIAN_POINT('Ctrl Pts',(2.92080278241338,1.87094900380797,-6.81723334327731));
#127574=CARTESIAN_POINT('Ctrl Pts',(2.88768920088988,1.85785290772959,-6.74077471128772));
#127575=CARTESIAN_POINT('Ctrl Pts',(2.87111353481052,1.85114594513236,-6.70255499693849));
#127576=CARTESIAN_POINT('Ctrl Pts',(2.854536852026,1.84427517338418,-6.66439189732531));
#127577=CARTESIAN_POINT('Ctrl Pts',(3.18188702,1.843494248,-6.791582657));
#127578=CARTESIAN_POINT('Ctrl Pts',(2.812128892,1.909007671,-6.964816003));
#127579=CARTESIAN_POINT('Ctrl Pts',(2.425749146,1.974320085,-7.09688249000001));
#127580=CARTESIAN_POINT('Ctrl Pts',(2.858861218,1.843494248,-6.662537995));
#127581=CARTESIAN_POINT('Ctrl Pts',(2.496128744,1.909007671,-6.818184657));
#127582=CARTESIAN_POINT('Ctrl Pts',(2.118642431,1.974320085,-6.933531153));
#127583=CARTESIAN_POINT('Origin',(-0.0738320489149108,1.87500005047324,
0.18530320439424));
#127584=CARTESIAN_POINT('Ctrl Pts',(1.98224007482369,1.97885290466213,-7.23390448551782));
#127585=CARTESIAN_POINT('Ctrl Pts',(1.96859722411596,1.97658649483104,-7.23758769956478));
#127586=CARTESIAN_POINT('Ctrl Pts',(1.95495437340829,1.974320085,-7.2412709136117));
#127587=CARTESIAN_POINT('Ctrl Pts',(1.55926025408112,1.908585653,-7.34809801080844));
#127588=CARTESIAN_POINT('Ctrl Pts',(1.1542819576241,1.843501847,-7.4111729312694));
#127589=CARTESIAN_POINT('Ctrl Pts',(2.14476854387364,1.97885290466213,-6.92554793491932));
#127590=CARTESIAN_POINT('Ctrl Pts',(2.13170548743684,1.97658649483104,-6.92953954395966));
#127591=CARTESIAN_POINT('Ctrl Pts',(2.118642431,1.974320085,-6.933531153));
#127592=CARTESIAN_POINT('Ctrl Pts',(1.739764532,1.908585653,-7.049302868));
#127593=CARTESIAN_POINT('Ctrl Pts',(1.350527695,1.843501847,-7.123101498));
#127594=CARTESIAN_POINT('',(1.35515210699593,1.84427517325148,-7.12222316151573));
#127595=CARTESIAN_POINT('Origin',(-0.0645573202645811,2.01783546286368,
0.186410085552468));
#127596=CARTESIAN_POINT('Ctrl Pts',(1.40287278318668,1.88359401260551,-7.36762837997682));
#127597=CARTESIAN_POINT('Ctrl Pts',(1.39495203533525,1.8773452349598,-7.32668090293733));
#127598=CARTESIAN_POINT('Ctrl Pts',(1.38701238381451,1.87094900380986,-7.28573647595215));
#127599=CARTESIAN_POINT('Ctrl Pts',(1.37110933005997,1.85785291182603,-7.20394698873801));
#127600=CARTESIAN_POINT('Ctrl Pts',(1.36313729993217,1.8511459471543,-7.16305753829043));
#127601=CARTESIAN_POINT('Ctrl Pts',(1.35515210661453,1.84427517341028,-7.12222316206877));
#127602=CARTESIAN_POINT('Ctrl Pts',(1.647506757,1.843494248,-7.316810882));
#127603=CARTESIAN_POINT('Ctrl Pts',(1.249153319,1.909007671,-7.40650706100001));
#127604=CARTESIAN_POINT('Ctrl Pts',(0.843416526000001,1.974320085,-7.452425683));
#127605=CARTESIAN_POINT('Ctrl Pts',(1.359773906,1.843494248,-7.121342214));
#127606=CARTESIAN_POINT('Ctrl Pts',(0.972062484,1.909007671,-7.195373184));
#127607=CARTESIAN_POINT('Ctrl Pts',(0.578605504,1.974320085,-7.226874544));
#127608=CARTESIAN_POINT('Origin',(-0.0322711797376609,1.87500005190778,
0.196842596558592));
#127609=CARTESIAN_POINT('Ctrl Pts',(0.363832912865866,1.97607974481604,
-7.49138129256546));
#127610=CARTESIAN_POINT('Ctrl Pts',(0.358353393929661,1.97519991490802,
-7.49163938192452));
#127611=CARTESIAN_POINT('Ctrl Pts',(0.352873874993457,1.974320085,-7.49189747128358));
#127612=CARTESIAN_POINT('Ctrl Pts',(-0.0565155554200859,1.908585653,-7.51118001358909));
#127613=CARTESIAN_POINT('Ctrl Pts',(-0.465568481217692,1.843501847,-7.48573935389003));
#127614=CARTESIAN_POINT('Ctrl Pts',(0.589176870235917,1.97607974481604,
-7.22602816834229));
#127615=CARTESIAN_POINT('Ctrl Pts',(0.583891187117959,1.97519991490802,
-7.22645135617115));
#127616=CARTESIAN_POINT('Ctrl Pts',(0.578605504000001,1.974320085,-7.226874544));
#127617=CARTESIAN_POINT('Ctrl Pts',(0.183698063,1.908585653,-7.258492032));
#127618=CARTESIAN_POINT('Ctrl Pts',(-0.212303156,1.843501847,-7.246890876));
#127619=CARTESIAN_POINT('',(-0.207598044914298,1.84427517323019,-7.24702718644853));
#127620=CARTESIAN_POINT('Origin',(-0.0229753300834366,2.01783542455855,
0.195929666395933));
#127621=CARTESIAN_POINT('Ctrl Pts',(-0.21374791896889,1.8835940087603,-7.49695347696991));
#127622=CARTESIAN_POINT('Ctrl Pts',(-0.212680986910686,1.87734523105937,
-7.45526060255581));
#127623=CARTESIAN_POINT('Ctrl Pts',(-0.211633172836878,1.87094900376037,
-7.41356666842629));
#127624=CARTESIAN_POINT('Ctrl Pts',(-0.209582099320414,1.85785290956532,
-7.33027067337607));
#127625=CARTESIAN_POINT('Ctrl Pts',(-0.208577724648135,1.85114594601346,
-7.28862345213287));
#127626=CARTESIAN_POINT('Ctrl Pts',(-0.207598044645778,1.84427517335404,
-7.24702718686974));
#127627=CARTESIAN_POINT('Ctrl Pts',(0.036090908,1.843494248,-7.499913163));
#127628=CARTESIAN_POINT('Ctrl Pts',(-0.372231275,1.909007671,-7.501878081));
#127629=CARTESIAN_POINT('Ctrl Pts',(-0.778353314,1.974320085,-7.459501734));
#127630=CARTESIAN_POINT('Ctrl Pts',(-0.202894923,1.843494248,-7.247160385));
#127631=CARTESIAN_POINT('Ctrl Pts',(-0.597456338,1.909007671,-7.236114058));
#127632=CARTESIAN_POINT('Ctrl Pts',(-0.988486373,1.974320085,-7.18229731300001));
#127633=CARTESIAN_POINT('Origin',(0.0107986194233051,1.87500008133751,0.199177593578839));
#127634=CARTESIAN_POINT('Ctrl Pts',(-1.23840528663667,1.97885290464283,
-7.3976349043454));
#127635=CARTESIAN_POINT('Ctrl Pts',(-1.25233374400524,1.97658649482139,
-7.39524921454754));
#127636=CARTESIAN_POINT('Ctrl Pts',(-1.26626220137385,1.974320085,-7.39286352474967));
#127637=CARTESIAN_POINT('Ctrl Pts',(-1.67023999264394,1.908585653,-7.32366952359896));
#127638=CARTESIAN_POINT('Ctrl Pts',(-2.06427281170063,1.843501847,-7.21086879728102));
#127639=CARTESIAN_POINT('Ctrl Pts',(-0.961422888963519,1.97885290464283,
-7.18602201056086));
#127640=CARTESIAN_POINT('Ctrl Pts',(-0.974954630981765,1.97658649482139,
-7.18415966178044));
#127641=CARTESIAN_POINT('Ctrl Pts',(-0.988486373,1.974320085,-7.182297313));
#127642=CARTESIAN_POINT('Ctrl Pts',(-1.380957923,1.908585653,-7.128282175));
#127643=CARTESIAN_POINT('Ctrl Pts',(-1.765206948,1.843501847,-7.031823692));
#127644=CARTESIAN_POINT('',(-1.76064114303171,1.84427517321804,-7.03296827513242));
#127645=CARTESIAN_POINT('Origin',(0.0196809364373435,2.01783541913575,0.196288130969764));
#127646=CARTESIAN_POINT('Ctrl Pts',(-1.82037400642531,1.88359401257156,
-7.27572941159547));
#127647=CARTESIAN_POINT('Ctrl Pts',(-1.81036928315231,1.8773452349258,-7.23524065217637));
#127648=CARTESIAN_POINT('Ctrl Pts',(-1.80038299703606,1.87094900377655,
-7.19474672350987));
#127649=CARTESIAN_POINT('Ctrl Pts',(-1.78047370253419,1.85785291130399,
-7.11383907339911));
#127650=CARTESIAN_POINT('Ctrl Pts',(-1.77053988675437,1.85114594686103,
-7.07338144623067));
#127651=CARTESIAN_POINT('Ctrl Pts',(-1.76064114249265,1.8442751733294,-7.03296827581398));
#127652=CARTESIAN_POINT('Ctrl Pts',(-1.577012512,1.843494248,-7.332327839));
#127653=CARTESIAN_POINT('Ctrl Pts',(-1.976210748,1.909007671,-7.246469619));
#127654=CARTESIAN_POINT('Ctrl Pts',(-2.363728217,1.974320085,-7.117779774));
#127655=CARTESIAN_POINT('Ctrl Pts',(-1.756076611,1.843494248,-7.034109392));
#127656=CARTESIAN_POINT('Ctrl Pts',(-2.139038765,1.909007671,-6.93850228));
#127657=CARTESIAN_POINT('Ctrl Pts',(-2.509357726,1.974320085,-6.801883842));
#127658=CARTESIAN_POINT('Origin',(0.0533635186575132,1.87500006335565,0.192199759904844));
#127659=CARTESIAN_POINT('Ctrl Pts',(-2.7997248903699,1.97885290475382,-6.95846178108168));
#127660=CARTESIAN_POINT('Ctrl Pts',(-2.81281485569747,1.97658649487688,
-6.95313766064793));
#127661=CARTESIAN_POINT('Ctrl Pts',(-2.82590482102504,1.974320085,-6.94781354021427));
#127662=CARTESIAN_POINT('Ctrl Pts',(-3.20556317165334,1.908585653,-6.79339397287292));
#127663=CARTESIAN_POINT('Ctrl Pts',(-3.56613489944187,1.843501847,-6.59852505700183));
#127664=CARTESIAN_POINT('Ctrl Pts',(-2.48372767044605,1.97885290475382,
-6.81133930751265));
#127665=CARTESIAN_POINT('Ctrl Pts',(-2.49654269822303,1.97658649487688,
-6.80661157475634));
#127666=CARTESIAN_POINT('Ctrl Pts',(-2.509357726,1.974320085,-6.801883842));
#127667=CARTESIAN_POINT('Ctrl Pts',(-2.881041851,1.908585653,-6.664761766));
#127668=CARTESIAN_POINT('Ctrl Pts',(-3.235571625,1.843501847,-6.487956247));
#127669=CARTESIAN_POINT('',(-3.23135861738484,1.84427517325405,-6.49005558348848));
#127670=CARTESIAN_POINT('Origin',(0.061416984041453,2.01783542994364,0.187468286320502));
#127671=CARTESIAN_POINT('Ctrl Pts',(-3.34188142830792,1.88359401257738,
-6.71430029947091));
#127672=CARTESIAN_POINT('Ctrl Pts',(-3.32340672345605,1.87734523493612,
-6.67690886461151));
#127673=CARTESIAN_POINT('Ctrl Pts',(-3.30494891336787,1.87094900375898,
-6.63950841770348));
#127674=CARTESIAN_POINT('Ctrl Pts',(-3.2681123138241,1.85785290416819,-6.5647722127061));
#127675=CARTESIAN_POINT('Ctrl Pts',(-3.24971356186856,1.85114594335815,
-6.52739596080021));
#127676=CARTESIAN_POINT('Ctrl Pts',(-3.2313586170509,1.84427517334694,-6.49005558433552));
#127677=CARTESIAN_POINT('Ctrl Pts',(-3.116376579,1.843494248,-6.821891015));
#127678=CARTESIAN_POINT('Ctrl Pts',(-3.487784803,1.909007671,-6.652224292));
#127679=CARTESIAN_POINT('Ctrl Pts',(-3.838577816,1.974320085,-6.443238343));
#127680=CARTESIAN_POINT('Ctrl Pts',(-3.227146108,1.843494248,-6.492151261));
#127681=CARTESIAN_POINT('Ctrl Pts',(-3.580602117,1.909007671,-6.316453848));
#127682=CARTESIAN_POINT('Ctrl Pts',(-3.912894301,1.974320085,-6.103421843));
#127683=CARTESIAN_POINT('Origin',(0.0934331116373954,1.8750000554617,0.176234561179568));
#127684=CARTESIAN_POINT('Ctrl Pts',(-4.23013246931658,1.97885290501278,
-6.19391872016159));
#127685=CARTESIAN_POINT('Ctrl Pts',(-4.2417718706794,1.97658649500636,-6.18590511866234));
#127686=CARTESIAN_POINT('Ctrl Pts',(-4.25341127204229,1.974320085,-6.17789151716295));
#127687=CARTESIAN_POINT('Ctrl Pts',(-4.590997779011,1.908585653,-5.94546687142094));
#127688=CARTESIAN_POINT('Ctrl Pts',(-4.90124848337868,1.843501847,-5.67764161845627));
#127689=CARTESIAN_POINT('Ctrl Pts',(-3.88989610614884,1.97885290501277,
-6.11816595014865));
#127690=CARTESIAN_POINT('Ctrl Pts',(-3.90139520357438,1.97658649500636,
-6.11079389657425));
#127691=CARTESIAN_POINT('Ctrl Pts',(-3.912894301,1.974320085,-6.103421843));
#127692=CARTESIAN_POINT('Ctrl Pts',(-4.246411465,1.908585653,-5.889604505));
#127693=CARTESIAN_POINT('Ctrl Pts',(-4.55464456900001,1.843501847,-5.640719178));
#127694=CARTESIAN_POINT('',(-4.55098135447045,1.84427517323348,-5.64367510627636));
#127695=CARTESIAN_POINT('Origin',(0.100281084782381,2.0178354216955,0.169882325749594));
#127696=CARTESIAN_POINT('Ctrl Pts',(-4.70712618881639,1.8835940125805,-5.83891796798881));
#127697=CARTESIAN_POINT('Ctrl Pts',(-4.68104535907145,1.87734523494553,
-5.80637223946444));
#127698=CARTESIAN_POINT('Ctrl Pts',(-4.65497909171563,1.87094900375453,
-5.77381407758736));
#127699=CARTESIAN_POINT('Ctrl Pts',(-4.60293773645489,1.85785292930389,
-5.70874406817867));
#127700=CARTESIAN_POINT('Ctrl Pts',(-4.57693429465633,1.85114595572434,
-5.67619677356006));
#127701=CARTESIAN_POINT('Ctrl Pts',(-4.55098135450667,1.84427517335135,
-5.64367510622254));
#127702=CARTESIAN_POINT('Ctrl Pts',(-4.510022341,1.843494248,-5.992470149));
#127703=CARTESIAN_POINT('Ctrl Pts',(-4.836273917,1.909007671,-5.746928351));
#127704=CARTESIAN_POINT('Ctrl Pts',(-5.133939783,1.974320085,-5.467418248));
#127705=CARTESIAN_POINT('Ctrl Pts',(-4.54731784,1.843494248,-5.646627353));
#127706=CARTESIAN_POINT('Ctrl Pts',(-4.854740493,1.909007671,-5.399055054));
#127707=CARTESIAN_POINT('Ctrl Pts',(-5.133468287,1.974320085,-5.119570621));
#127708=CARTESIAN_POINT('Origin',(0.129133949454096,1.87500001391295,0.152028971897913));
#127709=CARTESIAN_POINT('Ctrl Pts',(-5.46274375875203,1.97885290469671,
-5.13975490206963));
#127710=CARTESIAN_POINT('Ctrl Pts',(-5.4723883492393,1.97658649484833,-5.12942652758237));
#127711=CARTESIAN_POINT('Ctrl Pts',(-5.48203293972668,1.974320085,-5.11909815309525));
#127712=CARTESIAN_POINT('Ctrl Pts',(-5.7617624326188,1.908585653,-4.81953634573062));
#127713=CARTESIAN_POINT('Ctrl Pts',(-6.00718513649799,1.843501847,-4.49127796844836));
#127714=CARTESIAN_POINT('Ctrl Pts',(-5.11417732576643,1.97885290469671,
-5.13891394976885));
#127715=CARTESIAN_POINT('Ctrl Pts',(-5.12382280638329,1.97658649484833,
-5.12924228538445));
#127716=CARTESIAN_POINT('Ctrl Pts',(-5.133468287,1.974320085,-5.119570621));
#127717=CARTESIAN_POINT('Ctrl Pts',(-5.413223597,1.908585653,-4.839055883));
#127718=CARTESIAN_POINT('Ctrl Pts',(-5.660747395,1.843501847,-4.529728351));
#127719=CARTESIAN_POINT('',(-5.65780526120229,1.84427517321323,-4.53340265363974));
#127720=CARTESIAN_POINT('Origin',(0.134456337787581,2.01783546924622,0.144353208218378));
#127721=CARTESIAN_POINT('Ctrl Pts',(-5.85227096027949,1.8835940126381,-4.69051432171716));
#127722=CARTESIAN_POINT('Ctrl Pts',(-5.8198035162661,1.87734523498062,-4.66433610172389));
#127723=CARTESIAN_POINT('Ctrl Pts',(-5.78734762151557,1.87094900379007,
-4.6381426087021));
#127724=CARTESIAN_POINT('Ctrl Pts',(-5.72253480594809,1.85785292328267,
-4.58578122911845));
#127725=CARTESIAN_POINT('Ctrl Pts',(-5.69014261976781,1.85114595273634,
-4.55958485635383));
#127726=CARTESIAN_POINT('Ctrl Pts',(-5.65780526166866,1.84427517329743,
-4.5334026538501));
#127727=CARTESIAN_POINT('Ctrl Pts',(-5.692784471,1.843494248,-4.882848039));
#127728=CARTESIAN_POINT('Ctrl Pts',(-5.958624237,1.909007671,-4.572912427));
#127729=CARTESIAN_POINT('Ctrl Pts',(-6.189244432,1.974320085,-4.235947753));
#127730=CARTESIAN_POINT('Ctrl Pts',(-5.65486204400001,1.843494248,-4.537073425));
#127731=CARTESIAN_POINT('Ctrl Pts',(-5.9018766,1.909007671,-4.229202446));
#127732=CARTESIAN_POINT('Ctrl Pts',(-6.114007001,1.974320085,-3.896333968));
#127733=CARTESIAN_POINT('Origin',(0.158796591899705,1.87500003312575,0.120714626166288));
#127734=CARTESIAN_POINT('Ctrl Pts',(-6.43992321904848,1.97885290464865,
-3.845261857605));
#127735=CARTESIAN_POINT('Ctrl Pts',(-6.44712202908693,1.9765864948243,-3.83310165304336));
#127736=CARTESIAN_POINT('Ctrl Pts',(-6.45432083912527,1.974320085,-3.8209414484817));
#127737=CARTESIAN_POINT('Ctrl Pts',(-6.6631134784233,1.908585653,-3.46824965757397));
#127738=CARTESIAN_POINT('Ctrl Pts',(-6.83223248791254,1.843501847,-3.09490715287089));
#127739=CARTESIAN_POINT('Ctrl Pts',(-6.09932529574889,1.97885290464865,
-3.9193720467135));
#127740=CARTESIAN_POINT('Ctrl Pts',(-6.10666614837438,1.9765864948243,-3.90785300735674));
#127741=CARTESIAN_POINT('Ctrl Pts',(-6.114007001,1.974320085,-3.896333968));
#127742=CARTESIAN_POINT('Ctrl Pts',(-6.326919411,1.908585653,-3.562238386));
#127743=CARTESIAN_POINT('Ctrl Pts',(-6.502159964,1.843501847,-3.20693246));
#127744=CARTESIAN_POINT('',(-6.50007648227949,1.84427517319966,-3.21115333101409));
#127745=CARTESIAN_POINT('Origin',(0.162344440832116,2.0178354426907,0.112074132583747));
#127746=CARTESIAN_POINT('Ctrl Pts',(-6.72377004575471,1.88359401261591,
-3.32278743899844));
#127747=CARTESIAN_POINT('Ctrl Pts',(-6.68643412903717,1.87734523495608,
-3.30420079201031));
#127748=CARTESIAN_POINT('Ctrl Pts',(-6.64910620829137,1.87094900376282,
-3.28559674629494));
#127749=CARTESIAN_POINT('Ctrl Pts',(-6.57455251052133,1.85785291958716,
-3.24839237571781));
#127750=CARTESIAN_POINT('Ctrl Pts',(-6.5372862009905,1.8511459509194,-3.22977182764321));
#127751=CARTESIAN_POINT('Ctrl Pts',(-6.50007648257382,1.84427517330869,
-3.21115333145443));
#127752=CARTESIAN_POINT('Ctrl Pts',(-6.609358326,1.843494248,-3.544909382));
#127753=CARTESIAN_POINT('Ctrl Pts',(-6.80235591100001,1.909007671,-3.1850722));
#127754=CARTESIAN_POINT('Ctrl Pts',(-6.955146889,1.974320085,-2.806409048));
#127755=CARTESIAN_POINT('Ctrl Pts',(-6.497991183,1.843494248,-3.215370987));
#127756=CARTESIAN_POINT('Ctrl Pts',(-6.673047516,1.909007671,-2.861597032));
#127757=CARTESIAN_POINT('Ctrl Pts',(-6.808661543,1.974320085,-2.490909068));
#127758=CARTESIAN_POINT('Origin',(0.181034151572665,1.8750000352612,0.0837558341553082));
#127759=CARTESIAN_POINT('Ctrl Pts',(-7.11597902687631,1.97885290480238,
-2.37096864369072));
#127760=CARTESIAN_POINT('Ctrl Pts',(-7.12039544836194,1.97658649490116,
-2.35754520615908));
#127761=CARTESIAN_POINT('Ctrl Pts',(-7.1248118698477,1.974320085,-2.34412176862744));
#127762=CARTESIAN_POINT('Ctrl Pts',(-7.25290474381949,1.908585653,-1.95479147088445));
#127763=CARTESIAN_POINT('Ctrl Pts',(-7.3378122417283,1.843501847,-1.55382191763709));
#127764=CARTESIAN_POINT('Ctrl Pts',(-6.79927559345178,1.97885290480238,
-2.51656466271515));
#127765=CARTESIAN_POINT('Ctrl Pts',(-6.80396856822594,1.97658649490116,
-2.50373686535758));
#127766=CARTESIAN_POINT('Ctrl Pts',(-6.808661543,1.974320085,-2.490909068));
#127767=CARTESIAN_POINT('Ctrl Pts',(-6.944775505,1.908585653,-2.118854581));
#127768=CARTESIAN_POINT('Ctrl Pts',(-7.03953876,1.843501847,-1.734183971));
#127769=CARTESIAN_POINT('',(-7.03841135126299,1.84427517321604,-1.73875404815287));
#127770=CARTESIAN_POINT('Origin',(0.18264148930203,2.01783545948557,0.0745546352118537));
#127771=CARTESIAN_POINT('Ctrl Pts',(-7.2808731168689,1.88359401257483,-1.79969070845451));
#127772=CARTESIAN_POINT('Ctrl Pts',(-7.24041451346207,1.87734523492967,
-1.78956472535042));
#127773=CARTESIAN_POINT('Ctrl Pts',(-7.19995997890268,1.87094900375224,
-1.77942003139443));
#127774=CARTESIAN_POINT('Ctrl Pts',(-7.11915142346661,1.85785291281086,
-1.75911230892196));
#127775=CARTESIAN_POINT('Ctrl Pts',(-7.07875353435036,1.85114594757699,
-1.74893825936029));
#127776=CARTESIAN_POINT('Ctrl Pts',(-7.0384113518051,1.84427517329423,-1.73875404767566));
#127777=CARTESIAN_POINT('Ctrl Pts',(-7.216885931,1.843494248,-2.041214701));
#127778=CARTESIAN_POINT('Ctrl Pts',(-7.328016983,1.909007671,-1.648301537));
#127779=CARTESIAN_POINT('Ctrl Pts',(-7.395834409,1.974320085,-1.245645776));
#127780=CARTESIAN_POINT('Ctrl Pts',(-7.037281477,1.843494248,-1.743321375));
#127781=CARTESIAN_POINT('Ctrl Pts',(-7.132194147,1.909007671,-1.360186522));
#127782=CARTESIAN_POINT('Ctrl Pts',(-7.184950639,1.974320085,-0.969012029));
#127783=CARTESIAN_POINT('Origin',(0.194806796921273,1.87500000247012,0.0428807018730129));
#127784=CARTESIAN_POINT('Ctrl Pts',(-7.45929956467652,1.97885290464129,
-0.78581157002746));
#127785=CARTESIAN_POINT('Ctrl Pts',(-7.46072709035288,1.97658649482061,
-0.771752565412755));
#127786=CARTESIAN_POINT('Ctrl Pts',(-7.46215461602913,1.974320085,-0.757693560798031));
#127787=CARTESIAN_POINT('Ctrl Pts',(-7.50355824419952,1.908585653,-0.349929406925505));
#127788=CARTESIAN_POINT('Ctrl Pts',(-7.50028405152686,1.843501847,0.0599183031176641));
#127789=CARTESIAN_POINT('Ctrl Pts',(-7.18129932238051,1.97885290464129,
-0.996085510899448));
#127790=CARTESIAN_POINT('Ctrl Pts',(-7.18312498069023,1.97658649482062,
-0.982548769949733));
#127791=CARTESIAN_POINT('Ctrl Pts',(-7.184950639,1.974320085,-0.969012029));
#127792=CARTESIAN_POINT('Ctrl Pts',(-7.237901615,1.908585653,-0.576395491));
#127793=CARTESIAN_POINT('Ctrl Pts',(-7.24775654700001,1.843501847,-0.180346967));
#127794=CARTESIAN_POINT('',(-7.24763792831109,1.84427517320559,-0.185052557572839));
#127795=CARTESIAN_POINT('Origin',(0.194398464462716,2.01783547761427,0.033549063015667));
#127796=CARTESIAN_POINT('Ctrl Pts',(-7.49753065349355,1.88359401255793,
-0.192442440658495));
#127797=CARTESIAN_POINT('Ctrl Pts',(-7.45584116260488,1.87734523490727,
-0.191250601215969));
#127798=CARTESIAN_POINT('Ctrl Pts',(-7.41415162318411,1.8709490037309,-0.190039613672411));
#127799=CARTESIAN_POINT('Ctrl Pts',(-7.33086684937498,1.85785292580537,
-0.187578127585151));
#127800=CARTESIAN_POINT('Ctrl Pts',(-7.28922627644197,1.85114595396848,
-0.186326292333262));
#127801=CARTESIAN_POINT('Ctrl Pts',(-7.24763792841524,1.84427517330524,
-0.185052557297351));
#127802=CARTESIAN_POINT('Ctrl Pts',(-7.486959971,1.843494248,-0.44207509));
#127803=CARTESIAN_POINT('Ctrl Pts',(-7.511028126,1.909007671,-0.034458126));
#127804=CARTESIAN_POINT('Ctrl Pts',(-7.490700931,1.974320085,0.373362509));
#127805=CARTESIAN_POINT('Ctrl Pts',(-7.24751631,1.843494248,-0.189755993));
#127806=CARTESIAN_POINT('Ctrl Pts',(-7.25784730700001,1.909007671,0.204824799));
#127807=CARTESIAN_POINT('Ctrl Pts',(-7.225279428,1.974320085,0.598194935));
#127808=CARTESIAN_POINT('Origin',(0.199470203545421,1.8750000464348,4.69240410416738E-7));
#127809=CARTESIAN_POINT('Ctrl Pts',(-7.45383154587489,1.97885290461806,
0.836089179740119));
#127810=CARTESIAN_POINT('Ctrl Pts',(-7.45220342637013,1.97658649480901,
0.850126368365636));
#127811=CARTESIAN_POINT('Ctrl Pts',(-7.45057530686525,1.974320085,0.864163556991164));
#127812=CARTESIAN_POINT('Ctrl Pts',(-7.40335370093351,1.908585653,1.27129496698858));
#127813=CARTESIAN_POINT('Ctrl Pts',(-7.31205091452462,1.843501847,1.6708568105315));
#127814=CARTESIAN_POINT('Ctrl Pts',(-7.2275334754168,1.97885290461807,0.570969491001635));
#127815=CARTESIAN_POINT('Ctrl Pts',(-7.22640645170834,1.97658649480901,
0.584582213000813));
#127816=CARTESIAN_POINT('Ctrl Pts',(-7.225279428,1.974320085,0.598194935));
#127817=CARTESIAN_POINT('Ctrl Pts',(-7.19259149,1.908585653,0.993015212));
#127818=CARTESIAN_POINT('Ctrl Pts',(-7.117077294,1.843501847,1.38192286));
#127819=CARTESIAN_POINT('',(-7.11797301108935,1.84427517323171,1.37730178478774));
#127820=CARTESIAN_POINT('Origin',(0.197065557394361,2.01783543356719,-0.00902521413189389));
#127821=CARTESIAN_POINT('Ctrl Pts',(-7.36361198972978,1.88359401259995,
1.42380422152944));
#127822=CARTESIAN_POINT('Ctrl Pts',(-7.32264096579086,1.87734523495685,
1.41600618821186));
#127823=CARTESIAN_POINT('Ctrl Pts',(-7.28166577807059,1.87094900376748,
1.40822684487038));
#127824=CARTESIAN_POINT('Ctrl Pts',(-7.19979893011702,1.85785291315852,
1.39272700326356));
#127825=CARTESIAN_POINT('Ctrl Pts',(-7.15886282522385,1.85114594774797,
1.38499808700488));
#127826=CARTESIAN_POINT('Ctrl Pts',(-7.11797301143247,1.84427517330014,
1.37730178429855));
#127827=CARTESIAN_POINT('Ctrl Pts',(-7.406952085,1.843494248,1.17773546));
#127828=CARTESIAN_POINT('Ctrl Pts',(-7.34283194100001,1.909007671,1.580996508));
#127829=CARTESIAN_POINT('Ctrl Pts',(-7.235310603,1.974320085,1.974912778));
#127830=CARTESIAN_POINT('Ctrl Pts',(-7.118865336,1.843494248,1.372682168));
#127831=CARTESIAN_POINT('Ctrl Pts',(-7.044131593,1.909007671,1.760258739));
#127832=CARTESIAN_POINT('Ctrl Pts',(-6.927762182,1.974320085,2.137430969));
#127833=CARTESIAN_POINT('Origin',(0.194806978520468,1.87500002902488,-0.0428797811532663));
#127834=CARTESIAN_POINT('Ctrl Pts',(-7.0998306478305,1.97885290483717,2.41889532596028));
#127835=CARTESIAN_POINT('Ctrl Pts',(-7.09522301202677,1.97658649491861,
2.43225433604723));
#127836=CARTESIAN_POINT('Ctrl Pts',(-7.09061537622306,1.974320085,2.44561334613417));
#127837=CARTESIAN_POINT('Ctrl Pts',(-6.95697656713838,1.908585653,2.83307500209442));
#127838=CARTESIAN_POINT('Ctrl Pts',(-6.78191440264508,1.843501847,3.20366791034174));
#127839=CARTESIAN_POINT('Ctrl Pts',(-6.9358161971165,1.97885290483725,2.1113265930496));
#127840=CARTESIAN_POINT('Ctrl Pts',(-6.9317891895583,1.9765864949186,2.12437878102484));
#127841=CARTESIAN_POINT('Ctrl Pts',(-6.927762182,1.974320085,2.137430969));
#127842=CARTESIAN_POINT('Ctrl Pts',(-6.810963781,1.908585653,2.515993627));
#127843=CARTESIAN_POINT('Ctrl Pts',(-6.653611416,1.843501847,2.87957551));
#127844=CARTESIAN_POINT('',(-6.65547958671787,1.84427517323839,2.87525502574098));
#127845=CARTESIAN_POINT('Origin',(0.19051800560499,2.01783542516648,-0.0511774464633824));
#127846=CARTESIAN_POINT('Ctrl Pts',(-6.88537901292717,1.8835940125991,2.9734753811648));
#127847=CARTESIAN_POINT('Ctrl Pts',(-6.84704221537492,1.87734523494283,
2.95705210249745));
#127848=CARTESIAN_POINT('Ctrl Pts',(-6.8086973335707,1.87094900373705,2.94064618172785));
#127849=CARTESIAN_POINT('Ctrl Pts',(-6.73207659066844,1.85785292950792,
2.90790980639309));
#127850=CARTESIAN_POINT('Ctrl Pts',(-6.69375898680419,1.85114595578537,
2.8915615135695));
#127851=CARTESIAN_POINT('Ctrl Pts',(-6.65547958676117,1.8442751732726,2.87525502562493));
#127852=CARTESIAN_POINT('Ctrl Pts',(-6.98060335100001,1.843494248,2.74247641));
#127853=CARTESIAN_POINT('Ctrl Pts',(-6.831293095,1.909007671,3.122525503));
#127854=CARTESIAN_POINT('Ctrl Pts',(-6.641605193,1.974320085,3.48411832));
#127855=CARTESIAN_POINT('Ctrl Pts',(-6.65734413,1.843494248,2.870935237));
#127856=CARTESIAN_POINT('Ctrl Pts',(-6.501040115,1.909007671,3.233384938));
#127857=CARTESIAN_POINT('Ctrl Pts',(-6.30631047600001,1.974320085,3.576723107));
#127858=CARTESIAN_POINT('Origin',(0.181034478711073,1.8750000457319,-0.0837549443066887));
#127859=CARTESIAN_POINT('Ctrl Pts',(-6.41384955941865,1.9788529048304,3.88859661749972));
#127860=CARTESIAN_POINT('Ctrl Pts',(-6.40647785532257,1.97658649491523,
3.90065279583295));
#127861=CARTESIAN_POINT('Ctrl Pts',(-6.39910615122662,1.974320085,3.91270897416618));
#127862=CARTESIAN_POINT('Ctrl Pts',(-6.185298940816,1.908585653,4.26238359811813));
#127863=CARTESIAN_POINT('Ctrl Pts',(-5.93466311168911,1.843501847,4.58667905970337));
#127864=CARTESIAN_POINT('Ctrl Pts',(-6.31978786192062,1.97885290483039,
3.5529604120461));
#127865=CARTESIAN_POINT('Ctrl Pts',(-6.31304916896038,1.97658649491523,
3.56484175952307));
#127866=CARTESIAN_POINT('Ctrl Pts',(-6.306310476,1.974320085,3.576723107));
#127867=CARTESIAN_POINT('Ctrl Pts',(-6.110862975,1.908585653,3.921326977));
#127868=CARTESIAN_POINT('Ctrl Pts',(-5.879030064,1.843501847,4.24258241));
#127869=CARTESIAN_POINT('',(-5.88178333417953,1.84427517320727,4.2387645372747));
#127870=CARTESIAN_POINT('Origin',(0.175062231257839,2.01783539552014,-0.0909367358907742));
#127871=CARTESIAN_POINT('Ctrl Pts',(-6.08519336616643,1.8835940125841,4.38411013664153));
#127872=CARTESIAN_POINT('Ctrl Pts',(-6.05128338114171,1.87734523493651,
4.35982954685315));
#127873=CARTESIAN_POINT('Ctrl Pts',(-6.01736176949405,1.87094900374865,
4.33556417130605));
#127874=CARTESIAN_POINT('Ctrl Pts',(-5.94956971260758,1.85785292613734,
4.28712194686461));
#127875=CARTESIAN_POINT('Ctrl Pts',(-5.91566236205193,1.85114595411764,
4.26291872248372));
#127876=CARTESIAN_POINT('Ctrl Pts',(-5.88178333430147,1.84427517325654,
4.23876453754314));
#127877=CARTESIAN_POINT('Ctrl Pts',(-6.227849362,1.843494248,4.178982211));
#127878=CARTESIAN_POINT('Ctrl Pts',(-6.000330577,1.909007671,4.518048676));
#127879=CARTESIAN_POINT('Ctrl Pts',(-5.737345705,1.974320085,4.83041036200001));
#127880=CARTESIAN_POINT('Ctrl Pts',(-5.884532912,1.843494248,4.234946565));
#127881=CARTESIAN_POINT('Ctrl Pts',(-5.653967226,1.909007671,4.55532165));
#127882=CARTESIAN_POINT('Ctrl Pts',(-5.3899827,1.974320085,4.848771648));
#127883=CARTESIAN_POINT('Origin',(0.158797259040808,1.87500001238811,-0.120713940850057));
#127884=CARTESIAN_POINT('Ctrl Pts',(-5.42796399395947,1.97885290484628,
5.17647145251215));
#127885=CARTESIAN_POINT('Ctrl Pts',(-5.41817291423544,1.97658649492317,
5.18666106564932));
#127886=CARTESIAN_POINT('Ctrl Pts',(-5.40838183451139,1.974320085,5.1968506787866));
#127887=CARTESIAN_POINT('Ctrl Pts',(-5.12440361073545,1.908585653,5.4923878739928));
#127888=CARTESIAN_POINT('Ctrl Pts',(-4.80991356956785,1.843501847,5.75522219450518));
#127889=CARTESIAN_POINT('Ctrl Pts',(-5.40825326913996,1.97885290484627,
4.82846175120978));
#127890=CARTESIAN_POINT('Ctrl Pts',(-5.39911798456999,1.97658649492317,
4.83861669960489));
#127891=CARTESIAN_POINT('Ctrl Pts',(-5.3899827,1.974320085,4.848771648));
#127892=CARTESIAN_POINT('Ctrl Pts',(-5.125025008,1.908585653,5.143303435));
#127893=CARTESIAN_POINT('Ctrl Pts',(-4.8295518,1.843501847,5.407210872));
#127894=CARTESIAN_POINT('',(-4.83306143001308,1.84427517321803,5.40407413043285));
#127895=CARTESIAN_POINT('Origin',(0.151420717533058,2.01783542771218,-0.12644393058023));
#127896=CARTESIAN_POINT('Ctrl Pts',(-5.00047084119181,1.88359401262403,
5.58974877456317));
#127897=CARTESIAN_POINT('Ctrl Pts',(-4.9725732618044,1.87734523497229,5.55874620709685));
#127898=CARTESIAN_POINT('Ctrl Pts',(-4.94466105705933,1.87094900379013,
5.52775599881469));
#127899=CARTESIAN_POINT('Ctrl Pts',(-4.88886753539191,1.85785291404029,
5.46587298098978));
#127900=CARTESIAN_POINT('Ctrl Pts',(-4.86095592515359,1.85114594819124,
5.43494656698241));
#127901=CARTESIAN_POINT('Ctrl Pts',(-4.8330614303298,1.84427517330843,5.40407413074732));
#127902=CARTESIAN_POINT('Ctrl Pts',(-5.18388806,1.843494248,5.420083448));
#127903=CARTESIAN_POINT('Ctrl Pts',(-4.88879927000001,1.909007671,5.702312914));
#127904=CARTESIAN_POINT('Ctrl Pts',(-4.564814309,1.974320085,5.950837783));
#127905=CARTESIAN_POINT('Ctrl Pts',(-4.836567476,1.843494248,5.400936498));
#127906=CARTESIAN_POINT('Ctrl Pts',(-4.542521114,1.909007671,5.66425658500001));
#127907=CARTESIAN_POINT('Ctrl Pts',(-4.221625324,1.974320085,5.894097015));
#127908=CARTESIAN_POINT('Origin',(0.129134690010521,1.87500003313059,-0.152028384945208));
#127909=CARTESIAN_POINT('Ctrl Pts',(-4.18827286488025,1.97885290466945,
6.22230023654242));
#127910=CARTESIAN_POINT('Ctrl Pts',(-4.17652022996333,1.9765864948347,6.23014682915233));
#127911=CARTESIAN_POINT('Ctrl Pts',(-4.16476759504639,1.974320085,6.23799342176233));
#127912=CARTESIAN_POINT('Ctrl Pts',(-3.82389686242845,1.908585653,6.46557419751403));
#127913=CARTESIAN_POINT('Ctrl Pts',(-3.46025781439298,1.843501847,6.65465753517254));
#127914=CARTESIAN_POINT('Ctrl Pts',(-4.24383476395218,1.97885290466945,
5.87818958520869));
#127915=CARTESIAN_POINT('Ctrl Pts',(-4.23273004397611,1.9765864948347,5.88614330010443));
#127916=CARTESIAN_POINT('Ctrl Pts',(-4.221625324,1.974320085,5.894097015));
#127917=CARTESIAN_POINT('Ctrl Pts',(-3.899546568,1.908585653,6.124784741));
#127918=CARTESIAN_POINT('Ctrl Pts',(-3.554249061,1.843501847,6.319004163));
#127919=CARTESIAN_POINT('',(-3.55835094425643,1.84427517323502,6.3166952236111));
#127920=CARTESIAN_POINT('Origin',(0.120698810536738,2.01783543734752,-0.156038612833972));
#127921=CARTESIAN_POINT('Ctrl Pts',(-3.68193185676623,1.88359401262509,
6.5340169723509));
#127922=CARTESIAN_POINT('Ctrl Pts',(-3.66135114289436,1.87734523497312,
6.49774207272003));
#127923=CARTESIAN_POINT('Ctrl Pts',(-3.64075348875807,1.87094900379698,
6.4614760993466));
#127924=CARTESIAN_POINT('Ctrl Pts',(-3.59956739575161,1.85785291007888,
6.38904589216518));
#127925=CARTESIAN_POINT('Ctrl Pts',(-3.57895661493645,1.85114594625855,
6.35284236110538));
#127926=CARTESIAN_POINT('Ctrl Pts',(-3.55835094491587,1.84427517333389,
6.31669522370333));
#127927=CARTESIAN_POINT('Ctrl Pts',(-3.897533913,1.843494248,6.407747607));
#127928=CARTESIAN_POINT('Ctrl Pts',(-3.548673142,1.909007671,6.619943338));
#127929=CARTESIAN_POINT('Ctrl Pts',(-3.178837269,1.974320085,6.793010644));
#127930=CARTESIAN_POINT('Ctrl Pts',(-3.562449519,1.843494248,6.314384643));
#127931=CARTESIAN_POINT('Ctrl Pts',(-3.218671763,1.909007671,6.508337177));
#127932=CARTESIAN_POINT('Ctrl Pts',(-2.85586944,1.974320085,6.663820956));
#127933=CARTESIAN_POINT('Origin',(0.0934339420673402,1.87500003180126,-0.176234096547346));
#127934=CARTESIAN_POINT('Ctrl Pts',(-2.7527427519229,1.97885290481218,6.97718117610168));
#127935=CARTESIAN_POINT('Ctrl Pts',(-2.73957810122948,1.97658649490612,
6.98231785079368));
#127936=CARTESIAN_POINT('Ctrl Pts',(-2.72641345053611,1.974320085,6.98745452548581));
#127937=CARTESIAN_POINT('Ctrl Pts',(-2.34458894761934,1.908585653,7.13643745763093));
#127938=CARTESIAN_POINT('Ctrl Pts',(-1.94880424992615,1.843501847,7.2429284854553));
#127939=CARTESIAN_POINT('Ctrl Pts',(-2.88097926358645,1.97885290481218,
6.6530598058356));
#127940=CARTESIAN_POINT('Ctrl Pts',(-2.86842435179319,1.97658649490612,
6.65844038091781));
#127941=CARTESIAN_POINT('Ctrl Pts',(-2.85586944,1.974320085,6.66382095600001));
#127942=CARTESIAN_POINT('Ctrl Pts',(-2.491729664,1.908585653,6.819877919));
#127943=CARTESIAN_POINT('Ctrl Pts',(-2.112753586,1.843501847,6.935327843));
#127944=CARTESIAN_POINT('',(-2.11725592452661,1.84427517324134,6.93395466841877));
#127945=CARTESIAN_POINT('Origin',(0.08433334788541,2.0178354534903,-0.178337430490919));
#127946=CARTESIAN_POINT('Ctrl Pts',(-2.19122983104428,1.88359401259107,
7.1727617986861));
#127947=CARTESIAN_POINT('Ctrl Pts',(-2.178928313942,1.8773452349571,7.13291074102052));
#127948=CARTESIAN_POINT('Ctrl Pts',(-2.16660833371645,1.87094900378916,
7.09306475921236));
#127949=CARTESIAN_POINT('Ctrl Pts',(-2.14195551515702,1.85785291701669,
7.01347417968665));
#127950=CARTESIAN_POINT('Ctrl Pts',(-2.12960928501872,1.85114594968925,
6.97368633612843));
#127951=CARTESIAN_POINT('Ctrl Pts',(-2.11725592405781,1.84427517337193,
6.93395466915275));
#127952=CARTESIAN_POINT('Ctrl Pts',(-2.428935412,1.843494248,7.09579261));
#127953=CARTESIAN_POINT('Ctrl Pts',(-2.042615002,1.909007671,7.228032569));
#127954=CARTESIAN_POINT('Ctrl Pts',(-1.644221332,1.974320085,7.317549878));
#127955=CARTESIAN_POINT('Ctrl Pts',(-2.121755383,1.843494248,6.932579181));
#127956=CARTESIAN_POINT('Ctrl Pts',(-1.744320898,1.909007671,7.048095157));
#127957=CARTESIAN_POINT('Ctrl Pts',(-1.356576276,1.974320085,7.121952036));
#127958=CARTESIAN_POINT('Origin',(0.0533643618955854,1.87500006267099,-0.19219931587071));
#127959=CARTESIAN_POINT('Ctrl Pts',(-1.18849744514977,1.97885290443969,
7.40581687957402));
#127960=CARTESIAN_POINT('Ctrl Pts',(-1.17453634458622,1.97658649471982,
7.40800345071329));
#127961=CARTESIAN_POINT('Ctrl Pts',(-1.16057524402267,1.974320085,7.41019002185252));
#127962=CARTESIAN_POINT('Ctrl Pts',(-0.755650658846319,1.908585653,7.47360883382083));
#127963=CARTESIAN_POINT('Ctrl Pts',(-0.346226765269648,1.843501847,7.4925281505468));
#127964=CARTESIAN_POINT('Ctrl Pts',(-1.38341237288645,1.97885290443961,
7.11684034579532));
#127965=CARTESIAN_POINT('Ctrl Pts',(-1.36999432444322,1.97658649471983,
7.11939619089766));
#127966=CARTESIAN_POINT('Ctrl Pts',(-1.356576276,1.974320085,7.121952036));
#127967=CARTESIAN_POINT('Ctrl Pts',(-0.967402251,1.908585653,7.19608118600001));
#127968=CARTESIAN_POINT('Ctrl Pts',(-0.572468102,1.843501847,7.2273633));
#127969=CARTESIAN_POINT('',(-0.577160369379612,1.84427517324856,7.22699009949689));
#127970=CARTESIAN_POINT('Origin',(0.0440243840339853,2.01783543703188,-0.192297093393963));
#127971=CARTESIAN_POINT('Ctrl Pts',(-0.598068334408665,1.8835940126117,
7.4761162553008));
#127972=CARTESIAN_POINT('Ctrl Pts',(-0.5946212192703,1.8773452349364,7.43455243048903));
#127973=CARTESIAN_POINT('Ctrl Pts',(-0.591154981516255,1.87094900377116,
7.3929895940939));
#127974=CARTESIAN_POINT('Ctrl Pts',(-0.584188154548803,1.85785291826439,
7.30996017883959));
#127975=CARTESIAN_POINT('Ctrl Pts',(-0.580683782159009,1.85114595026308,
7.26844847389072));
#127976=CARTESIAN_POINT('Ctrl Pts',(-0.577160369361556,1.84427517331935,
7.22699009982512));
#127977=CARTESIAN_POINT('Ctrl Pts',(-0.846762591,1.843494248,7.452046237));
#127978=CARTESIAN_POINT('Ctrl Pts',(-0.441046456,1.909007671,7.49814703));
#127979=CARTESIAN_POINT('Ctrl Pts',(-0.032723432,1.974320085,7.499928611));
#127980=CARTESIAN_POINT('Ctrl Pts',(-0.581850323,1.843494248,7.226614021));
#127981=CARTESIAN_POINT('Ctrl Pts',(-0.188407526,1.909007671,7.25829204));
#127982=CARTESIAN_POINT('Ctrl Pts',(0.206148888,1.974320085,7.247068555));
#127983=CARTESIAN_POINT('Origin',(0.0107996477400095,1.87500005687486,-0.199177772428364));
#127984=CARTESIAN_POINT('Ctrl Pts',(-1.361045197,4.043593265,7.121099351));
#127985=CARTESIAN_POINT('Ctrl Pts',(-0.970451525,3.977881214,7.195752943));
#127986=CARTESIAN_POINT('Ctrl Pts',(-0.574036077000001,3.913265985,7.227238932));
#127987=CARTESIAN_POINT('Ctrl Pts',(-0.560316581672474,3.91102972418618,
7.2283286268672));
#127988=CARTESIAN_POINT('Ctrl Pts',(-0.546597086344946,3.90879346337243,
7.22941832173442));
#127989=CARTESIAN_POINT('Ctrl Pts',(-1.64941712647202,4.043593265,7.31692694226861));
#127990=CARTESIAN_POINT('Ctrl Pts',(-1.24808227386308,3.977881214,7.40739779012264));
#127991=CARTESIAN_POINT('Ctrl Pts',(-0.839260127710279,3.913265985,7.45343136981116));
#127992=CARTESIAN_POINT('Ctrl Pts',(-0.825111250434607,3.91102972418618,
7.45502454052292));
#127993=CARTESIAN_POINT('Ctrl Pts',(-0.810962373158929,3.90879346337243,
7.45661771123472));
#127994=CARTESIAN_POINT('',(-1.35637331166053,4.04280735947538,7.12199069250356));
#127995=CARTESIAN_POINT('Origin',(0.0550901651735161,4.16060449436388,-0.184791223054491));
#127996=CARTESIAN_POINT('Ctrl Pts',(-1.4023512112938,4.00345494164046,7.36772767377926));
#127997=CARTESIAN_POINT('Ctrl Pts',(-1.39471645654411,4.00969641606142,
7.32672440067642));
#127998=CARTESIAN_POINT('Ctrl Pts',(-1.38706468140527,4.01609134931217,
7.28572337574004));
#127999=CARTESIAN_POINT('Ctrl Pts',(-1.37174236273169,4.02919780697387,
7.20382449064816));
#128000=CARTESIAN_POINT('Ctrl Pts',(-1.36406293274999,4.03591692798231,
7.1628791187943));
#128001=CARTESIAN_POINT('Ctrl Pts',(-1.35637331617947,4.04280735924498,
7.1219906928173));
#128002=CARTESIAN_POINT('Ctrl Pts',(-2.114258167,3.913265985,6.934869314));
#128003=CARTESIAN_POINT('Ctrl Pts',(-1.738111442,3.978309763,7.049546498));
#128004=CARTESIAN_POINT('Ctrl Pts',(-1.351767779,4.043585554,7.122866268));
#128005=CARTESIAN_POINT('Ctrl Pts',(-1.95071269,3.913265985,7.241872686));
#128006=CARTESIAN_POINT('Ctrl Pts',(-1.557914128,3.978309763,7.347679177));
#128007=CARTESIAN_POINT('Ctrl Pts',(-1.155975786,4.043585554,7.410379206));
#128008=CARTESIAN_POINT('Origin',(0.0413517804109204,4.01785698658068,-0.195051286303896));
#128009=CARTESIAN_POINT('Ctrl Pts',(-2.860050579,4.043593265,6.662027521));
#128010=CARTESIAN_POINT('Ctrl Pts',(-2.494637086,3.977881214,6.818901846));
#128011=CARTESIAN_POINT('Ctrl Pts',(-2.114258167,3.913265985,6.934869314));
#128012=CARTESIAN_POINT('Ctrl Pts',(-2.10109367821903,3.91102972422222,
6.93888281831157));
#128013=CARTESIAN_POINT('Ctrl Pts',(-2.08792918943805,3.90879346344451,
6.9428963226233));
#128014=CARTESIAN_POINT('Ctrl Pts',(-3.18377767658012,4.043593265,6.79128533119683));
#128015=CARTESIAN_POINT('Ctrl Pts',(-2.81127436820558,3.977881214,6.96591615008532));
#128016=CARTESIAN_POINT('Ctrl Pts',(-2.42190611501457,3.913265985,7.09875816714873));
#128017=CARTESIAN_POINT('Ctrl Pts',(-2.40843051543541,3.91102972422222,
7.1033556807225));
#128018=CARTESIAN_POINT('Ctrl Pts',(-2.39495491585624,3.90879346344451,
7.10795319429614));
#128019=CARTESIAN_POINT('',(-2.85567953173816,4.04280735940842,6.66390234035358));
#128020=CARTESIAN_POINT('Origin',(0.093526238274001,4.1606042522063,-0.168626831068563));
#128021=CARTESIAN_POINT('Ctrl Pts',(-2.95340868090112,4.00345494158623,
6.89401023824049));
#128022=CARTESIAN_POINT('Ctrl Pts',(-2.93713793079008,4.00969641602971,
6.85560684540525));
#128023=CARTESIAN_POINT('Ctrl Pts',(-2.92085104149721,4.01609134928399,
6.81720930716438));
#128024=CARTESIAN_POINT('Ctrl Pts',(-2.88828110970197,4.02919780727587,
6.74051901626863));
#128025=CARTESIAN_POINT('Ctrl Pts',(-2.87197917614151,4.03591692811964,
6.70218177595648));
#128026=CARTESIAN_POINT('Ctrl Pts',(-2.85567953565621,4.04280735921878,
6.66390233986534));
#128027=CARTESIAN_POINT('Ctrl Pts',(-3.555619896,3.913265985,6.318232914));
#128028=CARTESIAN_POINT('Ctrl Pts',(-3.212919477,3.978309763,6.511089437));
#128029=CARTESIAN_POINT('Ctrl Pts',(-2.851369896,4.043585554,6.665747499));
#128030=CARTESIAN_POINT('Ctrl Pts',(-3.46189467,3.913265985,6.653216162));
#128031=CARTESIAN_POINT('Ctrl Pts',(-3.101024788,3.978309763,6.840989036));
#128032=CARTESIAN_POINT('Ctrl Pts',(-2.721962195,4.043585554,6.988628035));
#128033=CARTESIAN_POINT('Origin',(0.08231519453825,4.01785696096065,-0.18160153963801));
#128034=CARTESIAN_POINT('Ctrl Pts',(-4.225323174,4.043593265,5.891446688));
#128035=CARTESIAN_POINT('Ctrl Pts',(-3.902176188,3.977881214,6.123206478));
#128036=CARTESIAN_POINT('Ctrl Pts',(-3.555619896,3.913265985,6.318232914));
#128037=CARTESIAN_POINT('Ctrl Pts',(-3.54362597031878,3.9110297241893,6.32498256083445));
#128038=CARTESIAN_POINT('Ctrl Pts',(-3.53163204463758,3.90879346337866,
6.3317322076689));
#128039=CARTESIAN_POINT('Ctrl Pts',(-4.56926832085833,4.043593265,5.94809076502108));
#128040=CARTESIAN_POINT('Ctrl Pts',(-4.24301439629109,3.977881214,6.1987160133802));
#128041=CARTESIAN_POINT('Ctrl Pts',(-3.89130646372376,3.913265985,6.41215492265816));
#128042=CARTESIAN_POINT('Ctrl Pts',(-3.87913424552404,3.9110297241893,6.41954180460044));
#128043=CARTESIAN_POINT('Ctrl Pts',(-3.86696202732437,3.90879346337866,
6.42692868654285));
#128044=CARTESIAN_POINT('',(-4.22145735075434,4.04280735946812,5.89421732096231));
#128045=CARTESIAN_POINT('Origin',(0.127589615055383,4.16060422397286,-0.144579345889145));
#128046=CARTESIAN_POINT('Ctrl Pts',(-4.36636804309703,4.00345494166535,
6.0979365453881));
#128047=CARTESIAN_POINT('Ctrl Pts',(-4.34222209965502,4.00969641612163,
6.06392873275961));
#128048=CARTESIAN_POINT('Ctrl Pts',(-4.31806165314822,4.01609134933484,
6.02993010761872));
#128049=CARTESIAN_POINT('Ctrl Pts',(-4.26976703323223,4.02919780985992,
5.96203435267121));
#128050=CARTESIAN_POINT('Ctrl Pts',(-4.24560486129794,4.03591692942932,
5.9280978565823));
#128051=CARTESIAN_POINT('Ctrl Pts',(-4.22145735427668,4.04280735935845,
5.89421731921874));
#128052=CARTESIAN_POINT('Ctrl Pts',(-4.830724789,3.913265985,5.406162966));
#128053=CARTESIAN_POINT('Ctrl Pts',(-4.537494967,3.978309763,5.66818106999999));
#128054=CARTESIAN_POINT('Ctrl Pts',(-4.217645127,4.043585554,5.89694578400001));
#128055=CARTESIAN_POINT('Ctrl Pts',(-4.811202304,3.913265985,5.753462644));
#128056=CARTESIAN_POINT('Ctrl Pts',(-4.499134977,3.978309763,6.01442185));
#128057=CARTESIAN_POINT('Ctrl Pts',(-4.160672677,4.043585554,6.240096384));
#128058=CARTESIAN_POINT('Origin',(0.119429677617298,4.01785699117882,-0.159660485123626));
#128059=CARTESIAN_POINT('Ctrl Pts',(-5.393024354,4.043593265,4.845388355));
#128060=CARTESIAN_POINT('Ctrl Pts',(-5.12725387,3.977881214,5.14119678));
#128061=CARTESIAN_POINT('Ctrl Pts',(-4.830724789,3.913265985,5.406162966));
#128062=CARTESIAN_POINT('Ctrl Pts',(-4.82046224918153,3.911029724198,5.41533314932637));
#128063=CARTESIAN_POINT('Ctrl Pts',(-4.81019970936308,3.90879346339606,
5.42450333265286));
#128064=CARTESIAN_POINT('Ctrl Pts',(-5.74110505755348,4.043593265,4.82677008554403));
#128065=CARTESIAN_POINT('Ctrl Pts',(-5.47635578817261,3.977881214,5.14167080416162));
#128066=CARTESIAN_POINT('Ctrl Pts',(-5.17875364692804,3.913265985,5.42572643982063));
#128067=CARTESIAN_POINT('Ctrl Pts',(-5.16845396969476,3.911029724198,5.4355572876477));
#128068=CARTESIAN_POINT('Ctrl Pts',(-5.15815429246146,3.90879346339607,
5.44538813547477));
#128069=CARTESIAN_POINT('',(-5.38984451562663,4.04280735947174,4.84892525021678));
#128070=CARTESIAN_POINT('Origin',(0.155686880665156,4.16060425506628,-0.11377110263744));
#128071=CARTESIAN_POINT('Ctrl Pts',(-5.57516088824713,4.00345494158135,
5.01673011704008));
#128072=CARTESIAN_POINT('Ctrl Pts',(-5.54426878915666,4.00969641603625,
4.98870805233074));
#128073=CARTESIAN_POINT('Ctrl Pts',(-5.51336450100241,4.01609134927232,
4.96069807790655));
#128074=CARTESIAN_POINT('Ctrl Pts',(-5.45160341771255,4.02919780652563,
4.90477161763664));
#128075=CARTESIAN_POINT('Ctrl Pts',(-5.42071079214696,4.0359169277958,4.87682268306445));
#128076=CARTESIAN_POINT('Ctrl Pts',(-5.38984451945149,4.04280735930418,
4.8489252475705));
#128077=CARTESIAN_POINT('Ctrl Pts',(-5.87995036100001,3.913265985,4.241306845));
#128078=CARTESIAN_POINT('Ctrl Pts',(-5.649902236,3.978309763,4.560234855));
#128079=CARTESIAN_POINT('Ctrl Pts',(-5.386707959,4.043585554,4.852409439));
#128080=CARTESIAN_POINT('Ctrl Pts',(-5.935543465,3.913265985,4.584683607));
#128081=CARTESIAN_POINT('Ctrl Pts',(-5.686870614,3.978309763,4.906626983));
#128082=CARTESIAN_POINT('Ctrl Pts',(-5.404834728,4.043585554,5.199784761));
#128083=CARTESIAN_POINT('Origin',(0.150959951003408,4.01785697866393,-0.130254007742173));
#128084=CARTESIAN_POINT('Ctrl Pts',(-6.30855371000001,4.043593265,3.572765048));
#128085=CARTESIAN_POINT('Ctrl Pts',(-6.112586858,3.977881214,3.918790435));
#128086=CARTESIAN_POINT('Ctrl Pts',(-5.879950361,3.913265985,4.241306845));
#128087=CARTESIAN_POINT('Ctrl Pts',(-5.87189907219411,3.91102972423848,
4.25246877700563));
#128088=CARTESIAN_POINT('Ctrl Pts',(-5.86384778338835,3.90879346347703,
4.2636307090113));
#128089=CARTESIAN_POINT('Ctrl Pts',(-6.64449410151252,4.043593265,3.47975500206386));
#128090=CARTESIAN_POINT('Ctrl Pts',(-6.45362886927749,3.977881214,3.8442067835082));
#128091=CARTESIAN_POINT('Ctrl Pts',(-6.22404806647888,3.913265985,4.18559701939786));
#128092=CARTESIAN_POINT('Ctrl Pts',(-6.21610253182957,3.91102972423849,
4.19741215339487));
#128093=CARTESIAN_POINT('Ctrl Pts',(-6.20815699718011,3.90879346347704,
4.20922728739196));
#128094=CARTESIAN_POINT('',(-6.30620854175752,4.04280735942323,3.57690282405529));
#128095=CARTESIAN_POINT('Origin',(0.176504357918572,4.16060427540505,-0.0776430649302001));
#128096=CARTESIAN_POINT('Ctrl Pts',(-6.52326540639354,4.00345494158901,
3.70094696449352));
#128097=CARTESIAN_POINT('Ctrl Pts',(-6.48707163187172,4.00969641603995,
3.68022092820222));
#128098=CARTESIAN_POINT('Ctrl Pts',(-6.45086855211453,4.01609134930151,
3.65950931972563));
#128099=CARTESIAN_POINT('Ctrl Pts',(-6.37852886526694,4.02919780789907,
3.61816719197021));
#128100=CARTESIAN_POINT('Ctrl Pts',(-6.34235030148427,4.03591692842555,
3.59751269169148));
#128101=CARTESIAN_POINT('Ctrl Pts',(-6.30620854453905,4.04280735922747,
3.57690282104795));
#128102=CARTESIAN_POINT('Ctrl Pts',(-6.654235988,3.913265985,2.878131931));
#128103=CARTESIAN_POINT('Ctrl Pts',(-6.498126356,3.978309763,3.239057128));
#128104=CARTESIAN_POINT('Ctrl Pts',(-6.303894313,4.043585554,3.580979822));
#128105=CARTESIAN_POINT('Ctrl Pts',(-6.78234521,3.913265985,3.201529861));
#128106=CARTESIAN_POINT('Ctrl Pts',(-6.608694501,3.978309763,3.569403691));
#128107=CARTESIAN_POINT('Ctrl Pts',(-6.396272715,4.043585554,3.916336982));
#128108=CARTESIAN_POINT('Origin',(0.17543108332065,4.01785695518326,-0.0947566751364476));
#128109=CARTESIAN_POINT('Ctrl Pts',(-6.929102105,4.043593265,2.133083219));
#128110=CARTESIAN_POINT('Ctrl Pts',(-6.812102079,3.977881214,2.513145805));
#128111=CARTESIAN_POINT('Ctrl Pts',(-6.654235988,3.913265985,2.878131931));
#128112=CARTESIAN_POINT('Ctrl Pts',(-6.64877241920947,3.91102972421517,
2.89076369247807));
#128113=CARTESIAN_POINT('Ctrl Pts',(-6.64330885041899,3.9087934634304,2.90339545395617));
#128114=CARTESIAN_POINT('Ctrl Pts',(-7.23719398613233,4.043593265,1.97003044157168));
#128115=CARTESIAN_POINT('Ctrl Pts',(-7.12913743724499,3.977881214,2.36699192665264));
#128116=CARTESIAN_POINT('Ctrl Pts',(-6.9783129155358,3.913265985,2.74975373474382));
#128117=CARTESIAN_POINT('Ctrl Pts',(-6.97309304758036,3.91102972421517,
2.76300069269182));
#128118=CARTESIAN_POINT('Ctrl Pts',(-6.96787317962509,3.9087934634304,2.7762476506398));
#128119=CARTESIAN_POINT('',(-6.92770126536622,4.04280735945235,2.13762839710923));
#128120=CARTESIAN_POINT('Origin',(0.189068793117305,4.16060424051219,-0.0378846249697654));
#128121=CARTESIAN_POINT('Ctrl Pts',(-7.16634928428786,4.00345494158682,
2.21211164520099));
#128122=CARTESIAN_POINT('Ctrl Pts',(-7.12654621497235,4.00969641602803,
2.19965076379814));
#128123=CARTESIAN_POINT('Ctrl Pts',(-7.0867371595319,4.01609134928607,2.18720597323838));
#128124=CARTESIAN_POINT('Ctrl Pts',(-7.00720139359496,4.02919780879388,
2.16238129410652));
#128125=CARTESIAN_POINT('Ctrl Pts',(-6.96742856043411,4.03591692888643,
2.14998700724193));
#128126=CARTESIAN_POINT('Ctrl Pts',(-6.92770126721526,4.04280735930234,
2.13762839403927));
#128127=CARTESIAN_POINT('Ctrl Pts',(-7.117376937,3.913265985,1.380378766));
#128128=CARTESIAN_POINT('Ctrl Pts',(-7.042505309,3.978309763,1.766424689));
#128129=CARTESIAN_POINT('Ctrl Pts',(-6.926317576,4.043585554,2.142107568));
#128130=CARTESIAN_POINT('Ctrl Pts',(-7.312012032,3.913265985,1.668676136));
#128131=CARTESIAN_POINT('Ctrl Pts',(-7.221503179,3.978309763,2.06527905));
#128132=CARTESIAN_POINT('Ctrl Pts',(-7.088628098,4.043585554,2.449765639));
#128133=CARTESIAN_POINT('Origin',(0.191699739144654,4.01785698088617,-0.0548288895525728));
#128134=CARTESIAN_POINT('Ctrl Pts',(-7.225653387,4.043593265,0.593660789));
#128135=CARTESIAN_POINT('Ctrl Pts',(-7.193090978,3.977881214,0.989989269000001));
#128136=CARTESIAN_POINT('Ctrl Pts',(-7.117376937,3.913265985,1.380378766));
#128137=CARTESIAN_POINT('Ctrl Pts',(-7.11475655877205,3.91102972423475,
1.39388970960905));
#128138=CARTESIAN_POINT('Ctrl Pts',(-7.11213618054409,3.90879346346956,
1.40740065321813));
#128139=CARTESIAN_POINT('Ctrl Pts',(-7.49149072463913,4.043593265,0.368189448020171));
#128140=CARTESIAN_POINT('Ctrl Pts',(-7.47129546192345,3.977881214,0.779099157186393));
#128141=CARTESIAN_POINT('Ctrl Pts',(-7.40627960745195,3.913265985,1.18533502103219));
#128142=CARTESIAN_POINT('Ctrl Pts',(-7.40402948148748,3.91102972423475,
1.19939438966423));
#128143=CARTESIAN_POINT('Ctrl Pts',(-7.40177935552301,3.90879346346956,
1.21345375829623));
#128144=CARTESIAN_POINT('',(-7.22526237695295,4.04280735944336,0.598400842538234));
#128145=CARTESIAN_POINT('Origin',(0.19279253096347,4.16060420866803,0.00364529811502957));
#128146=CARTESIAN_POINT('Ctrl Pts',(-7.4743426348343,4.00345494159327,0.619840443920183));
#128147=CARTESIAN_POINT('Ctrl Pts',(-7.43279141797487,4.00969641603819,
0.616227374350984));
#128148=CARTESIAN_POINT('Ctrl Pts',(-7.39123781394975,4.01609134930466,
0.612631306257523));
#128149=CARTESIAN_POINT('Ctrl Pts',(-7.30822498460285,4.02919780773243,
0.605484853522622));
#128150=CARTESIAN_POINT('Ctrl Pts',(-7.26671760915875,4.03591692837949,
0.601930321309054));
#128151=CARTESIAN_POINT('Ctrl Pts',(-7.22526237832533,4.04280735930948,
0.598400839016713));
#128152=CARTESIAN_POINT('Ctrl Pts',(-7.24771725000001,3.913265985,-0.181919376));
#128153=CARTESIAN_POINT('Ctrl Pts',(-7.257584542,3.978309763,0.211196195));
#128154=CARTESIAN_POINT('Ctrl Pts',(-7.224873927,4.043585554,0.603072745000001));
#128155=CARTESIAN_POINT('Ctrl Pts',(-7.499777297,3.913265985,0.05779697));
#128156=CARTESIAN_POINT('Ctrl Pts',(-7.496642395,3.978309763,0.464584256));
#128157=CARTESIAN_POINT('Ctrl Pts',(-7.44952710999999,4.043585554,0.868645977));
#128158=CARTESIAN_POINT('Origin',(0.199004244133321,4.0178569914715,-0.0123372337777652));
#128159=CARTESIAN_POINT('Ctrl Pts',(-7.184341147,4.043593265,-0.97352056));
#128160=CARTESIAN_POINT('Ctrl Pts',(-7.237738938,3.977881214,-0.579458064));
#128161=CARTESIAN_POINT('Ctrl Pts',(-7.24771725,3.913265985,-0.181919376));
#128162=CARTESIAN_POINT('Ctrl Pts',(-7.24806258821313,3.91102972422533,
-0.168161006833082));
#128163=CARTESIAN_POINT('Ctrl Pts',(-7.24840792642623,3.90879346345072,
-0.154402637666171));
#128164=CARTESIAN_POINT('Ctrl Pts',(-7.39549368163611,4.043593265,-1.25086767559276));
#128165=CARTESIAN_POINT('Ctrl Pts',(-7.46410401451045,3.977881214,-0.845223421831474));
#128166=CARTESIAN_POINT('Ctrl Pts',(-7.48793689720315,3.913265985,-0.434508640665116));
#128167=CARTESIAN_POINT('Ctrl Pts',(-7.48876172660541,3.91102972422533,
-0.420294261657062));
#128168=CARTESIAN_POINT('Ctrl Pts',(-7.48958655600768,3.90879346345073,
-0.406079882649009));
#128169=CARTESIAN_POINT('',(-7.18497825053082,4.04280735945212,-0.968807270126785));
#128170=CARTESIAN_POINT('Origin',(0.18750158142266,4.16060424972495,0.0450047815784264));
#128171=CARTESIAN_POINT('Ctrl Pts',(-7.43284403029268,4.00345494162532,
-1.00141380765489));
#128172=CARTESIAN_POINT('Ctrl Pts',(-7.39148755465654,4.00969641607202,
-0.996010122351671));
#128173=CARTESIAN_POINT('Ctrl Pts',(-7.35013240261112,4.0160913493177,-0.990589319895412));
#128174=CARTESIAN_POINT('Ctrl Pts',(-7.26752408918023,4.02919780802441,
-0.979723387895262));
#128175=CARTESIAN_POINT('Ctrl Pts',(-7.22622301479033,4.03591692850297,
-0.974271958496376));
#128176=CARTESIAN_POINT('Ctrl Pts',(-7.18497825071308,4.04280735926566,
-0.968807274322354));
#128177=CARTESIAN_POINT('Ctrl Pts',(-7.03916236,3.913265985,-1.73571117));
#128178=CARTESIAN_POINT('Ctrl Pts',(-7.133307187,3.978309763,-1.353907599));
#128179=CARTESIAN_POINT('Ctrl Pts',(-7.185603203,4.043585554,-0.964161089));
#128180=CARTESIAN_POINT('Ctrl Pts',(-7.336861312,3.913265985,-1.555784718));
#128181=CARTESIAN_POINT('Ctrl Pts',(-7.421246943,3.978309763,-1.157833981));
#128182=CARTESIAN_POINT('Ctrl Pts',(-7.462094514,4.043585554,-0.753090606));
#128183=CARTESIAN_POINT('Origin',(0.197003933960296,4.01785696054259,0.0307312683205818));
#128184=CARTESIAN_POINT('Ctrl Pts',(-6.8070971,4.043593265,-2.495181169));
#128185=CARTESIAN_POINT('Ctrl Pts',(-6.943958268,3.977881214,-2.121810582));
#128186=CARTESIAN_POINT('Ctrl Pts',(-7.03916236,3.913265985,-1.73571117));
#128187=CARTESIAN_POINT('Ctrl Pts',(-7.04245726710452,3.91102972421939,
-1.72234870134003));
#128188=CARTESIAN_POINT('Ctrl Pts',(-7.04575217420907,3.9087934634388,-1.70898623267999));
#128189=CARTESIAN_POINT('Ctrl Pts',(-6.95369157447094,4.043593265,-2.81143561710356));
#128190=CARTESIAN_POINT('Ctrl Pts',(-7.10789935959764,3.977881214,-2.43002429438841));
#128191=CARTESIAN_POINT('Ctrl Pts',(-7.21946658014773,3.913265985,-2.0340351607318));
#128192=CARTESIAN_POINT('Ctrl Pts',(-7.22332779682342,3.91102972421939,
-2.02033041987044));
#128193=CARTESIAN_POINT('Ctrl Pts',(-7.22718901349899,3.9087934634388,-2.00662567900909));
#128194=CARTESIAN_POINT('',(-6.80873252631852,4.0428073594254,-2.49071503209414));
#128195=CARTESIAN_POINT('Origin',(0.173442981650553,4.16060425035759,0.0842598250759541));
#128196=CARTESIAN_POINT('Ctrl Pts',(-7.04379390051592,4.00345494159632,
-2.57584306268899));
#128197=CARTESIAN_POINT('Ctrl Pts',(-7.00456594895749,4.00969641603317,
-2.56167529283629));
#128198=CARTESIAN_POINT('Ctrl Pts',(-6.9653429695701,4.0160913492954,-2.5474910904707));
#128199=CARTESIAN_POINT('Ctrl Pts',(-6.88700185498726,4.02919780663038,
-2.51912085535247));
#128200=CARTESIAN_POINT('Ctrl Pts',(-6.84783826859157,4.0359169278048,-2.50491836557248));
#128201=CARTESIAN_POINT('Ctrl Pts',(-6.80873252610599,4.04280735920979,
-2.49071503615566));
#128202=CARTESIAN_POINT('Ctrl Pts',(-6.501464062,3.913265985,-3.208343039));
#128203=CARTESIAN_POINT('Ctrl Pts',(-6.675484317,3.978309763,-2.855704178));
#128204=CARTESIAN_POINT('Ctrl Pts',(-6.81034166,4.043585554,-2.486311822));
#128205=CARTESIAN_POINT('Ctrl Pts',(-6.830881846,3.913265985,-3.096619642));
#128206=CARTESIAN_POINT('Ctrl Pts',(-6.998842233,3.978309763,-2.726113188));
#128207=CARTESIAN_POINT('Ctrl Pts',(-7.125742672,4.043585554,-2.339613509));
#128208=CARTESIAN_POINT('Origin',(0.185791769945699,4.01785695583774,0.0723628059211712));
#128209=CARTESIAN_POINT('Ctrl Pts',(-6.111560759,4.043593265,-3.90016988));
#128210=CARTESIAN_POINT('Ctrl Pts',(-6.325485828,3.977881214,-3.564949595));
#128211=CARTESIAN_POINT('Ctrl Pts',(-6.501464062,3.913265985,-3.208343039));
#128212=CARTESIAN_POINT('Ctrl Pts',(-6.50755447170544,3.91102972424845,
-3.19600128524829));
#128213=CARTESIAN_POINT('Ctrl Pts',(-6.51364488141098,3.90879346349691,
-3.18365953149656));
#128214=CARTESIAN_POINT('Ctrl Pts',(-6.18674257775371,4.043593265,-4.24054395383126));
#128215=CARTESIAN_POINT('Ctrl Pts',(-6.41933723072147,3.977881214,-3.90119993089582));
#128216=CARTESIAN_POINT('Ctrl Pts',(-6.61342203006904,3.913265985,-3.53845245862718));
#128217=CARTESIAN_POINT('Ctrl Pts',(-6.62013908773441,3.91102972424845,
-3.52589817463696));
#128218=CARTESIAN_POINT('Ctrl Pts',(-6.62685614539979,3.90879346349691,
-3.51334389064676));
#128219=CARTESIAN_POINT('',(-6.11411803676986,4.04280735945579,-3.89615972702897));
#128220=CARTESIAN_POINT('Origin',(0.15127470020613,4.16060424379175,0.119575041319216));
#128221=CARTESIAN_POINT('Ctrl Pts',(-6.3253837967532,4.00345494159254,-4.02982875897273));
#128222=CARTESIAN_POINT('Ctrl Pts',(-6.29011862453826,4.00969641604317,
-4.00755937353869));
#128223=CARTESIAN_POINT('Ctrl Pts',(-6.2548618407542,4.01609134932245,-3.98527500864474));
#128224=CARTESIAN_POINT('Ctrl Pts',(-6.18445104407342,4.02919780960704,
-3.94072701982691));
#128225=CARTESIAN_POINT('Ctrl Pts',(-6.149256204571,4.03591692928036,-3.91843756826656));
#128226=CARTESIAN_POINT('Ctrl Pts',(-6.11411803576209,4.04280735930486,
-3.89615973061763));
#128227=CARTESIAN_POINT('Ctrl Pts',(-5.65976453,3.913265985,-4.530956353));
#128228=CARTESIAN_POINT('Ctrl Pts',(-5.905523219,3.978309763,-4.223971203));
#128229=CARTESIAN_POINT('Ctrl Pts',(-6.116636109,4.043585554,-3.892205378));
#128230=CARTESIAN_POINT('Ctrl Pts',(-6.005497937,3.913265985,-4.492660073));
#128231=CARTESIAN_POINT('Ctrl Pts',(-6.249179439,3.978309763,-4.166922373));
#128232=CARTESIAN_POINT('Ctrl Pts',(-6.456199023,4.043585554,-3.816738684));
#128233=CARTESIAN_POINT('Origin',(0.165892242201615,4.01785698412803,0.110610760434389));
#128234=CARTESIAN_POINT('Ctrl Pts',(-5.130254628,4.043593265,-5.122790982));
#128235=CARTESIAN_POINT('Ctrl Pts',(-5.411240701,3.977881214,-4.841395528));
#128236=CARTESIAN_POINT('Ctrl Pts',(-5.65976453,3.913265985,-4.530956353));
#128237=CARTESIAN_POINT('Ctrl Pts',(-5.66836566160238,3.91102972423425,
-4.52021240056111));
#128238=CARTESIAN_POINT('Ctrl Pts',(-5.67696679320477,3.90879346346851,
-4.50946844812222));
#128239=CARTESIAN_POINT('Ctrl Pts',(-5.13050837364047,4.043593265,-5.4713691678521));
#128240=CARTESIAN_POINT('Ctrl Pts',(-5.4306140264266,3.977881214,-5.18995979468907));
#128241=CARTESIAN_POINT('Ctrl Pts',(-5.69814121471092,3.913265985,-4.87741565142092));
#128242=CARTESIAN_POINT('Ctrl Pts',(-5.70740003131173,3.91102972423425,
-4.8665988483859));
#128243=CARTESIAN_POINT('Ctrl Pts',(-5.71665884791265,3.90879346346851,
-4.85578204535089));
#128244=CARTESIAN_POINT('',(-5.13361418334659,4.04280735946019,-5.11942432351775));
#128245=CARTESIAN_POINT('Origin',(0.122032764432595,4.16060423114288,0.149298916294309));
#128246=CARTESIAN_POINT('Ctrl Pts',(-5.31120577594162,4.00345494159354,
-5.29538414122324));
#128247=CARTESIAN_POINT('Ctrl Pts',(-5.2815523434773,4.00969641605275,-5.26605443207314));
#128248=CARTESIAN_POINT('Ctrl Pts',(-5.25191032365656,4.01609134929042,
-5.23671189715124));
#128249=CARTESIAN_POINT('Ctrl Pts',(-5.19272219896807,4.02919780824411,
-5.17806918153805));
#128250=CARTESIAN_POINT('Ctrl Pts',(-5.16314176519752,4.03591692858593,
-5.14873499164139));
#128251=CARTESIAN_POINT('Ctrl Pts',(-5.13361418103969,4.04280735921221,
-5.1194243271406));
#128252=CARTESIAN_POINT('Ctrl Pts',(-4.553420698,3.913265985,-5.641707183));
#128253=CARTESIAN_POINT('Ctrl Pts',(-4.85942641899999,3.978309763,-5.39473003));
#128254=CARTESIAN_POINT('Ctrl Pts',(-5.136923453,4.043585554,-5.116103736));
#128255=CARTESIAN_POINT('Ctrl Pts',(-4.899303619,3.913265985,-5.678628712));
#128256=CARTESIAN_POINT('Ctrl Pts',(-5.20731196000001,3.978309763,-5.412890898));
#128257=CARTESIAN_POINT('Ctrl Pts',(-5.484770682,4.043585554,-5.115397401));
#128258=CARTESIAN_POINT('Origin',(0.138235559680123,4.01785695374291,0.143686509914068));
#128259=CARTESIAN_POINT('Ctrl Pts',(-3.909063493,4.043593265,-6.105876072));
#128260=CARTESIAN_POINT('Ctrl Pts',(-4.243971972,3.977881214,-5.891463186));
#128261=CARTESIAN_POINT('Ctrl Pts',(-4.553420698,3.913265985,-5.64170718300001));
#128262=CARTESIAN_POINT('Ctrl Pts',(-4.56413037193816,3.91102972426959,
-5.63306340737098));
#128263=CARTESIAN_POINT('Ctrl Pts',(-4.57484004587628,3.90879346353919,
-5.62441963174208));
#128264=CARTESIAN_POINT('Ctrl Pts',(-3.8343773006698,4.043593265,-6.44635924039629));
#128265=CARTESIAN_POINT('Ctrl Pts',(-4.18796134717372,3.977881214,-6.23604290637241));
#128266=CARTESIAN_POINT('Ctrl Pts',(-4.51642165067599,3.913265985,-5.98831630932453));
#128267=CARTESIAN_POINT('Ctrl Pts',(-4.52778929402551,3.91102972426959,
-5.97974276916334));
#128268=CARTESIAN_POINT('Ctrl Pts',(-4.539156937375,3.9087934635392,-5.97116922900215));
#128269=CARTESIAN_POINT('',(-3.91306823576687,4.04280735944647,-6.10331032894653));
#128270=CARTESIAN_POINT('Origin',(0.0870848940551211,4.16060424395647,0.172041892549754));
#128271=CARTESIAN_POINT('Ctrl Pts',(-4.04868167678957,4.00345494162143,
-6.31333324611067));
#128272=CARTESIAN_POINT('Ctrl Pts',(-4.02602654552544,4.00969641605222,
-6.27831463799619));
#128273=CARTESIAN_POINT('Ctrl Pts',(-4.00338531713494,4.01609134929976,
-6.24328595714909));
#128274=CARTESIAN_POINT('Ctrl Pts',(-3.95818743098564,4.02919780741784,
-6.17329058298552));
#128275=CARTESIAN_POINT('Ctrl Pts',(-3.93560455346319,4.03591692817666,
-6.13828328903173));
#128276=CARTESIAN_POINT('Ctrl Pts',(-3.91306823295186,4.04280735919888,
-6.10331033194858));
#128277=CARTESIAN_POINT('Ctrl Pts',(-3.234163976,3.913265985,-6.488658057));
#128278=CARTESIAN_POINT('Ctrl Pts',(-3.58610824,3.978309763,-6.31323727599999));
#128279=CARTESIAN_POINT('Ctrl Pts',(-3.917013965,4.043585554,-6.10077877));
#128280=CARTESIAN_POINT('Ctrl Pts',(-3.564023309,3.913265985,-6.599070984));
#128281=CARTESIAN_POINT('Ctrl Pts',(-3.921956361,3.978309763,-6.40575866100001));
#128282=CARTESIAN_POINT('Ctrl Pts',(-4.25688056,4.043585554,-6.17486582));
#128283=CARTESIAN_POINT('Origin',(0.104115509673351,4.01785695580956,0.170044049114778));
#128284=CARTESIAN_POINT('Ctrl Pts',(-2.505088894,4.043593265,-6.803457182));
#128285=CARTESIAN_POINT('Ctrl Pts',(-2.878259831,3.977881214,-6.666052574));
#128286=CARTESIAN_POINT('Ctrl Pts',(-3.234163976,3.913265985,-6.488658057));
#128287=CARTESIAN_POINT('Ctrl Pts',(-3.24648142007391,3.91102972425195,
-6.4825186313348));
#128288=CARTESIAN_POINT('Ctrl Pts',(-3.25879886414786,3.90879346350392,
-6.47637920566949));
#128289=CARTESIAN_POINT('Ctrl Pts',(-2.35895500654199,4.043593265,-7.11992472055484));
#128290=CARTESIAN_POINT('Ctrl Pts',(-2.74948424915754,3.977881214,-6.99053558333539));
#128291=CARTESIAN_POINT('Ctrl Pts',(-3.12351922935454,3.913265985,-6.81920995168694));
#128292=CARTESIAN_POINT('Ctrl Pts',(-3.1364641613397,3.91102972425195,-6.8132805633505));
#128293=CARTESIAN_POINT('Ctrl Pts',(-3.14940909332493,3.90879346350392,
-6.80735117501388));
#128294=CARTESIAN_POINT('',(-2.50955156673443,4.04280735945939,-6.80181232628126));
#128295=CARTESIAN_POINT('Origin',(0.0480650262536675,4.16060428568896,0.186740464814262));
#128296=CARTESIAN_POINT('Ctrl Pts',(-2.59684572190937,4.00345494161758,
-7.03607790590514));
#128297=CARTESIAN_POINT('Ctrl Pts',(-2.58224822063566,4.00969641605882,
-6.99700782975648));
#128298=CARTESIAN_POINT('Ctrl Pts',(-2.56766646253128,4.01609134931304,
-6.95793090509845));
#128299=CARTESIAN_POINT('Ctrl Pts',(-2.53857221501533,4.02919780708633,
-6.87985577640105));
#128300=CARTESIAN_POINT('Ctrl Pts',(-2.52404284554597,4.03591692804071,
-6.84081228116046));
#128301=CARTESIAN_POINT('Ctrl Pts',(-2.50955156324783,4.04280735924479,
-6.80181232858497));
#128302=CARTESIAN_POINT('Ctrl Pts',(-1.763681341,3.913265985,-7.032206491));
#128303=CARTESIAN_POINT('Ctrl Pts',(-2.145107626,3.978309763,-6.936544564));
#128304=CARTESIAN_POINT('Ctrl Pts',(-2.513949257,4.043585554,-6.800188169));
#128305=CARTESIAN_POINT('Ctrl Pts',(-2.06209323,3.913265985,-7.21094803100001));
#128306=CARTESIAN_POINT('Ctrl Pts',(-2.453214441,3.978309763,-7.099100269));
#128307=CARTESIAN_POINT('Ctrl Pts',(-2.829943435,4.043585554,-6.945604377));
#128308=CARTESIAN_POINT('Origin',(0.0651268731426771,4.01785696157778,0.18845016650496));
#128309=CARTESIAN_POINT('Ctrl Pts',(-0.983979122,4.043593265,-7.182916197));
#128310=CARTESIAN_POINT('Ctrl Pts',(-1.37796346,3.977881214,-7.128944752));
#128311=CARTESIAN_POINT('Ctrl Pts',(-1.763681341,3.913265985,-7.032206491));
#128312=CARTESIAN_POINT('Ctrl Pts',(-1.77703060513271,3.91102972424724,
-7.0288584880646));
#128313=CARTESIAN_POINT('Ctrl Pts',(-1.79037986926543,3.90879346349449,
-7.02551048512909));
#128314=CARTESIAN_POINT('Ctrl Pts',(-0.773230597839176,4.043593265,-7.46057043305692));
#128315=CARTESIAN_POINT('Ctrl Pts',(-1.18244432400907,3.977881214,-7.41815858538808));
#128316=CARTESIAN_POINT('Ctrl Pts',(-1.58456451966031,3.913265985,-7.3312449165871));
#128317=CARTESIAN_POINT('Ctrl Pts',(-1.59848144954423,3.91102972424724,
-7.32823693179117));
#128318=CARTESIAN_POINT('Ctrl Pts',(-1.61239837942815,3.90879346349449,
-7.32522894699524));
#128319=CARTESIAN_POINT('',(-0.988691055522213,4.04280735945093,-7.18226913894742));
#128320=CARTESIAN_POINT('Origin',(0.00679763605742609,4.16060425918084,
0.19270726971797));
#128321=CARTESIAN_POINT('Ctrl Pts',(-1.02358414735161,4.00345494160357,
-7.42982338229497));
#128322=CARTESIAN_POINT('Ctrl Pts',(-1.01772683905242,4.00969641604632,
-7.38852871155796));
#128323=CARTESIAN_POINT('Ctrl Pts',(-1.01188637805703,4.01609134930418,
-7.3472307367515));
#128324=CARTESIAN_POINT('Ctrl Pts',(-1.00025618222515,4.02919780756502,
-7.26472655507422));
#128325=CARTESIAN_POINT('Ctrl Pts',(-0.994459698903276,4.03591692827595,
-7.22347249182076));
#128326=CARTESIAN_POINT('Ctrl Pts',(-0.988691051854008,4.04280735925939,
-7.18226914059731));
#128327=CARTESIAN_POINT('Ctrl Pts',(-0.210730926,3.913265985,-7.246936765));
#128328=CARTESIAN_POINT('Ctrl Pts',(-0.603804163,3.978309763,-7.235506737));
#128329=CARTESIAN_POINT('Ctrl Pts',(-0.993335076,4.043585554,-7.181628327));
#128330=CARTESIAN_POINT('Ctrl Pts',(-0.463741963,3.913265985,-7.485649163));
#128331=CARTESIAN_POINT('Ctrl Pts',(-0.869762941,3.978309763,-7.460495838));
#128332=CARTESIAN_POINT('Ctrl Pts',(-1.2706813,4.043585554,-7.391574192));
#128333=CARTESIAN_POINT('Origin',(0.0230930328050315,4.01785696223938,0.198044760085584));
#128334=CARTESIAN_POINT('Ctrl Pts',(0.583140419,4.043593265,-7.226510033));
#128335=CARTESIAN_POINT('Ctrl Pts',(0.186764952,3.977881214,-7.258495397));
#128336=CARTESIAN_POINT('Ctrl Pts',(-0.210730926,3.913265985,-7.246936765));
#128337=CARTESIAN_POINT('Ctrl Pts',(-0.224487813524214,3.91102972423126,
-7.24653673368102));
#128338=CARTESIAN_POINT('Ctrl Pts',(-0.238244701048428,3.90879346346254,
-7.24613670236216));
#128339=CARTESIAN_POINT('Ctrl Pts',(0.848649214287638,4.043593265,-7.45236816437252));
#128340=CARTESIAN_POINT('Ctrl Pts',(0.439885384551184,3.977881214,-7.49891673678223));
#128341=CARTESIAN_POINT('Ctrl Pts',(0.0284826653429041,3.913265985,-7.5004790163336));
#128342=CARTESIAN_POINT('Ctrl Pts',(0.0142444776067684,3.91102972423126,
-7.50053308508062));
#128343=CARTESIAN_POINT('Ctrl Pts',(6.28987063271302E-6,3.90879346346255,
-7.50058715382766));
#128344=CARTESIAN_POINT('',(0.578399550099043,4.04280735946618,-7.22689102929937));
#128345=CARTESIAN_POINT('Origin',(-0.034787638241215,4.16060423561476,0.189663017005176));
#128346=CARTESIAN_POINT('Ctrl Pts',(0.597539084743176,4.00345494159598,
-7.47615857517617));
#128347=CARTESIAN_POINT('Ctrl Pts',(0.594382318797106,4.00969641605215,
-7.43457020272798));
#128348=CARTESIAN_POINT('Ctrl Pts',(0.591208389122248,4.01609134932308,
-7.39298222514298));
#128349=CARTESIAN_POINT('Ctrl Pts',(0.584830715843343,4.02919780977328,
-7.30990678336319));
#128350=CARTESIAN_POINT('Ctrl Pts',(0.581623276858757,4.03591692937593,
-7.26837115206616));
#128351=CARTESIAN_POINT('Ctrl Pts',(0.578399553874348,4.04280735933351,
-7.22689102998411));
#128352=CARTESIAN_POINT('Ctrl Pts',(1.352073032,3.913265985,-7.122808331));
#128353=CARTESIAN_POINT('Ctrl Pts',(0.965732511,3.978309763,-7.19614465799999));
#128354=CARTESIAN_POINT('Ctrl Pts',(0.573726349,4.043585554,-7.227263526));
#128355=CARTESIAN_POINT('Ctrl Pts',(1.156293362,3.913265985,-7.410329659));
#128356=CARTESIAN_POINT('Ctrl Pts',(0.754357708,3.978309763,-7.473046914));
#128357=CARTESIAN_POINT('Ctrl Pts',(0.347996481,4.043585554,-7.491922213));
#128358=CARTESIAN_POINT('Origin',(-0.0200205943985987,4.01785696253182,
0.198378610296422));
#128359=CARTESIAN_POINT('Ctrl Pts',(2.122992963,4.043593265,-6.932200291));
#128360=CARTESIAN_POINT('Ctrl Pts',(1.742760442,3.977881214,-7.048646864));
#128361=CARTESIAN_POINT('Ctrl Pts',(1.352073032,3.913265985,-7.122808331));
#128362=CARTESIAN_POINT('Ctrl Pts',(1.33855177753404,3.91102972416506,-7.12537497645928));
#128363=CARTESIAN_POINT('Ctrl Pts',(1.32503052306806,3.90879346333014,-7.12794162191861));
#128364=CARTESIAN_POINT('Ctrl Pts',(2.43084713209943,4.043593265,-7.09570144285702));
#128365=CARTESIAN_POINT('Ctrl Pts',(2.04164654045871,3.977881214,-7.22903387662127));
#128366=CARTESIAN_POINT('Ctrl Pts',(1.64019803211851,3.913265985,-7.31899905409572));
#128367=CARTESIAN_POINT('Ctrl Pts',(1.62630434807006,3.91102972416506,-7.32211264830573));
#128368=CARTESIAN_POINT('Ctrl Pts',(1.6124106640216,3.90879346333014,-7.32522624251587));
#128369=CARTESIAN_POINT('',(2.11844483583129,4.04280735942594,-6.93359152700834));
#128370=CARTESIAN_POINT('Origin',(-0.0747462306194105,4.16060422367809,
0.177750342392968));
#128371=CARTESIAN_POINT('Ctrl Pts',(2.19072205301252,4.00345494162878,-7.17291690241065));
#128372=CARTESIAN_POINT('Ctrl Pts',(2.17869881975252,4.00969641607101,-7.13297945426373));
#128373=CARTESIAN_POINT('Ctrl Pts',(2.16665890893221,4.01609134932407,-7.09304608144558));
#128374=CARTESIAN_POINT('Ctrl Pts',(2.14257158065363,4.02919780818236,-7.01328391782595));
#128375=CARTESIAN_POINT('Ctrl Pts',(2.13051019526031,4.03591692859592,-6.97340886569841));
#128376=CARTESIAN_POINT('Ctrl Pts',(2.11844483965137,4.04280735930388,-6.93359152644189));
#128377=CARTESIAN_POINT('Ctrl Pts',(2.851655559,3.913265985,-6.665625295));
#128378=CARTESIAN_POINT('Ctrl Pts',(2.490112606,3.978309763,-6.820298851));
#128379=CARTESIAN_POINT('Ctrl Pts',(2.113960967,4.043585554,-6.934959915));
#128380=CARTESIAN_POINT('Ctrl Pts',(2.722261695,3.913265985,-6.988511377));
#128381=CARTESIAN_POINT('Ctrl Pts',(2.343205429,3.978309763,-7.136166621));
#128382=CARTESIAN_POINT('Ctrl Pts',(1.950402333,4.043585554,-7.241956279));
#128383=CARTESIAN_POINT('Origin',(-0.0621981411914818,4.01785698790786,
0.18943702702451));
#128384=CARTESIAN_POINT('Ctrl Pts',(3.563576716,4.043593265,-6.313748569));
#128385=CARTESIAN_POINT('Ctrl Pts',(3.21726639,3.977881214,-6.509211438));
#128386=CARTESIAN_POINT('Ctrl Pts',(2.851655559,3.913265985,-6.665625295));
#128387=CARTESIAN_POINT('Ctrl Pts',(2.83900217674919,3.91102972413889,-6.67103860378116));
#128388=CARTESIAN_POINT('Ctrl Pts',(2.82634879449839,3.90879346327781,-6.67645191256244));
#128389=CARTESIAN_POINT('Ctrl Pts',(3.89938133908574,4.043593265,-6.40724760846984));
#128390=CARTESIAN_POINT('Ctrl Pts',(3.5479425741295,3.977881214,-6.6211294263161));
#128391=CARTESIAN_POINT('Ctrl Pts',(3.1752195618941,3.913265985,-6.79529083046101));
#128392=CARTESIAN_POINT('Ctrl Pts',(3.16232003499938,3.91102972413889,-6.80131836201407));
#128393=CARTESIAN_POINT('Ctrl Pts',(3.14942050810468,3.9087934632778,-6.80734589356702));
#128394=CARTESIAN_POINT('',(3.55943399567121,4.04280735940916,-6.31608499157434));
#128395=CARTESIAN_POINT('Origin',(-0.111209903497371,4.16060421018104,0.1575266722846));
#128396=CARTESIAN_POINT('Ctrl Pts',(3.68146929256206,4.00345494161536,-6.53427760732435));
#128397=CARTESIAN_POINT('Ctrl Pts',(3.66114178509397,4.00969641604704,-6.4978585143677));
#128398=CARTESIAN_POINT('Ctrl Pts',(3.64079886599986,4.01609134930843,-6.46144698653662));
#128399=CARTESIAN_POINT('Ctrl Pts',(3.60012817905465,4.02919780807987,-6.3887276820716));
#128400=CARTESIAN_POINT('Ctrl Pts',(3.57977682462897,4.03591692852018,-6.35237772768086));
#128401=CARTESIAN_POINT('Ctrl Pts',(3.55943399940581,4.04280735924911,-6.31608499035852));
#128402=CARTESIAN_POINT('Ctrl Pts',(4.21789784,3.913265985,-5.896765029));
#128403=CARTESIAN_POINT('Ctrl Pts',(3.898057804,3.978309763,-6.125543451));
#128404=CARTESIAN_POINT('Ctrl Pts',(3.55534912,4.043585554,-6.318385287));
#128405=CARTESIAN_POINT('Ctrl Pts',(4.160940096,3.913265985,-6.23991807));
#128406=CARTESIAN_POINT('Ctrl Pts',(3.822487468,3.978309763,-6.465607109));
#128407=CARTESIAN_POINT('Ctrl Pts',(3.461609539,4.043585554,-6.653364517));
#128408=CARTESIAN_POINT('Origin',(-0.101467299579598,4.01785693399817,0.17163723126743));
#128409=CARTESIAN_POINT('Ctrl Pts',(4.837531582,4.043593265,-5.400072981));
#128410=CARTESIAN_POINT('Ctrl Pts',(4.541336538,3.977881214,-5.66541252));
#128411=CARTESIAN_POINT('Ctrl Pts',(4.21789784,3.913265985,-5.896765029));
#128412=CARTESIAN_POINT('Ctrl Pts',(4.20670398840656,3.91102972419208,-5.90477188058432));
#128413=CARTESIAN_POINT('Ctrl Pts',(4.19551013681311,3.90879346338417,-5.91277873216877));
#128414=CARTESIAN_POINT('Ctrl Pts',(5.18558480998941,4.043593265,-5.41919799617495));
#128415=CARTESIAN_POINT('Ctrl Pts',(4.8883407551324,3.977881214,-5.703628322637));
#128416=CARTESIAN_POINT('Ctrl Pts',(4.56177135477598,3.913265985,-5.95384235976156));
#128417=CARTESIAN_POINT('Ctrl Pts',(4.55046915307545,3.91102972419208,-5.96250198773891));
#128418=CARTESIAN_POINT('Ctrl Pts',(4.53916695137504,3.90879346338417,-5.9711616157164));
#128419=CARTESIAN_POINT('',(4.83398797799277,4.04280735943435,-5.40324534134335));
#128420=CARTESIAN_POINT('Origin',(-0.142473359438421,4.16060420788965,0.129936838326903));
#128421=CARTESIAN_POINT('Ctrl Pts',(5.00007512009465,4.0034549415684,-5.5901027533489));
#128422=CARTESIAN_POINT('Ctrl Pts',(4.97239382994866,4.00969641603501,-5.55890493168669));
#128423=CARTESIAN_POINT('Ctrl Pts',(4.9446991148708,4.01609134930492,-5.52771781147437));
#128424=CARTESIAN_POINT('Ctrl Pts',(4.88934677262722,4.02919781104827,-5.46544162554518));
#128425=CARTESIAN_POINT('Ctrl Pts',(4.8616570626464,4.03591692995295,-5.43431646029451));
#128426=CARTESIAN_POINT('Ctrl Pts',(4.83398798131907,4.0428073592582,-5.40324533969528));
#128427=CARTESIAN_POINT('Ctrl Pts',(5.386915907,3.913265985,-4.852178584));
#128428=CARTESIAN_POINT('Ctrl Pts',(5.123734151,3.978309763,-5.14436444699999));
#128429=CARTESIAN_POINT('Ctrl Pts',(4.8304931,4.043585554,-5.406369984));
#128430=CARTESIAN_POINT('Ctrl Pts',(5.405057563,3.913265985,-5.199553129));
#128431=CARTESIAN_POINT('Ctrl Pts',(5.123034241,3.978309763,-5.492722994));
#128432=CARTESIAN_POINT('Ctrl Pts',(4.810955731,4.043585554,-5.753668826));
#128433=CARTESIAN_POINT('Origin',(-0.135991943969817,4.01785695574899,0.145811955776194));
#128434=CARTESIAN_POINT('Ctrl Pts',(5.885288847,4.043593265,-4.233895981));
#128435=CARTESIAN_POINT('Ctrl Pts',(5.65305883699999,3.977881214,-4.556705209));
#128436=CARTESIAN_POINT('Ctrl Pts',(5.386915907,3.913265985,-4.852178584));
#128437=CARTESIAN_POINT('Ctrl Pts',(5.37770499780094,3.91102972417881,-4.8624045871024));
#128438=CARTESIAN_POINT('Ctrl Pts',(5.36849408860187,3.90879346335763,-4.87263059020483));
#128439=CARTESIAN_POINT('Ctrl Pts',(6.22931609688157,4.043593265,-4.177752709251));
#128440=CARTESIAN_POINT('Ctrl Pts',(6.00016555589542,3.977881214,-4.51943189804367));
#128441=CARTESIAN_POINT('Ctrl Pts',(5.73501978812069,3.913265985,-4.83399883832596));
#128442=CARTESIAN_POINT('Ctrl Pts',(5.72584338959121,3.91102972417881,-4.84488564837186));
#128443=CARTESIAN_POINT('Ctrl Pts',(5.71666699106165,3.90879346335762,-4.8557724584176));
#128444=CARTESIAN_POINT('',(5.88251005481746,4.04280735943236,-4.23775594359663));
#128445=CARTESIAN_POINT('Origin',(-0.1670748624342,4.16060423972647,0.0962713050176661));
#128446=CARTESIAN_POINT('Ctrl Pts',(6.08488299206126,4.00345494165232,-4.38454090746794));
#128447=CARTESIAN_POINT('Ctrl Pts',(6.05114226559023,4.00969641611188,-4.36002313261344));
#128448=CARTESIAN_POINT('Ctrl Pts',(6.0173907288278,4.01609134931989,-4.33551869516663));
#128449=CARTESIAN_POINT('Ctrl Pts',(5.94994497316006,4.02919780739118,-4.28659762264593));
#128450=CARTESIAN_POINT('Ctrl Pts',(5.91621163238369,4.03591692819812,-4.26215260797922));
#128451=CARTESIAN_POINT('Ctrl Pts',(5.88251005761056,4.04280735926177,-4.2377559410218));
#128452=CARTESIAN_POINT('Ctrl Pts',(6.304047773,3.913265985,-3.580709661));
#128453=CARTESIAN_POINT('Ctrl Pts',(6.109830384,3.978309763,-3.922640679));
#128454=CARTESIAN_POINT('Ctrl Pts',(5.879768591,4.043585554,-4.24155883));
#128455=CARTESIAN_POINT('Ctrl Pts',(6.396440546,3.913265985,-3.916062862));
#128456=CARTESIAN_POINT('Ctrl Pts',(6.184033628,3.978309763,-4.263005256));
#128457=CARTESIAN_POINT('Ctrl Pts',(5.93534698,4.043585554,-4.584937975));
#128458=CARTESIAN_POINT('Origin',(-0.164157702665602,4.01785694770381,0.113168649877501));
#128459=CARTESIAN_POINT('Ctrl Pts',(6.657856548,4.043593265,-2.869746712));
#128460=CARTESIAN_POINT('Ctrl Pts',(6.500450388,3.977881214,-3.234931426));
#128461=CARTESIAN_POINT('Ctrl Pts',(6.304047773,3.913265985,-3.580709661));
#128462=CARTESIAN_POINT('Ctrl Pts',(6.297250498457,3.91102972429048,-3.59267665845715));
#128463=CARTESIAN_POINT('Ctrl Pts',(6.29045322391415,3.90879346358098,-3.60464365591426));
#128464=CARTESIAN_POINT('Ctrl Pts',(6.98177148812167,4.043593265,-2.74096034957502));
#128465=CARTESIAN_POINT('Ctrl Pts',(6.83142928431638,3.977881214,-3.12391186004807));
#128466=CARTESIAN_POINT('Ctrl Pts',(6.64010507143617,3.913265985,-3.48812290292875));
#128467=CARTESIAN_POINT('Ctrl Pts',(6.63348355470297,3.91102972429048,-3.50072783922272));
#128468=CARTESIAN_POINT('Ctrl Pts',(6.62686203796978,3.90879346358098,-3.5133327755167));
#128469=CARTESIAN_POINT('',(6.65597249944044,4.04280735944133,-2.87411378903347));
#128470=CARTESIAN_POINT('Origin',(-0.18386436534236,4.16060427247911,0.0581044355760535));
#128471=CARTESIAN_POINT('Ctrl Pts',(6.88516849829515,4.0034549415845,-2.97396280252883));
#128472=CARTESIAN_POINT('Ctrl Pts',(6.84694601453568,4.00969641602047,-2.95727149861208));
#128473=CARTESIAN_POINT('Ctrl Pts',(6.80871583992959,4.01609134928458,-2.94059554396096));
#128474=CARTESIAN_POINT('Ctrl Pts',(6.73233034632253,4.02919780699493,-2.90731706378765));
#128475=CARTESIAN_POINT('Ctrl Pts',(6.69413071574023,4.03591692798957,-2.89069523065496));
#128476=CARTESIAN_POINT('Ctrl Pts',(6.65597250201484,4.042807359239,-2.87411378614891));
#128477=CARTESIAN_POINT('Ctrl Pts',(6.92640937100001,3.913265985,-2.141810735));
#128478=CARTESIAN_POINT('Ctrl Pts',(6.810237738,3.978309763,-2.517498593));
#128479=CARTESIAN_POINT('Ctrl Pts',(6.654112638,4.043585554,-2.8784171));
#128480=CARTESIAN_POINT('Ctrl Pts',(7.088733078,3.913265985,-2.449461849));
#128481=CARTESIAN_POINT('Ctrl Pts',(6.955874475,3.978309763,-2.833954131));
#128482=CARTESIAN_POINT('Ctrl Pts',(6.782208,4.043585554,-3.20182052));
#128483=CARTESIAN_POINT('Origin',(-0.184647872090897,4.01785694219713,0.0752338312692788));
#128484=CARTESIAN_POINT('Ctrl Pts',(7.119110275,4.043593265,-1.371411276));
#128485=CARTESIAN_POINT('Ctrl Pts',(7.043888103,3.977881214,-1.761895846));
#128486=CARTESIAN_POINT('Ctrl Pts',(6.926409371,3.913265985,-2.141810735));
#128487=CARTESIAN_POINT('Ctrl Pts',(6.92234356355036,3.91102972423215,-2.15495916416351));
#128488=CARTESIAN_POINT('Ctrl Pts',(6.91827775610086,3.90879346346433,-2.16810759332702));
#128489=CARTESIAN_POINT('Ctrl Pts',(7.40776700316154,4.043593265,-1.1760037288039));
#128490=CARTESIAN_POINT('Ctrl Pts',(7.3432629714967,3.977881214,-1.58232117638743));
#128491=CARTESIAN_POINT('Ctrl Pts',(7.23470641998915,3.913265985,-1.9791462180463));
#128492=CARTESIAN_POINT('Ctrl Pts',(7.23094939922197,3.91102972423215,-1.99287988866998));
#128493=CARTESIAN_POINT('Ctrl Pts',(7.22719237845479,3.90879346346432,-2.00661355929366));
#128494=CARTESIAN_POINT('',(7.11820906756662,4.0428073594531,-1.37608126740113));
#128495=CARTESIAN_POINT('Origin',(-0.192056303862034,4.16060420929109,0.0172205636934611));
#128496=CARTESIAN_POINT('Ctrl Pts',(7.36351117761108,4.00345494157173,-1.42432550160411));
#128497=CARTESIAN_POINT('Ctrl Pts',(7.32259417719401,4.00969641604598,-1.4162411351845));
#128498=CARTESIAN_POINT('Ctrl Pts',(7.28167296572909,4.01609134929106,-1.40817341256506));
#128499=CARTESIAN_POINT('Ctrl Pts',(7.19991942750863,4.02919780789818,-1.39209358688646));
#128500=CARTESIAN_POINT('Ctrl Pts',(7.15903968301819,4.03591692847851,-1.384072154959));
#128501=CARTESIAN_POINT('Ctrl Pts',(7.11820906898563,4.04280735933872,-1.37608126395451));
#128502=CARTESIAN_POINT('Ctrl Pts',(7.224899766,3.913265985,-0.602763118));
#128503=CARTESIAN_POINT('Ctrl Pts',(7.192205945,3.978309763,-0.99464107));
#128504=CARTESIAN_POINT('Ctrl Pts',(7.117317773,4.043585554,-1.380683784));
#128505=CARTESIAN_POINT('Ctrl Pts',(7.44956433,3.913265985,-0.868326722));
#128506=CARTESIAN_POINT('Ctrl Pts',(7.402466362,3.978309763,-1.272390461));
#128507=CARTESIAN_POINT('Ctrl Pts',(7.311940513,4.043585554,-1.668989496));
#128508=CARTESIAN_POINT('Origin',(-0.196503946990214,4.0178569579,0.0337810818113829));
#128509=CARTESIAN_POINT('Ctrl Pts',(7.247482319,4.043593265,0.191049828));
#128510=CARTESIAN_POINT('Ctrl Pts',(7.257961439,3.977881214,-0.206475974));
#128511=CARTESIAN_POINT('Ctrl Pts',(7.224899766,3.913265985,-0.602763118));
#128512=CARTESIAN_POINT('Ctrl Pts',(7.22439618107746,3.91228178631499,-0.608799238153792));
#128513=CARTESIAN_POINT('Ctrl Pts',(7.22389259615494,3.91129758763,-0.614835358307581));
#128514=CARTESIAN_POINT('Ctrl Pts',(7.4871021457591,4.043593265,0.443644859291128));
#128515=CARTESIAN_POINT('Ctrl Pts',(7.51143615240166,3.977881214,0.0329758636738649));
#128516=CARTESIAN_POINT('Ctrl Pts',(7.49070876024168,3.913265985,-0.377890955083214));
#128517=CARTESIAN_POINT('Ctrl Pts',(7.49039304717491,3.91228178631499,-0.384149148221127));
#128518=CARTESIAN_POINT('Ctrl Pts',(7.49007733410815,3.91129758763,-0.390407341359038));
#128519=CARTESIAN_POINT('',(7.24760609127573,4.04280735946006,0.186295284467327));
#128520=CARTESIAN_POINT('Origin',(-0.191268234115439,4.1606042421385,-0.0244684761355934));
#128521=CARTESIAN_POINT('Ctrl Pts',(7.49754425842133,4.00345494160375,0.191911676403569));
#128522=CARTESIAN_POINT('Ctrl Pts',(7.45584597507905,4.00969641604305,0.191011089299511));
#128523=CARTESIAN_POINT('Ctrl Pts',(7.41414715678095,4.01609134929557,0.190093342264412));
#128524=CARTESIAN_POINT('Ctrl Pts',(7.33084828706427,4.0291978073406,0.188222636638881));
#128525=CARTESIAN_POINT('Ctrl Pts',(7.28919991587735,4.03591692815706,0.187268595286477));
#128526=CARTESIAN_POINT('Ctrl Pts',(7.247606092197,4.0428073592334,0.186295288614052));
#128527=CARTESIAN_POINT('Ctrl Pts',(7.185561877,3.913265985,0.964469032));
#128528=CARTESIAN_POINT('Ctrl Pts',(7.237874596,3.978309763,0.574724763));
#128529=CARTESIAN_POINT('Ctrl Pts',(7.24772504,4.043585554,0.18160877));
#128530=CARTESIAN_POINT('Ctrl Pts',(7.462062233,3.913265985,0.753410398));
#128531=CARTESIAN_POINT('Ctrl Pts',(7.50292714899999,3.978309763,0.348668774));
#128532=CARTESIAN_POINT('Ctrl Pts',(7.49977481399999,4.043585554,-0.058118378));
#128533=CARTESIAN_POINT('Origin',(-0.199171610314072,4.01785698284914,-0.00925123469850048));
#128534=CARTESIAN_POINT('Ctrl Pts',(7.036970144,4.043593265,1.744577653));
#128535=CARTESIAN_POINT('Ctrl Pts',(7.132660565,3.977881214,1.358598485));
#128536=CARTESIAN_POINT('Ctrl Pts',(7.185561877,3.913265985,0.964469032));
#128537=CARTESIAN_POINT('Ctrl Pts',(7.18739273225864,3.91102972417149,0.950828652313265));
#128538=CARTESIAN_POINT('Ctrl Pts',(7.18922358751719,3.90879346334299,0.937188272626531));
#128539=CARTESIAN_POINT('Ctrl Pts',(7.2168983954371,4.043593265,2.04312855315919));
#128540=CARTESIAN_POINT('Ctrl Pts',(7.32896439106459,3.977881214,1.64728028570918));
#128541=CARTESIAN_POINT('Ctrl Pts',(7.39706364334686,3.913265985,1.24154991981403));
#128542=CARTESIAN_POINT('Ctrl Pts',(7.39942048232563,3.91102972417149,1.22750804550314));
#128543=CARTESIAN_POINT('Ctrl Pts',(7.40177732130451,3.90879346334299,1.21346617119224));
#128544=CARTESIAN_POINT('',(7.03811310896934,4.04280735943817,1.73996087631982));
#128545=CARTESIAN_POINT('Origin',(-0.181536210942169,4.16060424174822,-0.065013380066494));
#128546=CARTESIAN_POINT('Ctrl Pts',(7.28100050240532,4.00345494164967,1.79917527769442));
#128547=CARTESIAN_POINT('Ctrl Pts',(7.24047070142337,4.00969641607446,1.78933184746784));
#128548=CARTESIAN_POINT('Ctrl Pts',(7.19994406678762,4.0160913493275,1.77947154348191));
#128549=CARTESIAN_POINT('Ctrl Pts',(7.11899482593457,4.02919780717941,1.75973777943903));
#128550=CARTESIAN_POINT('Ctrl Pts',(7.07852526065663,4.03591692808004,1.74985287418798));
#128551=CARTESIAN_POINT('Ctrl Pts',(7.03811310915023,4.04280735923492,1.73996088015336));
#128552=CARTESIAN_POINT('Ctrl Pts',(6.81023510100001,3.913265985,2.486603681));
#128553=CARTESIAN_POINT('Ctrl Pts',(6.945108274,3.978309763,2.117217106));
#128554=CARTESIAN_POINT('Ctrl Pts',(7.039236739,4.043585554,1.7354095));
#128555=CARTESIAN_POINT('Ctrl Pts',(7.12564240000001,3.913265985,2.339918885));
#128556=CARTESIAN_POINT('Ctrl Pts',(7.252559402,3.978309763,1.953424644));
#128557=CARTESIAN_POINT('Ctrl Pts',(7.336927979,4.043585554,1.555470291));
#128558=CARTESIAN_POINT('Origin',(-0.192526489986816,4.01785691537832,-0.0518510129485522));
#128559=CARTESIAN_POINT('Ctrl Pts',(6.497417067,4.043593265,3.216530967));
#128560=CARTESIAN_POINT('Ctrl Pts',(6.67384440999999,3.977881214,2.860146389));
#128561=CARTESIAN_POINT('Ctrl Pts',(6.810235101,3.913265985,2.486603681));
#128562=CARTESIAN_POINT('Ctrl Pts',(6.81495543020653,3.91102972422297,2.47367578583701));
#128563=CARTESIAN_POINT('Ctrl Pts',(6.81967575941306,3.90879346344597,2.46074789067403));
#128564=CARTESIAN_POINT('Ctrl Pts',(6.60895907756968,4.043593265,3.54678116859732));
#128565=CARTESIAN_POINT('Ctrl Pts',(6.80350070809697,3.977881214,3.18427848912944));
#128566=CARTESIAN_POINT('Ctrl Pts',(6.95722787297176,3.913265985,2.80267320064579));
#128567=CARTESIAN_POINT('Ctrl Pts',(6.96254819814112,3.91102972422297,2.78946626859357));
#128568=CARTESIAN_POINT('Ctrl Pts',(6.96786852331048,3.90879346344595,2.77625933654135));
#128569=CARTESIAN_POINT('',(6.49952578032111,4.04280735945842,3.21226783088978));
#128570=CARTESIAN_POINT('Origin',(-0.163316158576928,4.16060424653016,-0.102518366934566));
#128571=CARTESIAN_POINT('Ctrl Pts',(6.72400525554583,4.0034549416088,3.32231144235511));
#128572=CARTESIAN_POINT('Ctrl Pts',(6.68653913777703,4.00969640396818,3.30398547236695));
#128573=CARTESIAN_POINT('Ctrl Pts',(6.64907962791028,4.01609134349056,3.28564364915466));
#128574=CARTESIAN_POINT('Ctrl Pts',(6.57426505880515,4.02919781055076,3.24896952995097));
#128575=CARTESIAN_POINT('Ctrl Pts',(6.53686662234059,4.03591692971601,3.23061597316373));
#128576=CARTESIAN_POINT('Ctrl Pts',(6.49952577957866,4.04280735926632,3.21226783479966));
#128577=CARTESIAN_POINT('Ctrl Pts',(6.116469301,3.913265985,3.892467507));
#128578=CARTESIAN_POINT('Ctrl Pts',(6.32759640899999,3.978309763,3.560710729));
#128579=CARTESIAN_POINT('Ctrl Pts',(6.501601551,4.043585554,3.208064411));
#128580=CARTESIAN_POINT('Ctrl Pts',(6.456035448,3.913265985,3.817015365));
#128581=CARTESIAN_POINT('Ctrl Pts',(6.663070038,3.978309763,3.466840548));
#128582=CARTESIAN_POINT('Ctrl Pts',(6.831014547,4.043585554,3.096326897));
#128583=CARTESIAN_POINT('Origin',(-0.176878902022397,4.01785697920935,-0.0920262527008903));
#128584=CARTESIAN_POINT('Ctrl Pts',(5.654051988,4.043593265,4.538082868));
#128585=CARTESIAN_POINT('Ctrl Pts',(5.902966708,3.977881214,4.227957027));
#128586=CARTESIAN_POINT('Ctrl Pts',(6.116469301,3.913265985,3.892467507));
#128587=CARTESIAN_POINT('Ctrl Pts',(6.12385838672874,3.9110297242607,3.88085659029149));
#128588=CARTESIAN_POINT('Ctrl Pts',(6.13124747245758,3.90879346352142,3.86924567358297));
#128589=CARTESIAN_POINT('Ctrl Pts',(5.69199217717727,4.043593265,4.88459023813079));
#128590=CARTESIAN_POINT('Ctrl Pts',(5.95991289298509,3.977881214,4.57238337002353));
#128591=CARTESIAN_POINT('Ctrl Pts',(6.19207986003697,3.913265985,4.23274659681963));
#128592=CARTESIAN_POINT('Ctrl Pts',(6.20011489885699,3.9110297242607,4.22099214832055));
#128593=CARTESIAN_POINT('Ctrl Pts',(6.20814993767701,3.90879346352142,4.20923769982152));
#128594=CARTESIAN_POINT('',(5.65702784913764,4.04280735944397,4.53437271253314));
#128595=CARTESIAN_POINT('Origin',(-0.137459569024259,4.16060421429331,-0.135229751280873));
#128596=CARTESIAN_POINT('Ctrl Pts',(5.85260299563805,4.00345494155613,4.69010001717245));
#128597=CARTESIAN_POINT('Ctrl Pts',(5.81995229347557,4.00969641600747,4.66414834014744));
#128598=CARTESIAN_POINT('Ctrl Pts',(5.7873115502117,4.01609134926909,4.63818267851389));
#128599=CARTESIAN_POINT('Ctrl Pts',(5.72213000906131,4.02919780559788,4.58628310167405));
#128600=CARTESIAN_POINT('Ctrl Pts',(5.68955138599866,4.03591692734122,4.5603190719445));
#128601=CARTESIAN_POINT('Ctrl Pts',(5.65702784741048,4.04280735928509,4.53437271658464));
#128602=CARTESIAN_POINT('Ctrl Pts',(5.136704194,3.913265985,5.11632387800001));
#128603=CARTESIAN_POINT('Ctrl Pts',(5.414213168,3.978309763,4.837709477));
#128604=CARTESIAN_POINT('Ctrl Pts',(5.659958701,4.043585554,4.530713796));
#128605=CARTESIAN_POINT('Ctrl Pts',(5.484551453,3.913265985,5.115632449));
#128606=CARTESIAN_POINT('Ctrl Pts',(5.762022925,3.978309763,4.818150842));
#128607=CARTESIAN_POINT('Ctrl Pts',(6.005690467,4.043585554,4.492402699));
#128608=CARTESIAN_POINT('Origin',(-0.152960641359825,4.0178569617403,-0.127898470072109));
#128609=CARTESIAN_POINT('Ctrl Pts',(4.546309723,4.043593265,5.647439057));
#128610=CARTESIAN_POINT('Ctrl Pts',(4.856072844,3.977881214,5.39807309299999));
#128611=CARTESIAN_POINT('Ctrl Pts',(5.136704194,3.913265985,5.116323878));
#128612=CARTESIAN_POINT('Ctrl Pts',(5.1464165311493,3.91102972419369,5.10657285279335));
#128613=CARTESIAN_POINT('Ctrl Pts',(5.15612886829848,3.9087934633874,5.0968218275867));
#128614=CARTESIAN_POINT('Ctrl Pts',(4.50887404986768,4.043593265,5.99400129611241));
#128615=CARTESIAN_POINT('Ctrl Pts',(4.83764617598171,3.977881214,5.74668868624019));
#128616=CARTESIAN_POINT('Ctrl Pts',(5.13739707470347,3.913265985,5.46490146661399));
#128617=CARTESIAN_POINT('Ctrl Pts',(5.14777111804963,3.91102972419369,5.45514912610975));
#128618=CARTESIAN_POINT('Ctrl Pts',(5.15814516139567,3.9087934633874,5.4453967856054));
#128619=CARTESIAN_POINT('',(4.5500135837177,4.0428073594318,5.64445536550249));
#128620=CARTESIAN_POINT('Origin',(-0.105175429544502,4.16060423354011,-0.161617879588788));
#128621=CARTESIAN_POINT('Ctrl Pts',(4.70753952467976,4.00345494161455,5.83858472753934));
#128622=CARTESIAN_POINT('Ctrl Pts',(4.68123102122189,4.0096964160736,5.80622085031341));
#128623=CARTESIAN_POINT('Ctrl Pts',(4.65493525026559,4.01609134930381,5.7738454564778));
#128624=CARTESIAN_POINT('Ctrl Pts',(4.60243447779962,4.02919780923709,5.70914714015498));
#128625=CARTESIAN_POINT('Ctrl Pts',(4.57619903173416,4.03591692907489,5.67678670369158));
#128626=CARTESIAN_POINT('Ctrl Pts',(4.55001358156977,4.04280735924305,5.64445536838016));
#128627=CARTESIAN_POINT('Ctrl Pts',(3.916752508,3.913265985,6.100946631));
#128628=CARTESIAN_POINT('Ctrl Pts',(4.247667337,3.978309763,5.88850230599999));
#128629=CARTESIAN_POINT('Ctrl Pts',(4.553662473,4.043585554,5.641512038));
#128630=CARTESIAN_POINT('Ctrl Pts',(4.256615929,3.913265985,6.175048246));
#128631=CARTESIAN_POINT('Ctrl Pts',(4.591550023,3.978309763,5.944169758));
#128632=CARTESIAN_POINT('Ctrl Pts',(4.899546976,4.043585554,5.678418744));
#128633=CARTESIAN_POINT('Origin',(-0.121890082464141,4.01785694597163,-0.15779024085729));
#128634=CARTESIAN_POINT('Ctrl Pts',(3.225987068,4.043593265,6.492727273));
#128635=CARTESIAN_POINT('Ctrl Pts',(3.58211441,3.977881214,6.31578126));
#128636=CARTESIAN_POINT('Ctrl Pts',(3.916752508,3.913265985,6.100946631));
#128637=CARTESIAN_POINT('Ctrl Pts',(3.92833395842363,3.91102972416853,6.09351144469005));
#128638=CARTESIAN_POINT('Ctrl Pts',(3.93991540884725,3.90879346333707,6.08607625837996));
#128639=CARTESIAN_POINT('Ctrl Pts',(3.114925983046,4.043593265,6.82313951611881));
#128640=CARTESIAN_POINT('Ctrl Pts',(3.4891765001953,3.977881214,6.65228522632004));
#128641=CARTESIAN_POINT('Ctrl Pts',(3.84249531148228,3.913265985,6.44152361799445));
#128642=CARTESIAN_POINT('Ctrl Pts',(3.85472328050648,3.91102972416852,6.43422939437612));
#128643=CARTESIAN_POINT('Ctrl Pts',(3.86695124953061,3.90879346333707,6.42693517075777));
#128644=CARTESIAN_POINT('',(3.23024573998459,4.04280735943644,6.49060955893343));
#128645=CARTESIAN_POINT('Origin',(-0.0679733892149625,4.16060421634694,
-0.180448891774344));
#128646=CARTESIAN_POINT('Ctrl Pts',(3.34235673751932,4.00345494162258,6.71406370518684));
#128647=CARTESIAN_POINT('Ctrl Pts',(3.32362058915715,4.00969641608109,6.67680092687676));
#128648=CARTESIAN_POINT('Ctrl Pts',(3.30489935139104,4.01609134929957,6.6395296383611));
#128649=CARTESIAN_POINT('Ctrl Pts',(3.26753424118094,4.02919781000407,6.56505781410496));
#128650=CARTESIAN_POINT('Ctrl Pts',(3.24886870383412,4.03591692942377,6.52781410369642));
#128651=CARTESIAN_POINT('Ctrl Pts',(3.23024573750669,4.04280735919962,6.49060956132151));
#128652=CARTESIAN_POINT('Ctrl Pts',(2.513657828,3.913265985,6.8002959));
#128653=CARTESIAN_POINT('Ctrl Pts',(2.882505303,3.978309763,6.663955312));
#128654=CARTESIAN_POINT('Ctrl Pts',(3.234442049,4.043585554,6.488519448));
#128655=CARTESIAN_POINT('Ctrl Pts',(2.829645774,3.913265985,6.945725649));
#128656=CARTESIAN_POINT('Ctrl Pts',(3.206381346,3.978309763,6.792245902));
#128657=CARTESIAN_POINT('Ctrl Pts',(3.564306113,4.043585554,6.59891824));
#128658=CARTESIAN_POINT('Origin',(-0.0851200586046991,4.0178569676344,-0.180303803708096));
#128659=CARTESIAN_POINT('Ctrl Pts',(1.754820843,4.043593265,7.034422777));
#128660=CARTESIAN_POINT('Ctrl Pts',(2.140660288,3.977881214,6.938170516));
#128661=CARTESIAN_POINT('Ctrl Pts',(2.513657828,3.913265985,6.8002959));
#128662=CARTESIAN_POINT('Ctrl Pts',(2.52656685588248,3.91102972415818,6.79552421367136));
#128663=CARTESIAN_POINT('Ctrl Pts',(2.53947588376501,3.90879346331638,6.79075252734283));
#128664=CARTESIAN_POINT('Ctrl Pts',(1.5753274386396,4.043593265,7.33323531634172));
#128665=CARTESIAN_POINT('Ctrl Pts',(1.97755680933523,3.977881214,7.24682830281787));
#128666=CARTESIAN_POINT('Ctrl Pts',(2.36792273908028,3.913265985,7.11694728376972));
#128667=CARTESIAN_POINT('Ctrl Pts',(2.38143286751558,3.91102972415818,7.1124522468955));
#128668=CARTESIAN_POINT('Ctrl Pts',(2.39494299595088,3.90879346331638,7.10795721002117));
#128669=CARTESIAN_POINT('',(1.75943519548214,4.04280735942786,7.03327006341456));
#128670=CARTESIAN_POINT('Origin',(-0.0275930671524408,4.16060426191353,
-0.190842484786877));
#128671=CARTESIAN_POINT('Ctrl Pts',(1.82088906445054,4.00345494158803,7.27560052582954));
#128672=CARTESIAN_POINT('Ctrl Pts',(1.81060137241643,4.00969640404014,7.23518129027532));
#128673=CARTESIAN_POINT('Ctrl Pts',(1.80033004124381,4.01609134347794,7.19475682903795));
#128674=CARTESIAN_POINT('Ctrl Pts',(1.77984774251408,4.02919780709716,7.11399370280583));
#128675=CARTESIAN_POINT('Ctrl Pts',(1.76962488919475,4.03591692801806,7.07360818143289));
#128676=CARTESIAN_POINT('Ctrl Pts',(1.75943519192525,4.04280735920122,7.03327006541419));
#128677=CARTESIAN_POINT('Ctrl Pts',(0.993027302,3.913265985,7.18167089));
#128678=CARTESIAN_POINT('Ctrl Pts',(1.382560524,3.978309763,7.127809173));
#128679=CARTESIAN_POINT('Ctrl Pts',(1.763982709,4.043585554,7.032130901));
#128680=CARTESIAN_POINT('Ctrl Pts',(1.270364528,3.913265985,7.391628641));
#128681=CARTESIAN_POINT('Ctrl Pts',(1.67128584,3.978309763,7.322724176));
#128682=CARTESIAN_POINT('Ctrl Pts',(2.062402258,4.043585554,7.210859652));
#128683=CARTESIAN_POINT('Origin',(-0.0443700637133654,4.01785698804151,
-0.194387020948577));
#128684=CARTESIAN_POINT('Ctrl Pts',(0.201601146,4.043593265,7.247196491));
#128685=CARTESIAN_POINT('Ctrl Pts',(0.59911127,3.977881214,7.236138629));
#128686=CARTESIAN_POINT('Ctrl Pts',(0.993027301999999,3.913265985,7.18167089));
#128687=CARTESIAN_POINT('Ctrl Pts',(1.0066602952472,3.91102972420058,7.17978582247885));
#128688=CARTESIAN_POINT('Ctrl Pts',(1.02029328849439,3.90879346340122,7.17790075495781));
#128689=CARTESIAN_POINT('Ctrl Pts',(-0.0379316651698515,4.043593265,7.50043718252154));
#128690=CARTESIAN_POINT('Ctrl Pts',(0.373468759383329,3.977881214,7.50251774175908));
#128691=CARTESIAN_POINT('Ctrl Pts',(0.78262873003964,3.913265985,7.45959040487349));
#128692=CARTESIAN_POINT('Ctrl Pts',(0.796789298952412,3.91102972420058,
7.45810473776085));
#128693=CARTESIAN_POINT('Ctrl Pts',(0.810949867865185,3.90879346340121,
7.45661907064821));
#128694=CARTESIAN_POINT('',(0.20635541671928,4.04280735947359,7.24706267597459));
#128695=CARTESIAN_POINT('Origin',(0.0140775383825686,4.16060426862506,-0.192312383134926));
#128696=CARTESIAN_POINT('Ctrl Pts',(0.214278641765392,4.00345494161275,
7.4969383524598));
#128697=CARTESIAN_POINT('Ctrl Pts',(0.21292040859655,4.00969641605623,7.45525246640273));
#128698=CARTESIAN_POINT('Ctrl Pts',(0.211579281215642,4.01609134932557,
7.41356511708819));
#128699=CARTESIAN_POINT('Ctrl Pts',(0.208937532970993,4.02919780991452,
7.3302871182516));
#128700=CARTESIAN_POINT('Ctrl Pts',(0.20763537809521,4.03591692941635,7.28864818600079));
#128701=CARTESIAN_POINT('Ctrl Pts',(0.206355413357484,4.04280735927498,
7.24706267686669));
#128702=CARTESIAN_POINT('Ctrl Pts',(-0.574036077,3.913265985,7.227238932));
#128703=CARTESIAN_POINT('Ctrl Pts',(-0.182031249,3.978309763,7.2583746));
#128704=CARTESIAN_POINT('Ctrl Pts',(0.211041498,4.043585554,7.246927727));
#128705=CARTESIAN_POINT('Ctrl Pts',(-0.348317552,3.913265985,7.491907293));
#128706=CARTESIAN_POINT('Ctrl Pts',(0.0580428659999999,3.978309763,7.510800007));
#128707=CARTESIAN_POINT('Ctrl Pts',(0.464062765,4.043585554,7.485629282));
#128708=CARTESIAN_POINT('Origin',(-0.00154526844133959,4.01785679159005,
-0.199381631082065));
#128709=CARTESIAN_POINT('Ctrl Pts',(0.201420355,1.975104983,7.247201518));
#128710=CARTESIAN_POINT('Ctrl Pts',(0.597450238,1.909367073,7.23619472));
#128711=CARTESIAN_POINT('Ctrl Pts',(0.989922563999999,1.844275173,7.182099506));
#128712=CARTESIAN_POINT('Ctrl Pts',(0.993831803810694,1.84362682194445,
7.18156068797354));
#128713=CARTESIAN_POINT('Ctrl Pts',(0.997741043621388,1.84297847088892,
7.18102186994708));
#128714=CARTESIAN_POINT('Ctrl Pts',(-0.037616899,1.975104983,7.49990566400001));
#128715=CARTESIAN_POINT('Ctrl Pts',(0.372222232,1.909367073,7.501961273));
#128716=CARTESIAN_POINT('Ctrl Pts',(0.77984494,1.844275173,7.459345941));
#128717=CARTESIAN_POINT('Ctrl Pts',(0.783905085932064,1.84362682194446,
7.45892146890002));
#128718=CARTESIAN_POINT('Ctrl Pts',(0.787965231864127,1.84297847088891,
7.45849699680004));
#128719=CARTESIAN_POINT('',(0.213157852172123,1.93490816642933,7.49697023463349));
#128720=CARTESIAN_POINT('',(0.779844939665357,1.84427517280771,7.459345940031));
#128721=CARTESIAN_POINT('Origin',(0.00791499441159103,2.01782137169043,
-0.189678174975023));
#128722=CARTESIAN_POINT('',(0.884883748724035,1.84427517246151,7.32072272389598));
#128723=CARTESIAN_POINT('Ctrl Pts',(0.213157850962533,1.9349081733935,7.49697023571379));
#128724=CARTESIAN_POINT('Ctrl Pts',(0.211950237202354,1.94116543724157,
7.45528053998422));
#128725=CARTESIAN_POINT('Ctrl Pts',(0.210760567417153,1.94757342722814,
7.41358973092107));
#128726=CARTESIAN_POINT('Ctrl Pts',(0.208423369809919,1.96070006887751,
7.33030278216503));
#128727=CARTESIAN_POINT('Ctrl Pts',(0.20727451674072,1.967426141464,7.28865951924096));
#128728=CARTESIAN_POINT('Ctrl Pts',(0.206148889166361,1.97432008375446,
7.24706856084113));
#128729=CARTESIAN_POINT('Ctrl Pts',(0.963002974177823,1.83976484773663,
7.1858098847225));
#128730=CARTESIAN_POINT('Ctrl Pts',(0.976462769088904,1.84202001036834,
7.18395469536125));
#128731=CARTESIAN_POINT('Ctrl Pts',(0.989922564,1.844275173,7.182099506));
#128732=CARTESIAN_POINT('Ctrl Pts',(1.380938204,1.909789088,7.12820507000001));
#128733=CARTESIAN_POINT('Ctrl Pts',(1.763791699,1.975097379,7.032178812));
#128734=CARTESIAN_POINT('Ctrl Pts',(1.24002876832294,1.83976484773663,7.39735947533262));
#128735=CARTESIAN_POINT('Ctrl Pts',(1.25388307164246,1.84202001036834,7.39498364010001));
#128736=CARTESIAN_POINT('Ctrl Pts',(1.26773737496199,1.844275173,7.39260780486741));
#128737=CARTESIAN_POINT('Ctrl Pts',(1.67021373623052,1.909789088,7.32358827372707));
#128738=CARTESIAN_POINT('Ctrl Pts',(2.06281816648083,1.975097379,7.21128209294712));
#128739=CARTESIAN_POINT('',(1.26716903471351,1.8442751723037,7.39217717123405));
#128740=CARTESIAN_POINT('',(1.81980133219834,1.93490816640524,7.2758725994878));
#128741=CARTESIAN_POINT('Origin',(-0.0374597101700138,1.87499929406416,
-0.18934890740966));
#128742=CARTESIAN_POINT('Ctrl Pts',(1.75923475895739,1.97432008480599,7.03332020162639));
#128743=CARTESIAN_POINT('Ctrl Pts',(1.76927489670746,1.9674261427311,7.07369680848882));
#128744=CARTESIAN_POINT('Ctrl Pts',(1.77934896230285,1.96070006933456,7.11411951036083));
#128745=CARTESIAN_POINT('Ctrl Pts',(1.79953573986834,1.94757343428078,7.19495678728885));
#128746=CARTESIAN_POINT('Ctrl Pts',(1.80965987568692,1.94116545127622,7.235417097252));
#128747=CARTESIAN_POINT('Ctrl Pts',(1.81980133128369,1.93490817334207,7.27587260079001));
#128748=CARTESIAN_POINT('',(1.12854578661553,1.84427517216382,7.28713831720777));
#128749=CARTESIAN_POINT('Origin',(4.32271406169971E-13,1.93599222700044,
1.56385321359309E-12));
#128750=CARTESIAN_POINT('',(1.82542260132892,1.75423095989052,7.27446440115187));
#128751=CARTESIAN_POINT('Origin',(-0.00348377670905842,2.01767780014573,
-0.183605604020702));
#128752=CARTESIAN_POINT('',(2.365151478457,1.84427517280771,7.1173069671318));
#128753=CARTESIAN_POINT('Origin',(-0.065213110636855,1.87499309172002,-0.180566992369885));
#128754=CARTESIAN_POINT('Origin',(-0.0330452119085806,2.01782140614763,
-0.186944947047757));
#128755=CARTESIAN_POINT('Ctrl Pts',(1.754645359,1.975104983,7.03446655100001));
#128756=CARTESIAN_POINT('Ctrl Pts',(2.139050148,1.909367073,6.938582368));
#128757=CARTESIAN_POINT('Ctrl Pts',(2.510717817,1.844275173,6.801381922));
#128758=CARTESIAN_POINT('Ctrl Pts',(2.51441983100647,1.84362682194445,6.80001533024304));
#128759=CARTESIAN_POINT('Ctrl Pts',(2.51812184501293,1.84297847088892,6.79864873848607));
#128760=CARTESIAN_POINT('Ctrl Pts',(1.575520586,1.975104983,7.332648559));
#128761=CARTESIAN_POINT('Ctrl Pts',(1.9762198,1.909367073,7.246552811));
#128762=CARTESIAN_POINT('Ctrl Pts',(2.365151479,1.844275173,7.11730696800001));
#128763=CARTESIAN_POINT('Ctrl Pts',(2.36902545202297,1.84362682194445,7.11601960845552));
#128764=CARTESIAN_POINT('Ctrl Pts',(2.37289942504594,1.84297847088892,7.11473224891103));
#128765=CARTESIAN_POINT('',(2.43793464488575,1.84427517246151,6.95934444609096));
#128766=CARTESIAN_POINT('Ctrl Pts',(2.48522521582265,1.83976484806346,6.81079246957085));
#128767=CARTESIAN_POINT('Ctrl Pts',(2.49797151641135,1.84202001053176,6.80608719578537));
#128768=CARTESIAN_POINT('Ctrl Pts',(2.510717817,1.844275173,6.801381922));
#128769=CARTESIAN_POINT('Ctrl Pts',(2.881006018,1.909789088,6.664690703));
#128770=CARTESIAN_POINT('Ctrl Pts',(3.234265804,1.975097379,6.488607301));
#128771=CARTESIAN_POINT('Ctrl Pts',(2.80125120977367,1.83976484806346,6.95784379157643));
#128772=CARTESIAN_POINT('Ctrl Pts',(2.81427087187049,1.84202001053176,6.95254523672656));
#128773=CARTESIAN_POINT('Ctrl Pts',(2.82729053396737,1.844275173,6.94724668187658));
#128774=CARTESIAN_POINT('Ctrl Pts',(3.20552006197391,1.909789088,6.79332026772587));
#128775=CARTESIAN_POINT('Ctrl Pts',(3.56480310984828,1.975097379,6.5992413961445));
#128776=CARTESIAN_POINT('',(2.8266429077416,1.8442751723037,6.94694829259179));
#128777=CARTESIAN_POINT('',(3.3413529234146,1.93490816639311,6.71456324812156));
#128778=CARTESIAN_POINT('Origin',(-0.0772883907455425,1.87499928331842,
-0.176869385909534));
#128779=CARTESIAN_POINT('Ctrl Pts',(3.23006076814399,1.9743200848156,6.49070161308116));
#128780=CARTESIAN_POINT('Ctrl Pts',(3.24854594976339,1.96742614274508,6.52797590452996));
#128781=CARTESIAN_POINT('Ctrl Pts',(3.26707417510478,1.96070006935587,6.5652879197994));
#128782=CARTESIAN_POINT('Ctrl Pts',(3.30416664053432,1.94757342764407,6.63989574361088));
#128783=CARTESIAN_POINT('Ctrl Pts',(3.32275187261112,1.9411654374316,6.6772337690076));
#128784=CARTESIAN_POINT('Ctrl Pts',(3.34135292276299,1.93490817334722,6.71456324961192));
#128785=CARTESIAN_POINT('',(2.66868034532562,1.84427517216382,6.87416508912661));
#128786=CARTESIAN_POINT('Origin',(5.60966204044E-13,1.93599222699961,1.18524981496115E-12));
#128787=CARTESIAN_POINT('',(3.34654004958858,1.75423095987511,6.71197956603296));
#128788=CARTESIAN_POINT('Origin',(-0.0428723253219038,2.01767774273086,
-0.178564540033815));
#128789=CARTESIAN_POINT('',(3.83986616329838,1.84427517280772,6.44247063125013));
#128790=CARTESIAN_POINT('Origin',(-0.102505000051829,1.87499306998262,-0.162326509816113));
#128791=CARTESIAN_POINT('Origin',(-0.0724602198121888,2.01782139366673,
-0.175470450256001));
#128792=CARTESIAN_POINT('Ctrl Pts',(3.225825097,1.975104983,6.492807747));
#128793=CARTESIAN_POINT('Ctrl Pts',(3.580630451,1.909367073,6.316529616));
#128794=CARTESIAN_POINT('Ctrl Pts',(3.914114695,1.844275173,6.102639278));
#128795=CARTESIAN_POINT('Ctrl Pts',(3.91743638113306,1.84362682194445,6.10050881282057));
#128796=CARTESIAN_POINT('Ctrl Pts',(3.92075806726612,1.84297847088892,6.09837834764114));
#128797=CARTESIAN_POINT('Ctrl Pts',(3.114988478,1.975104983,6.822524956));
#128798=CARTESIAN_POINT('Ctrl Pts',(3.487811527,1.909367073,6.652303593));
#128799=CARTESIAN_POINT('Ctrl Pts',(3.839866164,1.844275173,6.442470632));
#128800=CARTESIAN_POINT('Ctrl Pts',(3.84337282144137,1.84362682194445,6.44038058052275));
#128801=CARTESIAN_POINT('Ctrl Pts',(3.84687947888274,1.84297847088892,6.4382905290455));
#128802=CARTESIAN_POINT('',(3.87699042669309,1.84427517246151,6.27255495673493));
#128803=CARTESIAN_POINT('Ctrl Pts',(3.89124108478693,1.83976484779183,6.11730996879012));
#128804=CARTESIAN_POINT('Ctrl Pts',(3.90267788989351,1.84202001039595,6.10997462339513));
#128805=CARTESIAN_POINT('Ctrl Pts',(3.914114695,1.844275173,6.102639278));
#128806=CARTESIAN_POINT('Ctrl Pts',(4.246361193,1.909789088,5.889542806));
#128807=CARTESIAN_POINT('Ctrl Pts',(4.553509235,1.975097379,5.641635724));
#128808=CARTESIAN_POINT('Ctrl Pts',(4.23149025439034,1.83976484779184,6.19298706509833));
#128809=CARTESIAN_POINT('Ctrl Pts',(4.24306649205931,1.84202001039594,6.18501354457374));
#128810=CARTESIAN_POINT('Ctrl Pts',(4.25464272972824,1.844275173,6.17704002404914));
#128811=CARTESIAN_POINT('Ctrl Pts',(4.59093983278288,1.909789088,5.94540415665823));
#128812=CARTESIAN_POINT('Ctrl Pts',(4.90010182207874,1.975097379,5.67862750577175));
#128813=CARTESIAN_POINT('',(4.25394609972331,1.84427517230371,6.17688783142564));
#128814=CARTESIAN_POINT('',(4.70666656643382,1.9349081664224,5.83928838194006));
#128815=CARTESIAN_POINT('Origin',(-0.11350299420495,1.87499925757301,-0.156119410337943));
#128816=CARTESIAN_POINT('Ctrl Pts',(4.54985272534518,1.9743200847369,5.64458503093839));
#128817=CARTESIAN_POINT('Ctrl Pts',(4.57591860462525,1.96742614269182,5.67701410255906));
#128818=CARTESIAN_POINT('Ctrl Pts',(4.60203463076806,1.96070006932564,5.70947076292011));
#128819=CARTESIAN_POINT('Ctrl Pts',(4.65429837177693,1.94757342765889,5.77436051368685));
#128820=CARTESIAN_POINT('Ctrl Pts',(4.68047566329595,1.94116543745121,5.80683032136998));
#128821=CARTESIAN_POINT('Ctrl Pts',(4.7066665661253,1.93490817338302,5.83928838353088));
#128822=CARTESIAN_POINT('',(4.08403037681007,1.84427517216382,6.13976354063303));
#128823=CARTESIAN_POINT('Origin',(-4.96564594998361E-13,1.93599222700044,
-6.63098048692135E-13));
#128824=CARTESIAN_POINT('',(4.7111770048529,1.75423095988382,5.83565002604275));
#128825=CARTESIAN_POINT('Origin',(-0.0802558982021118,2.01767775762883,
-0.165173268931585));
#128826=CARTESIAN_POINT('',(5.1350329741554,1.84427517280772,5.46639152841487));
#128827=CARTESIAN_POINT('Origin',(-0.13500413187521,1.87499307142583,-0.13649613936879));
#128828=CARTESIAN_POINT('Origin',(-0.108487184789677,2.01782137235173,-0.155791332412841));
#128829=CARTESIAN_POINT('Ctrl Pts',(4.546168838,1.975104983,5.647552469));
#128830=CARTESIAN_POINT('Ctrl Pts',(4.854784453,1.909367073,5.39912296));
#128831=CARTESIAN_POINT('Ctrl Pts',(5.134491921,1.844275173,5.118544003));
#128832=CARTESIAN_POINT('Ctrl Pts',(5.13727796092389,1.84362682194446,5.11574928256729));
#128833=CARTESIAN_POINT('Ctrl Pts',(5.14006400084776,1.84297847088891,5.11295456213457));
#128834=CARTESIAN_POINT('Ctrl Pts',(4.508802972,1.975104983,5.99338767));
#128835=CARTESIAN_POINT('Ctrl Pts',(4.836317064,1.909367073,5.747000052));
#128836=CARTESIAN_POINT('Ctrl Pts',(5.135032975,1.844275173,5.466391529));
#128837=CARTESIAN_POINT('Ctrl Pts',(5.13800834945066,1.84362682194446,5.4635965140737));
#128838=CARTESIAN_POINT('Ctrl Pts',(5.1409837239013,1.84297847088891,5.46080149914739));
#128839=CARTESIAN_POINT('',(5.13476244563166,1.84427517246151,5.29246776829776));
#128840=CARTESIAN_POINT('Ctrl Pts',(5.11530684846201,1.83976484789648,5.13778885074469));
#128841=CARTESIAN_POINT('Ctrl Pts',(5.12489938473102,1.84202001044827,5.12816642687234));
#128842=CARTESIAN_POINT('Ctrl Pts',(5.134491921,1.844275173,5.118544003));
#128843=CARTESIAN_POINT('Ctrl Pts',(5.413161237,1.909789088,4.839006433));
#128844=CARTESIAN_POINT('Ctrl Pts',(5.659835635,1.975097379,4.530867531));
#128845=CARTESIAN_POINT('Ctrl Pts',(5.46386952005827,1.83976484789648,5.13855314624981));
#128846=CARTESIAN_POINT('Ctrl Pts',(5.47346104026047,1.84202001044827,5.12827749352533));
#128847=CARTESIAN_POINT('Ctrl Pts',(5.4830525604627,1.844275173,5.11800184080086));
#128848=CARTESIAN_POINT('Ctrl Pts',(5.76169235907365,1.909789088,4.81948755470486));
#128849=CARTESIAN_POINT('Ctrl Pts',(6.00627721912842,1.975097379,4.49248730463809));
#128850=CARTESIAN_POINT('',(5.48233950037921,1.84427517230372,5.11800296121163));
#128851=CARTESIAN_POINT('',(5.85190171137635,1.93490816642628,4.69097488087022));
#128852=CARTESIAN_POINT('Origin',(-0.144410508305228,1.87499923698847,-0.128069709885178));
#128853=CARTESIAN_POINT('Ctrl Pts',(5.65689862657596,1.97432008475222,4.5345339261759));
#128854=CARTESIAN_POINT('Ctrl Pts',(5.68932639172034,1.96742614271044,4.56060143059601));
#128855=CARTESIAN_POINT('Ctrl Pts',(5.72180906206406,1.96070006934937,4.58668509865171));
#128856=CARTESIAN_POINT('Ctrl Pts',(5.78680028388126,1.9475734276705,4.6388226038334));
#128857=CARTESIAN_POINT('Ctrl Pts',(5.81934561353501,1.94116543746918,4.66490594160808));
#128858=CARTESIAN_POINT('Ctrl Pts',(5.85190171140948,1.9349081733955,4.69097488250165));
#128859=CARTESIAN_POINT('',(5.308415687593,1.84427517216382,5.11827347277353));
#128860=CARTESIAN_POINT('Origin',(-1.30494573480355E-12,1.93599222700033,
-1.11239142897013E-12));
#128861=CARTESIAN_POINT('',(5.85552455985458,1.754230959877,4.68645197672461));
#128862=CARTESIAN_POINT('Origin',(-0.11388718633198,2.01767782005154,-0.144059198590631));
#128863=CARTESIAN_POINT('',(6.19009135031759,1.84427517280653,4.23471003320411));
#128864=CARTESIAN_POINT('Origin',(-0.161190268281893,1.874993126293,-0.104282894811087));
#128865=CARTESIAN_POINT('Origin',(-0.139441557183412,2.01782139164873,-0.128827646493924));
#128866=CARTESIAN_POINT('Ctrl Pts',(5.653938778,1.975104983,4.538223914));
#128867=CARTESIAN_POINT('Ctrl Pts',(5.90193413,1.909367073,4.229259314));
#128868=CARTESIAN_POINT('Ctrl Pts',(6.114786011,1.844275173,3.895111301));
#128869=CARTESIAN_POINT('Ctrl Pts',(6.11690613257765,1.84362682194445,3.89178300336333));
#128870=CARTESIAN_POINT('Ctrl Pts',(6.11902625415531,1.84297847088892,3.88845470572666));
#128871=CARTESIAN_POINT('Ctrl Pts',(5.69179085,1.975104983,4.884006237));
#128872=CARTESIAN_POINT('Ctrl Pts',(5.958681789,1.909367073,4.572973176));
#128873=CARTESIAN_POINT('Ctrl Pts',(6.190091351,1.844275173,4.234710034));
#128874=CARTESIAN_POINT('Ctrl Pts',(6.19239631726747,1.84362682194445,4.23134074741953));
#128875=CARTESIAN_POINT('Ctrl Pts',(6.19470128353494,1.84297847088892,4.22797146083906));
#128876=CARTESIAN_POINT('',(6.15243867918099,1.84427517246151,4.06491067025317));
#128877=CARTESIAN_POINT('Ctrl Pts',(6.10018654800587,1.83976484784501,3.91803043868467));
#128878=CARTESIAN_POINT('Ctrl Pts',(6.10748627950293,1.84202001042253,3.90657086984234));
#128879=CARTESIAN_POINT('Ctrl Pts',(6.114786011,1.844275173,3.895111301));
#128880=CARTESIAN_POINT('Ctrl Pts',(6.326847879,1.909789088,3.562203498));
#128881=CARTESIAN_POINT('Ctrl Pts',(6.501514411,1.975097379,3.208241008));
#128882=CARTESIAN_POINT('Ctrl Pts',(6.44076431822769,1.83976484784501,3.84384619369943));
#128883=CARTESIAN_POINT('Ctrl Pts',(6.44792263252751,1.84202001042254,3.83174888655724));
#128884=CARTESIAN_POINT('Ctrl Pts',(6.45508094682746,1.844275173,3.8196515794151));
#128885=CARTESIAN_POINT('Ctrl Pts',(6.66303455481777,1.909789088,3.46821707098679));
#128886=CARTESIAN_POINT('Ctrl Pts',(6.83160576852397,1.975097379,3.09628339007489));
#128887=CARTESIAN_POINT('',(6.45438479854498,1.84427517230371,3.81980596047474));
#128888=CARTESIAN_POINT('',(6.72350843623044,1.93490816641997,3.32331660799437));
#128889=CARTESIAN_POINT('Origin',(-0.168565380183781,1.87499926396933,-0.0940314670157107));
#128890=CARTESIAN_POINT('Ctrl Pts',(6.49943423469485,1.97432008473515,3.21245305500109));
#128891=CARTESIAN_POINT('Ctrl Pts',(6.53670759948147,1.9674261426851,3.23094010477837));
#128892=CARTESIAN_POINT('Ctrl Pts',(6.57403806058471,1.96070006931838,3.24943113724768));
#128893=CARTESIAN_POINT('Ctrl Pts',(6.64871784604601,1.94757342764741,3.28637850489496));
#128894=CARTESIAN_POINT('Ctrl Pts',(6.68610943057429,1.94116543744624,3.30485574482876));
#128895=CARTESIAN_POINT('Ctrl Pts',(6.7235084366159,1.93490817338319,3.32331660957366));
#128896=CARTESIAN_POINT('',(6.28458538020791,1.84427517216382,3.85745862658826));
#128897=CARTESIAN_POINT('Origin',(1.45499931547555E-12,1.93599222699967,
7.1427239123345E-13));
#128898=CARTESIAN_POINT('',(6.72607429391972,1.75423095987622,3.31812064156621));
#128899=CARTESIAN_POINT('Origin',(-0.14219294244321,2.01767772921235,-0.116208729104463));
#128900=CARTESIAN_POINT('',(6.95570793398766,1.84427517280772,2.80501820382695));
#128901=CARTESIAN_POINT('Origin',(-0.179839597763203,1.87499310911281,-0.0671937332859013));
#128902=CARTESIAN_POINT('Origin',(-0.163875474593108,2.01782135634014,-0.0958398398494609));
#128903=CARTESIAN_POINT('Ctrl Pts',(6.497336824,1.975104983,3.216693053));
#128904=CARTESIAN_POINT('Ctrl Pts',(6.673115926,1.909367073,2.861640204));
#128905=CARTESIAN_POINT('Ctrl Pts',(6.809159503,1.844275173,2.489547522));
#128906=CARTESIAN_POINT('Ctrl Pts',(6.81051457170667,1.84362682194445,2.48584127463075));
#128907=CARTESIAN_POINT('Ctrl Pts',(6.81186964041335,1.84297847088892,2.48213502726149));
#128908=CARTESIAN_POINT('Ctrl Pts',(6.608636913,1.975104983,3.546254101));
#128909=CARTESIAN_POINT('Ctrl Pts',(6.802425177,1.909367073,3.185119157));
#128910=CARTESIAN_POINT('Ctrl Pts',(6.955707935,1.844275173,2.805018204));
#128911=CARTESIAN_POINT('Ctrl Pts',(6.95723471541271,1.84362682194445,2.80123218985553));
#128912=CARTESIAN_POINT('Ctrl Pts',(6.95876149582542,1.84297847088892,2.79744617571105));
#128913=CARTESIAN_POINT('',(6.88243371781536,1.84427517246151,2.64728286607984));
#128914=CARTESIAN_POINT('Ctrl Pts',(6.79982830483685,1.83976484801591,2.51506927495473));
#128915=CARTESIAN_POINT('Ctrl Pts',(6.80449390391836,1.84202001050798,2.50230839847734));
#128916=CARTESIAN_POINT('Ctrl Pts',(6.809159503,1.844275173,2.489547522));
#128917=CARTESIAN_POINT('Ctrl Pts',(6.94469814500001,1.909789088,2.118835886));
#128918=CARTESIAN_POINT('Ctrl Pts',(7.039189599,1.975097379,1.735600702));
#128919=CARTESIAN_POINT('Ctrl Pts',(7.11649613591557,1.83976484801591,2.36940526333307));
#128920=CARTESIAN_POINT('Ctrl Pts',(7.12088652920278,1.84202001050798,2.3560519590436));
#128921=CARTESIAN_POINT('Ctrl Pts',(7.12527692248992,1.844275173,2.34269865475413));
#128922=CARTESIAN_POINT('Ctrl Pts',(7.25282065986981,1.909789088,1.95477661131576));
#128923=CARTESIAN_POINT('Ctrl Pts',(7.33749602632692,1.975097379,1.55530070573886));
#128924=CARTESIAN_POINT('',(7.12463023715776,1.84427517230371,2.34299907776131));
#128925=CARTESIAN_POINT('',(7.28073137975271,1.93490816642443,1.80026374393309));
#128926=CARTESIAN_POINT('Origin',(-0.184838558833566,1.87499926562464,-0.0555965455474414));
#128927=CARTESIAN_POINT('Ctrl Pts',(7.03806352124641,1.97432008478782,1.7401614500682));
#128928=CARTESIAN_POINT('Ctrl Pts',(7.07843962488715,1.96742614271635,1.75020361104315));
#128929=CARTESIAN_POINT('Ctrl Pts',(7.11887234612364,1.96070006932726,1.76023738760861));
#128930=CARTESIAN_POINT('Ctrl Pts',(7.19974875171057,1.94757342764899,1.78026699959939));
#128931=CARTESIAN_POINT('Ctrl Pts',(7.24023820215542,1.94116543745568,1.79027416636109));
#128932=CARTESIAN_POINT('Ctrl Pts',(7.28073138046778,1.93490817339319,1.80026374539963));
#128933=CARTESIAN_POINT('',(6.96689484519621,1.84427517216382,2.41627330110929));
#128934=CARTESIAN_POINT('Origin',(2.55958448880378E-12,1.93599222699967,
5.89263880745872E-13));
#128935=CARTESIAN_POINT('',(7.28212026979303,1.75423095986773,1.79463767307641));
#128936=CARTESIAN_POINT('Origin',(-0.163849812250907,2.01767778307472,-0.0829245243346644));
#128937=CARTESIAN_POINT('',(7.3960833459743,1.84427517280772,1.24416684004963));
#128938=CARTESIAN_POINT('Origin',(-0.190079571013307,1.87499311850125,-0.0269625512453872));
#128939=CARTESIAN_POINT('Origin',(-0.180646895981356,2.01782136270622,-0.0583707742404796));
#128940=CARTESIAN_POINT('Ctrl Pts',(7.036926621,1.975104983,1.7447532));
#128941=CARTESIAN_POINT('Ctrl Pts',(7.132270238,1.909367073,1.360213978));
#128942=CARTESIAN_POINT('Ctrl Pts',(7.18514426400001,1.844275173,0.967575269));
#128943=CARTESIAN_POINT('Ctrl Pts',(7.18567091832362,1.84362682194445,0.963664371923291));
#128944=CARTESIAN_POINT('Ctrl Pts',(7.18619757264725,1.84297847088892,0.959753474846583));
#128945=CARTESIAN_POINT('Ctrl Pts',(7.21647046,1.975104983,2.042683064));
#128946=CARTESIAN_POINT('Ctrl Pts',(7.328094724,1.909367073,1.648332506));
#128947=CARTESIAN_POINT('Ctrl Pts',(7.396083347,1.844275173,1.24416684));
#128948=CARTESIAN_POINT('Ctrl Pts',(7.39676055100675,1.84362682194445,1.24014112810397));
#128949=CARTESIAN_POINT('Ctrl Pts',(7.39743775501351,1.84297847088892,1.23611541620793));
#128950=CARTESIAN_POINT('',(7.29061380500513,1.84427517246151,1.10587105776249));
#128951=CARTESIAN_POINT('Ctrl Pts',(7.18151764643602,1.83976484795739,0.994506269714354));
#128952=CARTESIAN_POINT('Ctrl Pts',(7.18333095521794,1.84202001047872,0.981040769357178));
#128953=CARTESIAN_POINT('Ctrl Pts',(7.18514426400001,1.844275173,0.967575269));
#128954=CARTESIAN_POINT('Ctrl Pts',(7.237822045,1.909789088,0.576393863000001));
#128955=CARTESIAN_POINT('Ctrl Pts',(7.247720104,1.975097379,0.181805635));
#128956=CARTESIAN_POINT('Ctrl Pts',(7.4594685041631,1.83976484795739,0.784173577930784));
#128957=CARTESIAN_POINT('Ctrl Pts',(7.46088568678953,1.84202001047873,0.770188661514518));
#128958=CARTESIAN_POINT('Ctrl Pts',(7.46230286941607,1.844275173,0.756203745098238));
#128959=CARTESIAN_POINT('Ctrl Pts',(7.50347293199812,1.909789088,0.349932970050721));
#128960=CARTESIAN_POINT('Ctrl Pts',(7.50029312324209,1.975097379,-0.0584061115540076));
#128961=CARTESIAN_POINT('Ctrl Pts',(7.24760078043643,1.97432008472553,0.18650182808193));
#128962=CARTESIAN_POINT('Ctrl Pts',(7.28919168066759,1.96742614270402,0.187629540275795));
#128963=CARTESIAN_POINT('Ctrl Pts',(7.3308360723623,1.96070006936449,0.188736892956852));
#128964=CARTESIAN_POINT('Ctrl Pts',(7.41412740699392,1.94757342767362,0.190912187477736));
#128965=CARTESIAN_POINT('Ctrl Pts',(7.45582148176827,1.94116543744791,0.191981357371365));
#128966=CARTESIAN_POINT('Ctrl Pts',(7.49751541633979,1.93490817336454,0.193032549346399));
#128967=CARTESIAN_POINT('',(7.32344005060519,1.84427517216382,0.862105722358991));
#128968=CARTESIAN_POINT('Ctrl Pts',(7.24747755100001,1.975104983,0.191230626));
#128969=CARTESIAN_POINT('Ctrl Pts',(7.257927521,1.909367073,-0.204814342));
#128970=CARTESIAN_POINT('Ctrl Pts',(7.225159666,1.844275173,-0.599639729));
#128971=CARTESIAN_POINT('Ctrl Pts',(7.22483328017661,1.84362682194445,-0.603572406589943));
#128972=CARTESIAN_POINT('Ctrl Pts',(7.22450689435324,1.84297847088892,-0.607505084179886));
#128973=CARTESIAN_POINT('Ctrl Pts',(7.486869868,1.975104983,0.443598437));
#128974=CARTESIAN_POINT('Ctrl Pts',(7.511110706,1.909367073,0.03447166));
#128975=CARTESIAN_POINT('Ctrl Pts',(7.490626122,1.844275173,-0.374860382));
#128976=CARTESIAN_POINT('Ctrl Pts',(7.49042208429855,1.84362682194446,-0.378937553837025));
#128977=CARTESIAN_POINT('Ctrl Pts',(7.49021804659711,1.84297847088891,-0.383014725674051));
#128978=CARTESIAN_POINT('',(7.35789289421804,1.84427517246151,-0.487250052207402));
#128979=CARTESIAN_POINT('Ctrl Pts',(7.22740720595187,1.83976484778612,-0.572558743505817));
#128980=CARTESIAN_POINT('Ctrl Pts',(7.22628343597594,1.84202001039309,-0.586099236252907));
#128981=CARTESIAN_POINT('Ctrl Pts',(7.225159666,1.844275173,-0.599639729));
#128982=CARTESIAN_POINT('Ctrl Pts',(7.19251343,1.909789088,-0.992999697));
#128983=CARTESIAN_POINT('Ctrl Pts',(7.117355273,1.975097379,-1.380490461));
#128984=CARTESIAN_POINT('Ctrl Pts',(7.45364441441404,1.83976484778612,-0.837725190583261));
#128985=CARTESIAN_POINT('Ctrl Pts',(7.45202212045395,1.84202001039309,-0.85168780034889));
#128986=CARTESIAN_POINT('Ctrl Pts',(7.45039982649387,1.844275173,-0.865650410114524));
#128987=CARTESIAN_POINT('Ctrl Pts',(7.40327115014889,1.909789088,-1.2712731472771));
#128988=CARTESIAN_POINT('Ctrl Pts',(7.31238485124716,1.975097379,-1.66938192346314));
#128989=CARTESIAN_POINT('',(7.44993905510662,1.8442751723037,-0.865106217428465));
#128990=CARTESIAN_POINT('',(7.3637239637713,1.93490816643208,-1.42322463483128));
#128991=CARTESIAN_POINT('Origin',(-0.191098975792415,1.87499926932447,0.0271535804640089));
#128992=CARTESIAN_POINT('Ctrl Pts',(7.11824828163573,1.97432008472359,-1.37587841094358));
#128993=CARTESIAN_POINT('Ctrl Pts',(7.15910923470359,1.96742614268816,-1.38371787822969));
#128994=CARTESIAN_POINT('Ctrl Pts',(7.20001805197713,1.96070006933971,-1.39158872810979));
#128995=CARTESIAN_POINT('Ctrl Pts',(7.28182970572695,1.94757342767431,-1.40736946568964));
#128996=CARTESIAN_POINT('Ctrl Pts',(7.32277883618453,1.94116543747195,-1.41528828601095));
#128997=CARTESIAN_POINT('Ctrl Pts',(7.36372396503634,1.93490817340353,-1.42322463380124));
#128998=CARTESIAN_POINT('',(7.33754933848588,1.84427517216382,-0.732372961650914));
#128999=CARTESIAN_POINT('Origin',(3.17020715234761E-13,1.9359922270005,
-2.51534904016637E-14));
#129000=CARTESIAN_POINT('',(7.36262215996559,1.75423095990768,-1.42891389846464));
#129001=CARTESIAN_POINT('Origin',(-0.183524819945431,2.01767779273109,-0.0064615644315455));
#129002=CARTESIAN_POINT('',(7.23491554310284,1.84427517280771,-1.97635954850599));
#129003=CARTESIAN_POINT('Origin',(-0.18383269442569,1.87499310861105,0.0553417618074034));
#129004=CARTESIAN_POINT('Origin',(-0.188459740288789,2.01782134606628,0.0228757494982959));
#129005=CARTESIAN_POINT('Ctrl Pts',(7.119144485,1.975104983,-1.371233679));
#129006=CARTESIAN_POINT('Ctrl Pts',(7.04421218,1.909367073,-1.76026577));
#129007=CARTESIAN_POINT('Ctrl Pts',(6.927334631,1.844275173,-2.138816239));
#129008=CARTESIAN_POINT('Ctrl Pts',(6.9261704664532,1.84362682194445,-2.14258680947271));
#129009=CARTESIAN_POINT('Ctrl Pts',(6.92500630190641,1.84297847088892,-2.14635737994542));
#129010=CARTESIAN_POINT('Ctrl Pts',(7.407191563,1.975104983,-1.176228359));
#129011=CARTESIAN_POINT('Ctrl Pts',(7.3429155,1.909367073,-1.581001044));
#129012=CARTESIAN_POINT('Ctrl Pts',(7.23491554400001,1.844275173,-1.976359549));
#129013=CARTESIAN_POINT('Ctrl Pts',(7.23383980515275,1.84362682194445,-1.98029753673787));
#129014=CARTESIAN_POINT('Ctrl Pts',(7.2327640663055,1.84297847088892,-1.98423552447575));
#129015=CARTESIAN_POINT('',(7.08112508842076,1.84427517246151,-2.05758789083126));
#129016=CARTESIAN_POINT('Ctrl Pts',(6.93535123579539,1.83976484792752,-2.11285154735182));
#129017=CARTESIAN_POINT('Ctrl Pts',(6.93134293339768,1.84202001046379,-2.12583389317593));
#129018=CARTESIAN_POINT('Ctrl Pts',(6.927334631,1.844275173,-2.138816239));
#129019=CARTESIAN_POINT('Ctrl Pts',(6.810890881,1.909789088,-2.515961694));
#129020=CARTESIAN_POINT('Ctrl Pts',(6.65419082,1.975097379,-2.878236358));
#129021=CARTESIAN_POINT('Ctrl Pts',(7.09929619710389,1.83976484792752,-2.42045286383165));
#129022=CARTESIAN_POINT('Ctrl Pts',(7.09471028323739,1.84202001046379,-2.43374028985965));
#129023=CARTESIAN_POINT('Ctrl Pts',(7.09012436937103,1.844275173,-2.44702771588773));
#129024=CARTESIAN_POINT('Ctrl Pts',(6.95690063652932,1.909789088,-2.83303594606772));
#129025=CARTESIAN_POINT('Ctrl Pts',(6.7825575900873,1.975097379,-3.20229929207681));
#129026=CARTESIAN_POINT('',(7.08979135591328,1.8442751723037,-2.44639719391422));
#129027=CARTESIAN_POINT('',(6.88561296333098,1.93490816641965,-2.9729334158594));
#129028=CARTESIAN_POINT('Origin',(-0.180794007691721,1.87499927918276,0.0675994000123735));
#129029=CARTESIAN_POINT('Ctrl Pts',(6.65605440467582,1.97432008470038,-2.87392410442729));
#129030=CARTESIAN_POINT('Ctrl Pts',(6.69427479778625,1.967426142658,-2.89036418659408));
#129031=CARTESIAN_POINT('Ctrl Pts',(6.7325351897511,1.96070006929071,-2.90684520700082));
#129032=CARTESIAN_POINT('Ctrl Pts',(6.80904174041082,1.94757342763362,-2.93984408706496));
#129033=CARTESIAN_POINT('Ctrl Pts',(6.84733119051825,1.94116543745505,-2.95638062234516));
#129034=CARTESIAN_POINT('Ctrl Pts',(6.88561296479118,1.93490817339084,-2.97293341511763));
#129035=CARTESIAN_POINT('',(7.0085629743906,1.84427517216382,-2.29260670041997));
#129036=CARTESIAN_POINT('Origin',(8.08381139805192E-13,1.93599222699978,
-2.81892564846231E-13));
#129037=CARTESIAN_POINT('',(6.88331389561855,1.75423095987297,-2.9782528121271));
#129038=CARTESIAN_POINT('Origin',(-0.180623275883013,2.01767780073337,0.0331419700085889));
#129039=CARTESIAN_POINT('',(6.64090835621196,1.84427517280772,-3.48544634034117));
#129040=CARTESIAN_POINT('Origin',(-0.167638058107709,1.87499306230618,0.0935665359471533));
#129041=CARTESIAN_POINT('Origin',(-0.17913610751596,2.01782140902048,0.0628542123918951));
#129042=CARTESIAN_POINT('Ctrl Pts',(6.657928135,1.975104983,-2.869580621));
#129043=CARTESIAN_POINT('Ctrl Pts',(6.501117306,1.909367073,-3.233409128));
#129044=CARTESIAN_POINT('Ctrl Pts',(6.305595129,1.844275173,-3.577984079));
#129045=CARTESIAN_POINT('Ctrl Pts',(6.30364762078715,1.84362682194445,-3.58141623466291));
#129046=CARTESIAN_POINT('Ctrl Pts',(6.3017001125743,1.84297847088892,-3.58484839032582));
#129047=CARTESIAN_POINT('Ctrl Pts',(6.981161212,1.975104983,-2.741056025));
#129048=CARTESIAN_POINT('Ctrl Pts',(6.831373726,1.909367073,-3.122547895));
#129049=CARTESIAN_POINT('Ctrl Pts',(6.640908357,1.844275173,-3.485446341));
#129050=CARTESIAN_POINT('Ctrl Pts',(6.63901121737071,1.84362682194445,-3.48906100873161));
#129051=CARTESIAN_POINT('Ctrl Pts',(6.63711407774142,1.84297847088892,-3.49267567646322));
#129052=CARTESIAN_POINT('',(6.47325174458042,1.84427517246151,-3.53171520710327));
#129053=CARTESIAN_POINT('Ctrl Pts',(6.31900595189991,1.83976484771587,-3.55434975934237));
#129054=CARTESIAN_POINT('Ctrl Pts',(6.31230054044995,1.84202001035797,-3.56616691917117));
#129055=CARTESIAN_POINT('Ctrl Pts',(6.305595129,1.844275173,-3.577984079));
#129056=CARTESIAN_POINT('Ctrl Pts',(6.11079864400001,1.909789088,-3.921280119));
#129057=CARTESIAN_POINT('Ctrl Pts',(5.87988380000001,1.975097379,-4.241399121));
#129058=CARTESIAN_POINT('Ctrl Pts',(6.41299278012332,1.83976484771587,-3.8900028482065));
#129059=CARTESIAN_POINT('Ctrl Pts',(6.40565767820976,1.84202001035797,-3.90199378622383));
#129060=CARTESIAN_POINT('Ctrl Pts',(6.3983225762964,1.844275173,-3.91398472424112));
#129061=CARTESIAN_POINT('Ctrl Pts',(6.18523318118433,1.909789088,-4.26232913159854));
#129062=CARTESIAN_POINT('Ctrl Pts',(5.93558547398072,1.975097379,-4.58548070487765));
#129063=CARTESIAN_POINT('',(6.3981328920845,1.84427517230371,-3.91329735543593));
#129064=CARTESIAN_POINT('',(6.085538353362,1.93490816644465,-4.38363113444891));
#129065=CARTESIAN_POINT('Origin',(-0.162035375565994,1.87499924434966,0.104884392132654));
#129066=CARTESIAN_POINT('Ctrl Pts',(5.88263082197736,1.97432008474662,-4.23758830135794));
#129067=CARTESIAN_POINT('Ctrl Pts',(5.91642351171437,1.96742614268605,-4.26186027830983));
#129068=CARTESIAN_POINT('Ctrl Pts',(5.95024646467421,1.9607000693096,-4.28618083493031));
#129069=CARTESIAN_POINT('Ctrl Pts',(6.01787055070326,1.94757342765885,-4.33485486632169));
#129070=CARTESIAN_POINT('Ctrl Pts',(6.05170994853469,1.94116543746026,-4.35923588659744));
#129071=CARTESIAN_POINT('Ctrl Pts',(6.08553835493332,1.93490817341264,-4.38363113405725));
#129072=CARTESIAN_POINT('',(6.35186399537058,1.84427517216382,-3.74564069745897));
#129073=CARTESIAN_POINT('Origin',(-9.35015953551499E-13,1.9359922270005,
6.64832772168111E-13));
#129074=CARTESIAN_POINT('',(6.08214952384334,1.75423095986658,-4.38833193473268));
#129075=CARTESIAN_POINT('Origin',(-0.169275759552884,2.01767772774323,0.0711957342580904));
#129076=CARTESIAN_POINT('',(5.73637967537476,1.84427517280772,-4.83155753418558));
#129077=CARTESIAN_POINT('Origin',(-0.143604888526623,1.87499308571353,0.127416356990073));
#129078=CARTESIAN_POINT('Origin',(-0.161436088595061,2.01782137054624,0.0998935968133235));
#129079=CARTESIAN_POINT('Ctrl Pts',(5.885394466,1.975104983,-4.233749163));
#129080=CARTESIAN_POINT('Ctrl Pts',(5.654037413,1.909367073,-4.555361869));
#129081=CARTESIAN_POINT('Ctrl Pts',(5.389013006,1.844275173,-4.84984936));
#129082=CARTESIAN_POINT('Ctrl Pts',(5.3863732174238,1.84362682194446,-4.85278261706631));
#129083=CARTESIAN_POINT('Ctrl Pts',(5.3837334288476,1.84297847088891,-4.8557158741326));
#129084=CARTESIAN_POINT('Ctrl Pts',(6.228699522,1.975104983,-4.177714957));
#129085=CARTESIAN_POINT('Ctrl Pts',(6.00040450900001,1.909367073,-4.518087878));
#129086=CARTESIAN_POINT('Ctrl Pts',(5.736379676,1.844275173,-4.831557535));
#129087=CARTESIAN_POINT('Ctrl Pts',(5.73374984372954,1.84362682194446,-4.83467986485973));
#129088=CARTESIAN_POINT('Ctrl Pts',(5.73112001145909,1.84297847088891,-4.83780219471946));
#129089=CARTESIAN_POINT('',(5.56269634316618,1.84427517246151,-4.84070344501074));
#129090=CARTESIAN_POINT('Ctrl Pts',(5.40719096992761,1.83976484806293,-4.8296505296743));
#129091=CARTESIAN_POINT('Ctrl Pts',(5.39810198796378,1.8420200105315,-4.83974994483714));
#129092=CARTESIAN_POINT('Ctrl Pts',(5.389013006,1.844275173,-4.84984936));
#129093=CARTESIAN_POINT('Ctrl Pts',(5.124972255,1.909789088,-5.143243843));
#129094=CARTESIAN_POINT('Ctrl Pts',(4.830639948,1.975097379,-5.406238775));
#129095=CARTESIAN_POINT('Ctrl Pts',(5.42682494726768,1.83976484806292,-5.17766062628129));
#129096=CARTESIAN_POINT('Ctrl Pts',(5.41708363943925,1.8420200105315,-5.18779439196334));
#129097=CARTESIAN_POINT('Ctrl Pts',(5.40734233161094,1.844275173,-5.19792815764526));
#129098=CARTESIAN_POINT('Ctrl Pts',(5.12435109618326,1.909789088,-5.49232054523886));
#129099=CARTESIAN_POINT('Ctrl Pts',(4.81107197827115,1.975097379,-5.75425013667933));
#129100=CARTESIAN_POINT('',(5.40730484608771,1.8442751723037,-5.1972160827018));
#129101=CARTESIAN_POINT('',(5.00091073363334,1.93490816642164,-5.58935513343184));
#129102=CARTESIAN_POINT('Origin',(-0.135700172412214,1.87499929261683,0.137265238893015));
#129103=CARTESIAN_POINT('Ctrl Pts',(4.83414195973404,1.97432008473011,-5.40310757969719));
#129104=CARTESIAN_POINT('Ctrl Pts',(4.86192683762261,1.96742614269327,-5.4340765203924));
#129105=CARTESIAN_POINT('Ctrl Pts',(4.88973082789581,1.9607000693384,-5.46509941077988));
#129106=CARTESIAN_POINT('Ctrl Pts',(4.94531042243446,1.94757342766584,-5.5271726498645));
#129107=CARTESIAN_POINT('Ctrl Pts',(4.97311747527434,1.94116543745111,-5.5582581257389));
#129108=CARTESIAN_POINT('Ctrl Pts',(5.000910735254,1.93490817338302,-5.58935513338412));
#129109=CARTESIAN_POINT('',(5.39815891547351,1.84427517216382,-5.02353269878948));
#129110=CARTESIAN_POINT('Origin',(5.77229236631283E-13,1.93599222699989,
-5.20850723662036E-13));
#129111=CARTESIAN_POINT('',(4.9965905998539,1.75423095988625,-5.5932175331293));
#129112=CARTESIAN_POINT('Origin',(-0.150013602016426,2.01767780695757,0.105920921450683));
#129113=CARTESIAN_POINT('',(4.56362425617614,1.84427517280653,-5.95175046836297));
#129114=CARTESIAN_POINT('Origin',(-0.112856569995003,1.8749930938328,0.155308033179116));
#129115=CARTESIAN_POINT('Origin',(-0.136187621335671,2.01782136224198,0.132262112235459));
#129116=CARTESIAN_POINT('Ctrl Pts',(4.837666293,1.975104983,-5.3999523));
#129117=CARTESIAN_POINT('Ctrl Pts',(4.542581014,1.909367073,-5.664310951));
#129118=CARTESIAN_POINT('Ctrl Pts',(4.220446625,1.844275173,-5.894941076));
#129119=CARTESIAN_POINT('Ctrl Pts',(4.21723798965313,1.84362682194446,-5.89723827864708));
#129120=CARTESIAN_POINT('Ctrl Pts',(4.21402935430626,1.84297847088891,-5.89953548129417));
#129121=CARTESIAN_POINT('Ctrl Pts',(5.184990765,1.975104983,-5.419028581));
#129122=CARTESIAN_POINT('Ctrl Pts',(4.888863046,1.909367073,-5.702367093));
#129123=CARTESIAN_POINT('Ctrl Pts',(4.563624257,1.844275173,-5.951750469));
#129124=CARTESIAN_POINT('Ctrl Pts',(4.560384700125,1.84362682194446,-5.95423446432145));
#129125=CARTESIAN_POINT('Ctrl Pts',(4.55714514325,1.84297847088891,-5.95671845964291));
#129126=CARTESIAN_POINT('',(4.39203544365065,1.84427517246151,-5.9233457705346));
#129127=CARTESIAN_POINT('Ctrl Pts',(4.24254175093117,1.83976484781954,-5.87912220719468));
#129128=CARTESIAN_POINT('Ctrl Pts',(4.23149418796559,1.8420200104098,-5.88703164159738));
#129129=CARTESIAN_POINT('Ctrl Pts',(4.220446625,1.844275173,-5.894941076));
#129130=CARTESIAN_POINT('Ctrl Pts',(3.899507858,1.909789088,-6.124715202));
#129131=CARTESIAN_POINT('Ctrl Pts',(3.555520741,1.975097379,-6.318288713));
#129132=CARTESIAN_POINT('Ctrl Pts',(4.18690481276021,1.83976484781954,-6.22321674467366));
#129133=CARTESIAN_POINT('Ctrl Pts',(4.17521279062538,1.8420200104098,-6.23101949575683));
#129134=CARTESIAN_POINT('Ctrl Pts',(4.16352076849056,1.844275173,-6.23882224684012));
#129135=CARTESIAN_POINT('Ctrl Pts',(3.82386005061316,1.909789088,-6.46549715420862));
#129136=CARTESIAN_POINT('Ctrl Pts',(3.46159810449352,1.975097379,-6.65395722672367));
#129137=CARTESIAN_POINT('',(4.16363723442891,1.8442751723037,-6.23811876149708));
#129138=CARTESIAN_POINT('',(3.68244608643453,1.93490816646172,-6.53372709829258));
#129139=CARTESIAN_POINT('Origin',(-0.103019443528005,1.87499926512958,0.1632272891718));
#129140=CARTESIAN_POINT('Ctrl Pts',(3.55961399212249,1.97432008477344,-6.31598355143885));
#129141=CARTESIAN_POINT('Ctrl Pts',(3.58009186819303,1.96742614271751,-6.35220138327312));
#129142=CARTESIAN_POINT('Ctrl Pts',(3.60057681232157,1.96070006934248,-6.38847601203026));
#129143=CARTESIAN_POINT('Ctrl Pts',(3.64151307538492,1.94757342769032,-6.46104598332777));
#129144=CARTESIAN_POINT('Ctrl Pts',(3.66198755638972,1.94116543749851,-6.49738239239404));
#129145=CARTESIAN_POINT('Ctrl Pts',(3.68244608803867,1.93490817344443,-6.53372709859178));
#129146=CARTESIAN_POINT('',(4.19204192424133,1.84427517216382,-6.06652989444278));
#129147=CARTESIAN_POINT('Origin',(8.97719398817998E-14,1.93599222699945,
-2.86229373536173E-13));
#129148=CARTESIAN_POINT('',(3.67739665313504,1.7542309598772,-6.53657049652741));
#129149=CARTESIAN_POINT('Origin',(-0.123736379684608,2.01767771480689,0.135692840214087));
#129150=CARTESIAN_POINT('',(3.17747883877507,1.84427517280771,-6.79364616499826));
#129151=CARTESIAN_POINT('Origin',(-0.0768314298773742,1.87499312527885,
0.175937908447522));
#129152=CARTESIAN_POINT('Origin',(-0.104571309852137,2.01782136834141,0.158446457629746));
#129153=CARTESIAN_POINT('Ctrl Pts',(3.56373422,1.975104983,-6.313659668));
#129154=CARTESIAN_POINT('Ctrl Pts',(3.218718575,1.909367073,-6.508403149));
#129155=CARTESIAN_POINT('Ctrl Pts',(2.85453685,1.844275173,-6.664391898));
#129156=CARTESIAN_POINT('Ctrl Pts',(2.85090940010511,1.84362682194445,-6.66594563156849));
#129157=CARTESIAN_POINT('Ctrl Pts',(2.84728195021021,1.84297847088892,-6.66749936513699));
#129158=CARTESIAN_POINT('Ctrl Pts',(3.898837603,1.975104983,-6.40695445200001));
#129159=CARTESIAN_POINT('Ctrl Pts',(3.54872378,1.909367073,-6.62000996));
#129160=CARTESIAN_POINT('Ctrl Pts',(3.177478839,1.844275173,-6.793646166));
#129161=CARTESIAN_POINT('Ctrl Pts',(3.17378103559647,1.84362682194445,-6.7953756779276));
#129162=CARTESIAN_POINT('Ctrl Pts',(3.17008323219293,1.84297847088892,-6.79710518985521));
#129163=CARTESIAN_POINT('',(3.01600784751118,1.84427517246151,-6.72901903065036));
#129164=CARTESIAN_POINT('Ctrl Pts',(2.87951599392262,1.83976484771735,-6.65369266423465));
#129165=CARTESIAN_POINT('Ctrl Pts',(2.86702642196131,1.84202001035871,-6.65904228111732));
#129166=CARTESIAN_POINT('Ctrl Pts',(2.85453685,1.844275173,-6.664391898));
#129167=CARTESIAN_POINT('Ctrl Pts',(2.491706808,1.909789088,-6.819801685));
#129168=CARTESIAN_POINT('Ctrl Pts',(2.114149336,1.975097379,-6.934902493));
#129169=CARTESIAN_POINT('Ctrl Pts',(2.75120966161612,1.83976484771735,-6.97778216615797));
#129170=CARTESIAN_POINT('Ctrl Pts',(2.73811363134117,1.84202001035871,-6.98288905421602));
#129171=CARTESIAN_POINT('Ctrl Pts',(2.7250176010662,1.844275173,-6.98799594227393));
#129172=CARTESIAN_POINT('Ctrl Pts',(2.34456955773702,1.909789088,-7.13635430189462));
#129173=CARTESIAN_POINT('Ctrl Pts',(1.95026374963917,1.975097379,-7.24253267265233));
#129174=CARTESIAN_POINT('',(2.72528257265718,1.8442751723037,-6.98733394074222));
#129175=CARTESIAN_POINT('',(2.1917943525619,1.93490816642349,-7.17258924576138));
#129176=CARTESIAN_POINT('Origin',(-0.0655218890860726,1.87499927162194,
0.181557335832974));
#129177=CARTESIAN_POINT('Ctrl Pts',(2.1186424305649,1.97432008479257,-6.93353115305763));
#129178=CARTESIAN_POINT('Ctrl Pts',(2.13085578203134,1.96742614271259,-6.97330437001318));
#129179=CARTESIAN_POINT('Ctrl Pts',(2.14306382662412,1.96070006932251,-7.01313457545201));
#129180=CARTESIAN_POINT('Ctrl Pts',(2.16744262388015,1.94757342764595,-7.09280798748468));
#129181=CARTESIAN_POINT('Ctrl Pts',(2.17962716904188,1.94116543742711,-7.13269627976358));
#129182=CARTESIAN_POINT('Ctrl Pts',(2.19179435403524,1.93490817337569,-7.17258924640248));
#129183=CARTESIAN_POINT('',(2.78990971120828,1.84427517216382,-6.8258628944585));
#129184=CARTESIAN_POINT('Origin',(-1.52330405234213E-13,1.93599222700022,
4.20670442924376E-13));
#129185=CARTESIAN_POINT('',(2.18625172570706,1.75423095985805,-7.17428068787748));
#129186=CARTESIAN_POINT('Origin',(-0.0916735934150878,2.01767777303238,
0.159120217776577));
#129187=CARTESIAN_POINT('',(1.64275804250921,1.84427517280653,-7.31787851806874));
#129188=CARTESIAN_POINT('Origin',(-0.0372137556883542,1.87499310686471,
0.188341216210165));
#129189=CARTESIAN_POINT('Origin',(-0.0680652128771495,2.01782136026042,
0.17722188718693));
#129190=CARTESIAN_POINT('Ctrl Pts',(2.123165896,1.975104983,-6.932147328));
#129191=CARTESIAN_POINT('Ctrl Pts',(1.744352434,1.909367073,-7.048169649));
#129192=CARTESIAN_POINT('Ctrl Pts',(1.355152105,1.844275173,-7.122223162));
#129193=CARTESIAN_POINT('Ctrl Pts',(1.35127545607555,1.84362682194446,-7.12296077564041));
#129194=CARTESIAN_POINT('Ctrl Pts',(1.34739880715111,1.84297847088891,-7.12369838928083));
#129195=CARTESIAN_POINT('Ctrl Pts',(2.430379128,1.975104983,-7.095298253));
#129196=CARTESIAN_POINT('Ctrl Pts',(2.042650135,1.909367073,-7.228108519));
#129197=CARTESIAN_POINT('Ctrl Pts',(1.642758043,1.844275173,-7.317878519));
#129198=CARTESIAN_POINT('Ctrl Pts',(1.63877489824694,1.84362682194446,-7.31877267747834));
#129199=CARTESIAN_POINT('Ctrl Pts',(1.63479175349388,1.84297847088891,-7.31966683595668));
#129200=CARTESIAN_POINT('',(1.49895507723091,1.84427517246151,-7.22005083982923));
#129201=CARTESIAN_POINT('Ctrl Pts',(1.38184726753537,1.83976484802767,-7.11714384826785));
#129202=CARTESIAN_POINT('Ctrl Pts',(1.36849968626769,1.84202001051386,-7.11968350513391));
#129203=CARTESIAN_POINT('Ctrl Pts',(1.355152105,1.844275173,-7.122223162));
#129204=CARTESIAN_POINT('Ctrl Pts',(0.967396318,1.909789088,-7.196001821));
#129205=CARTESIAN_POINT('Ctrl Pts',(0.573922658000001,1.975097379,-7.22724794000001));
#129206=CARTESIAN_POINT('Ctrl Pts',(1.18687100372472,1.83976484802767,-7.4060742490486));
#129207=CARTESIAN_POINT('Ctrl Pts',(1.17298332230654,1.84202001051386,-7.4082464813648));
#129208=CARTESIAN_POINT('Ctrl Pts',(1.15909564088837,1.844275173,-7.41041871368114));
#129209=CARTESIAN_POINT('Ctrl Pts',(0.755649598499641,1.909789088,-7.47352345411848));
#129210=CARTESIAN_POINT('Ctrl Pts',(0.34773722962562,1.975097379,-7.49245534066952));
#129211=CARTESIAN_POINT('',(1.15949672832168,1.8442751723037,-7.4098291504801));
#129212=CARTESIAN_POINT('',(0.598656751323674,1.93490816637869,-7.47606909172004));
#129213=CARTESIAN_POINT('Origin',(-0.0249605442852397,1.87499930398572,
0.191397811646769));
#129214=CARTESIAN_POINT('Ctrl Pts',(0.578605504166122,1.97432008478999,
-7.22687454364312));
#129215=CARTESIAN_POINT('Ctrl Pts',(0.58198324830084,1.96742614270447,-7.26834339443569));
#129216=CARTESIAN_POINT('Ctrl Pts',(0.585343558780459,1.96070006930478,
-7.30986676053086));
#129217=CARTESIAN_POINT('Ctrl Pts',(0.592024964817653,1.94757342759785,
-7.39291817330326));
#129218=CARTESIAN_POINT('Ctrl Pts',(0.595349838294234,1.94116543741407,
-7.43449321620619));
#129219=CARTESIAN_POINT('Ctrl Pts',(0.598656752668666,1.93490817333718,
-7.47606909266033));
#129220=CARTESIAN_POINT('',(1.25732442189929,1.84427517216382,-7.26602613188263));
#129221=CARTESIAN_POINT('Origin',(3.98681467613654E-14,1.93599222699989,
-1.71087102818213E-12));
#129222=CARTESIAN_POINT('',(0.592880097740823,1.75423095986685,-7.47652948834918));
#129223=CARTESIAN_POINT('Origin',(-0.0553241390603929,2.0176777484641,0.175106894883671));
#129224=CARTESIAN_POINT('',(0.0312237062239616,1.84427517280772,-7.49993500399908));
#129225=CARTESIAN_POINT('Origin',(0.00414408988284653,1.87499310458502,
0.191937658090853));
#129226=CARTESIAN_POINT('Origin',(-0.0283764098568524,2.01782136553556,
0.187710425868436));
#129227=CARTESIAN_POINT('Ctrl Pts',(0.583320695,1.975104983,-7.226495483));
#129228=CARTESIAN_POINT('Ctrl Pts',(0.188422311,1.909367073,-7.25837157));
#129229=CARTESIAN_POINT('Ctrl Pts',(-0.207598047,1.844275173,-7.247027187));
#129230=CARTESIAN_POINT('Ctrl Pts',(-0.21154262715707,1.84362682194445,
-7.24691419071793));
#129231=CARTESIAN_POINT('Ctrl Pts',(-0.215487207314141,1.84297847088892,
-7.24680119443587));
#129232=CARTESIAN_POINT('Ctrl Pts',(0.848278826,1.975104983,-7.451873793));
#129233=CARTESIAN_POINT('Ctrl Pts',(0.44106444,1.909367073,-7.49822875700001));
#129234=CARTESIAN_POINT('Ctrl Pts',(0.031223706,1.844275173,-7.499935005));
#129235=CARTESIAN_POINT('Ctrl Pts',(0.027141467311413,1.84362682194445,
-7.49995200016671));
#129236=CARTESIAN_POINT('Ctrl Pts',(0.0230592286228261,1.84297847088892,
-7.49996899533341));
#129237=CARTESIAN_POINT('',(-0.0881871672004261,1.84427517246151,-7.37348109603946));
#129238=CARTESIAN_POINT('Ctrl Pts',(-0.180435098984076,1.83976484782248,
-7.24780529572746));
#129239=CARTESIAN_POINT('Ctrl Pts',(-0.194016572992038,1.84202001041127,
-7.24741624136368));
#129240=CARTESIAN_POINT('Ctrl Pts',(-0.207598047,1.844275173,-7.247027187));
#129241=CARTESIAN_POINT('Ctrl Pts',(-0.60214855,1.909789088,-7.23572490900001));
#129242=CARTESIAN_POINT('Ctrl Pts',(-0.993140006,1.975097379,-7.181655306));
#129243=CARTESIAN_POINT('Ctrl Pts',(-0.432964422026658,1.83976484782248,
-7.48806653106592));
#129244=CARTESIAN_POINT('Ctrl Pts',(-0.446994383495375,1.84202001041127,
-7.48720253677105));
#129245=CARTESIAN_POINT('Ctrl Pts',(-0.461024344964088,1.844275173,-7.4863385424761));
#129246=CARTESIAN_POINT('Ctrl Pts',(-0.868603695431265,1.909789088,-7.46123895582905));
#129247=CARTESIAN_POINT('Ctrl Pts',(-1.27104909583471,1.975097379,-7.39203912418675));
#129248=CARTESIAN_POINT('',(-0.460505896043215,1.84427517230371,-7.48584898484908));
#129249=CARTESIAN_POINT('',(-1.02247337458115,1.93490816642325,-7.42997625662627));
#129250=CARTESIAN_POINT('Origin',(0.0167678890584535,1.87499924426971,0.192288926901991));
#129251=CARTESIAN_POINT('Ctrl Pts',(-0.988486372994197,1.97432008480372,
-7.18229731285597));
#129252=CARTESIAN_POINT('Ctrl Pts',(-0.994102175903929,1.96742614273032,
-7.22352276015986));
#129253=CARTESIAN_POINT('Ctrl Pts',(-0.999746723954761,1.96070006934087,
-7.26479770050498));
#129254=CARTESIAN_POINT('Ctrl Pts',(-1.01107512422156,1.94757342765696,
-7.34734372224098));
#129255=CARTESIAN_POINT('Ctrl Pts',(-1.01676538966857,1.94116543745716,
-7.38866151343647));
#129256=CARTESIAN_POINT('Ctrl Pts',(-1.02247337348717,1.93490817338918,
-7.42997625783242));
#129257=CARTESIAN_POINT('',(-0.334051961171194,1.84427517216382,-7.3664380632655));
#129258=CARTESIAN_POINT('Origin',(-2.28224557308199E-14,1.93599222699978,
-2.59774840527527E-13));
#129259=CARTESIAN_POINT('',(-1.0282139448201,1.75423095989281,-7.42918407905391));
#129260=CARTESIAN_POINT('Origin',(-0.0163878639005517,2.01767778891665,
0.182906237919405));
#129261=CARTESIAN_POINT('',(-1.58177061555176,1.8442751728077,-7.33130286507962));
#129262=CARTESIAN_POINT('Origin',(0.0453081133266309,1.87499312495344,0.186559308706026));
#129263=CARTESIAN_POINT('Origin',(0.0126391854568975,2.01782138537541,0.189421789738689));
#129264=CARTESIAN_POINT('Ctrl Pts',(-0.983799934,1.975104983,-7.182940741));
#129265=CARTESIAN_POINT('Ctrl Pts',(-1.37631823,1.909367073,-7.129180104));
#129266=CARTESIAN_POINT('Ctrl Pts',(-1.760641144,1.844275173,-7.032968275));
#129267=CARTESIAN_POINT('Ctrl Pts',(-1.76446921119364,1.84362682194445,
-7.03200995236865));
#129268=CARTESIAN_POINT('Ctrl Pts',(-1.76829727838728,1.84297847088892,
-7.03105162973729));
#129269=CARTESIAN_POINT('Ctrl Pts',(-0.773486052000001,1.975104983,-7.460007998));
#129270=CARTESIAN_POINT('Ctrl Pts',(-1.181144938,1.909367073,-7.417740153));
#129271=CARTESIAN_POINT('Ctrl Pts',(-1.581770616,1.844275173,-7.33130286600001));
#129272=CARTESIAN_POINT('Ctrl Pts',(-1.58576106767231,1.84362682194445,
-7.3304419031726));
#129273=CARTESIAN_POINT('Ctrl Pts',(-1.58975151934463,1.84297847088892,
-7.3295809403452));
#129274=CARTESIAN_POINT('',(-1.67120587678606,1.84427517246151,-7.18213557124785));
#129275=CARTESIAN_POINT('Ctrl Pts',(-1.73428052152909,1.83976484791691,
-7.0395674227088));
#129276=CARTESIAN_POINT('Ctrl Pts',(-1.74746083276452,1.84202001045849,
-7.03626784885441));
#129277=CARTESIAN_POINT('Ctrl Pts',(-1.760641144,1.844275173,-7.032968275));
#129278=CARTESIAN_POINT('Ctrl Pts',(-2.14353762,1.909789088,-6.937113543));
#129279=CARTESIAN_POINT('Ctrl Pts',(-2.513764547,1.975097379,-6.800256451));
#129280=CARTESIAN_POINT('Ctrl Pts',(-2.0325549126968,1.83976484791691,-7.21992514398248));
#129281=CARTESIAN_POINT('Ctrl Pts',(-2.04607112796701,1.84202001045849,
-7.21606532247525));
#129282=CARTESIAN_POINT('Ctrl Pts',(-2.05958734323724,1.844275173,-7.21220550096806));
#129283=CARTESIAN_POINT('Ctrl Pts',(-2.45224204640514,1.909789088,-7.10007521612984));
#129284=CARTESIAN_POINT('Ctrl Pts',(-2.83040257861434,1.975097379,-6.94597937370433));
#129285=CARTESIAN_POINT('',(-2.0589757749614,1.8442751723037,-7.21183884013004));
#129286=CARTESIAN_POINT('',(-2.59579378182585,1.93490816644005,-7.0364659890224));
#129287=CARTESIAN_POINT('Origin',(0.0577123295222959,1.87499926002918,0.184188807617139));
#129288=CARTESIAN_POINT('Ctrl Pts',(-2.50935772659468,1.97432008481419,
-6.80188384193689));
#129289=CARTESIAN_POINT('Ctrl Pts',(-2.52370448738016,1.96742614276615,
-6.84093822952676));
#129290=CARTESIAN_POINT('Ctrl Pts',(-2.53808996090291,1.96070006940037,
-6.8800347736293));
#129291=CARTESIAN_POINT('Ctrl Pts',(-2.56689846390454,1.94757342770655,
-6.95821564414435));
#129292=CARTESIAN_POINT('Ctrl Pts',(-2.58133779786748,1.941165437491,-6.99734420955772));
#129293=CARTESIAN_POINT('Ctrl Pts',(-2.59579378101694,1.93490817341297,
-7.03646599043658));
#129294=CARTESIAN_POINT('',(-1.90980844449988,1.84427517216382,-7.12240353765932));
#129295=CARTESIAN_POINT('Origin',(2.32236105346395E-13,1.9359922269995,
5.42968447980741E-13));
#129296=CARTESIAN_POINT('',(-2.60122984629159,1.7542309598968,-7.03445827962168));
#129297=CARTESIAN_POINT('Origin',(0.0233147369726394,2.01767778271143,0.182153020485395));
#129298=CARTESIAN_POINT('',(-3.1208031028258,1.84427517280652,-6.81986715296561));
#129299=CARTESIAN_POINT('Origin',(0.0843535976500759,1.8749931240214,0.172457830983335));
#129300=CARTESIAN_POINT('Origin',(0.053063772342255,2.01782137990498,0.182276190606282));
#129301=CARTESIAN_POINT('Ctrl Pts',(-2.504919172,1.975104983,-6.803519673));
#129302=CARTESIAN_POINT('Ctrl Pts',(-2.87670366,1.909367073,-6.66663609900001));
#129303=CARTESIAN_POINT('Ctrl Pts',(-3.231358619,1.844275173,-6.490055583));
#129304=CARTESIAN_POINT('Ctrl Pts',(-3.23489117707591,1.84362682194445,
-6.48829674412855));
#129305=CARTESIAN_POINT('Ctrl Pts',(-3.23842373515182,1.84297847088892,
-6.48653790525708));
#129306=CARTESIAN_POINT('Ctrl Pts',(-2.359083581,1.975104983,-7.11932051900001));
#129307=CARTESIAN_POINT('Ctrl Pts',(-2.748125292,1.909367073,-6.99040626299999));
#129308=CARTESIAN_POINT('Ctrl Pts',(-3.120803103,1.844275173,-6.819867154));
#129309=CARTESIAN_POINT('Ctrl Pts',(-3.1245151785753,1.84362682194445,-6.81816849085864));
#129310=CARTESIAN_POINT('Ctrl Pts',(-3.12822725415059,1.84297847088892,
-6.81646982771727));
#129311=CARTESIAN_POINT('',(-3.17608085802196,1.84427517246151,-6.65496136992127));
#129312=CARTESIAN_POINT('Ctrl Pts',(-3.20703291362491,1.83976484767348,
-6.5021672015293));
#129313=CARTESIAN_POINT('Ctrl Pts',(-3.21919576631243,1.84202001033677,
-6.49611139226473));
#129314=CARTESIAN_POINT('Ctrl Pts',(-3.231358619,1.844275173,-6.490055583));
#129315=CARTESIAN_POINT('Ctrl Pts',(-3.584697254,1.909789088,-6.314130458));
#129316=CARTESIAN_POINT('Ctrl Pts',(-3.916848252,1.975097379,-6.100885163));
#129317=CARTESIAN_POINT('Ctrl Pts',(-3.53710539384575,1.83976484767348,
-6.61418808232894));
#129318=CARTESIAN_POINT('Ctrl Pts',(-3.54947586064107,1.84202001033677,
-6.60751291421119));
#129319=CARTESIAN_POINT('Ctrl Pts',(-3.56184632743642,1.844275173,-6.60083774609345));
#129320=CARTESIAN_POINT('Ctrl Pts',(-3.92121628480267,1.909789088,-6.40691985103178));
#129321=CARTESIAN_POINT('Ctrl Pts',(-4.2574095828665,1.975097379,-6.17513334692924));
#129322=CARTESIAN_POINT('',(-3.56117023600558,1.84427517230372,-6.60061112666912));
#129323=CARTESIAN_POINT('',(-4.04773775692025,1.93490816643309,-6.31393839224868));
#129324=CARTESIAN_POINT('Origin',(0.0959581384459198,1.8749992416038,0.167476038574007));
#129325=CARTESIAN_POINT('Ctrl Pts',(-3.91289430058519,1.97432008476561,
-6.10342184256812));
#129326=CARTESIAN_POINT('Ctrl Pts',(-3.93530118123749,1.96742614271418,
-6.13847903078324));
#129327=CARTESIAN_POINT('Ctrl Pts',(-3.95775493188805,1.96070006933818,
-6.17356906786166));
#129328=CARTESIAN_POINT('Ctrl Pts',(-4.00269648439312,1.94757342766985,
-6.24372913630939));
#129329=CARTESIAN_POINT('Ctrl Pts',(-4.02520971972781,1.94116543745747,
-6.27883886758349));
#129330=CARTESIAN_POINT('Ctrl Pts',(-4.0477377564473,1.93490817339409,-6.31393839379318));
#129331=CARTESIAN_POINT('',(-3.39626440859479,1.84427517216382,-6.54533333861584));
#129332=CARTESIAN_POINT('Origin',(-7.53737350311923E-13,1.9359922269995,
-1.12713657851593E-12));
#129333=CARTESIAN_POINT('',(-4.05261513072725,1.75423095989077,-6.31080902887057));
#129334=CARTESIAN_POINT('Origin',(0.0619271358873585,2.01767776407916,0.17288233858718));
#129335=CARTESIAN_POINT('',(-4.51391030460794,1.84427517280653,-5.98954203202318));
#129336=CARTESIAN_POINT('Origin',(0.119454723687895,1.87499306953623,0.150292257931243));
#129337=CARTESIAN_POINT('Origin',(0.0910073243481019,2.01782139378126,0.166607771974832));
#129338=CARTESIAN_POINT('Ctrl Pts',(-3.908911172,1.975104983,-6.105973587));
#129339=CARTESIAN_POINT('Ctrl Pts',(-4.242577624,1.909367073,-5.892367599));
#129340=CARTESIAN_POINT('Ctrl Pts',(-4.550981356,1.844275173,-5.643675106));
#129341=CARTESIAN_POINT('Ctrl Pts',(-4.55405322646585,1.84362682194445,
-5.64119799225248));
#129342=CARTESIAN_POINT('Ctrl Pts',(-4.5571250969317,1.84297847088892,-5.63872087850496));
#129343=CARTESIAN_POINT('Ctrl Pts',(-3.834372984,1.975104983,-6.445741526));
#129344=CARTESIAN_POINT('Ctrl Pts',(-4.186606361,1.909367073,-6.236208745));
#129345=CARTESIAN_POINT('Ctrl Pts',(-4.513910305,1.844275173,-5.989542033));
#129346=CARTESIAN_POINT('Ctrl Pts',(-4.51717043195245,1.84362682194445,
-5.98708509714327));
#129347=CARTESIAN_POINT('Ctrl Pts',(-4.52043055890489,1.84297847088892,
-5.98462816128654));
#129348=CARTESIAN_POINT('',(-4.53244582789712,1.84427517246151,-5.81660857152823));
#129349=CARTESIAN_POINT('Ctrl Pts',(-4.52982801346281,1.83976484797872,
-5.66073286810881));
#129350=CARTESIAN_POINT('Ctrl Pts',(-4.54040468473138,1.84202001048939,
-5.65220398705446));
#129351=CARTESIAN_POINT('Ctrl Pts',(-4.550981356,1.844275173,-5.643675106));
#129352=CARTESIAN_POINT('Ctrl Pts',(-4.858240429,1.909789088,-5.39590565));
#129353=CARTESIAN_POINT('Ctrl Pts',(-5.136784486,1.975097379,-5.116243265));
#129354=CARTESIAN_POINT('Ctrl Pts',(-4.87626476083307,1.83976484797873,
-5.69917893640965));
#129355=CARTESIAN_POINT('Ctrl Pts',(-4.88691104845316,1.84202001048939,
-5.6900005459186));
#129356=CARTESIAN_POINT('Ctrl Pts',(-4.89755733607325,1.844275173,-5.68082215542769));
#129357=CARTESIAN_POINT('Ctrl Pts',(-5.20683880866133,1.909789088,-5.41418403439199));
#129358=CARTESIAN_POINT('Ctrl Pts',(-5.48534484687944,1.975097379,-5.11554494932952));
#129359=CARTESIAN_POINT('',(-4.89684833486108,1.8442751723037,-5.68074617391997));
#129360=CARTESIAN_POINT('',(-5.31041401337923,1.93490816641524,-5.29617805429529));
#129361=CARTESIAN_POINT('Origin',(0.129717093787129,1.87499928879841,0.142932365974908));
#129362=CARTESIAN_POINT('Ctrl Pts',(-5.13346828674901,1.97432008473599,
-5.11957062121532));
#129363=CARTESIAN_POINT('Ctrl Pts',(-5.16288756611726,1.96742614269138,
-5.14899137500026));
#129364=CARTESIAN_POINT('Ctrl Pts',(-5.19235968126211,1.96070006931876,
-5.17843413396415));
#129365=CARTESIAN_POINT('Ctrl Pts',(-5.25133286608795,1.94757342764768,
-5.23729279388055));
#129366=CARTESIAN_POINT('Ctrl Pts',(-5.28086730880979,1.94116543745644,
-5.26674199900533));
#129367=CARTESIAN_POINT('Ctrl Pts',(-5.31041401323378,1.93490817338208,
-5.29617805592223));
#129368=CARTESIAN_POINT('',(-4.72391482347484,1.84427517216382,-5.66221062818384));
#129369=CARTESIAN_POINT('Origin',(1.17657619758127E-12,1.935992227,1.09547787507935E-12));
#129370=CARTESIAN_POINT('',(-5.31450463659943,1.75423095987771,-5.29207336206581));
#129371=CARTESIAN_POINT('Origin',(0.0976439592437239,2.01767779117054,0.155528002201123));
#129372=CARTESIAN_POINT('',(-5.69595207709764,1.84427517280772,-4.87915258250815));
#129373=CARTESIAN_POINT('Origin',(0.148970427177585,1.87499306971534,0.121099350130393));
#129374=CARTESIAN_POINT('Origin',(0.124695325715196,2.01782141253908,0.143148641268627));
#129375=CARTESIAN_POINT('Ctrl Pts',(-5.130126831,1.975104983,-5.122918962));
#129376=CARTESIAN_POINT('Ctrl Pts',(-5.410073373,1.909367073,-4.84257854));
#129377=CARTESIAN_POINT('Ctrl Pts',(-5.657805263,1.844275173,-4.533402653));
#129378=CARTESIAN_POINT('Ctrl Pts',(-5.66027280861433,1.84362682194445,
-4.53032309144649));
#129379=CARTESIAN_POINT('Ctrl Pts',(-5.66274035422866,1.84297847088892,
-4.52724352989297));
#129380=CARTESIAN_POINT('Ctrl Pts',(-5.130371368,1.975104983,-5.470766823));
#129381=CARTESIAN_POINT('Ctrl Pts',(-5.42932637000001,1.909367073,-5.190413038));
#129382=CARTESIAN_POINT('Ctrl Pts',(-5.695952078,1.844275173,-4.879152583));
#129383=CARTESIAN_POINT('Ctrl Pts',(-5.69860781641318,1.84362682194445,
-4.8760522580049));
#129384=CARTESIAN_POINT('Ctrl Pts',(-5.70126355482636,1.84297847088892,
-4.87295193300981));
#129385=CARTESIAN_POINT('',(-5.67687866839398,1.84427517246151,-4.70627762054036));
#129386=CARTESIAN_POINT('Ctrl Pts',(-5.64081338858096,1.83976484799314,
-4.55460895740009));
#129387=CARTESIAN_POINT('Ctrl Pts',(-5.64930932579043,1.8420200104966,-4.54400580520006));
#129388=CARTESIAN_POINT('Ctrl Pts',(-5.657805263,1.844275173,-4.533402653));
#129389=CARTESIAN_POINT('Ctrl Pts',(-5.90461768,1.909789088,-4.225374291));
#129390=CARTESIAN_POINT('Ctrl Pts',(-6.11653038600001,1.975097379,-3.892371519));
#129391=CARTESIAN_POINT('Ctrl Pts',(-5.98741540489952,1.83976484799315,
-4.51768251699911));
#129392=CARTESIAN_POINT('Ctrl Pts',(-5.99583970555893,1.8420200104966,-4.50643007508651));
#129393=CARTESIAN_POINT('Ctrl Pts',(-6.00426400621848,1.844275173,-4.49517763317383));
#129394=CARTESIAN_POINT('Ctrl Pts',(-6.24899533556163,1.909789088,-4.16828698919722));
#129395=CARTESIAN_POINT('Ctrl Pts',(-6.45679148257349,1.975097379,-3.81675935454026));
#129396=CARTESIAN_POINT('',(-6.00355524728374,1.8442751723037,-4.49525584237545));
#129397=CARTESIAN_POINT('',(-6.32478121248456,1.93490816642691,-4.03077431595155));
#129398=CARTESIAN_POINT('Origin',(0.157410688850646,1.87499926823127,0.111705409770206));
#129399=CARTESIAN_POINT('Ctrl Pts',(-6.11400700101207,1.97432008478699,
-3.89633396802979));
#129400=CARTESIAN_POINT('Ctrl Pts',(-6.14906306633504,1.96742614273179,
-3.91874260539025));
#129401=CARTESIAN_POINT('Ctrl Pts',(-6.18417546265735,1.96070006935083,
-3.94116137532613));
#129402=CARTESIAN_POINT('Ctrl Pts',(-6.25442275922522,1.94757342766965,
-3.98596646072418));
#129403=CARTESIAN_POINT('Ctrl Pts',(-6.28959741168097,1.94116543747655,
-4.00837812750807));
#129404=CARTESIAN_POINT('Ctrl Pts',(-6.32478121269039,1.93490817340087,
-4.03077431757664));
#129405=CARTESIAN_POINT('',(-5.83068023116903,1.84427517216382,-4.5143292409069));
#129406=CARTESIAN_POINT('Origin',(-5.48172618408671E-13,1.93599222700028,
-3.3133218391157E-13));
#129407=CARTESIAN_POINT('',(-6.32789381150226,1.75423095987766,-4.02588622653618));
#129408=CARTESIAN_POINT('Origin',(0.128794683593468,2.01767775631336,0.130901045922478));
#129409=CARTESIAN_POINT('',(-6.61165746100905,1.84427517280771,-3.54061938074093));
#129410=CARTESIAN_POINT('Origin',(0.171520220308146,1.87499311130849,0.0862437827628504));
#129411=CARTESIAN_POINT('Origin',(0.152552479145713,2.01782135366553,0.112995927333402));
#129412=CARTESIAN_POINT('Ctrl Pts',(-6.111463461,1.975104983,-3.90032234));
#129413=CARTESIAN_POINT('Ctrl Pts',(-6.324600105,1.909367073,-3.56635589));
#129414=CARTESIAN_POINT('Ctrl Pts',(-6.500076484,1.844275173,-3.21115333));
#129415=CARTESIAN_POINT('Ctrl Pts',(-6.50182432506083,1.84362682194445,
-3.20761531751753));
#129416=CARTESIAN_POINT('Ctrl Pts',(-6.50357216612167,1.84297847088892,
-3.20407730503506));
#129417=CARTESIAN_POINT('Ctrl Pts',(-6.186479288,1.975104983,-4.239985143));
#129418=CARTESIAN_POINT('Ctrl Pts',(-6.418177113,1.909367073,-3.901919385));
#129419=CARTESIAN_POINT('Ctrl Pts',(-6.611657462,1.844275173,-3.540619381));
#129420=CARTESIAN_POINT('Ctrl Pts',(-6.61358463248514,1.84362682194445,
-3.53702063462816));
#129421=CARTESIAN_POINT('Ctrl Pts',(-6.61551180297026,1.84297847088892,
-3.53342188825632));
#129422=CARTESIAN_POINT('',(-6.55586697148932,1.84427517246151,-3.3758863584337));
#129423=CARTESIAN_POINT('Ctrl Pts',(-6.48804059799724,1.83976484770246,
-3.23551659508166));
#129424=CARTESIAN_POINT('Ctrl Pts',(-6.49405854099866,1.84202001035126,
-3.22333496254083));
#129425=CARTESIAN_POINT('Ctrl Pts',(-6.500076484,1.844275173,-3.21115333));
#129426=CARTESIAN_POINT('Ctrl Pts',(-6.674901571,1.909789088,-2.857269126));
#129427=CARTESIAN_POINT('Ctrl Pts',(-6.810274123,1.975097379,-2.486496806));
#129428=CARTESIAN_POINT('Ctrl Pts',(-6.81860115874642,1.83976484770246,
-3.12494428663886));
#129429=CARTESIAN_POINT('Ctrl Pts',(-6.82440956191935,1.84202001035126,
-3.11214394413541));
#129430=CARTESIAN_POINT('Ctrl Pts',(-6.83021796509225,1.844275173,-3.09934360163201));
#129431=CARTESIAN_POINT('Ctrl Pts',(-6.99895578627246,1.909789088,-2.72748547813659));
#129432=CARTESIAN_POINT('Ctrl Pts',(-7.12632572387792,1.975097379,-2.33950633402682));
#129433=CARTESIAN_POINT('',(-6.82954258916494,1.84427517230372,-3.09957234458067));
#129434=CARTESIAN_POINT('',(-7.04340867139713,1.93490816642142,-2.57689605099186));
#129435=CARTESIAN_POINT('Origin',(0.177743741960253,1.87499924246271,0.0752551014249897));
#129436=CARTESIAN_POINT('Ctrl Pts',(-6.80866154308647,1.97432008477238,
-2.49090906827571));
#129437=CARTESIAN_POINT('Ctrl Pts',(-6.84771521168073,1.96742614270981,
-2.50525778639195));
#129438=CARTESIAN_POINT('Ctrl Pts',(-6.88682607247638,1.96070006933242,
-2.51960429070294));
#129439=CARTESIAN_POINT('Ctrl Pts',(-6.96506279519489,1.94757342765555,
-2.54826076597791));
#129440=CARTESIAN_POINT('Ctrl Pts',(-7.00423292981718,1.94116543744924,
-2.56258695004634));
#129441=CARTESIAN_POINT('Ctrl Pts',(-7.04340867195185,1.93490817338345,
-2.57689605251758));
#129442=CARTESIAN_POINT('',(-6.66480951171505,1.84427517216382,-3.15536283582134));
#129443=CARTESIAN_POINT('Origin',(-9.29811783123569E-13,1.93599222699928,
-3.15069151324288E-13));
#129444=CARTESIAN_POINT('',(-7.04539770509782,1.75423095989962,-2.57145312556847));
#129445=CARTESIAN_POINT('Origin',(0.153923849122756,2.01767775774706,0.100153790920415));
#129446=CARTESIAN_POINT('',(-7.21820909110488,1.84427517280653,-2.03653075247311));
#129447=CARTESIAN_POINT('Origin',(0.186050156972235,1.87499306391399,0.047355726206694));
#129448=CARTESIAN_POINT('Origin',(0.173276963324477,2.01782136225575,0.0775599770843804));
#129449=CARTESIAN_POINT('Ctrl Pts',(-6.807034852,1.975104983,-2.495350981));
#129450=CARTESIAN_POINT('Ctrl Pts',(-6.943395564,1.909367073,-2.123374403));
#129451=CARTESIAN_POINT('Ctrl Pts',(-7.038411352,1.844275173,-1.738754046));
#129452=CARTESIAN_POINT('Ctrl Pts',(-7.03935776140644,1.84362682194445,
-1.7349230161108));
#129453=CARTESIAN_POINT('Ctrl Pts',(-7.04030417081289,1.84297847088892,
-1.73109198622161));
#129454=CARTESIAN_POINT('Ctrl Pts',(-6.953314313,1.975104983,-2.810946471));
#129455=CARTESIAN_POINT('Ctrl Pts',(-7.106921026,1.909367073,-2.430976319));
#129456=CARTESIAN_POINT('Ctrl Pts',(-7.21820909200001,1.844275173,-2.036530753));
#129457=CARTESIAN_POINT('Ctrl Pts',(-7.21931758222782,1.84362682194445,
-2.03260185863572));
#129458=CARTESIAN_POINT('Ctrl Pts',(-7.22042607245565,1.84297847088892,
-2.02867296427143));
#129459=CARTESIAN_POINT('',(-7.12831022115529,1.84427517246151,-1.88764240268987));
#129460=CARTESIAN_POINT('Ctrl Pts',(-7.03189424239342,1.83976484928362,
-1.76513506195534));
#129461=CARTESIAN_POINT('Ctrl Pts',(-7.0351527971967,1.84202001114184,-1.75194455397764));
#129462=CARTESIAN_POINT('Ctrl Pts',(-7.038411352,1.844275173,-1.738754046));
#129463=CARTESIAN_POINT('Ctrl Pts',(-7.13307448300001,1.909789088,-1.355561232));
#129464=CARTESIAN_POINT('Ctrl Pts',(-7.185577012,1.975097379,-0.964356266));
#129465=CARTESIAN_POINT('Ctrl Pts',(-7.33095670468933,1.83976484928362,
-1.58608712354138));
#129466=CARTESIAN_POINT('Ctrl Pts',(-7.33387761430758,1.84202001114184,
-1.57233741574218));
#129467=CARTESIAN_POINT('Ctrl Pts',(-7.33679852392583,1.844275173,-1.55858770794298));
#129468=CARTESIAN_POINT('Ctrl Pts',(-7.42165284325518,1.909789088,-1.15914977635031));
#129469=CARTESIAN_POINT('Ctrl Pts',(-7.46264089599617,1.975097379,-0.752860597832355));
#129470=CARTESIAN_POINT('',(-7.33618811052153,1.84427517230371,-1.55895628908607));
#129471=CARTESIAN_POINT('',(-7.43269416961486,1.9349081664758,-1.00252499180948));
#129472=CARTESIAN_POINT('Origin',(0.189766226780289,1.87499935596518,0.0352860788185521));
#129473=CARTESIAN_POINT('Ctrl Pts',(-7.18495063902355,1.97432008477277,
-0.969012029225634));
#129474=CARTESIAN_POINT('Ctrl Pts',(-7.22617580490572,1.96742614269331,
-0.97462989791423));
#129475=CARTESIAN_POINT('Ctrl Pts',(-7.26745634996787,1.96070006929825,
-0.980233309935613));
#129476=CARTESIAN_POINT('Ctrl Pts',(-7.35002423663735,1.94757342763221,
-0.991401229963115));
#129477=CARTESIAN_POINT('Ctrl Pts',(-7.39135830166391,1.94116543738299,
-0.996972054759698));
#129478=CARTESIAN_POINT('Ctrl Pts',(-7.43269417065052,1.93490817334005,
-1.002524991835));
#129479=CARTESIAN_POINT('',(-7.18729970665748,1.84427517216382,-1.64885517145456));
#129480=CARTESIAN_POINT('Ctrl Pts',(-7.184316859,1.975104983,-0.973699783));
#129481=CARTESIAN_POINT('Ctrl Pts',(-7.237525565,1.909367073,-0.581106288000001));
#129482=CARTESIAN_POINT('Ctrl Pts',(-7.24763792900001,1.844275173,-0.185052556));
#129483=CARTESIAN_POINT('Ctrl Pts',(-7.24773865369652,1.84362682194445,
-0.181107643419569));
#129484=CARTESIAN_POINT('Ctrl Pts',(-7.24783937839304,1.84297847088892,
-0.177162730839138));
#129485=CARTESIAN_POINT('Ctrl Pts',(-7.39502008900001,1.975104983,-1.250471066));
#129486=CARTESIAN_POINT('Ctrl Pts',(-7.463353212,1.909367073,-0.846363502));
#129487=CARTESIAN_POINT('Ctrl Pts',(-7.487245287,1.844275173,-0.437216209));
#129488=CARTESIAN_POINT('Ctrl Pts',(-7.48748326518231,1.84362682194445,
-0.433140877364431));
#129489=CARTESIAN_POINT('Ctrl Pts',(-7.48772124336463,1.84297847088892,
-0.429065545728861));
#129490=CARTESIAN_POINT('',(-7.48724528278758,1.84427517281017,-0.437216207964299));
#129491=CARTESIAN_POINT('Origin',(0.185898732641985,2.01782134991888,0.0384971496779662));
#129492=CARTESIAN_POINT('',(-7.36744160786082,1.8442751724617,-0.311134385795709));
#129493=CARTESIAN_POINT('Origin',(1.83447007584547E-13,1.93599222699972,
1.10859672136643E-13));
#129494=CARTESIAN_POINT('',(-7.43346663215192,1.75423095987132,-0.996781734801308));
#129495=CARTESIAN_POINT('Origin',(0.171855021166949,2.01767774414194,0.0647231140259243));
#129496=CARTESIAN_POINT('Origin',(0.19187885663823,1.87499240687786,0.00625317968707198));
#129497=CARTESIAN_POINT('Ctrl Pts',(-7.24694432414292,1.83976484770062,
-0.212217793924953));
#129498=CARTESIAN_POINT('Ctrl Pts',(-7.2472911265714,1.84202001035034,-0.198635174962476));
#129499=CARTESIAN_POINT('Ctrl Pts',(-7.24763792900001,1.844275173,-0.185052556));
#129500=CARTESIAN_POINT('Ctrl Pts',(-7.257712761,1.909789088,0.209531198));
#129501=CARTESIAN_POINT('Ctrl Pts',(-7.224890305,1.975097379,0.602876501));
#129502=CARTESIAN_POINT('Ctrl Pts',(-7.50052485709175,1.83976484770062,
0.0269336922108996));
#129503=CARTESIAN_POINT('Ctrl Pts',(-7.50042169673789,1.84202001035034,
0.0409898536246645));
#129504=CARTESIAN_POINT('Ctrl Pts',(-7.50031853638406,1.844275173,0.0550460150384293));
#129505=CARTESIAN_POINT('Ctrl Pts',(-7.49732166223242,1.909789088,0.463386479627454));
#129506=CARTESIAN_POINT('Ctrl Pts',(-7.45001127264835,1.975097379,0.868988062514227));
#129507=CARTESIAN_POINT('',(-7.49980162846453,1.84427517230371,0.0545548305699198));
#129508=CARTESIAN_POINT('',(-7.3737197555458,1.84427517216382,-0.0652488718236939));
#129509=CARTESIAN_POINT('',(-7.47443514884404,1.93490816642042,0.618723024003911));
#129510=CARTESIAN_POINT('Origin',(0.192914594014201,1.87499925147378,-0.00633297397302638));
#129511=CARTESIAN_POINT('Ctrl Pts',(-7.22527942811084,1.97432008477231,
0.59819493566734));
#129512=CARTESIAN_POINT('Ctrl Pts',(-7.26674844815987,1.96742614272921,
0.601570601553237));
#129513=CARTESIAN_POINT('Ctrl Pts',(-7.30826844486245,1.96070006936509,
0.604972290993));
#129514=CARTESIAN_POINT('Ctrl Pts',(-7.39130671311814,1.94757342767871,
0.611815125446106));
#129515=CARTESIAN_POINT('Ctrl Pts',(-7.43287197311172,1.94116543746252,
0.615260145461762));
#129516=CARTESIAN_POINT('Ctrl Pts',(-7.47443514998797,1.93490817338182,
0.618723022852726));
#129517=CARTESIAN_POINT('Origin',(1.31405303305243E-13,1.93599222699994,
-8.93856928578518E-14));
#129518=CARTESIAN_POINT('',(-7.40618621304167,1.84427517280771,1.18254207762937));
#129519=CARTESIAN_POINT('Origin',(0.189828273627123,2.01782140642892,-0.00236555032836309));
#129520=CARTESIAN_POINT('',(-7.47395492142815,1.75423095988376,0.62449806323406));
#129521=CARTESIAN_POINT('Origin',(0.181750375798407,2.01767778599679,0.0262662027630737));
#129522=CARTESIAN_POINT('Origin',(0.188738899843145,1.87499310194232,-0.0351415693773048));
#129523=CARTESIAN_POINT('Ctrl Pts',(-7.225668194,1.975104983,0.593480535));
#129524=CARTESIAN_POINT('Ctrl Pts',(-7.193236914,1.909367073,0.988333711));
#129525=CARTESIAN_POINT('Ctrl Pts',(-7.117973011,1.844275173,1.377301786));
#129526=CARTESIAN_POINT('Ctrl Pts',(-7.11722334121076,1.84362682194446,
1.38117612154711));
#129527=CARTESIAN_POINT('Ctrl Pts',(-7.11647367142152,1.84297847088891,
1.38505045709422));
#129528=CARTESIAN_POINT('Ctrl Pts',(-7.490942944,1.975104983,0.368474977));
#129529=CARTESIAN_POINT('Ctrl Pts',(-7.470807296,1.909367073,0.777824331));
#129530=CARTESIAN_POINT('Ctrl Pts',(-7.406186214,1.844275173,1.182542078));
#129531=CARTESIAN_POINT('Ctrl Pts',(-7.40554255255019,1.84362682194446,
1.18657328892585));
#129532=CARTESIAN_POINT('Ctrl Pts',(-7.40489889110037,1.84297847088891,
1.19060449985171));
#129533=CARTESIAN_POINT('',(-7.26207961307277,1.8442751724615,1.27992192875023));
#129534=CARTESIAN_POINT('Ctrl Pts',(-7.12313534524776,1.83976484781228,
1.35062255237286));
#129535=CARTESIAN_POINT('Ctrl Pts',(-7.12055417812381,1.84202001040617,
1.36396216918644));
#129536=CARTESIAN_POINT('Ctrl Pts',(-7.117973011,1.844275173,1.377301786));
#129537=CARTESIAN_POINT('Ctrl Pts',(-7.042988456,1.909789088,1.764826182));
#129538=CARTESIAN_POINT('Ctrl Pts',(-6.926375758,1.975097379,2.141919433));
#129539=CARTESIAN_POINT('Ctrl Pts',(-7.31937680634634,1.83976484781228,
1.63869512780091));
#129540=CARTESIAN_POINT('Ctrl Pts',(-7.31625439866584,1.84202001040617,
1.65240048722346));
#129541=CARTESIAN_POINT('Ctrl Pts',(-7.31313199098535,1.844275173,1.66610584664601));
#129542=CARTESIAN_POINT('Ctrl Pts',(-7.22242405181757,1.909789088,2.06425529924396));
#129543=CARTESIAN_POINT('Ctrl Pts',(-7.08902740285667,1.975097379,2.45020380704269));
#129544=CARTESIAN_POINT('',(-7.31273275824016,1.8442751723037,1.6655150258936));
#129545=CARTESIAN_POINT('',(-7.16667984767001,1.93490816644713,2.21104023792926));
#129546=CARTESIAN_POINT('Origin',(0.187043282828443,1.8749992713524,-0.0476559397633659));
#129547=CARTESIAN_POINT('Ctrl Pts',(-6.92776218226152,1.97432008467218,
2.13743097000644));
#129548=CARTESIAN_POINT('Ctrl Pts',(-6.96753601105857,1.96742614267118,
2.14964232808322));
#129549=CARTESIAN_POINT('Ctrl Pts',(-7.00735403038993,1.96070006934577,
2.16189005982757));
#129550=CARTESIAN_POINT('Ctrl Pts',(-7.08697986235771,1.94757343434173,
2.18642367327992));
#129551=CARTESIAN_POINT('Ctrl Pts',(-7.12683272412762,1.94116545135372,
2.19872343805099));
#129552=CARTESIAN_POINT('Ctrl Pts',(-7.16667984902619,1.93490817340589,
2.211040237077));
#129553=CARTESIAN_POINT('',(-7.21535286393197,1.84427517216381,1.52140839206518));
#129554=CARTESIAN_POINT('Origin',(3.06612374378901E-13,1.93599222699956,
-2.61617984220752E-13));
#129555=CARTESIAN_POINT('',(-7.16496938547227,1.75423095987033,2.216577024765));
#129556=CARTESIAN_POINT('Origin',(0.183147693307631,2.01767775526487,-0.0134188668528029));
#129557=CARTESIAN_POINT('',(-6.97882210397126,1.84427517280652,2.74700601187666));
#129558=CARTESIAN_POINT('Origin',(0.176771704887981,1.87499304877816,-0.0748931927939472));
#129559=CARTESIAN_POINT('Origin',(0.184881712020416,2.01782137571191,-0.0431177300554872));
#129560=CARTESIAN_POINT('Ctrl Pts',(-6.929155316,1.975104983,2.132910362));
#129561=CARTESIAN_POINT('Ctrl Pts',(-6.81260049900001,1.909367073,2.511560324));
#129562=CARTESIAN_POINT('Ctrl Pts',(-6.655479587,1.844275173,2.875255027));
#129563=CARTESIAN_POINT('Ctrl Pts',(-6.65391457646654,1.84362682194446,
2.87887762588843));
#129564=CARTESIAN_POINT('Ctrl Pts',(-6.65234956593308,1.84297847088891,
2.88250022477685));
#129565=CARTESIAN_POINT('Ctrl Pts',(-7.236597633,1.975104983,1.970191539));
#129566=CARTESIAN_POINT('Ctrl Pts',(-7.128934734,1.909367073,2.365641964));
#129567=CARTESIAN_POINT('Ctrl Pts',(-6.978822105,1.844275173,2.747006012));
#129568=CARTESIAN_POINT('Ctrl Pts',(-6.97732690081234,1.84362682194446,
2.75080460726404));
#129569=CARTESIAN_POINT('Ctrl Pts',(-6.97583169662468,1.84297847088891,
2.75460320252807));
#129570=CARTESIAN_POINT('',(-6.81715084725798,1.8442751724615,2.81113051644934));
#129571=CARTESIAN_POINT('Ctrl Pts',(-6.66625647519525,1.83976484790778,
2.85030928883513));
#129572=CARTESIAN_POINT('Ctrl Pts',(-6.66086803109762,1.84202001045392,
2.86278215791755));
#129573=CARTESIAN_POINT('Ctrl Pts',(-6.655479587,1.844275173,2.875255027));
#129574=CARTESIAN_POINT('Ctrl Pts',(-6.49894183800001,1.909789088,3.237599855));
#129575=CARTESIAN_POINT('Ctrl Pts',(-6.30399157900001,1.975097379,3.580808593));
#129576=CARTESIAN_POINT('Ctrl Pts',(-6.79598283116813,1.83976484790778,
3.17383300112513));
#129577=CARTESIAN_POINT('Ctrl Pts',(-6.78998717662345,1.84202001045392,
3.18654671124277));
#129578=CARTESIAN_POINT('Ctrl Pts',(-6.7839915220787,1.844275173,3.19926042136032));
#129579=CARTESIAN_POINT('Ctrl Pts',(-6.60981392104711,1.909789088,3.56860183554046));
#129580=CARTESIAN_POINT('Ctrl Pts',(-6.39656849030963,1.975097379,3.91685074512989));
#129581=CARTESIAN_POINT('',(-6.78372863217671,1.8442751723037,3.1985975904431));
#129582=CARTESIAN_POINT('',(-6.52381856217684,1.93490816641423,3.69997166723722));
#129583=CARTESIAN_POINT('Origin',(0.17242549256259,1.87499928258689,-0.0867504515316227));
#129584=CARTESIAN_POINT('Ctrl Pts',(-6.30631047561054,1.97432008478727,
3.57672310740659));
#129585=CARTESIAN_POINT('Ctrl Pts',(-6.34252933352834,1.96742614270498,
3.59719916832535));
#129586=CARTESIAN_POINT('Ctrl Pts',(-6.37878352963317,1.96070006931012,
3.61772025216601));
#129587=CARTESIAN_POINT('Ctrl Pts',(-6.4512737889157,1.94757342762861,3.65879750425718));
#129588=CARTESIAN_POINT('Ctrl Pts',(-6.48755087065177,1.94116543743315,
3.67937691934155));
#129589=CARTESIAN_POINT('Ctrl Pts',(-6.52381856370022,1.93490817337558,
3.69997166666959));
#129590=CARTESIAN_POINT('',(-6.71960409236808,1.84427517216381,3.03692629071717));
#129591=CARTESIAN_POINT('Origin',(1.40469233467222E-12,1.93599222700022,
-7.65013052905772E-13));
#129592=CARTESIAN_POINT('',(-6.52095784408861,1.75423095986924,3.70501130874087));
#129593=CARTESIAN_POINT('Origin',(0.175981522065984,2.01767778536792,-0.0524766778138985));
#129594=CARTESIAN_POINT('',(-6.22513603000557,1.84427517280653,4.18302299766104));
#129595=CARTESIAN_POINT('Origin',(0.156539136163832,1.87499309963404,-0.111142978868746));
#129596=CARTESIAN_POINT('Origin',(0.171290313807868,2.01782138396538,-0.0818538011439141));
#129597=CARTESIAN_POINT('Ctrl Pts',(-6.308642835,1.975104983,3.572607672));
#129598=CARTESIAN_POINT('Ctrl Pts',(-6.113414457,1.909367073,3.917349167));
#129599=CARTESIAN_POINT('Ctrl Pts',(-5.881783334,1.844275173,4.238764539));
#129600=CARTESIAN_POINT('Ctrl Pts',(-5.87947616086335,1.84362682194446,
4.24196601254285));
#129601=CARTESIAN_POINT('Ctrl Pts',(-5.87716898772669,1.84297847088891,
4.24516748608571));
#129602=CARTESIAN_POINT('Ctrl Pts',(-6.643877059,1.975104983,3.479784134));
#129603=CARTESIAN_POINT('Ctrl Pts',(-6.453721107,1.909367073,3.842844807));
#129604=CARTESIAN_POINT('Ctrl Pts',(-6.225136031,1.844275173,4.183022998));
#129605=CARTESIAN_POINT('Ctrl Pts',(-6.22285919816356,1.84362682194446,
4.18641135951976));
#129606=CARTESIAN_POINT('Ctrl Pts',(-6.22058236532713,1.84297847088891,
4.18979972103951));
#129607=CARTESIAN_POINT('',(-6.05345968438437,1.8442751724615,4.21089376579109));
#129608=CARTESIAN_POINT('Ctrl Pts',(-5.89767086073434,1.83976484792964,
4.21671873080049));
#129609=CARTESIAN_POINT('Ctrl Pts',(-5.88972709736717,1.84202001046485,
4.22774163490021));
#129610=CARTESIAN_POINT('Ctrl Pts',(-5.881783334,1.844275173,4.238764539));
#129611=CARTESIAN_POINT('Ctrl Pts',(-5.651011924,1.909789088,4.558986958));
#129612=CARTESIAN_POINT('Ctrl Pts',(-5.386839759,1.975097379,4.852263122));
#129613=CARTESIAN_POINT('Ctrl Pts',(-5.95481625195012,1.83976484792964,
4.56056597055263));
#129614=CARTESIAN_POINT('Ctrl Pts',(-5.94622770064011,1.84202001046485,
4.57169355263703));
#129615=CARTESIAN_POINT('Ctrl Pts',(-5.93763914933008,1.844275173,4.5828211347213));
#129616=CARTESIAN_POINT('Ctrl Pts',(-5.68813623691231,1.909789088,4.90608451616743));
#129617=CARTESIAN_POINT('Ctrl Pts',(-5.40501314457735,1.975097379,5.20035009539286));
#129618=CARTESIAN_POINT('',(-5.93752489475053,1.84427517230362,4.58211728676164));
#129619=CARTESIAN_POINT('',(-5.57591077120322,1.93490816643902,5.01589653422082));
#129620=CARTESIAN_POINT('Origin',(0.149745580527058,1.87499928425088,-0.12178873420025));
#129621=CARTESIAN_POINT('Ctrl Pts',(-5.38998270015481,1.97432008470267,
4.84877164788896));
#129622=CARTESIAN_POINT('Ctrl Pts',(-5.4209530333933,1.96742614267996,4.87655497353722));
#129623=CARTESIAN_POINT('Ctrl Pts',(-5.45194819995815,1.96070006933894,
4.90438986621784));
#129624=CARTESIAN_POINT('Ctrl Pts',(-5.5139132822696,1.94757342768204,4.96009001806846));
#129625=CARTESIAN_POINT('Ctrl Pts',(-5.54491826017082,1.94116543746585,
4.98798679832514));
#129626=CARTESIAN_POINT('Ctrl Pts',(-5.57591077280683,1.93490817340487,
5.01589653400181));
#129627=CARTESIAN_POINT('',(-5.90965410140387,1.84427517216381,4.41044089164858));
#129628=CARTESIAN_POINT('Origin',(-7.24247051220317E-13,1.93599222699922,
5.2432017061399E-13));
#129629=CARTESIAN_POINT('',(-5.57203356127325,1.75423095987769,5.02020338153605));
#129630=CARTESIAN_POINT('Origin',(0.160586504670851,2.01767779640965,-0.0890808571676227));
#129631=CARTESIAN_POINT('',(-5.18036951346625,1.84427517280771,5.42344647712285));
#129632=CARTESIAN_POINT('Origin',(0.12898694124733,1.87499308356648,-0.142195858114513));
#129633=CARTESIAN_POINT('Origin',(0.149689335412058,2.01782137334422,-0.116762313732693));
#129634=CARTESIAN_POINT('Ctrl Pts',(-5.393145228,1.975104983,4.845253817));
#129635=CARTESIAN_POINT('Ctrl Pts',(-5.128371949,1.909367073,5.139967117));
#129636=CARTESIAN_POINT('Ctrl Pts',(-4.833061429,1.844275173,5.404074132));
#129637=CARTESIAN_POINT('Ctrl Pts',(-4.83011997411306,1.84362682194446,
5.40670478284829));
#129638=CARTESIAN_POINT('Ctrl Pts',(-4.82717851922612,1.84297847088891,
5.40933543369657));
#129639=CARTESIAN_POINT('Ctrl Pts',(-5.740496178,1.975104983,4.826665891));
#129640=CARTESIAN_POINT('Ctrl Pts',(-5.476738654,1.909367073,5.14036049900001));
#129641=CARTESIAN_POINT('Ctrl Pts',(-5.180369514,1.844275173,5.423446478));
#129642=CARTESIAN_POINT('Ctrl Pts',(-5.17741751467674,1.84362682194446,
5.42626616974804));
#129643=CARTESIAN_POINT('Ctrl Pts',(-5.17446551535348,1.84297847088891,
5.42908586149607));
#129644=CARTESIAN_POINT('',(-5.00671547392265,1.8442751724615,5.4137603027595));
#129645=CARTESIAN_POINT('Ctrl Pts',(-4.85331671130139,1.83976484792442,
5.38595909115377));
#129646=CARTESIAN_POINT('Ctrl Pts',(-4.84318907015065,1.84202001046224,
5.39501661157687));
#129647=CARTESIAN_POINT('Ctrl Pts',(-4.83306142900001,1.844275173,5.404074132));
#129648=CARTESIAN_POINT('Ctrl Pts',(-4.538846972,1.909789088,5.667200897));
#129649=CARTESIAN_POINT('Ctrl Pts',(-4.2178053,1.975097379,5.896831221));
#129650=CARTESIAN_POINT('Ctrl Pts',(-4.83520908217589,1.83976484792441,
5.73405194302275));
#129651=CARTESIAN_POINT('Ctrl Pts',(-4.82442922520848,1.84202001046224,
5.74307308379315));
#129652=CARTESIAN_POINT('Ctrl Pts',(-4.81364936824105,1.844275173,5.75209422456359));
#129653=CARTESIAN_POINT('Ctrl Pts',(-4.50048762435396,1.909789088,6.01416413737017));
#129654=CARTESIAN_POINT('Ctrl Pts',(-4.1607253913209,1.975097379,6.2406868555797));
#129655=CARTESIAN_POINT('',(-4.81368909130657,1.8442751723037,5.75138227091392));
#129656=CARTESIAN_POINT('',(-4.36727958982717,1.93490816641456,6.09728365358735));
#129657=CARTESIAN_POINT('Origin',(0.120063566074309,1.87499928118574,-0.151132151585901));
#129658=CARTESIAN_POINT('Ctrl Pts',(-4.2216253242295,1.97432008482041,5.89409701454771));
#129659=CARTESIAN_POINT('Ctrl Pts',(-4.24589899453292,1.9674261427479,5.9278884878857));
#129660=CARTESIAN_POINT('Ctrl Pts',(-4.27018583224409,1.96070006935906,
5.96173566104478));
#129661=CARTESIAN_POINT('Ctrl Pts',(-4.31872831918151,1.94757342765911,
6.02945423542534));
#129662=CARTESIAN_POINT('Ctrl Pts',(-4.34301143469336,1.94116543745499,
6.06336395806756));
#129663=CARTESIAN_POINT('Ctrl Pts',(-4.367279591454,1.93490817337971,6.0972836537083));
#129664=CARTESIAN_POINT('',(-4.82337525208443,1.84427517216381,5.57772817788601));
#129665=CARTESIAN_POINT('Origin',(3.03576608295941E-15,1.9359922269995,
6.37510877421477E-14));
#129666=CARTESIAN_POINT('',(-4.36256718233698,1.75423095984561,6.10065632351581));
#129667=CARTESIAN_POINT('Origin',(0.137681771613398,2.01767770434297,-0.121518839677397));
#129668=CARTESIAN_POINT('',(-3.89337467666301,1.84427517280772,6.41027562702946));
#129669=CARTESIAN_POINT('Origin',(0.0954033633209667,1.87499309498197,-0.166599734341152));
#129670=CARTESIAN_POINT('Origin',(0.121089346307142,2.01782136500259,-0.146211421620384));
#129671=CARTESIAN_POINT('Ctrl Pts',(-4.225470143,1.975104983,5.891341279));
#129672=CARTESIAN_POINT('Ctrl Pts',(-3.903532469,1.909367073,6.122245918));
#129673=CARTESIAN_POINT('Ctrl Pts',(-3.558350943,1.844275173,6.316695225));
#129674=CARTESIAN_POINT('Ctrl Pts',(-3.55491274551712,1.84362682194446,
6.31863204683871));
#129675=CARTESIAN_POINT('Ctrl Pts',(-3.55147454803423,1.84297847088891,
6.32056886867742));
#129676=CARTESIAN_POINT('Ctrl Pts',(-4.568696076,1.975104983,5.947858115));
#129677=CARTESIAN_POINT('Ctrl Pts',(-4.243669988,1.909367073,6.197518646));
#129678=CARTESIAN_POINT('Ctrl Pts',(-3.893374677,1.844275173,6.410275628));
#129679=CARTESIAN_POINT('Ctrl Pts',(-3.88988554341135,1.84362682194446,
6.41239480433152));
#129680=CARTESIAN_POINT('Ctrl Pts',(-3.88639640982271,1.84297847088891,
6.41451398066305));
#129681=CARTESIAN_POINT('',(-3.72586281284765,1.8442751724615,6.36348542483268));
#129682=CARTESIAN_POINT('Ctrl Pts',(-3.58202686786243,1.8397648476387,6.30335798985825));
#129683=CARTESIAN_POINT('Ctrl Pts',(-3.57018890543119,1.84202001031938,
6.31002660742913));
#129684=CARTESIAN_POINT('Ctrl Pts',(-3.558350943,1.844275173,6.316695225));
#129685=CARTESIAN_POINT('Ctrl Pts',(-3.21445058,1.909789088,6.510422821));
#129686=CARTESIAN_POINT('Ctrl Pts',(-2.851550952,1.975097379,6.665670046));
#129687=CARTESIAN_POINT('Ctrl Pts',(-3.48951291167448,1.8397648476387,6.63942001909199));
#129688=CARTESIAN_POINT('Ctrl Pts',(-3.47704580241671,1.84202001031938,
6.64591290042925));
#129689=CARTESIAN_POINT('Ctrl Pts',(-3.46457869315892,1.844275173,6.65240578176653));
#129690=CARTESIAN_POINT('Ctrl Pts',(-3.10240121335745,1.909789088,6.84102812803436));
#129691=CARTESIAN_POINT('Ctrl Pts',(-2.72188674349151,1.975097379,6.98921603451046));
#129692=CARTESIAN_POINT('',(-3.46477053652249,1.84427517230371,6.65171901243283));
#129693=CARTESIAN_POINT('',(-2.95443926928893,1.93490816641705,6.89356856655105));
#129694=CARTESIAN_POINT('Origin',(0.0847675782078298,1.87499924514342,-0.173408794056555));
#129695=CARTESIAN_POINT('Ctrl Pts',(-2.85586943983058,1.97432008474088,
6.6638209567827));
#129696=CARTESIAN_POINT('Ctrl Pts',(-2.87231143740344,1.96742614270362,
6.70204052568845));
#129697=CARTESIAN_POINT('Ctrl Pts',(-2.88875432072029,1.96070006935415,
6.74031732275798));
#129698=CARTESIAN_POINT('Ctrl Pts',(-2.92160441985889,1.94757342767156,
6.81688787426888));
#129699=CARTESIAN_POINT('Ctrl Pts',(-2.93803022184158,1.94116543744954,
6.85522495862428));
#129700=CARTESIAN_POINT('Ctrl Pts',(-2.95443927083686,1.93490817337398,
6.89356856702391));
#129701=CARTESIAN_POINT('',(-3.51156073694809,1.84427517216381,6.48420709396512));
#129702=CARTESIAN_POINT('Origin',(5.48172618408671E-13,1.93599222700033,
-1.30581309654154E-12));
#129703=CARTESIAN_POINT('',(-2.94911201030461,1.75423095990399,6.89584935679358));
#129704=CARTESIAN_POINT('Origin',(0.108340146961858,2.01767777290915,-0.148275807789205));
#129705=CARTESIAN_POINT('',(-2.42432996691648,1.84427517280609,7.09736741297175));
#129706=CARTESIAN_POINT('Origin',(0.0573589000589378,1.87499309175534,-0.183213729321554));
#129707=CARTESIAN_POINT('Origin',(0.0868271630715356,2.0178213733533,-0.168823616204068));
#129708=CARTESIAN_POINT('Ctrl Pts',(-2.860216771,1.975104983,6.66195617100001));
#129709=CARTESIAN_POINT('Ctrl Pts',(-2.496168149,1.909367073,6.818255304));
#129710=CARTESIAN_POINT('Ctrl Pts',(-2.117255923,1.844275173,6.933954669));
#129711=CARTESIAN_POINT('Ctrl Pts',(-2.11348174922899,1.84362682194446,
6.9351070981874));
#129712=CARTESIAN_POINT('Ctrl Pts',(-2.10970757545798,1.84297847088891,
6.93625952737481));
#129713=CARTESIAN_POINT('Ctrl Pts',(-3.183268824,1.975104983,6.790935105));
#129714=CARTESIAN_POINT('Ctrl Pts',(-2.812172031,1.909367073,6.96488771));
#129715=CARTESIAN_POINT('Ctrl Pts',(-2.424329967,1.844275173,7.097367414));
#129716=CARTESIAN_POINT('Ctrl Pts',(-2.42046684714056,1.84362682194446,
7.09868698457524));
#129717=CARTESIAN_POINT('Ctrl Pts',(-2.41660372728113,1.84297847088891,
7.10000655515048));
#129718=CARTESIAN_POINT('',(-2.27079294816725,1.84427517245675,7.01566104047484));
#129719=CARTESIAN_POINT('Ctrl Pts',(-2.1432454269271,1.83976484804352,6.92601887564033));
#129720=CARTESIAN_POINT('Ctrl Pts',(-2.13025067496355,1.84202001052179,
6.92998677232021));
#129721=CARTESIAN_POINT('Ctrl Pts',(-2.117255923,1.844275173,6.933954669));
#129722=CARTESIAN_POINT('Ctrl Pts',(-1.739750052,1.909789088,7.04922461));
#129723=CARTESIAN_POINT('Ctrl Pts',(-1.351961251,1.975097379,7.122829548));
#129724=CARTESIAN_POINT('Ctrl Pts',(-1.98065099273836,1.83976484804352,
7.23433619666886));
#129725=CARTESIAN_POINT('Ctrl Pts',(-1.96707958119578,1.84202001052179,
7.23799721771154));
#129726=CARTESIAN_POINT('Ctrl Pts',(-1.95350816965328,1.844275173,7.24165823875426));
#129727=CARTESIAN_POINT('Ctrl Pts',(-1.5592499683863,1.909789088,7.34801324586424));
#129728=CARTESIAN_POINT('Ctrl Pts',(-1.15577569678679,1.975097379,7.41093723892653));
#129729=CARTESIAN_POINT('',(-1.95384316290116,1.8442751723037,7.24102876641797));
#129730=CARTESIAN_POINT('',(-1.40345265154337,1.93490816642678,7.36751787427784));
#129731=CARTESIAN_POINT('Origin',(0.0455080576337361,1.87499926986637,-0.187577469996594));
#129732=CARTESIAN_POINT('Ctrl Pts',(-1.35657627490455,1.9743200846916,7.12195203649257));
#129733=CARTESIAN_POINT('Ctrl Pts',(-1.36441779022587,1.9674261426747,7.16281259655497));
#129734=CARTESIAN_POINT('Ctrl Pts',(-1.37224786815185,1.96070006933634,
7.20372923723952));
#129735=CARTESIAN_POINT('Ctrl Pts',(-1.38786954499056,1.94757342767207,
7.28557141204423));
#129736=CARTESIAN_POINT('Ctrl Pts',(-1.39566998086786,1.94116543746633,
7.32654325846433));
#129737=CARTESIAN_POINT('Ctrl Pts',(-1.4034526529648,1.93490817339425,7.36751787507186));
#129738=CARTESIAN_POINT('',(-2.03554954552458,1.84427517216381,7.08749169292896));
#129739=CARTESIAN_POINT('Origin',(4.55364912443912E-15,1.93599222699994,
-1.80844922370582E-13));
#129740=CARTESIAN_POINT('',(-1.39775963854105,1.75423095988713,7.36860013786871));
#129741=CARTESIAN_POINT('Origin',(0.0739322772112747,2.01767774345327,-0.168099117039335));
#129742=CARTESIAN_POINT('',(-0.841926282128371,1.8442751728077,7.45259418698405));
#129743=CARTESIAN_POINT('Origin',(0.01663228595669,1.87499309352602,-0.191260385054375));
#129744=CARTESIAN_POINT('Origin',(0.0485051041280235,2.01782134416412,-0.183541901016625));
#129745=CARTESIAN_POINT('Ctrl Pts',(-1.361222842,1.975104983,7.121065396));
#129746=CARTESIAN_POINT('Ctrl Pts',(-0.972085781,1.909367073,7.19545065));
#129747=CARTESIAN_POINT('Ctrl Pts',(-0.577160368,1.844275173,7.2269901));
#129748=CARTESIAN_POINT('Ctrl Pts',(-0.573226694096189,1.84362682194446,
7.22730425023526));
#129749=CARTESIAN_POINT('Ctrl Pts',(-0.569293020192376,1.84297847088891,
7.22761840047053));
#129750=CARTESIAN_POINT('Ctrl Pts',(-1.648995459,1.975104983,7.316475516));
#129751=CARTESIAN_POINT('Ctrl Pts',(-1.249180034,1.909367073,7.406586365));
#129752=CARTESIAN_POINT('Ctrl Pts',(-0.841926282,1.844275173,7.452594188));
#129753=CARTESIAN_POINT('Ctrl Pts',(-0.837869811072231,1.84362682194446,
7.45305245117261));
#129754=CARTESIAN_POINT('Ctrl Pts',(-0.833813340144462,1.84297847088891,
7.45351071434522));
#129755=CARTESIAN_POINT('',(-0.709543328284545,1.8442751724615,7.33979214368248));
#129756=CARTESIAN_POINT('Origin',(-3.72694496791892E-14,1.93599222700011,
5.42101086242752E-14));
#129757=CARTESIAN_POINT('',(0.218950416952298,1.75423096007169,7.49680336637767));
#129758=CARTESIAN_POINT('',(-0.351556253986197,1.8442751723037,7.49175606294591));
#129759=CARTESIAN_POINT('Origin',(0.0360674549391415,2.01767783439293,-0.180062609324158));
#129760=CARTESIAN_POINT('Origin',(-0.0248718942039444,1.87499308268038,
-0.190364284420828));
#129761=CARTESIAN_POINT('Origin',(0.00412048493843249,1.87499926526327,
-0.192974814822687));
#129762=CARTESIAN_POINT('Ctrl Pts',(-0.604248213242546,1.83976484794618,
7.22482681617143));
#129763=CARTESIAN_POINT('Ctrl Pts',(-0.59070429062127,1.84202001047312,
7.22590845808572));
#129764=CARTESIAN_POINT('Ctrl Pts',(-0.577160368,1.844275173,7.2269901));
#129765=CARTESIAN_POINT('Ctrl Pts',(-0.183700746,1.909789088,7.25841249));
#129766=CARTESIAN_POINT('Ctrl Pts',(0.210844655,1.975097379,7.246933457));
#129767=CARTESIAN_POINT('Ctrl Pts',(-0.379176036910304,1.83976484794618,
7.49098285274321));
#129768=CARTESIAN_POINT('Ctrl Pts',(-0.365134905824976,1.84202001047312,
7.49164082883958));
#129769=CARTESIAN_POINT('Ctrl Pts',(-0.351093774739651,1.844275173,7.49229880493583));
#129770=CARTESIAN_POINT('Ctrl Pts',(0.0568100714185217,1.909789088,7.51141343172169));
#129771=CARTESIAN_POINT('Ctrl Pts',(0.464378137235999,1.975097379,7.48613125413578));
#129772=CARTESIAN_POINT('',(-0.464358318833719,1.84427517216381,7.35937305782598));
#129773=CARTESIAN_POINT('Ctrl Pts',(-1.160767276,4.042807359,7.409630175));
#129774=CARTESIAN_POINT('Ctrl Pts',(-0.754367972,3.977102825,7.473295298));
#129775=CARTESIAN_POINT('Ctrl Pts',(-0.343443638,3.912499672,7.49213230400001));
#129776=CARTESIAN_POINT('Ctrl Pts',(-1.356373314,4.042807359,7.121990693));
#129777=CARTESIAN_POINT('Ctrl Pts',(-0.965750302,3.977102825,7.196384307));
#129778=CARTESIAN_POINT('Ctrl Pts',(-0.569334295,3.912499672,7.22761084000001));
#129779=CARTESIAN_POINT('',(-0.595762404227082,3.95233946559532,7.47630027399342));
#129780=CARTESIAN_POINT('Ctrl Pts',(-0.595762404863384,3.95233945647622,
7.47630027530279));
#129781=CARTESIAN_POINT('Ctrl Pts',(-0.592182366064195,3.94612348982327,
7.43474870639099));
#129782=CARTESIAN_POINT('Ctrl Pts',(-0.588581597117314,3.93976379156922,
7.39319744671796));
#129783=CARTESIAN_POINT('Ctrl Pts',(-0.581342220634875,3.9267491041166,
7.31018955732445));
#129784=CARTESIAN_POINT('Ctrl Pts',(-0.577699717669751,3.92008711220508,
7.2686882076048));
#129785=CARTESIAN_POINT('Ctrl Pts',(-0.574036078608516,3.91326598549935,
7.22723893645966));
#129786=CARTESIAN_POINT('',(-1.16076727022619,4.04280736030966,7.40963015407995));
#129787=CARTESIAN_POINT('Origin',(0.0475501136360631,4.16063865198492,-0.181696116530682));
#129788=CARTESIAN_POINT('',(-1.25857027269469,4.04280736269456,7.26581043786369));
#129789=CARTESIAN_POINT('Ctrl Pts',(-2.42647005212533,3.912491975,7.09718410019861));
#129790=CARTESIAN_POINT('Ctrl Pts',(-2.04152351657078,3.97753138,7.22879421861146));
#129791=CARTESIAN_POINT('Ctrl Pts',(-1.64460027740355,4.042807359,7.31799624221166));
#129792=CARTESIAN_POINT('Ctrl Pts',(-1.63094216828536,4.0450535022237,7.3210656794521));
#129793=CARTESIAN_POINT('Ctrl Pts',(-1.61728405916712,4.04729964544735,
7.32413511669249));
#129794=CARTESIAN_POINT('Ctrl Pts',(-2.118733935,3.912491975,6.933503192));
#129795=CARTESIAN_POINT('Ctrl Pts',(-1.742665343,3.97753138,7.048421908));
#129796=CARTESIAN_POINT('Ctrl Pts',(-1.356373314,4.042807359,7.121990693));
#129797=CARTESIAN_POINT('Ctrl Pts',(-1.34308102430026,4.04505350222369,
7.12452219126988));
#129798=CARTESIAN_POINT('Ctrl Pts',(-1.32978873460052,4.04729964544735,
7.12705368953974));
#129799=CARTESIAN_POINT('',(-1.64401284267851,4.04280735814476,7.31759679238927));
#129800=CARTESIAN_POINT('',(-1.50019304561873,4.04280735744341,7.21979371444933));
#129801=CARTESIAN_POINT('',(-2.18901737117743,3.95233946528201,7.17343722208511));
#129802=CARTESIAN_POINT('Origin',(0.046198773551316,4.01785666264986,-0.187368441160566));
#129803=CARTESIAN_POINT('Ctrl Pts',(-2.11425816787987,3.91326598475539,
6.93486931359651));
#129804=CARTESIAN_POINT('Ctrl Pts',(-2.12674657908886,3.9200871429414,6.97456213285606));
#129805=CARTESIAN_POINT('Ctrl Pts',(-2.13922555207015,3.92674916804717,
7.01431038548526));
#129806=CARTESIAN_POINT('Ctrl Pts',(-2.1641397865704,3.93976378656247,7.09382092338471));
#129807=CARTESIAN_POINT('Ctrl Pts',(-2.17658865449891,3.94612348023444,
7.13362664806682));
#129808=CARTESIAN_POINT('Ctrl Pts',(-2.18901737207597,3.95233945645758,
7.17343722318243));
#129809=CARTESIAN_POINT('Ctrl Pts',(-2.726480643,4.042807359,6.986866487));
#129810=CARTESIAN_POINT('Ctrl Pts',(-2.343268848,3.977102825,7.136406991));
#129811=CARTESIAN_POINT('Ctrl Pts',(-1.946001096,3.912499672,7.243140185));
#129812=CARTESIAN_POINT('Ctrl Pts',(-2.855679535,4.042807359,6.66390234));
#129813=CARTESIAN_POINT('Ctrl Pts',(-2.4901815,3.977102825,6.820529074));
#129814=CARTESIAN_POINT('Ctrl Pts',(-2.109746259,3.912499672,6.936243271));
#129815=CARTESIAN_POINT('',(-2.72648063280564,4.04280736030989,6.98686646784853));
#129816=CARTESIAN_POINT('Origin',(0.0854978739401674,4.16063868872144,-0.167226751539388));
#129817=CARTESIAN_POINT('',(-2.79172606251171,4.04280736269456,6.82376960133532));
#129818=CARTESIAN_POINT('Origin',(-4.35849273339173E-14,4.13463032199956,
3.13984949151802E-13));
#129819=CARTESIAN_POINT('',(-2.19152447942122,4.13354310062559,7.17267177917869));
#129820=CARTESIAN_POINT('Origin',(0.0602927793603003,4.16070813241699,-0.182368014149964));
#129821=CARTESIAN_POINT('Origin',(0.0735723243195169,4.0178646340646,-0.177487496657471));
#129822=CARTESIAN_POINT('Ctrl Pts',(-3.89542532178459,3.912491975,6.40963654487194));
#129823=CARTESIAN_POINT('Ctrl Pts',(-3.54777090689269,3.97753138,6.62092181788924));
#129824=CARTESIAN_POINT('Ctrl Pts',(-3.17930331128518,4.042807359,6.79336511074186));
#129825=CARTESIAN_POINT('Ctrl Pts',(-3.16662435976257,4.04505350217026,
6.79929887581794));
#129826=CARTESIAN_POINT('Ctrl Pts',(-3.15394540823987,4.04729964534048,
6.80523264089403));
#129827=CARTESIAN_POINT('Ctrl Pts',(-3.559697347,3.912491975,6.315936573));
#129828=CARTESIAN_POINT('Ctrl Pts',(-3.217125156,3.97753138,6.509012185));
#129829=CARTESIAN_POINT('Ctrl Pts',(-2.855679535,4.042807359,6.66390234));
#129830=CARTESIAN_POINT('Ctrl Pts',(-2.84324220927218,4.04505350217026,
6.66923210248114));
#129831=CARTESIAN_POINT('Ctrl Pts',(-2.8308048835443,4.04729964534049,6.67456186496213));
#129832=CARTESIAN_POINT('',(-3.17864374056489,4.04280735814475,6.79310128093997));
#129833=CARTESIAN_POINT('',(-3.0171615997571,4.04280735744341,6.72850178992045));
#129834=CARTESIAN_POINT('',(-3.67991631910299,3.95233946528539,6.53515221828794));
#129835=CARTESIAN_POINT('Origin',(0.085397309970424,4.01785666792284,-0.173056431550604));
#129836=CARTESIAN_POINT('Ctrl Pts',(-3.555619897094,3.91326598481269,6.31823291346998));
#129837=CARTESIAN_POINT('Ctrl Pts',(-3.57634910582588,3.92008713877303,
6.35431307523612));
#129838=CARTESIAN_POINT('Ctrl Pts',(-3.59708101209336,3.92674915953913,
6.39044940039092));
#129839=CARTESIAN_POINT('Ctrl Pts',(-3.63850520916451,3.93976378698617,
6.46274525194019));
#129840=CARTESIAN_POINT('Ctrl Pts',(-3.65922008492869,3.94612348103791,
6.49894420465417));
#129841=CARTESIAN_POINT('Ctrl Pts',(-3.67991632022434,3.95233945646779,
6.53515221916074));
#129842=CARTESIAN_POINT('Ctrl Pts',(-4.164706805,4.042807359,6.237404687));
#129843=CARTESIAN_POINT('Ctrl Pts',(-3.822601077,3.977102825,6.465828226));
#129844=CARTESIAN_POINT('Ctrl Pts',(-3.457565706,3.912499672,6.65546688));
#129845=CARTESIAN_POINT('Ctrl Pts',(-4.221457354,4.042807359,5.89421732));
#129846=CARTESIAN_POINT('Ctrl Pts',(-3.898174577,3.977102825,6.125753481));
#129847=CARTESIAN_POINT('Ctrl Pts',(-3.551508834,3.912499672,6.320544676));
#129848=CARTESIAN_POINT('',(-4.16470679092074,4.0428073603099,6.23740467049541));
#129849=CARTESIAN_POINT('Origin',(0.119447674717098,4.16063866399011,-0.144937381015162));
#129850=CARTESIAN_POINT('',(-4.19336581362883,4.04280736269456,6.06409507953821));
#129851=CARTESIAN_POINT('Origin',(2.72568426162856E-13,4.13463032200044,
-2.20309881449055E-13));
#129852=CARTESIAN_POINT('',(-3.6822002655948,4.13354310057997,6.5338657166798));
#129853=CARTESIAN_POINT('Origin',(0.0980868956556286,4.16070812044129,-0.165143190232435));
#129854=CARTESIAN_POINT('Origin',(0.1100067681996,4.01786468285577,-0.157521998228017));
#129855=CARTESIAN_POINT('Ctrl Pts',(-5.18223483131303,3.912491975,5.42238150830926));
#129856=CARTESIAN_POINT('Ctrl Pts',(-4.88812847245207,3.97753138,5.70346247143213));
#129857=CARTESIAN_POINT('Ctrl Pts',(-4.56534565464645,4.042807359,5.95108377760583));
#129858=CARTESIAN_POINT('Ctrl Pts',(-4.55423871405474,4.04505350216756,
5.9596044143473));
#129859=CARTESIAN_POINT('Ctrl Pts',(-4.54313177346315,4.0472996453351,5.96812505108879));
#129860=CARTESIAN_POINT('Ctrl Pts',(-4.834213266,3.912491975,5.403043781));
#129861=CARTESIAN_POINT('Ctrl Pts',(-4.541155773,3.97753138,5.665248286));
#129862=CARTESIAN_POINT('Ctrl Pts',(-4.221457354,4.042807359,5.89421732));
#129863=CARTESIAN_POINT('Ctrl Pts',(-4.2104565474167,4.04505350216756,5.90209613299033));
#129864=CARTESIAN_POINT('Ctrl Pts',(-4.19945574083342,4.04729964533509,
5.90997494598055));
#129865=CARTESIAN_POINT('',(-4.56464478872052,4.04280735814476,5.95096790420922));
#129866=CARTESIAN_POINT('',(-4.39305102980428,4.04280735744341,5.92259260020826));
#129867=CARTESIAN_POINT('',(-4.99874646950625,3.95233946528412,5.59129076012302));
#129868=CARTESIAN_POINT('Origin',(0.120602791296842,4.0178566388305,-0.150652566420965));
#129869=CARTESIAN_POINT('Ctrl Pts',(-4.83072478992622,3.91326598477064,
5.406162965312));
#129870=CARTESIAN_POINT('Ctrl Pts',(-4.8587255272726,3.92008713815959,5.43694342298863));
#129871=CARTESIAN_POINT('Ctrl Pts',(-4.88674097220958,3.92674915833406,
5.46777815080322));
#129872=CARTESIAN_POINT('Ctrl Pts',(-4.94273817031434,3.93976378685885,
5.52947879248528));
#129873=CARTESIAN_POINT('Ctrl Pts',(-4.97075044803058,3.94612348078679,
5.5603783471148));
#129874=CARTESIAN_POINT('Ctrl Pts',(-4.99874647078695,3.95233945646387,
5.59129076073675));
#129875=CARTESIAN_POINT('Ctrl Pts',(-5.408195905,4.042807359,5.19628877700001));
#129876=CARTESIAN_POINT('Ctrl Pts',(-5.123192728,3.977102825,5.492914519));
#129877=CARTESIAN_POINT('Ctrl Pts',(-4.807458386,3.912499672,5.756591341));
#129878=CARTESIAN_POINT('Ctrl Pts',(-5.389844518,4.042807359,4.848925249));
#129879=CARTESIAN_POINT('Ctrl Pts',(-5.12389334400001,3.977102825,5.144544464));
#129880=CARTESIAN_POINT('Ctrl Pts',(-4.827206802,3.912499672,5.409304437));
#129881=CARTESIAN_POINT('',(-5.4081958877456,4.04280736030966,5.19628876383342));
#129882=CARTESIAN_POINT('Origin',(0.147812296518153,4.16063868253327,-0.115871092322576));
#129883=CARTESIAN_POINT('',(-5.39892843915143,4.04280736269456,5.02087021193417));
#129884=CARTESIAN_POINT('Origin',(9.61036805691151E-13,4.13463032200111,
-9.48026379621325E-13));
#129885=CARTESIAN_POINT('',(-5.00070045828517,4.13354310060792,5.58954335523504));
#129886=CARTESIAN_POINT('Origin',(0.131294733959384,4.16070811736415,-0.140196623117392));
#129887=CARTESIAN_POINT('Origin',(0.141297377257072,4.01786463695052,-0.13019094599066));
#129888=CARTESIAN_POINT('Ctrl Pts',(-6.22672880104064,3.912491975,4.18158193873128));
#129889=CARTESIAN_POINT('Ctrl Pts',(-5.99992258317702,3.97753138,4.51931555890433));
#129890=CARTESIAN_POINT('Ctrl Pts',(-5.73791750913712,4.042807359,4.83053638071154));
#129891=CARTESIAN_POINT('Ctrl Pts',(-5.72890192760565,4.04505350218207,
4.84124547366929));
#129892=CARTESIAN_POINT('Ctrl Pts',(-5.71988634607416,4.04729964536412,
4.85195456662708));
#129893=CARTESIAN_POINT('Ctrl Pts',(-5.882686747,3.912491975,4.237510666));
#129894=CARTESIAN_POINT('Ctrl Pts',(-5.652846992,3.97753138,4.556583674));
#129895=CARTESIAN_POINT('Ctrl Pts',(-5.389844518,4.042807359,4.848925249));
#129896=CARTESIAN_POINT('Ctrl Pts',(-5.38079461598564,4.04505350218207,
4.85898470801665));
#129897=CARTESIAN_POINT('Ctrl Pts',(-5.37174471397128,4.04729964536412,
4.86904416703315));
#129898=CARTESIAN_POINT('',(-5.73720811971194,4.04280735814475,4.83057388182148));
#129899=CARTESIAN_POINT('',(-5.56352627571132,4.04280735744341,4.83974956272915));
#129900=CARTESIAN_POINT('',(-6.08384079109198,3.95233946527227,4.38598675996371));
#129901=CARTESIAN_POINT('Origin',(0.150168970924535,4.01785667742024,-0.121204340528558));
#129902=CARTESIAN_POINT('Ctrl Pts',(-5.87995036175847,3.9132659847659,4.24130684477094));
#129903=CARTESIAN_POINT('Ctrl Pts',(-5.91391334079663,3.9200871371288,4.26534833799181));
#129904=CARTESIAN_POINT('Ctrl Pts',(-5.94790234940561,3.92674915624501,
4.2894396703587));
#129905=CARTESIAN_POINT('Ctrl Pts',(-6.01585418149866,3.93976378540211,
4.33766004531525));
#129906=CARTESIAN_POINT('Ctrl Pts',(-6.04985403012971,3.9461234778491,4.36181536781961));
#129907=CARTESIAN_POINT('Ctrl Pts',(-6.0838407924566,3.95233945642855,4.38598676031923));
#129908=CARTESIAN_POINT('Ctrl Pts',(-6.398803776,4.042807359,3.912200178));
#129909=CARTESIAN_POINT('Ctrl Pts',(-6.184229582,3.977102825,4.263158233));
#129910=CARTESIAN_POINT('Ctrl Pts',(-5.932559655,3.912499672,4.58854398900001));
#129911=CARTESIAN_POINT('Ctrl Pts',(-6.306208544,4.042807359,3.576902822));
#129912=CARTESIAN_POINT('Ctrl Pts',(-6.110024554,3.977102825,3.922782265));
#129913=CARTESIAN_POINT('Ctrl Pts',(-5.877189946,3.912499672,4.245131134));
#129914=CARTESIAN_POINT('',(-6.39880375628837,4.04280736030989,3.91220016894969));
#129915=CARTESIAN_POINT('Origin',(0.169265304818327,4.16063873557015,-0.0813867475649099));
#129916=CARTESIAN_POINT('',(-6.35204317234975,4.04280736269456,3.74287503272014));
#129917=CARTESIAN_POINT('Origin',(-1.25767452008319E-14,4.134630322,-9.84455572616838E-14));
#129918=CARTESIAN_POINT('',(-6.08537345602736,4.13354310061625,4.38386015920024));
#129919=CARTESIAN_POINT('Origin',(0.158363050465506,4.16070812830415,-0.108694257231567));
#129920=CARTESIAN_POINT('Origin',(0.165981115668196,4.01786465600101,-0.0967723840180312));
#129921=CARTESIAN_POINT('Ctrl Pts',(-6.98006785221684,3.912491975,2.7452562455473));
#129922=CARTESIAN_POINT('Ctrl Pts',(-6.83116698223101,3.97753138,3.12385047328293));
#129923=CARTESIAN_POINT('Ctrl Pts',(-6.64219071889822,4.042807359,3.48411847140535));
#129924=CARTESIAN_POINT('Ctrl Pts',(-6.63568805525163,4.04505350213012,
3.49651527496737));
#129925=CARTESIAN_POINT('Ctrl Pts',(-6.6291853916049,4.0472996452602,3.50891207852946));
#129926=CARTESIAN_POINT('Ctrl Pts',(-6.656092333,3.912491975,2.873836261));
#129927=CARTESIAN_POINT('Ctrl Pts',(-6.500217369,3.97753138,3.234858274));
#129928=CARTESIAN_POINT('Ctrl Pts',(-6.306208544,4.042807359,3.576902822));
#129929=CARTESIAN_POINT('Ctrl Pts',(-6.2995327101614,4.04505350213012,3.58867255756663));
#129930=CARTESIAN_POINT('Ctrl Pts',(-6.2928568763229,4.04729964526021,3.60044229313331));
#129931=CARTESIAN_POINT('',(-6.64150597624777,4.04280735814476,3.4843075935145));
#129932=CARTESIAN_POINT('',(-6.47385721741239,4.04280735744341,3.53060521441202));
#129933=CARTESIAN_POINT('',(-6.88446147873679,3.95233946528909,2.97559889404972));
#129934=CARTESIAN_POINT('Origin',(0.17271367438223,4.0178566438613,-0.0860888581960229));
#129935=CARTESIAN_POINT('Ctrl Pts',(-6.65423598875174,3.91326598480925,
2.8781319295331));
#129936=CARTESIAN_POINT('Ctrl Pts',(-6.69257316711119,3.9200871415113,2.89431032003077));
#129937=CARTESIAN_POINT('Ctrl Pts',(-6.73094648359607,3.9267491651031,2.91053179016838));
#129938=CARTESIAN_POINT('Ctrl Pts',(-6.80767555484976,3.93976378744888,
2.94301714747179));
#129939=CARTESIAN_POINT('Ctrl Pts',(-6.84607319970337,3.94612348197739,
2.95929877525651));
#129940=CARTESIAN_POINT('Ctrl Pts',(-6.88446148016122,3.95233945647872,
2.97559889405487));
#129941=CARTESIAN_POINT('Ctrl Pts',(-7.090210694,4.042807359,2.445181447));
#129942=CARTESIAN_POINT('Ctrl Pts',(-6.956098733,3.977102825,2.834061408));
#129943=CARTESIAN_POINT('Ctrl Pts',(-6.78026102800001,3.912499672,3.20594142));
#129944=CARTESIAN_POINT('Ctrl Pts',(-6.927701267,4.042807359,2.137628395));
#129945=CARTESIAN_POINT('Ctrl Pts',(-6.810457805,3.977102825,2.517595128));
#129946=CARTESIAN_POINT('Ctrl Pts',(-6.65236221900001,3.912499672,2.882460217));
#129947=CARTESIAN_POINT('',(-7.09021067281184,4.04280736030966,2.44518144232082));
#129948=CARTESIAN_POINT('Origin',(0.182803577580881,4.1606386766149,-0.043096885077048));
#129949=CARTESIAN_POINT('',(-7.00814342633534,4.04280736269456,2.2898671772543));
#129950=CARTESIAN_POINT('Origin',(2.70183181383388E-13,4.13463032199933,
-3.4477629085039E-14));
#129951=CARTESIAN_POINT('',(-6.88550115512097,4.13354310058775,2.97319253349686));
#129952=CARTESIAN_POINT('Origin',(0.178026526882995,4.16070809325089,-0.0721096142243627));
#129953=CARTESIAN_POINT('Origin',(0.182903650094188,4.01786467042396,-0.0588288152680649));
#129954=CARTESIAN_POINT('Ctrl Pts',(-7.4070266874212,3.912491975,1.18056542085387));
#129955=CARTESIAN_POINT('Ctrl Pts',(-7.34299360664207,3.97753138,1.58231761241509));
#129956=CARTESIAN_POINT('Ctrl Pts',(-7.23588247237805,4.042807359,1.97478705503451));
#129957=CARTESIAN_POINT('Ctrl Pts',(-7.2321967832453,4.04505350239193,1.98829191024431));
#129958=CARTESIAN_POINT('Ctrl Pts',(-7.22851109411266,4.04729964578383,
2.00179676545403));
#129959=CARTESIAN_POINT('Ctrl Pts',(-7.118266439,3.912491975,1.375784468));
#129960=CARTESIAN_POINT('Ctrl Pts',(-7.043644806,3.97753138,1.761874495));
#129961=CARTESIAN_POINT('Ctrl Pts',(-6.927701267,4.042807359,2.137628395));
#129962=CARTESIAN_POINT('Ctrl Pts',(-6.92371165523237,4.04505350239193,
2.15055806916811));
#129963=CARTESIAN_POINT('Ctrl Pts',(-6.91972204346475,4.04729964578383,
2.1634877433363));
#129964=CARTESIAN_POINT('',(-7.23525439422029,4.04280735814475,1.97511895503816));
#129965=CARTESIAN_POINT('',(-7.08147779032799,4.04280735744341,2.05637369070155));
#129966=CARTESIAN_POINT('',(-7.36317239935864,3.95233946528238,1.42607533064351));
#129967=CARTESIAN_POINT('Origin',(0.187181807889715,4.01785668190154,-0.0469477129738381));
#129968=CARTESIAN_POINT('Ctrl Pts',(-7.11737693710714,3.91326598474417,
1.38037876477042));
#129969=CARTESIAN_POINT('Ctrl Pts',(-7.15829567884329,3.92008713974062,
1.38793755120874));
#129970=CARTESIAN_POINT('Ctrl Pts',(-7.19925897335171,3.92674916156521,
1.39553064136023));
#129971=CARTESIAN_POINT('Ctrl Pts',(-7.28117757015847,3.93976378662875,
1.41076202997068));
#129972=CARTESIAN_POINT('Ctrl Pts',(-7.32217756234829,3.94612348031645,
1.41840864270744));
#129973=CARTESIAN_POINT('Ctrl Pts',(-7.36317240074903,3.95233945645877,
1.42607533036288));
#129974=CARTESIAN_POINT('Ctrl Pts',(-7.450087241,4.042807359,0.86382875));
#129975=CARTESIAN_POINT('Ctrl Pts',(-7.402708438,3.977102825,1.27244702));
#129976=CARTESIAN_POINT('Ctrl Pts',(-7.310924932,3.912499672,1.673432593));
#129977=CARTESIAN_POINT('Ctrl Pts',(-7.225262378,4.042807359,0.59840084));
#129978=CARTESIAN_POINT('Ctrl Pts',(-7.192441619,3.977102825,0.994688041));
#129979=CARTESIAN_POINT('Ctrl Pts',(-7.116477429,3.912499672,1.385008664));
#129980=CARTESIAN_POINT('',(-7.45008721928956,4.04280736030965,0.863828749933751));
#129981=CARTESIAN_POINT('Origin',(0.187794765762662,4.1606387163103,-0.00279201758977748));
#129982=CARTESIAN_POINT('',(-7.33655068294462,4.04280736269456,0.729787677972479));
#129983=CARTESIAN_POINT('Origin',(1.0698907038087E-12,4.13463032200044,
-2.8200098506348E-13));
#129984=CARTESIAN_POINT('',(-7.36367047205426,4.13354310059326,1.42350172983018));
#129985=CARTESIAN_POINT('Origin',(0.189366034920901,4.16070809352831,-0.0321533447766773));
#129986=CARTESIAN_POINT('Origin',(0.191273883476633,4.01786465346802,-0.0181345584468363));
#129987=CARTESIAN_POINT('Ctrl Pts',(-7.48764118870734,3.912491975,-0.439327330070044));
#129988=CARTESIAN_POINT('Ctrl Pts',(-7.5114700099638,3.97753138,-0.0332026624065126));
#129989=CARTESIAN_POINT('Ctrl Pts',(-7.49123240398283,4.042807359,0.373116790603217));
#129990=CARTESIAN_POINT('Ctrl Pts',(-7.49053602896029,4.04505350221427,
0.387098222918463));
#129991=CARTESIAN_POINT('Ctrl Pts',(-7.4898396539377,4.04729964542849,0.401079655233702));
#129992=CARTESIAN_POINT('Ctrl Pts',(-7.24759831800001,3.912491975,-0.186597478));
#129993=CARTESIAN_POINT('Ctrl Pts',(-7.257719241,3.97753138,0.206507424));
#129994=CARTESIAN_POINT('Ctrl Pts',(-7.225262378,4.042807359,0.59840084));
#129995=CARTESIAN_POINT('Ctrl Pts',(-7.22414553894681,4.04505350221427,
0.611885873094053));
#129996=CARTESIAN_POINT('Ctrl Pts',(-7.22302869989349,4.0472996454285,0.625370906188109));
#129997=CARTESIAN_POINT('',(-7.49069035867608,4.04280735814475,0.373575949174865));
#129998=CARTESIAN_POINT('',(-7.35797633236851,4.04280735744341,0.485988418560827));
#129999=CARTESIAN_POINT('',(-7.49758956224147,3.95233946528052,-0.190129930137772));
#130000=CARTESIAN_POINT('Origin',(0.192898267892459,4.01785666442251,-0.00561154578427628));
#130001=CARTESIAN_POINT('Ctrl Pts',(-7.24771725059274,3.91326598480197,
-0.181919376803831));
#130002=CARTESIAN_POINT('Ctrl Pts',(-7.28930422197603,3.92008713508906,
-0.183333629475567));
#130003=CARTESIAN_POINT('Ctrl Pts',(-7.33094207501763,3.92674915206884,
-0.18472395798091));
#130004=CARTESIAN_POINT('Ctrl Pts',(-7.4142198183722,3.93976378642255,-0.187458749621351));
#130005=CARTESIAN_POINT('Ctrl Pts',(-7.4559050477043,3.94612347989405,-0.188804696837706));
#130006=CARTESIAN_POINT('Ctrl Pts',(-7.49758956353974,3.95233945645325,
-0.190129930705654));
#130007=CARTESIAN_POINT('Ctrl Pts',(-7.461605988,4.042807359,-0.757915620000001));
#130008=CARTESIAN_POINT('Ctrl Pts',(-7.50317572500001,3.977102825,-0.348665576));
#130009=CARTESIAN_POINT('Ctrl Pts',(-7.499738111,3.912499672,0.062675918));
#130010=CARTESIAN_POINT('Ctrl Pts',(-7.18497825100001,4.042807359,-0.968807273));
#130011=CARTESIAN_POINT('Ctrl Pts',(-7.238114857,3.977102825,-0.574729554));
#130012=CARTESIAN_POINT('Ctrl Pts',(-7.24783406400001,3.912499672,-0.177204354));
#130013=CARTESIAN_POINT('',(-7.46160596678344,4.04280736030965,-0.757915615395764));
#130014=CARTESIAN_POINT('Origin',(0.184004250522272,4.16063871261539,0.0376435729130676));
#130015=CARTESIAN_POINT('',(-7.32190898346867,4.04280736269456,-0.864415882287469));
#130016=CARTESIAN_POINT('Origin',(1.65839564303383E-12,4.134630322,3.6239457615328E-14));
#130017=CARTESIAN_POINT('',(-7.49752274183165,4.13354310057391,-0.192750432608097));
#130018=CARTESIAN_POINT('Origin',(0.19185085619743,4.1607081097785,0.00930648937395421));
#130019=CARTESIAN_POINT('Origin',(0.190700775333477,4.01786464775998,0.0234076710092347));
#130020=CARTESIAN_POINT('Ctrl Pts',(-7.21814190835588,3.912491975,-2.03867762420809));
#130021=CARTESIAN_POINT('Ctrl Pts',(-7.32871842420211,3.97753138,-1.64717041730805));
#130022=CARTESIAN_POINT('Ctrl Pts',(-7.39630063392665,4.042807359,-1.24600000080534));
#130023=CARTESIAN_POINT('Ctrl Pts',(-7.39862613459791,4.04505350238006,
-1.23219574556317));
#130024=CARTESIAN_POINT('Ctrl Pts',(-7.40095163526915,4.04729964576008,
-1.21839149032102));
#130025=CARTESIAN_POINT('Ctrl Pts',(-7.038040555,3.912491975,-1.740254334));
#130026=CARTESIAN_POINT('Ctrl Pts',(-7.13243079,3.97753138,-1.358515705));
#130027=CARTESIAN_POINT('Ctrl Pts',(-7.184978251,4.042807359,-0.968807273));
#130028=CARTESIAN_POINT('Ctrl Pts',(-7.18678640667185,4.04505350238006,
-0.955397424107718));
#130029=CARTESIAN_POINT('Ctrl Pts',(-7.18859456234357,4.04729964576008,
-0.941987575215448));
#130030=CARTESIAN_POINT('',(-7.39586996682337,4.04280735814475,-1.24543505334257));
#130031=CARTESIAN_POINT('',(-7.29042407893858,4.04280735744341,-1.10712113202695));
#130032=CARTESIAN_POINT('',(-7.28142776983371,3.95233946530271,-1.79744492687227));
#130033=CARTESIAN_POINT('Origin',(0.189594772458952,4.01785666382256,0.0359870838592783));
#130034=CARTESIAN_POINT('Ctrl Pts',(-7.03916236014506,3.91326598479388,
-1.73571117070117));
#130035=CARTESIAN_POINT('Ctrl Pts',(-7.07947305393982,3.92008713936462,
-1.74603233504673));
#130036=CARTESIAN_POINT('Ctrl Pts',(-7.11983858613362,3.92674916075612,
-1.75634107334237));
#130037=CARTESIAN_POINT('Ctrl Pts',(-7.20058140535285,3.93976378909938,
-1.77691417074854));
#130038=CARTESIAN_POINT('Ctrl Pts',(-7.24100273676367,3.94612348529266,
-1.78718974722731));
#130039=CARTESIAN_POINT('Ctrl Pts',(-7.28142777095667,3.95233945651953,
-1.79744492776942));
#130040=CARTESIAN_POINT('Ctrl Pts',(-7.124228332,4.042807359,-2.344220698));
#130041=CARTESIAN_POINT('Ctrl Pts',(-7.252802854,3.977102825,-1.953474957));
#130042=CARTESIAN_POINT('Ctrl Pts',(-7.337871871,3.912499672,-1.551011413));
#130043=CARTESIAN_POINT('Ctrl Pts',(-6.808732526,4.042807359,-2.490715035));
#130044=CARTESIAN_POINT('Ctrl Pts',(-6.945341889,3.977102825,-2.117273434));
#130045=CARTESIAN_POINT('Ctrl Pts',(-7.04029003300001,3.912499672,-1.731131494));
#130046=CARTESIAN_POINT('',(-7.1242283122693,4.04280736030965,-2.34422068894288));
#130047=CARTESIAN_POINT('Origin',(0.17160996885161,4.1606386991441,0.0763189263862812));
#130048=CARTESIAN_POINT('',(-6.96490295739362,4.04280736269456,-2.41820031680348));
#130049=CARTESIAN_POINT('Origin',(-8.32667268468867E-13,4.13463032199911,
-3.12141805458577E-13));
#130050=CARTESIAN_POINT('',(-7.28079918139993,4.13354310058009,-1.79998979899541));
#130051=CARTESIAN_POINT('Origin',(0.185364917121934,4.16070811704502,0.0503311790112895));
#130052=CARTESIAN_POINT('Origin',(0.181210223905396,4.01786465413451,0.0638554106367939));
#130053=CARTESIAN_POINT('Ctrl Pts',(-6.61113033607533,3.912491975,-3.54270161749554));
#130054=CARTESIAN_POINT('Ctrl Pts',(-6.80328411084193,3.97753138,-3.18411831437587));
#130055=CARTESIAN_POINT('Ctrl Pts',(-6.95552606635459,4.042807359,-2.80685521578371));
#130056=CARTESIAN_POINT('Ctrl Pts',(-6.9607647044976,4.04505350220186,-2.79387361126094));
#130057=CARTESIAN_POINT('Ctrl Pts',(-6.9660033426406,4.0472996454037,-2.7808920067382));
#130058=CARTESIAN_POINT('Ctrl Pts',(-6.499391838,3.912491975,-3.212538831));
#130059=CARTESIAN_POINT('Ctrl Pts',(-6.673637803,3.97753138,-2.860016149));
#130060=CARTESIAN_POINT('Ctrl Pts',(-6.808732526,4.042807359,-2.490715035));
#130061=CARTESIAN_POINT('Ctrl Pts',(-6.81338112872218,4.04505350220186,
-2.47800740197241));
#130062=CARTESIAN_POINT('Ctrl Pts',(-6.81802973144437,4.04729964540369,
-2.46529976894482));
#130063=CARTESIAN_POINT('',(-6.95522691503914,4.04280735814474,-2.80621089584825));
#130064=CARTESIAN_POINT('',(-6.88197969794138,4.04280735744339,-2.64846292855763));
#130065=CARTESIAN_POINT('',(-6.7247945077253,3.95233946527634,-3.32071339609417));
#130066=CARTESIAN_POINT('Origin',(0.177425631813312,4.01785665619084,0.0759028331350597));
#130067=CARTESIAN_POINT('Ctrl Pts',(-6.50146406158771,3.91326598472177,
-3.20834303966903));
#130068=CARTESIAN_POINT('Ctrl Pts',(-6.53861356724024,3.92008713904787,
-3.22708850772555));
#130069=CARTESIAN_POINT('Ctrl Pts',(-6.5758193002426,3.92674916019177,-3.24583362881935));
#130070=CARTESIAN_POINT('Ctrl Pts',(-6.65025177415825,3.93976378587443,
-3.28328305016212));
#130071=CARTESIAN_POINT('Ctrl Pts',(-6.68751911182413,3.94612347883912,
-3.30200777054742));
#130072=CARTESIAN_POINT('Ctrl Pts',(-6.72479450867199,3.95233945644068,
-3.32071339714379));
#130073=CARTESIAN_POINT('Ctrl Pts',(-6.453729677,4.042807359,-3.820912621));
#130074=CARTESIAN_POINT('Ctrl Pts',(-6.663296982,3.977102825,-3.46694202));
#130075=CARTESIAN_POINT('Ctrl Pts',(-6.83289489800001,3.912499672,-3.092175175));
#130076=CARTESIAN_POINT('Ctrl Pts',(-6.114118036,4.042807359,-3.89615973));
#130077=CARTESIAN_POINT('Ctrl Pts',(-6.327812453,3.977102825,-3.560815961));
#130078=CARTESIAN_POINT('Ctrl Pts',(-6.503549865,3.912499672,-3.20411285));
#130079=CARTESIAN_POINT('',(-6.45372965975711,4.0428073603099,-3.82091260783521));
#130080=CARTESIAN_POINT('Origin',(0.151191584710254,4.16063868549269,0.111425745006766));
#130081=CARTESIAN_POINT('',(-6.28222581014146,4.04280736269456,-3.85891239175924));
#130082=CARTESIAN_POINT('Origin',(3.16153353496773E-13,4.13463032200067,
2.28766658394441E-13));
#130083=CARTESIAN_POINT('',(-6.72363354311164,4.13354310059453,-3.32306364287935));
#130084=CARTESIAN_POINT('Origin',(0.170211178350446,4.16070808827327,0.0890022978908028));
#130085=CARTESIAN_POINT('Origin',(0.163246422937403,4.01786466078058,0.101317255762698));
#130086=CARTESIAN_POINT('Ctrl Pts',(-5.69498965639203,3.912491975,-4.88107282109577));
#130087=CARTESIAN_POINT('Ctrl Pts',(-5.95973579334589,3.97753138,-4.57218037737035));
#130088=CARTESIAN_POINT('Ctrl Pts',(-6.189518831403,4.042807359,-4.23646500152237));
#130089=CARTESIAN_POINT('Ctrl Pts',(-6.19742565445324,4.04505350223037,
-4.22491305193323));
#130090=CARTESIAN_POINT('Ctrl Pts',(-6.20533247750354,4.04729964546071,
-4.21336110234407));
#130091=CARTESIAN_POINT('Ctrl Pts',(-5.65683878100001,3.912491975,-4.534608583));
#130092=CARTESIAN_POINT('Ctrl Pts',(-5.902792929,3.97753138,-4.227785417));
#130093=CARTESIAN_POINT('Ctrl Pts',(-6.11411803600001,4.042807359,-3.89615973));
#130094=CARTESIAN_POINT('Ctrl Pts',(-6.1213897225494,4.04505350223037,-3.88474850640318));
#130095=CARTESIAN_POINT('Ctrl Pts',(-6.12866140909881,4.04729964546071,
-3.87333728280642));
#130096=CARTESIAN_POINT('',(-6.18936518382027,4.04280735814474,-4.23577143670967));
#130097=CARTESIAN_POINT('',(-6.15174159578327,4.04280735744339,-4.0659655425065));
#130098=CARTESIAN_POINT('',(-5.85371732862051,3.95233946527141,-4.68870899803957));
#130099=CARTESIAN_POINT('Origin',(0.156960845813895,4.01785670332497,0.112269676904007));
#130100=CARTESIAN_POINT('Ctrl Pts',(-5.6597645288131,3.91326598485026,-4.53095635367109));
#130101=CARTESIAN_POINT('Ctrl Pts',(-5.69201580768911,3.92008714537315,
-4.55724963271236));
#130102=CARTESIAN_POINT('Ctrl Pts',(-5.72432207755014,3.9267491728499,-4.58355466295653));
#130103=CARTESIAN_POINT('Ctrl Pts',(-5.78896377745649,3.93976378526525,
-4.63612926594674));
#130104=CARTESIAN_POINT('Ctrl Pts',(-5.82133456077178,3.9461234775913,-4.66242758604197));
#130105=CARTESIAN_POINT('Ctrl Pts',(-5.85371732933022,3.95233945642611,
-4.68870899925716));
#130106=CARTESIAN_POINT('Ctrl Pts',(-5.481461795,4.042807359,-5.118942917));
#130107=CARTESIAN_POINT('Ctrl Pts',(-5.762222749,3.977102825,-4.818298728));
#130108=CARTESIAN_POINT('Ctrl Pts',(-6.008419354,3.912499672,-4.488752262));
#130109=CARTESIAN_POINT('Ctrl Pts',(-5.133614182,4.042807359,-5.119424326));
#130110=CARTESIAN_POINT('Ctrl Pts',(-5.41440154,3.977102825,-4.837858691));
#130111=CARTESIAN_POINT('Ctrl Pts',(-5.662710933,3.912499672,-4.527273449));
#130112=CARTESIAN_POINT('',(-5.48146178092909,4.04280736030966,-5.11894290047791));
#130113=CARTESIAN_POINT('Origin',(0.123703542979664,4.16063869601417,0.141322381082165));
#130114=CARTESIAN_POINT('',(-5.30579876615036,4.04280736269456,-5.11918601225676));
#130115=CARTESIAN_POINT('Origin',(-6.67001176513082E-13,4.13463032199978,
-5.13911829758129E-13));
#130116=CARTESIAN_POINT('',(-5.8520782731024,4.13354310059652,-4.69075472387006));
#130117=CARTESIAN_POINT('Origin',(0.147099097435169,4.16070813559084,0.123512037761863));
#130118=CARTESIAN_POINT('Origin',(0.137649683437396,4.01786468222999,0.134041740787689));
#130119=CARTESIAN_POINT('Ctrl Pts',(-4.51255758966453,3.912491975,-5.99121048432391));
#130120=CARTESIAN_POINT('Ctrl Pts',(-4.83751685380577,3.97753138,-5.74645236820935));
#130121=CARTESIAN_POINT('Ctrl Pts',(-5.13409657424069,4.042807359,-5.46798239187965));
#130122=CARTESIAN_POINT('Ctrl Pts',(-5.14430186812406,4.04505350229073,
-5.45840025341797));
#130123=CARTESIAN_POINT('Ctrl Pts',(-5.15450716200743,4.04729964558143,
-5.44881811495625));
#130124=CARTESIAN_POINT('Ctrl Pts',(-4.549778231,3.912491975,-5.64464507700001));
#130125=CARTESIAN_POINT('Ctrl Pts',(-4.855940018,3.97753138,-5.397868138));
#130126=CARTESIAN_POINT('Ctrl Pts',(-5.133614182,4.042807359,-5.119424326));
#130127=CARTESIAN_POINT('Ctrl Pts',(-5.14316893659779,4.04505350229073,
-5.10984308785164));
#130128=CARTESIAN_POINT('Ctrl Pts',(-5.15272369119556,4.04729964558143,
-5.10026184970315));
#130129=CARTESIAN_POINT('',(-5.13409561478568,4.04280735814474,-5.4672720125227));
#130130=CARTESIAN_POINT('',(-5.13385489337812,4.04280735744339,-5.29334812632912));
#130131=CARTESIAN_POINT('',(-4.7089268331995,3.95233946528876,-5.83746577823621));
#130132=CARTESIAN_POINT('Origin',(0.129156504148766,4.01785666691168,0.143386795471282));
#130133=CARTESIAN_POINT('Ctrl Pts',(-4.55342069737005,3.91326598475465,
-5.64170718417175));
#130134=CARTESIAN_POINT('Ctrl Pts',(-4.57926564397507,3.92008713542126,
-5.67431876535296));
#130135=CARTESIAN_POINT('Ctrl Pts',(-4.60516176501408,3.9267491527984,-5.7069536386321));
#130136=CARTESIAN_POINT('Ctrl Pts',(-4.65699028047525,3.93976378738226,
-5.77219524223799));
#130137=CARTESIAN_POINT('Ctrl Pts',(-4.68295090080554,3.94612348186694,
-5.80483749548642));
#130138=CARTESIAN_POINT('Ctrl Pts',(-4.70892683358658,3.95233945647787,
-5.83746577960661));
#130139=CARTESIAN_POINT('Ctrl Pts',(-4.252886852,4.042807359,-6.177617131));
#130140=CARTESIAN_POINT('Ctrl Pts',(-4.591713385,3.977102825,-5.944357142));
#130141=CARTESIAN_POINT('Ctrl Pts',(-4.902996799,3.912499672,-5.675440282));
#130142=CARTESIAN_POINT('Ctrl Pts',(-3.913068234,4.042807359,-6.103310331));
#130143=CARTESIAN_POINT('Ctrl Pts',(-4.247819228,3.977102825,-5.888688526));
#130144=CARTESIAN_POINT('Ctrl Pts',(-4.557089932,3.912499672,-5.638743774));
#130145=CARTESIAN_POINT('',(-4.25288684182705,4.04280736030967,-6.17761711183535));
#130146=CARTESIAN_POINT('Origin',(0.0904312725799133,4.16063868171559,0.164610930327612));
#130147=CARTESIAN_POINT('',(-4.08127846875943,4.04280736269456,-6.14009218447091));
#130148=CARTESIAN_POINT('Origin',(-5.33427468862868E-14,4.13463032200022,
-1.29236898960272E-13));
#130149=CARTESIAN_POINT('',(-4.70688632716557,4.13354310061502,-5.83911132777436));
#130150=CARTESIAN_POINT('Origin',(0.117108542261745,4.16070812578763,0.152246319600126));
#130151=CARTESIAN_POINT('Origin',(0.105616433177164,4.01786462505133,0.160498468657823));
#130152=CARTESIAN_POINT('Ctrl Pts',(-3.11912334532114,3.912491975,-6.82120580448832));
#130153=CARTESIAN_POINT('Ctrl Pts',(-3.48910100211822,3.97753138,-6.65202663257592));
#130154=CARTESIAN_POINT('Ctrl Pts',(-3.83860966710354,4.042807359,-6.44382300225625));
#130155=CARTESIAN_POINT('Ctrl Pts',(-3.85063624307732,4.04505350222721,
-6.43665872557614));
#130156=CARTESIAN_POINT('Ctrl Pts',(-3.86266281905113,4.0472996454544,-6.42949444889594));
#130157=CARTESIAN_POINT('Ctrl Pts',(-3.229975107,3.912491975,-6.490744241));
#130158=CARTESIAN_POINT('Ctrl Pts',(-3.582028749,3.97753138,-6.315552544));
#130159=CARTESIAN_POINT('Ctrl Pts',(-3.913068234,4.042807359,-6.103310331));
#130160=CARTESIAN_POINT('Ctrl Pts',(-3.92445928639878,4.04505350222722,
-6.09600708688845));
#130161=CARTESIAN_POINT('Ctrl Pts',(-3.93585033879756,4.04729964545439,
-6.08870384277701));
#130162=CARTESIAN_POINT('',(-3.83876144062878,4.04280735814475,-6.44312902495228));
#130163=CARTESIAN_POINT('',(-3.87591484165136,4.04280735744339,-6.27321963496368));
#130164=CARTESIAN_POINT('',(-3.34395215217457,3.95233946529221,-6.71326914644803));
#130165=CARTESIAN_POINT('Origin',(0.0953130054425495,4.01785664550041,0.167799374054779));
#130166=CARTESIAN_POINT('Ctrl Pts',(-3.23416397491899,3.91326598485202,
-6.4886580575758));
#130167=CARTESIAN_POINT('Ctrl Pts',(-3.25239416135484,3.92008713785229,
-6.52606311046376));
#130168=CARTESIAN_POINT('Ctrl Pts',(-3.27066931949185,3.92674915763536,
-6.56350191354768));
#130169=CARTESIAN_POINT('Ctrl Pts',(-3.30726108442044,3.9397637878327,-6.63835977825753));
#130170=CARTESIAN_POINT('Ctrl Pts',(-3.3255976415518,3.94612348273404,-6.67581964236287));
#130171=CARTESIAN_POINT('Ctrl Pts',(-3.34395215224815,3.95233945648807,
-6.71326914787331));
#130172=CARTESIAN_POINT('Ctrl Pts',(-2.825451647,4.042807359,-6.947432835));
#130173=CARTESIAN_POINT('Ctrl Pts',(-3.206500606,3.977102825,-6.792464023));
#130174=CARTESIAN_POINT('Ctrl Pts',(-3.568315562,3.912499672,-6.596751022));
#130175=CARTESIAN_POINT('Ctrl Pts',(-2.509551565,4.042807359,-6.801812328));
#130176=CARTESIAN_POINT('Ctrl Pts',(-2.88261361,3.977102825,-6.66416983));
#130177=CARTESIAN_POINT('Ctrl Pts',(-3.238384471,3.912499672,-6.486552707));
#130178=CARTESIAN_POINT('',(-2.82545164113304,4.04280736030965,-6.94743281409805));
#130179=CARTESIAN_POINT('Origin',(0.0529306025410337,4.16063867944897,0.180202534763928));
#130180=CARTESIAN_POINT('',(-2.66592212669213,4.04280736269456,-6.8738944707809));
#130181=CARTESIAN_POINT('Origin',(-5.57279916657549E-14,4.13463032200022,
-6.80878964320897E-14));
#130182=CARTESIAN_POINT('',(-3.34160560861239,4.13354310063453,-6.71443757508186));
#130183=CARTESIAN_POINT('Origin',(0.081642032993165,4.16070809414406,0.173861515886751));
#130184=CARTESIAN_POINT('Origin',(0.0686448621175723,4.01786462420063,0.179450723692286));
#130185=CARTESIAN_POINT('Ctrl Pts',(-1.57984236089796,3.912491975,-7.33224912145048));
#130186=CARTESIAN_POINT('Ctrl Pts',(-1.97753866607176,3.97753138,-7.24655952471014));
#130187=CARTESIAN_POINT('Ctrl Pts',(-2.36363363937118,4.042807359,-7.11835761149783));
#130188=CARTESIAN_POINT('Ctrl Pts',(-2.37691914846762,4.04505350223615,
-7.11394618995146));
#130189=CARTESIAN_POINT('Ctrl Pts',(-2.39020465756409,4.04729964547227,
-7.10953476840506));
#130190=CARTESIAN_POINT('Ctrl Pts',(-1.759141937,3.912491975,-7.033343419));
#130191=CARTESIAN_POINT('Ctrl Pts',(-2.140625797,3.97753138,-6.937928732));
#130192=CARTESIAN_POINT('Ctrl Pts',(-2.509551565,4.042807359,-6.801812328));
#130193=CARTESIAN_POINT('Ctrl Pts',(-2.52224628258409,4.04505350223615,
-6.79712856921376));
#130194=CARTESIAN_POINT('Ctrl Pts',(-2.5349410001682,4.04729964547226,-6.79244481042748));
#130195=CARTESIAN_POINT('',(-2.36393104912808,4.04280735814475,-7.1177124858181));
#130196=CARTESIAN_POINT('',(-2.43674132054344,4.04280735744339,-6.95976236583373));
#130197=CARTESIAN_POINT('',(-1.82261798542014,3.95233946528193,-7.27516751064553));
#130198=CARTESIAN_POINT('Origin',(0.0570127704426948,4.01785664805416,0.184365935620861));
#130199=CARTESIAN_POINT('Ctrl Pts',(-1.76368133957539,3.91326598486179,
-7.03220649175487));
#130200=CARTESIAN_POINT('Ctrl Pts',(-1.77344433390099,3.92008713797502,
-7.07265598703867));
#130201=CARTESIAN_POINT('Ctrl Pts',(-1.78324399318066,3.92674915786431,
-7.11314811114959));
#130202=CARTESIAN_POINT('Ctrl Pts',(-1.80288803263736,3.93976378662721,
-7.19412197946823));
#130203=CARTESIAN_POINT('Ctrl Pts',(-1.81274312564909,3.94612348027624,
-7.23464786204897));
#130204=CARTESIAN_POINT('Ctrl Pts',(-1.8226179852158,3.95233945645733,-7.27516751204908));
#130205=CARTESIAN_POINT('Ctrl Pts',(-1.265901463,4.042807359,-7.3923943));
#130206=CARTESIAN_POINT('Ctrl Pts',(-1.671355422,3.977102825,-7.322962836));
#130207=CARTESIAN_POINT('Ctrl Pts',(-2.066783856,3.912499672,-7.209605016));
#130208=CARTESIAN_POINT('Ctrl Pts',(-0.988691053000001,4.042807359,-7.18226914));
#130209=CARTESIAN_POINT('Ctrl Pts',(-1.382620184,3.977102825,-7.128041959));
#130210=CARTESIAN_POINT('Ctrl Pts',(-1.768255751,3.912499672,-7.031057645));
#130211=CARTESIAN_POINT('',(-1.26590146178554,4.04280736030965,-7.39239427832976));
#130212=CARTESIAN_POINT('Origin',(0.0129548444620933,4.1606387157555,0.187367821990734));
#130213=CARTESIAN_POINT('',(-1.12591022831811,4.04280736269456,-7.28628109074357));
#130214=CARTESIAN_POINT('Origin',(-4.87890977618477E-13,4.134630322,-1.20996962449382E-12));
#130215=CARTESIAN_POINT('',(-1.82007512463073,4.1335431006253,-7.27580418518327));
#130216=CARTESIAN_POINT('Origin',(0.0423581923295008,4.16070811576174,0.187347329555972));
#130217=CARTESIAN_POINT('Origin',(0.0284633256112127,4.01786458818801,0.190011699064334));
#130218=CARTESIAN_POINT('Ctrl Pts',(0.0333102964695516,3.912491975,-7.50044461904883));
#130219=CARTESIAN_POINT('Ctrl Pts',(-0.373508820894604,3.97753138,-7.50225134757834));
#130220=CARTESIAN_POINT('Ctrl Pts',(-0.778136729128367,4.042807359,-7.46004573014145));
#130221=CARTESIAN_POINT('Ctrl Pts',(-0.792059962488441,4.04505350334628,
-7.45859343619753));
#130222=CARTESIAN_POINT('Ctrl Pts',(-0.805983195848512,4.04729964769253,
-7.45714114225351));
#130223=CARTESIAN_POINT('Ctrl Pts',(-0.206053246,3.912491975,-7.247071275));
#130224=CARTESIAN_POINT('Ctrl Pts',(-0.599129562,3.97753138,-7.235895084));
#130225=CARTESIAN_POINT('Ctrl Pts',(-0.988691053,4.042807359,-7.18226914));
#130226=CARTESIAN_POINT('Ctrl Pts',(-1.00209585142571,4.04505350334628,
-7.18042387298486));
#130227=CARTESIAN_POINT('Ctrl Pts',(-1.01550064985142,4.04729964769254,
-7.17857860596984));
#130228=CARTESIAN_POINT('',(-0.883628482512665,4.04280735744339,-7.32087434385182));
#130229=CARTESIAN_POINT('Ctrl Pts',(-0.210730925519537,3.91326598472829,
-7.24693676511879));
#130230=CARTESIAN_POINT('Ctrl Pts',(-0.211570220743726,3.92008714020356,
-7.28853934331192));
#130231=CARTESIAN_POINT('Ctrl Pts',(-0.212436159929306,3.9267491625338,
-7.33019143747321));
#130232=CARTESIAN_POINT('Ctrl Pts',(-0.214213943682518,3.93976378611332,
-7.41349503639186));
#130233=CARTESIAN_POINT('Ctrl Pts',(-0.215126763178154,3.94612347931079,
-7.45519199686624));
#130234=CARTESIAN_POINT('Ctrl Pts',(-0.216060227165054,3.95233945644668,
-7.49688712928287));
#130235=CARTESIAN_POINT('Ctrl Pts',(0.352840867,4.042807359,-7.491695624));
#130236=CARTESIAN_POINT('Ctrl Pts',(-0.058059517,3.977102825,-7.511048045));
#130237=CARTESIAN_POINT('Ctrl Pts',(-0.468611634,3.912499672,-7.48534589300001));
#130238=CARTESIAN_POINT('Ctrl Pts',(0.578399553,4.042807359,-7.22689103));
#130239=CARTESIAN_POINT('Ctrl Pts',(0.182023025,3.977102825,-7.258614769));
#130240=CARTESIAN_POINT('Ctrl Pts',(-0.215445357,3.912499672,-7.246798141));
#130241=CARTESIAN_POINT('',(0.466747980841814,4.04280736269456,-7.35796930546287));
#130242=CARTESIAN_POINT('Ctrl Pts',(1.64490540305164,3.912491975,-7.31792766371014));
#130243=CARTESIAN_POINT('Ctrl Pts',(1.24798588321235,3.97753138,-7.40714623621052));
#130244=CARTESIAN_POINT('Ctrl Pts',(0.843744989901137,4.042807359,-7.45291040216964));
#130245=CARTESIAN_POINT('Ctrl Pts',(0.829835080901927,4.04505350218529,
-7.45448514484029));
#130246=CARTESIAN_POINT('Ctrl Pts',(0.815925171902729,4.04729964537055,
-7.45605988751085));
#130247=CARTESIAN_POINT('Ctrl Pts',(1.356670267,3.912491975,-7.121934132));
#130248=CARTESIAN_POINT('Ctrl Pts',(0.970381306,3.97753138,-7.195519024));
#130249=CARTESIAN_POINT('Ctrl Pts',(0.578399553,4.042807359,-7.22689103));
#130250=CARTESIAN_POINT('Ctrl Pts',(0.564911480408142,4.04505350218529,
-7.22797053916349));
#130251=CARTESIAN_POINT('Ctrl Pts',(0.551423407816283,4.04729964537055,
-7.22905004832698));
#130252=CARTESIAN_POINT('',(0.843204186876859,4.04280735814475,-7.45244978107983));
#130253=CARTESIAN_POINT('',(0.710801840462912,4.04280735744339,-7.33967037392361));
#130254=CARTESIAN_POINT('',(1.40060026653628,3.95233946528707,-7.36806063541257));
#130255=CARTESIAN_POINT('Origin',(-0.0256698380379148,4.01785665389522,
0.191264910989279));
#130256=CARTESIAN_POINT('Ctrl Pts',(1.35207303361503,3.91326598486611,-7.12280833059856));
#130257=CARTESIAN_POINT('Ctrl Pts',(1.36019668436733,3.92008713977612,-7.16361868414385));
#130258=CARTESIAN_POINT('Ctrl Pts',(1.36830495852077,3.92674916152212,-7.2044831231636));
#130259=CARTESIAN_POINT('Ctrl Pts',(1.3844765521872,3.93976378721589,-7.28622131472965));
#130260=CARTESIAN_POINT('Ctrl Pts',(1.39254868926144,3.9461234814825,-7.32713966009896));
#130261=CARTESIAN_POINT('Ctrl Pts',(1.40060026732549,3.95233945647285,-7.36806063659619));
#130262=CARTESIAN_POINT('Ctrl Pts',(1.95508475,4.042807359,-7.24069358700001));
#130263=CARTESIAN_POINT('Ctrl Pts',(1.557951187,3.977102825,-7.347924996));
#130264=CARTESIAN_POINT('Ctrl Pts',(1.151472347,3.912499672,-7.411080315));
#130265=CARTESIAN_POINT('Ctrl Pts',(2.118444839,4.042807359,-6.933591527));
#130266=CARTESIAN_POINT('Ctrl Pts',(1.73815504,3.977102825,-7.04978282));
#130267=CARTESIAN_POINT('Ctrl Pts',(1.347439022,3.912499672,-7.123686411));
#130268=CARTESIAN_POINT('',(1.95508474192627,4.04280736030989,-7.24069356686469));
#130269=CARTESIAN_POINT('Origin',(-0.0669162103268045,4.16063868480358,
0.175490039129509));
#130270=CARTESIAN_POINT('',(2.03758157319294,4.04280736269456,-7.08560705295516));
#130271=CARTESIAN_POINT('Origin',(-1.46475713502792E-13,4.134630322,4.87023615880489E-13));
#130272=CARTESIAN_POINT('',(1.40317543671779,4.13354310063947,-7.36757074555853));
#130273=CARTESIAN_POINT('Origin',(-0.0402218681886213,4.16070815660101,
0.187817616273244));
#130274=CARTESIAN_POINT('Origin',(-0.0539512478212259,4.01786461752988,
0.184401513983244));
#130275=CARTESIAN_POINT('Ctrl Pts',(3.17958655931402,3.912491975,-6.79323254224789));
#130276=CARTESIAN_POINT('Ctrl Pts',(2.81112615420095,3.97753138,-6.96569119870049));
#130277=CARTESIAN_POINT('Ctrl Pts',(2.42617413122656,4.042807359,-7.0972852663583));
#130278=CARTESIAN_POINT('Ctrl Pts',(2.41292795081507,4.04505350226662,-7.10181341183424));
#130279=CARTESIAN_POINT('Ctrl Pts',(2.39968177040358,4.0472996455332,-7.10634155731016));
#130280=CARTESIAN_POINT('Ctrl Pts',(2.855957386,3.912491975,-6.663783266));
#130281=CARTESIAN_POINT('Ctrl Pts',(2.494518222,3.97753138,-6.81868849100001));
#130282=CARTESIAN_POINT('Ctrl Pts',(2.118444839,4.042807359,-6.933591527));
#130283=CARTESIAN_POINT('Ctrl Pts',(2.10550417215875,4.04505350226662,-6.93754533488736));
#130284=CARTESIAN_POINT('Ctrl Pts',(2.09256350531744,4.0472996455332,-6.94149914277462));
#130285=CARTESIAN_POINT('',(2.42554695194231,4.04280735814475,-7.0969516709872));
#130286=CARTESIAN_POINT('',(2.27199585988443,4.04280735744339,-7.01527157445221));
#130287=CARTESIAN_POINT('',(2.95177024883494,3.95233946528638,-6.89471181604777));
#130288=CARTESIAN_POINT('Origin',(-0.0661859235379966,4.01785664201628,
0.181274795380851));
#130289=CARTESIAN_POINT('Ctrl Pts',(2.8516555602423,3.91326598479036,-6.6656252952509));
#130290=CARTESIAN_POINT('Ctrl Pts',(2.8683622922366,3.92008713489517,-6.70373515344066));
#130291=CARTESIAN_POINT('Ctrl Pts',(2.88506563246586,3.9267491516805,-6.74190113461209));
#130292=CARTESIAN_POINT('Ctrl Pts',(2.91843046311368,3.93976378714705,-6.81825197501983));
#130293=CARTESIAN_POINT('Ctrl Pts',(2.93511011255253,3.94612348134051,-6.8564784007494));
#130294=CARTESIAN_POINT('Ctrl Pts',(2.95177024985849,3.95233945647065,-6.89471181703501));
#130295=CARTESIAN_POINT('Ctrl Pts',(3.465911043,4.042807359,-6.651124765));
#130296=CARTESIAN_POINT('Ctrl Pts',(3.101113825,3.977102825,-6.84122114));
#130297=CARTESIAN_POINT('Ctrl Pts',(2.717714761,3.912499672,-6.99028085800001));
#130298=CARTESIAN_POINT('Ctrl Pts',(3.559433999,4.042807359,-6.316084991));
#130299=CARTESIAN_POINT('Ctrl Pts',(3.213012857,3.977102825,-6.51131086100001));
#130300=CARTESIAN_POINT('Ctrl Pts',(2.847318651,3.912499672,-6.667479022));
#130301=CARTESIAN_POINT('',(3.46591103084481,4.04280736030966,-6.6511247470209));
#130302=CARTESIAN_POINT('Origin',(-0.103076933933817,4.1606386869864,0.15700221155554));
#130303=CARTESIAN_POINT('',(3.51314011588116,4.04280736269456,-6.48192968991497));
#130304=CARTESIAN_POINT('Origin',(-4.38885039422132E-13,4.13463032199911,
7.97539118080337E-13));
#130305=CARTESIAN_POINT('',(2.95417990197285,4.13354310061305,-6.89367979403913));
#130306=CARTESIAN_POINT('Origin',(-0.079656774662682,4.16070809307365,0.174780159875999));
#130307=CARTESIAN_POINT('Origin',(-0.09233079221727,4.01786464488332,0.168492434329938));
#130308=CARTESIAN_POINT('Ctrl Pts',(4.56559378250116,3.912491975,-5.95089341838246));
#130309=CARTESIAN_POINT('Ctrl Pts',(4.2428212902823,3.97753138,-6.19852818282084));
#130310=CARTESIAN_POINT('Ctrl Pts',(3.89515806583989,4.042807359,-6.40979896040833));
#130311=CARTESIAN_POINT('Ctrl Pts',(3.88319499132248,4.04505350223884,-6.41706877751275));
#130312=CARTESIAN_POINT('Ctrl Pts',(3.87123191680507,4.04729964547766,-6.42433859461714));
#130313=CARTESIAN_POINT('Ctrl Pts',(4.221703111,3.912491975,-5.8940413));
#130314=CARTESIAN_POINT('Ctrl Pts',(3.902014239,3.97753138,-6.123023663));
#130315=CARTESIAN_POINT('Ctrl Pts',(3.559433999,4.042807359,-6.316084991));
#130316=CARTESIAN_POINT('Ctrl Pts',(3.54764582972819,4.04505350223885,-6.32272822183637));
#130317=CARTESIAN_POINT('Ctrl Pts',(3.53585766045637,4.04729964547766,-6.32937145267288));
#130318=CARTESIAN_POINT('',(3.89447383652341,4.04280735814476,-6.40960798932368));
#130319=CARTESIAN_POINT('',(3.72695387773219,4.04280735744339,-6.36284647384277));
#130320=CARTESIAN_POINT('',(4.36491873504013,3.95233946527757,-6.09897393563535));
#130321=CARTESIAN_POINT('Origin',(-0.103607243489299,4.01785664252565,0.162808653726628));
#130322=CARTESIAN_POINT('Ctrl Pts',(4.21789784076116,3.91326598469089,-5.89676502847127));
#130323=CARTESIAN_POINT('Ctrl Pts',(4.24240649246361,3.9200871405027,-5.93039247398505));
#130324=CARTESIAN_POINT('Ctrl Pts',(4.2669238990547,3.92674916318505,-5.9640754633098));
#130325=CARTESIAN_POINT('Ctrl Pts',(4.31592180509563,3.93976378604036,-6.03146874593862));
#130326=CARTESIAN_POINT('Ctrl Pts',(4.34042904091571,3.94612347918163,-6.06521582155868));
#130327=CARTESIAN_POINT('Ctrl Pts',(4.36491873623229,3.95233945644434,-6.09897393639698));
#130328=CARTESIAN_POINT('Ctrl Pts',(4.814675187,4.042807359,-5.750556742));
#130329=CARTESIAN_POINT('Ctrl Pts',(4.499271827,3.977102825,-6.014629387));
#130330=CARTESIAN_POINT('Ctrl Pts',(4.156879854,3.912499672,-6.242623638));
#130331=CARTESIAN_POINT('Ctrl Pts',(4.833987981,4.042807359,-5.40324534));
#130332=CARTESIAN_POINT('Ctrl Pts',(4.537633764,3.977102825,-5.668377243));
#130333=CARTESIAN_POINT('Ctrl Pts',(4.214060823,3.912499672,-5.899507723));
#130334=CARTESIAN_POINT('',(4.81467517126731,4.04280736030966,-5.75055672705016));
#130335=CARTESIAN_POINT('Origin',(-0.134418047111175,4.16063871796191,0.131173290137131));
#130336=CARTESIAN_POINT('',(4.82442813085483,4.04280736269456,-5.57516449880049));
#130337=CARTESIAN_POINT('Origin',(-8.08164299370695E-13,4.13463032200022,
9.68409380464053E-13));
#130338=CARTESIAN_POINT('',(4.36705019746166,4.13354310060638,-6.09744803724894));
#130339=CARTESIAN_POINT('Origin',(-0.115367111426155,4.16070813913995,0.15357017334568));
#130340=CARTESIAN_POINT('Origin',(-0.126392979154755,4.0178646284018,0.144704703487445));
#130341=CARTESIAN_POINT('Ctrl Pts',(5.7381189155374,3.912491975,-4.83029713213311));
#130342=CARTESIAN_POINT('Ctrl Pts',(5.4761268181007,3.97753138,-5.14152887785456));
#130343=CARTESIAN_POINT('Ctrl Pts',(5.18200873963653,4.042807359,-5.42259757788377));
#130344=CARTESIAN_POINT('Ctrl Pts',(5.171888151756,4.04505350206407,-5.43226913732674));
#130345=CARTESIAN_POINT('Ctrl Pts',(5.16176756387534,4.04729964512812,-5.44194069676973));
#130346=CARTESIAN_POINT('Ctrl Pts',(5.390046691,3.912491975,-4.848700513));
#130347=CARTESIAN_POINT('Ctrl Pts',(5.127056407,3.97753138,-5.141053053));
#130348=CARTESIAN_POINT('Ctrl Pts',(4.833987981,4.042807359,-5.40324534));
#130349=CARTESIAN_POINT('Ctrl Pts',(4.82390351160652,4.04505350206407,-5.41226736304614));
#130350=CARTESIAN_POINT('Ctrl Pts',(4.81381904221294,4.04729964512812,-5.42128938609216));
#130351=CARTESIAN_POINT('',(5.18129945413042,4.04280735814474,-5.42255816067613));
#130352=CARTESIAN_POINT('',(5.00764367496653,4.04280735744339,-5.41290174300688));
#130353=CARTESIAN_POINT('',(5.57396847208562,3.95233946527127,-5.01805481218518));
#130354=CARTESIAN_POINT('Origin',(-0.136184000983926,4.0178566698653,0.13672977369069));
#130355=CARTESIAN_POINT('Ctrl Pts',(5.38691590761031,3.91326598479672,-4.85217858324993));
#130356=CARTESIAN_POINT('Ctrl Pts',(5.4180804633958,3.92008713973162,-4.87975119871123));
#130357=CARTESIAN_POINT('Ctrl Pts',(5.44926550910729,3.92674916150384,-4.90737617685124));
#130358=CARTESIAN_POINT('Ctrl Pts',(5.51160543921952,3.9397637852627,-4.96266074458048));
#130359=CARTESIAN_POINT('Ctrl Pts',(5.54279432879826,3.94612347757219,-4.99035049725823));
#130360=CARTESIAN_POINT('Ctrl Pts',(5.57396847340179,3.95233945642564,-5.01805481268885));
#130361=CARTESIAN_POINT('Ctrl Pts',(5.938310471,4.042807359,-4.581099076));
#130362=CARTESIAN_POINT('Ctrl Pts',(5.687048879,3.977102825,-4.906800249));
#130363=CARTESIAN_POINT('Ctrl Pts',(5.401673864,3.912499672,-5.203068274));
#130364=CARTESIAN_POINT('Ctrl Pts',(5.882510057,4.042807359,-4.237755942));
#130365=CARTESIAN_POINT('Ctrl Pts',(5.65007996,3.977102825,-4.560396605));
#130366=CARTESIAN_POINT('Ctrl Pts',(5.383758195,3.912499672,-4.855682001));
#130367=CARTESIAN_POINT('',(5.93831045237977,4.0428073603099,-4.58109906488038));
#130368=CARTESIAN_POINT('Origin',(-0.159473693902303,4.16063870385668,0.0992105328740411));
#130369=CARTESIAN_POINT('',(5.9101312483988,4.04280736269456,-4.40771081147348));
#130370=CARTESIAN_POINT('Origin',(-7.66747776381749E-13,4.13463032199978,
7.53303669442928E-13));
#130371=CARTESIAN_POINT('',(5.57572207905876,4.13354310060491,-5.01610638780029));
#130372=CARTESIAN_POINT('Origin',(-0.145682930494174,4.16070809090573,0.12517927535747));
#130373=CARTESIAN_POINT('Origin',(-0.154545132451127,4.01786462453061,0.114150754036674));
#130374=CARTESIAN_POINT('Ctrl Pts',(6.64233598404738,3.912491975,-3.48384151984001));
#130375=CARTESIAN_POINT('Ctrl Pts',(6.45337474226534,3.97753138,-3.84411739653553));
#130376=CARTESIAN_POINT('Ctrl Pts',(6.22655444281494,4.042807359,-4.1818415599671));
#130377=CARTESIAN_POINT('Ctrl Pts',(6.21874956738325,4.04505350225091,-4.19346263194456));
#130378=CARTESIAN_POINT('Ctrl Pts',(6.21094469195147,4.04729964550179,-4.20508370392205));
#130379=CARTESIAN_POINT('Ctrl Pts',(6.306357679,3.912491975,-3.57663988));
#130380=CARTESIAN_POINT('Ctrl Pts',(6.112363115,3.97753138,-3.918692517));
#130381=CARTESIAN_POINT('Ctrl Pts',(5.882510057,4.042807359,-4.237755942));
#130382=CARTESIAN_POINT('Ctrl Pts',(5.87460082449465,4.04505350225091,-4.24873489887897));
#130383=CARTESIAN_POINT('Ctrl Pts',(5.8666915919893,4.04729964550179,-4.25971385575793));
#130384=CARTESIAN_POINT('',(6.22585326643108,4.04280735814475,-4.18195553973078));
#130385=CARTESIAN_POINT('',(6.05418161852976,4.04280735744339,-4.20985574286674));
#130386=CARTESIAN_POINT('',(6.52238563876683,3.95233946529696,-3.70249702295116));
#130387=CARTESIAN_POINT('Origin',(-0.162393127489747,4.01785661752674,0.104257678319604));
#130388=CARTESIAN_POINT('Ctrl Pts',(6.30404777361277,3.91326598474248,-3.58070966061121));
#130389=CARTESIAN_POINT('Ctrl Pts',(6.3404110065364,3.92008713781498,-3.6009381796591));
#130390=CARTESIAN_POINT('Ctrl Pts',(6.37680550547289,3.92674915766183,-3.62121343168818));
#130391=CARTESIAN_POINT('Ctrl Pts',(6.44957254934357,3.93976378842026,-3.66180425625756));
#130392=CARTESIAN_POINT('Ctrl Pts',(6.4859847578353,3.94612348394098,-3.68214195945266));
#130393=CARTESIAN_POINT('Ctrl Pts',(6.52238564019206,3.95233945650218,-3.70249702308815));
#130394=CARTESIAN_POINT('Ctrl Pts',(6.784276957,4.042807359,-3.19743431));
#130395=CARTESIAN_POINT('Ctrl Pts',(6.608905846,3.977102825,-3.569534585));
#130396=CARTESIAN_POINT('Ctrl Pts',(6.393891608,3.912499672,-3.920223221));
#130397=CARTESIAN_POINT('Ctrl Pts',(6.655972501,4.042807359,-2.874113787));
#130398=CARTESIAN_POINT('Ctrl Pts',(6.498334696,3.977102825,-3.23917689));
#130399=CARTESIAN_POINT('Ctrl Pts',(6.301717018,3.912499672,-3.584809985));
#130400=CARTESIAN_POINT('',(6.78427693644271,4.04280736030966,-3.19743430304974));
#130401=CARTESIAN_POINT('Origin',(-0.177072652585477,4.16063872579149,0.0626089307403355));
#130402=CARTESIAN_POINT('',(6.71948319740546,4.04280736269456,-3.0341574665131));
#130403=CARTESIAN_POINT('Origin',(-2.02528965820292E-13,4.13463032200022,
1.0321604682062E-13));
#130404=CARTESIAN_POINT('',(6.52367939390571,4.13354310057799,-3.70021717765555));
#130405=CARTESIAN_POINT('Origin',(-0.169186457818068,4.16070813326555,0.0909349252870628));
#130406=CARTESIAN_POINT('Origin',(-0.175471187222578,4.01786465903462,0.0782594480763255));
#130407=CARTESIAN_POINT('Ctrl Pts',(7.23596480548825,3.912491975,-1.97448535086908));
#130408=CARTESIAN_POINT('Ctrl Pts',(7.12887003564431,3.97753138,-2.36695925973825));
#130409=CARTESIAN_POINT('Ctrl Pts',(6.97995338116804,4.042807359,-2.74554727906954));
#130410=CARTESIAN_POINT('Ctrl Pts',(6.97482916644641,4.04505350221171,-2.75857447410635));
#130411=CARTESIAN_POINT('Ctrl Pts',(6.96970495172464,4.04729964542339,-2.77160166914315));
#130412=CARTESIAN_POINT('Ctrl Pts',(6.92779039,3.912491975,-2.137339541));
#130413=CARTESIAN_POINT('Ctrl Pts',(6.811862518,3.97753138,-2.513098274));
#130414=CARTESIAN_POINT('Ctrl Pts',(6.655972501,4.042807359,-2.874113787));
#130415=CARTESIAN_POINT('Ctrl Pts',(6.65060833321854,4.04505350221171,-2.88653631296233));
#130416=CARTESIAN_POINT('Ctrl Pts',(6.64524416543696,4.04729964542339,-2.89895883892467));
#130417=CARTESIAN_POINT('',(6.97929310018125,4.04280735814474,-2.74580932624543));
#130418=CARTESIAN_POINT('',(6.81763275884877,4.04280735744339,-2.80996156785876));
#130419=CARTESIAN_POINT('',(7.16582330193381,3.95233946527704,-2.21381458834179));
#130420=CARTESIAN_POINT('Origin',(-0.181008804869115,4.01785668701233,0.0669104859044277));
#130421=CARTESIAN_POINT('Ctrl Pts',(6.92640937123344,3.91326598469505,-2.14181073366623));
#130422=CARTESIAN_POINT('Ctrl Pts',(6.96627100041619,3.92008714027779,-2.15374930542941));
#130423=CARTESIAN_POINT('Ctrl Pts',(7.00617321276977,3.92674916271554,-2.16572679693359));
#130424=CARTESIAN_POINT('Ctrl Pts',(7.08596478508344,3.93976378594542,-2.18972585333134));
#130425=CARTESIAN_POINT('Ctrl Pts',(7.12589768481122,3.94612347897943,-2.20176051882883));
#130426=CARTESIAN_POINT('Ctrl Pts',(7.16582330334321,3.95233945644287,-2.21381458822912));
#130427=CARTESIAN_POINT('Ctrl Pts',(7.313018193,4.042807359,-1.664261068));
#130428=CARTESIAN_POINT('Ctrl Pts',(7.221737721,3.977102825,-2.065361451));
#130429=CARTESIAN_POINT('Ctrl Pts',(7.087138087,3.912499672,-2.454072887));
#130430=CARTESIAN_POINT('Ctrl Pts',(7.118209069,4.042807359,-1.376081265));
#130431=CARTESIAN_POINT('Ctrl Pts',(7.042734524,3.977102825,-1.766496865));
#130432=CARTESIAN_POINT('Ctrl Pts',(6.925014556,3.912499672,-2.146316238));
#130433=CARTESIAN_POINT('',(7.31301817143122,4.04280736030966,-1.66426106564211));
#130434=CARTESIAN_POINT('Origin',(-0.186391878506125,4.16063870704355,0.0230797878023903));
#130435=CARTESIAN_POINT('',(7.21463958071766,4.04280736269456,-1.51873028963318));
#130436=CARTESIAN_POINT('Origin',(7.93635990259389E-14,4.134630322,5.48606299277665E-14));
#130437=CARTESIAN_POINT('',(7.16659671034123,4.13354310061321,-2.21130992580493));
#130438=CARTESIAN_POINT('Origin',(-0.184779512955822,4.16070810473172,0.0524389094179195));
#130439=CARTESIAN_POINT('Origin',(-0.188191923671757,4.01786463325267,0.0387085766334819));
#130440=CARTESIAN_POINT('Ctrl Pts',(7.49124795482483,3.912491975,-0.372804441010172));
#130441=CARTESIAN_POINT('Ctrl Pts',(7.4710272900667,3.97753138,-0.779124736979639));
#130442=CARTESIAN_POINT('Ctrl Pts',(7.40697745695167,4.042807359,-1.18087425843626));
#130443=CARTESIAN_POINT('Ctrl Pts',(7.40477350540734,4.04505350216274,-1.19469843931525));
#130444=CARTESIAN_POINT('Ctrl Pts',(7.40256955386291,4.04729964532543,-1.20852262019425));
#130445=CARTESIAN_POINT('Ctrl Pts',(7.225287322,3.912491975,-0.59809958));
#130446=CARTESIAN_POINT('Ctrl Pts',(7.19284679999999,3.97753138,-0.989994349));
#130447=CARTESIAN_POINT('Ctrl Pts',(7.118209069,4.042807359,-1.376081265));
#130448=CARTESIAN_POINT('Ctrl Pts',(7.11564078842061,4.04505350216274,-1.38936649641096));
#130449=CARTESIAN_POINT('Ctrl Pts',(7.1130725078412,4.04729964532544,-1.40265172782197));
#130450=CARTESIAN_POINT('',(7.40638894538665,4.04280735814476,-1.18127211997347));
#130451=CARTESIAN_POINT('',(7.26229896883851,4.04280735744341,-1.27867671243651));
#130452=CARTESIAN_POINT('',(7.47419503215417,3.95233946528439,-0.621616643560051));
#130453=CARTESIAN_POINT('Origin',(-0.191160705533955,4.01785662612324,0.0264346106921929));
#130454=CARTESIAN_POINT('Ctrl Pts',(7.22489976603804,3.91326598485069,-0.602763116835091));
#130455=CARTESIAN_POINT('Ctrl Pts',(7.26639587926392,3.92008713822626,-0.605853498624219));
#130456=CARTESIAN_POINT('Ctrl Pts',(7.30793999166212,3.92674915839138,-0.608973165802315));
#130457=CARTESIAN_POINT('Ctrl Pts',(7.39102520304202,3.93976378691293,-0.61525831079887));
#130458=CARTESIAN_POINT('Ctrl Pts',(7.43261159764799,3.94612348087459,-0.618427219959677));
#130459=CARTESIAN_POINT('Ctrl Pts',(7.47419503350602,3.95233945646465,-0.621616643123829));
#130460=CARTESIAN_POINT('Ctrl Pts',(7.499810826,4.042807359,-0.0532688290000001));
#130461=CARTESIAN_POINT('Ctrl Pts',(7.496889167,3.977102825,-0.464614311));
#130462=CARTESIAN_POINT('Ctrl Pts',(7.448997866,3.912499672,-0.873172832));
#130463=CARTESIAN_POINT('Ctrl Pts',(7.247606092,4.042807359,0.186295287));
#130464=CARTESIAN_POINT('Ctrl Pts',(7.257823913,3.977102825,-0.211217409));
#130465=CARTESIAN_POINT('Ctrl Pts',(7.224506111,3.912499672,-0.60746313));
#130466=CARTESIAN_POINT('',(7.49981080442722,4.04280736030966,-0.0532688313318097));
#130467=CARTESIAN_POINT('Origin',(-0.18699551190703,4.16063870247584,-0.0175285563611807));
#130468=CARTESIAN_POINT('',(7.37244743553787,4.04280736269456,0.0677110269473681));
#130469=CARTESIAN_POINT('Origin',(-1.32706345912226E-13,4.13463032200111,
4.27649994409751E-14));
#130470=CARTESIAN_POINT('',(7.47441192976062,4.13354310062207,-0.619004279110432));
#130471=CARTESIAN_POINT('Origin',(-0.19173213084235,4.1607081265445,0.01149076061306));
#130472=CARTESIAN_POINT('Origin',(-0.192113445256573,4.01786460469813,-0.00265210371298302));
#130473=CARTESIAN_POINT('Ctrl Pts',(7.3962486753266,3.912491975,1.24630839070828));
#130474=CARTESIAN_POINT('Ctrl Pts',(7.46384761202233,3.97753138,0.845140791482356));
#130475=CARTESIAN_POINT('Ctrl Pts',(7.4876594991711,4.042807359,0.439015130657355));
#130476=CARTESIAN_POINT('Ctrl Pts',(7.48847886501099,4.04505350215634,0.425040367082017));
#130477=CARTESIAN_POINT('Ctrl Pts',(7.4892982308509,4.04729964531265,0.411065603506677));
#130478=CARTESIAN_POINT('Ctrl Pts',(7.18493785000001,3.912491975,0.969106852));
#130479=CARTESIAN_POINT('Ctrl Pts',(7.23750156,3.97753138,0.579400611999999));
#130480=CARTESIAN_POINT('Ctrl Pts',(7.247606092,4.042807359,0.186295287));
#130481=CARTESIAN_POINT('Ctrl Pts',(7.24795378843822,4.04505350215634,0.172768552525941));
#130482=CARTESIAN_POINT('Ctrl Pts',(7.24830148487646,4.04729964531265,0.159241818051882));
#130483=CARTESIAN_POINT('',(7.4871702751445,4.04280735814474,0.438500058308231));
#130484=CARTESIAN_POINT('',(7.36738815040593,4.04280735744339,0.312397644926896));
#130485=CARTESIAN_POINT('',(7.43308170904286,3.95233946527388,0.999647404285365));
#130486=CARTESIAN_POINT('Origin',(-0.192373731644399,4.01785666929138,-0.0152772730488699));
#130487=CARTESIAN_POINT('Ctrl Pts',(7.18556187680774,3.91326598473617,0.96446903296805));
#130488=CARTESIAN_POINT('Ctrl Pts',(7.22675217651942,3.92008713843996,0.970371340687591));
#130489=CARTESIAN_POINT('Ctrl Pts',(7.26799564899922,3.9267491589428,0.976255366041739));
#130490=CARTESIAN_POINT('Ctrl Pts',(7.35048948246961,3.93976378556259,0.987978026920435));
#130491=CARTESIAN_POINT('Ctrl Pts',(7.39178482283155,3.94612347820117,0.993823049286259));
#130492=CARTESIAN_POINT('Ctrl Pts',(7.43308171027695,3.95233945643343,0.999647404970062));
#130493=CARTESIAN_POINT('Ctrl Pts',(7.33592064100001,4.042807359,1.560214201));
#130494=CARTESIAN_POINT('Ctrl Pts',(7.421494407,3.977102825,1.157857678));
#130495=CARTESIAN_POINT('Ctrl Pts',(7.462550783,3.912499672,0.748555814));
#130496=CARTESIAN_POINT('Ctrl Pts',(7.038113109,4.042807359,1.739960879));
#130497=CARTESIAN_POINT('Ctrl Pts',(7.133545523,3.977102825,1.353938339));
#130498=CARTESIAN_POINT('Ctrl Pts',(7.18618778900001,3.912499672,0.95979428));
#130499=CARTESIAN_POINT('',(7.33592062045006,4.04280736030989,1.56021419403977));
#130500=CARTESIAN_POINT('Origin',(-0.178855668896493,4.16063873214872,-0.0573172701771181));
#130501=CARTESIAN_POINT('',(7.18552784240835,4.04280736269456,1.65098625133119));
#130502=CARTESIAN_POINT('Origin',(-8.49580822359641E-13,4.13463032200089,
-9.39732233001811E-14));
#130503=CARTESIAN_POINT('',(7.43273195498472,4.13354310059326,1.00224532016575));
#130504=CARTESIAN_POINT('Origin',(-0.189719945425788,4.16070812904751,-0.0299946459788324));
#130505=CARTESIAN_POINT('Origin',(-0.187051916916066,4.01786466354787,-0.0438888126460474));
#130506=CARTESIAN_POINT('Ctrl Pts',(6.95540902751334,3.912491975,2.80714522631661));
#130507=CARTESIAN_POINT('Ctrl Pts',(7.10766671470722,3.97753138,2.42988847618128));
#130508=CARTESIAN_POINT('Ctrl Pts',(7.21822690572252,4.042807359,2.03837665990852));
#130509=CARTESIAN_POINT('Ctrl Pts',(7.22203127675693,4.04505350240363,2.0249047565065));
#130510=CARTESIAN_POINT('Ctrl Pts',(7.22583564779146,4.04729964580723,2.01143285310446));
#130511=CARTESIAN_POINT('Ctrl Pts',(6.80862866900001,3.912491975,2.490998925));
#130512=CARTESIAN_POINT('Ctrl Pts',(6.943738791,3.97753138,2.121703444));
#130513=CARTESIAN_POINT('Ctrl Pts',(7.038113109,4.042807359,1.739960879));
#130514=CARTESIAN_POINT('Ctrl Pts',(7.04136052489626,4.04505350240363,1.72682513508024));
#130515=CARTESIAN_POINT('Ctrl Pts',(7.04460794079238,4.04729964580723,1.71368939116042));
#130516=CARTESIAN_POINT('',(7.21785984476897,4.04280735814474,2.03776846087977));
#130517=CARTESIAN_POINT('',(7.12798645045437,4.04280735744339,1.88886463573798));
#130518=CARTESIAN_POINT('',(7.04440574707233,3.95233946528394,2.5741690509787));
#130519=CARTESIAN_POINT('Origin',(-0.184592186119418,4.01785669121865,-0.0562748305058976));
#130520=CARTESIAN_POINT('Ctrl Pts',(6.81023510049717,3.91326598479217,2.48660368253256));
#130521=CARTESIAN_POINT('Ctrl Pts',(6.84919357950587,3.92008713976044,2.50122269724142));
#130522=CARTESIAN_POINT('Ctrl Pts',(6.88820791922027,3.92674916155891,2.51583528793693));
#130523=CARTESIAN_POINT('Ctrl Pts',(6.9662530591139,3.9397637868083,2.54501761238485));
#130524=CARTESIAN_POINT('Ctrl Pts',(7.00532643854862,3.94612348068096,2.55960326201085));
#130525=CARTESIAN_POINT('Ctrl Pts',(7.04440574811698,3.95233945646352,2.57416905194011));
#130526=CARTESIAN_POINT('Ctrl Pts',(6.829010959,4.042807359,3.10074335));
#130527=CARTESIAN_POINT('Ctrl Pts',(6.999078818,3.977102825,2.726189529));
#130528=CARTESIAN_POINT('Ctrl Pts',(7.12716312,3.912499672,2.335282822));
#130529=CARTESIAN_POINT('Ctrl Pts',(6.49952578000001,4.042807359,3.212267834));
#130530=CARTESIAN_POINT('Ctrl Pts',(6.675710472,3.977102825,2.855785434));
#130531=CARTESIAN_POINT('Ctrl Pts',(6.81185131300001,3.912499672,2.482172775));
#130532=CARTESIAN_POINT('',(6.82901094038103,4.04280736030966,3.10074333884465));
#130533=CARTESIAN_POINT('Origin',(-0.162352327731182,4.16063870640799,-0.0944257980160096));
#130534=CARTESIAN_POINT('',(6.66262095329685,4.04280736269456,3.15706319396646));
#130535=CARTESIAN_POINT('Origin',(-1.58727198051878E-13,4.13463032199933,
1.01915004213637E-14));
#130536=CARTESIAN_POINT('',(7.04350569485826,4.13354310058752,2.57663104168863));
#130537=CARTESIAN_POINT('Origin',(-0.178836261171845,4.16070812928274,-0.0700775177326174));
#130538=CARTESIAN_POINT('Origin',(-0.17324391522071,4.01786469226385,-0.0830733358114233));
#130539=CARTESIAN_POINT('Ctrl Pts',(6.18934218547474,3.912491975,4.23672307189534));
#130540=CARTESIAN_POINT('Ctrl Pts',(6.41913922087722,3.97753138,3.90101727661634));
#130541=CARTESIAN_POINT('Ctrl Pts',(6.61127804412574,4.042807359,3.54242596097349));
#130542=CARTESIAN_POINT('Ctrl Pts',(6.61788953126837,4.04505350211977,3.53008685202745));
#130543=CARTESIAN_POINT('Ctrl Pts',(6.62450101841088,4.04729964523953,3.51774774308143));
#130544=CARTESIAN_POINT('Ctrl Pts',(6.113955579,3.912491975,3.896414657));
#130545=CARTESIAN_POINT('Ctrl Pts',(6.325294513,3.97753138,3.564797781));
#130546=CARTESIAN_POINT('Ctrl Pts',(6.49952578,4.042807359,3.212267834));
#130547=CARTESIAN_POINT('Ctrl Pts',(6.50552106904223,4.04505350211977,3.20013729644091));
#130548=CARTESIAN_POINT('Ctrl Pts',(6.51151635808462,4.04729964523953,3.18800675888175));
#130549=CARTESIAN_POINT('',(6.61105030969852,4.04280735814475,3.54175307414439));
#130550=CARTESIAN_POINT('',(6.55528802638805,4.04280735744339,3.37701041498213));
#130551=CARTESIAN_POINT('',(6.32634120131164,3.95233946527627,4.02832541343909));
#130552=CARTESIAN_POINT('Origin',(-0.168179181945322,4.01785664306235,-0.094641074836807));
#130553=CARTESIAN_POINT('Ctrl Pts',(6.1164693003912,3.9132659848096,3.89246750855191));
#130554=CARTESIAN_POINT('Ctrl Pts',(6.15137427892296,3.92008713647702,3.91511964903297));
#130555=CARTESIAN_POINT('Ctrl Pts',(6.18633519089755,3.92674915487793,3.93777752275454));
#130556=CARTESIAN_POINT('Ctrl Pts',(6.25628237277549,3.93976378592067,3.98305499865668));
#130557=CARTESIAN_POINT('Ctrl Pts',(6.29130674935267,3.94612347887328,4.00569926190145));
#130558=CARTESIAN_POINT('Ctrl Pts',(6.32634120213922,3.9523394564405,4.02832541458508));
#130559=CARTESIAN_POINT('Ctrl Pts',(6.002784315,4.042807359,4.496285186));
#130560=CARTESIAN_POINT('Ctrl Pts',(6.249394081,3.977102825,4.167047787));
#130561=CARTESIAN_POINT('Ctrl Pts',(6.45851723100001,3.912499672,3.812814601));
#130562=CARTESIAN_POINT('Ctrl Pts',(5.657027848,4.042807359,4.534372715));
#130563=CARTESIAN_POINT('Ctrl Pts',(5.905726619,3.977102825,4.224099176));
#130564=CARTESIAN_POINT('Ctrl Pts',(6.119000241,3.912499672,3.888487631));
#130565=CARTESIAN_POINT('',(6.00278429926573,4.0428073603099,4.49628517105897));
#130566=CARTESIAN_POINT('Origin',(-0.138258169227965,4.16063871858951,-0.127119332806599));
#130567=CARTESIAN_POINT('',(5.82817731302716,4.04280736269456,4.51551937025311));
#130568=CARTESIAN_POINT('Origin',(-9.12030867494806E-13,4.13463032200044,
-4.96130914129367E-13));
#130569=CARTESIAN_POINT('',(6.32493293650023,4.13354310060994,4.0305363596011));
#130570=CARTESIAN_POINT('Origin',(-0.159590726451847,4.16070811817244,-0.106883739022645));
#130571=CARTESIAN_POINT('Origin',(-0.151335490861449,4.01786464595953,-0.118373611190034));
#130572=CARTESIAN_POINT('Ctrl Pts',(5.13386858061938,3.912491975,5.46819645487303));
#130573=CARTESIAN_POINT('Ctrl Pts',(5.43045991205592,3.97753138,5.18973884414867));
#130574=CARTESIAN_POINT('Ctrl Pts',(5.69519316883271,4.042807359,4.88083536282829));
#130575=CARTESIAN_POINT('Ctrl Pts',(5.70430262685269,4.04505350214671,4.87020600960848));
#130576=CARTESIAN_POINT('Ctrl Pts',(5.71341208487259,4.04729964529339,4.85957665638869));
#130577=CARTESIAN_POINT('Ctrl Pts',(5.133400721,3.912491975,5.11963837));
#130578=CARTESIAN_POINT('Ctrl Pts',(5.411086494,3.97753138,4.841206136));
#130579=CARTESIAN_POINT('Ctrl Pts',(5.657027848,4.042807359,4.534372715));
#130580=CARTESIAN_POINT('Ctrl Pts',(5.66549067759277,4.04505350214671,4.52381459245147));
#130581=CARTESIAN_POINT('Ctrl Pts',(5.6739535071854,4.04729964529339,4.51325646990289));
#130582=CARTESIAN_POINT('',(5.69511540948553,4.04280735814474,4.88012925152558));
#130583=CARTESIAN_POINT('',(5.67607161911655,4.04280735744339,4.70725094112458));
#130584=CARTESIAN_POINT('',(5.31246397217453,3.9523394652784,5.294121756425));
#130585=CARTESIAN_POINT('Origin',(-0.143902203581194,4.01785668194033,-0.128581964472328));
#130586=CARTESIAN_POINT('Ctrl Pts',(5.13670419329786,3.91326598482771,5.11632387889823));
#130587=CARTESIAN_POINT('Ctrl Pts',(5.16592358955759,3.92008714054823,5.14594998118222));
#130588=CARTESIAN_POINT('Ctrl Pts',(5.19519638141407,3.92674916312298,5.17559370893724));
#130589=CARTESIAN_POINT('Ctrl Pts',(5.25377488201198,3.93976378613899,5.23484916257931));
#130590=CARTESIAN_POINT('Ctrl Pts',(5.28311256198989,3.94612347931016,5.26449322226433));
#130591=CARTESIAN_POINT('Ctrl Pts',(5.31246397273214,3.95233945644694,5.29412175772542));
#130592=CARTESIAN_POINT('Ctrl Pts',(4.895874148,4.042807359,5.681585723));
#130593=CARTESIAN_POINT('Ctrl Pts',(5.207494623,3.977102825,5.413059522));
#130594=CARTESIAN_POINT('Ctrl Pts',(5.487878254,3.912499672,5.112063406));
#130595=CARTESIAN_POINT('Ctrl Pts',(4.550013582,4.042807359,5.644455368));
#130596=CARTESIAN_POINT('Ctrl Pts',(4.85959755300001,3.977102825,5.39489873600001));
#130597=CARTESIAN_POINT('Ctrl Pts',(5.14003151800001,3.912499672,5.112981126));
#130598=CARTESIAN_POINT('',(4.89587413578614,4.04280736030966,5.68158570505802));
#130599=CARTESIAN_POINT('Origin',(-0.107698786012628,4.16063874448231,-0.153868688590458));
#130600=CARTESIAN_POINT('',(4.72121457955431,4.04280736269456,5.66283487923137));
#130601=CARTESIAN_POINT('Origin',(-3.95516952522712E-13,4.13463032200044,
-2.42861286636753E-13));
#130602=CARTESIAN_POINT('',(5.31061334356406,4.13354310060541,5.29597827693931));
#130603=CARTESIAN_POINT('Origin',(-0.13288273199195,4.16070809434328,-0.138692140882561));
#130604=CARTESIAN_POINT('Origin',(-0.122350310308714,4.01786464218424,-0.148138533803406));
#130605=CARTESIAN_POINT('Ctrl Pts',(3.83834098716584,3.912491975,6.44398304893183));
#130606=CARTESIAN_POINT('Ctrl Pts',(4.18785833280819,3.97753138,6.23579399218282));
#130607=CARTESIAN_POINT('Ctrl Pts',(4.51280739112009,4.042807359,5.99102232646896));
#130608=CARTESIAN_POINT('Ctrl Pts',(4.52398887228891,4.04505350223783,5.98259974544947));
#130609=CARTESIAN_POINT('Ctrl Pts',(4.53517035345769,4.04729964547563,5.97417716442989));
#130610=CARTESIAN_POINT('Ctrl Pts',(3.912813751,3.912491975,6.10347348200001));
#130611=CARTESIAN_POINT('Ctrl Pts',(4.243862085,3.97753138,5.891245072));
#130612=CARTESIAN_POINT('Ctrl Pts',(4.550013582,4.042807359,5.644455368));
#130613=CARTESIAN_POINT('Ctrl Pts',(4.56054824000545,4.04505350223783,5.63596334638202));
#130614=CARTESIAN_POINT('Ctrl Pts',(4.57108289801093,4.04729964547563,5.62747132476391));
#130615=CARTESIAN_POINT('',(4.51288324280057,4.04280735814475,5.99031600768151));
#130616=CARTESIAN_POINT('',(4.53144841205905,4.04280735744339,5.81738564461189));
#130617=CARTESIAN_POINT('',(4.0501818321928,3.95233946528875,6.31237085081574));
#130618=CARTESIAN_POINT('Origin',(-0.112896553892237,4.01785663290102,-0.15651054669219));
#130619=CARTESIAN_POINT('Ctrl Pts',(3.91675250729274,3.91326598481149,6.10094663167513));
#130620=CARTESIAN_POINT('Ctrl Pts',(3.93892001924894,3.9200871359772,6.13616137514948));
#130621=CARTESIAN_POINT('Ctrl Pts',(3.96113588749605,3.9267491538669,6.17140480746271));
#130622=CARTESIAN_POINT('Ctrl Pts',(4.00560672030579,3.93976378742859,6.24186760464295));
#130623=CARTESIAN_POINT('Ctrl Pts',(4.02788591000546,3.94612348192951,6.27712534449124));
#130624=CARTESIAN_POINT('Ctrl Pts',(4.0501818324289,3.95233945647772,6.31237085222031));
#130625=CARTESIAN_POINT('Ctrl Pts',(3.560038347,4.042807359,6.601221627));
#130626=CARTESIAN_POINT('Ctrl Pts',(3.922098505,3.977102825,6.40596261));
#130627=CARTESIAN_POINT('Ctrl Pts',(4.26063218900001,3.912499672,6.172277809));
#130628=CARTESIAN_POINT('Ctrl Pts',(3.230245738,4.042807359,6.490609561));
#130629=CARTESIAN_POINT('Ctrl Pts',(3.586239107,3.977102825,6.313438827));
#130630=CARTESIAN_POINT('Ctrl Pts',(3.920720634,3.912499672,6.098397307));
#130631=CARTESIAN_POINT('',(3.56003833892888,4.04280736030966,6.60122160685206));
#130632=CARTESIAN_POINT('Origin',(-0.0721035891149052,4.16063868785459,
-0.173423303239003));
#130633=CARTESIAN_POINT('',(3.39349309954857,4.04280736269456,6.54536252325234));
#130634=CARTESIAN_POINT('Origin',(-5.67037736209919E-13,4.13463032199956,
-8.59989163215502E-13));
#130635=CARTESIAN_POINT('',(4.04797537267607,4.13354310057253,6.31378613641161));
#130636=CARTESIAN_POINT('Origin',(-0.0999613416876721,4.16070812441472,
-0.164015522838298));
#130637=CARTESIAN_POINT('Origin',(-0.0876443290261331,4.01786465820202,
-0.170976672463546));
#130638=CARTESIAN_POINT('Ctrl Pts',(2.3633368354835,3.912491975,7.11845615806791));
#130639=CARTESIAN_POINT('Ctrl Pts',(2.74943715310942,3.97753138,6.99027034331523));
#130640=CARTESIAN_POINT('Ctrl Pts',(3.11940775541563,4.042807359,6.82107574487869));
#130641=CARTESIAN_POINT('Ctrl Pts',(3.13213842513397,4.04505350213681,6.81525376730157));
#130642=CARTESIAN_POINT('Ctrl Pts',(3.14486909485237,4.0472996452736,6.80943178972441));
#130643=CARTESIAN_POINT('Ctrl Pts',(2.509267959,3.912491975,6.801916959));
#130644=CARTESIAN_POINT('Ctrl Pts',(2.878199401,3.97753138,6.665815937));
#130645=CARTESIAN_POINT('Ctrl Pts',(3.230245738,4.042807359,6.490609561));
#130646=CARTESIAN_POINT('Ctrl Pts',(3.24235963465547,4.04505350213681,6.4845807184609));
#130647=CARTESIAN_POINT('Ctrl Pts',(3.25447353131099,4.0472996452736,6.47855187592175));
#130648=CARTESIAN_POINT('',(3.11963367137329,4.04280735814475,6.82040224533391));
#130649=CARTESIAN_POINT('',(3.1749397136481,4.04280735744339,6.65550586087452));
#130650=CARTESIAN_POINT('',(2.59851769115575,3.95233946526203,7.03546049927267));
#130651=CARTESIAN_POINT('Origin',(-0.0766118672617057,4.01785667276765,
-0.177120613451401));
#130652=CARTESIAN_POINT('Ctrl Pts',(2.51365782782729,3.91326598475245,6.80029589983965));
#130653=CARTESIAN_POINT('Ctrl Pts',(2.52773696267312,3.92008714372177,6.8394527469043));
#130654=CARTESIAN_POINT('Ctrl Pts',(2.54185715832841,3.92674916966057,6.87864801310127));
#130655=CARTESIAN_POINT('Ctrl Pts',(2.5701408276257,3.93976378413994,6.95702322897541));
#130656=CARTESIAN_POINT('Ctrl Pts',(2.58431976246207,3.94612347533749,6.99624600796395));
#130657=CARTESIAN_POINT('Ctrl Pts',(2.59851769116312,3.95233945639798,7.03546050067506));
#130658=CARTESIAN_POINT('Ctrl Pts',(2.057739109,4.042807359,7.212191744));
#130659=CARTESIAN_POINT('Ctrl Pts',(2.453309419,3.977102825,7.099330006));
#130660=CARTESIAN_POINT('Ctrl Pts',(2.834163698,3.912499672,6.94388336100001));
#130661=CARTESIAN_POINT('Ctrl Pts',(1.759435193,4.042807359,7.033270065));
#130662=CARTESIAN_POINT('Ctrl Pts',(2.145192105,3.977102825,6.93676953500001));
#130663=CARTESIAN_POINT('Ctrl Pts',(2.518081211,3.912499672,6.798659207));
#130664=CARTESIAN_POINT('',(2.05773910548016,4.04280736030967,7.21219172259054));
#130665=CARTESIAN_POINT('Origin',(-0.0331369552820981,4.16063867128506,
-0.184868880908445));
#130666=CARTESIAN_POINT('',(1.90709565328332,4.04280736269456,7.12183629025041));
#130667=CARTESIAN_POINT('Origin',(9.0205620750794E-14,4.13463032200022,
4.76181594155634E-13));
#130668=CARTESIAN_POINT('',(2.59605857272175,4.1335431006069,7.03636837301566));
#130669=CARTESIAN_POINT('Origin',(-0.0623657656160265,4.16070813488204,
-0.181669549789484));
#130670=CARTESIAN_POINT('Origin',(-0.048840390273833,4.01786463811681,-0.185820511644359));
#130671=CARTESIAN_POINT('Ctrl Pts',(0.777825678986312,3.912491975,7.46007816895252));
#130672=CARTESIAN_POINT('Ctrl Pts',(1.18245534728826,3.97753138,7.41788942182325));
#130673=CARTESIAN_POINT('Ctrl Pts',(1.5801480792901,4.042807359,7.33218324370478));
#130674=CARTESIAN_POINT('Ctrl Pts',(1.59383266704732,4.04505350229402,7.32923409824292));
#130675=CARTESIAN_POINT('Ctrl Pts',(1.60751725480453,4.04729964558801,7.32628495278109));
#130676=CARTESIAN_POINT('Ctrl Pts',(0.988391585,3.912491975,7.182310358));
#130677=CARTESIAN_POINT('Ctrl Pts',(1.377955312,3.97753138,7.128700657));
#130678=CARTESIAN_POINT('Ctrl Pts',(1.759435193,4.042807359,7.033270065));
#130679=CARTESIAN_POINT('Ctrl Pts',(1.77256189733497,4.04505350229402,7.02998630292476));
#130680=CARTESIAN_POINT('Ctrl Pts',(1.78568860166998,4.04729964558801,7.02670254084949));
#130681=CARTESIAN_POINT('',(1.58051349599226,4.04280735814474,7.33157405540269));
#130682=CARTESIAN_POINT('',(1.66997436233271,4.04280735744341,7.18242202083006));
#130683=CARTESIAN_POINT('',(1.02534975047086,3.95233946528273,7.42957983493419));
#130684=CARTESIAN_POINT('Origin',(-0.036745124488227,4.01785670278804,-0.189449450308088));
#130685=CARTESIAN_POINT('Ctrl Pts',(0.993027301226501,3.91326598480419,
7.18167089032804));
#130686=CARTESIAN_POINT('Ctrl Pts',(0.998359708367689,3.92008714285065,
7.22293886440218));
#130687=CARTESIAN_POINT('Ctrl Pts',(1.003723957203,3.92674916782895,7.26425318546155));
#130688=CARTESIAN_POINT('Ctrl Pts',(1.01449801886883,3.93976378664668,7.34687621292028));
#130689=CARTESIAN_POINT('Ctrl Pts',(1.01991372227921,3.94612348037166,7.38823005464852));
#130690=CARTESIAN_POINT('Ctrl Pts',(1.02534975011445,3.95233945645996,7.42957983630734));
#130691=CARTESIAN_POINT('Ctrl Pts',(0.459222278,4.042807359,7.485927791));
#130692=CARTESIAN_POINT('Ctrl Pts',(0.869806311,3.977102825,7.460740622));
#130693=CARTESIAN_POINT('Ctrl Pts',(1.275172863,3.912499672,7.390800645));
#130694=CARTESIAN_POINT('Ctrl Pts',(0.206355414,4.042807359,7.247062677));
#130695=CARTESIAN_POINT('Ctrl Pts',(0.603838305,3.977102825,7.235744609));
#130696=CARTESIAN_POINT('Ctrl Pts',(0.997699109,3.912499672,7.181023359));
#130697=CARTESIAN_POINT('',(0.459222279251959,4.04280736030989,7.48592776935031));
#130698=CARTESIAN_POINT('Origin',(0.00737913518409336,4.16063869814088,
-0.187670095542209));
#130699=CARTESIAN_POINT('',(0.33152453429074,4.04280736269456,7.36530090741226));
#130700=CARTESIAN_POINT('Origin',(-9.78492460668168E-14,4.13463032200089,
-6.80011602582908E-13));
#130701=CARTESIAN_POINT('',(1.02275296005204,4.13354310061224,7.42993784484346));
#130702=CARTESIAN_POINT('Origin',(-0.0218540842582848,4.16070810453062,
-0.190828900716857));
#130703=CARTESIAN_POINT('Origin',(-0.00775259710145776,4.01786466043825,
-0.19197520892641));
#130704=CARTESIAN_POINT('Origin',(6.06492530893024E-14,4.13463032200089,
6.67868538251071E-14));
#130705=CARTESIAN_POINT('',(-0.0325097326105853,4.04280735814475,7.49992961001098));
#130706=CARTESIAN_POINT('Origin',(0.00483994282610858,4.01785698933134,
-0.192919282839389));
#130707=CARTESIAN_POINT('',(-0.59837544577304,4.13354310060964,7.47609168112341));
#130708=CARTESIAN_POINT('Origin',(0.0196794318998593,4.16070814981991,-0.191065540488097));
#130709=CARTESIAN_POINT('Origin',(0.0336976693805624,4.01786467675851,-0.189153730885039));
#130710=CARTESIAN_POINT('Ctrl Pts',(-0.844055740452712,3.912491975,7.45287521505932));
#130711=CARTESIAN_POINT('Ctrl Pts',(-0.439816755395279,3.97753138,7.49865623502238));
#130712=CARTESIAN_POINT('Ctrl Pts',(-0.0329975629266134,4.042807359,7.50044600138323));
#130713=CARTESIAN_POINT('Ctrl Pts',(-0.0189989277660423,4.04505350331101,
7.5005075871854));
#130714=CARTESIAN_POINT('Ctrl Pts',(-0.00500029260547111,4.04729964762199,
7.50056917298754));
#130715=CARTESIAN_POINT('Ctrl Pts',(-0.57870088,3.912491975,7.226866907));
#130716=CARTESIAN_POINT('Ctrl Pts',(-0.186720435,3.97753138,7.258255257));
#130717=CARTESIAN_POINT('Ctrl Pts',(0.206355414,4.042807359,7.247062677));
#130718=CARTESIAN_POINT('Ctrl Pts',(0.219881141159508,4.04505350331101,
7.24667754068681));
#130719=CARTESIAN_POINT('Ctrl Pts',(0.233406868319017,4.04729964762199,
7.24629240437362));
#130720=CARTESIAN_POINT('',(0.0869228665809933,4.04280735744341,7.37349610888705));
#130721=CARTESIAN_POINT('Ctrl Pts',(-0.029933757,1.714555786,7.499940264));
#130722=CARTESIAN_POINT('Ctrl Pts',(0.376054321,1.779135389,7.501560644));
#130723=CARTESIAN_POINT('Ctrl Pts',(0.77984494,1.844275173,7.459345941));
#130724=CARTESIAN_POINT('Ctrl Pts',(0.208844493,1.714555786,7.246991374));
#130725=CARTESIAN_POINT('Ctrl Pts',(0.601139897,1.779135389,7.235686168));
#130726=CARTESIAN_POINT('Ctrl Pts',(0.989922564,1.844275173,7.182099506));
#130727=CARTESIAN_POINT('',(0.213507114722386,1.71532338722497,7.24685550662799));
#130728=CARTESIAN_POINT('Origin',(-0.032091044012674,1.87498565506657,-0.195217911735541));
#130729=CARTESIAN_POINT('Ctrl Pts',(0.213507105706348,1.71532338483848,
7.24685550518316));
#130730=CARTESIAN_POINT('Ctrl Pts',(0.214203604296676,1.72001058631643,
7.27547631941166));
#130731=CARTESIAN_POINT('Ctrl Pts',(0.21487319422308,1.72461579686785,7.30411137271521));
#130732=CARTESIAN_POINT('Ctrl Pts',(0.215517557274855,1.72914335948484,
7.33275913756504));
#130733=CARTESIAN_POINT('Ctrl Pts',(0.216132017743193,1.73346081412226,
7.36007746216163));
#130734=CARTESIAN_POINT('Ctrl Pts',(0.216723540251772,1.73770768900512,
7.38740755584595));
#130735=CARTESIAN_POINT('Ctrl Pts',(0.217293427047396,1.74188747690247,
7.41474825875923));
#130736=CARTESIAN_POINT('Ctrl Pts',(0.217863328787458,1.74606737440856,
7.44208967864198));
#130737=CARTESIAN_POINT('Ctrl Pts',(0.218401490924672,1.75017861767189,
7.46944231625121));
#130738=CARTESIAN_POINT('Ctrl Pts',(0.218950417172741,1.75423096090297,
7.49680336627066));
#130739=CARTESIAN_POINT('Ctrl Pts',(1.267168999,1.844275173,7.39217713));
#130740=CARTESIAN_POINT('Ctrl Pts',(1.561876092,1.796786772,7.34165836100001));
#130741=CARTESIAN_POINT('Ctrl Pts',(1.851626136,1.75,7.267838788));
#130742=CARTESIAN_POINT('Ctrl Pts',(1.961045444,1.73233175,7.23996204900001));
#130743=CARTESIAN_POINT('Ctrl Pts',(2.069575967,1.714550109,7.208804014));
#130744=CARTESIAN_POINT('Ctrl Pts',(0.989922564,1.844275173,7.182099506));
#130745=CARTESIAN_POINT('Ctrl Pts',(1.276254403,1.796786772,7.142633839));
#130746=CARTESIAN_POINT('Ctrl Pts',(1.558535692,1.75,7.080499029));
#130747=CARTESIAN_POINT('Ctrl Pts',(1.665134548,1.73233175,7.057034846));
#130748=CARTESIAN_POINT('Ctrl Pts',(1.770978732,1.714550109,7.030372275));
#130749=CARTESIAN_POINT('',(1.76637515398525,1.71532338698357,7.03153033320607));
#130750=CARTESIAN_POINT('Ctrl Pts',(1.76637514766015,1.71532338940836,7.03153033360228));
#130751=CARTESIAN_POINT('Ctrl Pts',(1.6972361653671,1.72693520766404,7.04889858427259));
#130752=CARTESIAN_POINT('Ctrl Pts',(1.62794074337612,1.73849644464516,7.06522182174804));
#130753=CARTESIAN_POINT('Ctrl Pts',(1.55853569172686,1.75000000004527,7.08049902906013));
#130754=CARTESIAN_POINT('Ctrl Pts',(1.41430587426279,1.7739054021007,7.11224641273725));
#130755=CARTESIAN_POINT('Ctrl Pts',(1.26860743160117,1.79806016316673,7.1396923432409));
#130756=CARTESIAN_POINT('Ctrl Pts',(1.12183172733537,1.82239950660864,7.16268061375448));
#130757=CARTESIAN_POINT('Ctrl Pts',(1.07795450523445,1.82967552537028,7.16955274191823));
#130758=CARTESIAN_POINT('Ctrl Pts',(1.03398117244366,1.83696801257088,7.17602682336411));
#130759=CARTESIAN_POINT('Ctrl Pts',(0.989922562874548,1.84427517378427,
7.18209950596451));
#130760=CARTESIAN_POINT('Ctrl Pts',(1.82542260143802,1.75423096139436,7.27446440098633));
#130761=CARTESIAN_POINT('Ctrl Pts',(1.81869255493087,1.74998153251652,7.24656718951041));
#130762=CARTESIAN_POINT('Ctrl Pts',(1.81197503635218,1.74566717065959,7.21867673251375));
#130763=CARTESIAN_POINT('Ctrl Pts',(1.80522601115323,1.74127713117588,7.19080589214249));
#130764=CARTESIAN_POINT('Ctrl Pts',(1.79879017446392,1.73709081147133,7.16422839809913));
#130765=CARTESIAN_POINT('Ctrl Pts',(1.79233543785889,1.73283723876425,7.13766596825941));
#130766=CARTESIAN_POINT('Ctrl Pts',(1.78586077386494,1.72851290760487,7.11112002136436));
#130767=CARTESIAN_POINT('Ctrl Pts',(1.77938592092048,1.72418845024827,7.08457329977732));
#130768=CARTESIAN_POINT('Ctrl Pts',(1.77289109239293,1.71979319993659,7.05804286345013));
#130769=CARTESIAN_POINT('Ctrl Pts',(1.76637514608156,1.71532338474562,7.03153033395513));
#130770=CARTESIAN_POINT('Ctrl Pts',(1.583031538,1.714555786,7.331030702));
#130771=CARTESIAN_POINT('Ctrl Pts',(1.979876174,1.779135389,7.245337762));
#130772=CARTESIAN_POINT('Ctrl Pts',(2.365151479,1.844275173,7.117306968));
#130773=CARTESIAN_POINT('Ctrl Pts',(1.761850751,1.714555786,7.03266535000001));
#130774=CARTESIAN_POINT('Ctrl Pts',(2.142544221,1.779135389,6.937292538));
#130775=CARTESIAN_POINT('Ctrl Pts',(2.510717817,1.844275173,6.801381922));
#130776=CARTESIAN_POINT('Origin',(-0.0733067813757693,1.87498561224495,
-0.18375499371407));
#130777=CARTESIAN_POINT('Ctrl Pts',(2.826642864,1.844275173,6.94694826000001));
#130778=CARTESIAN_POINT('Ctrl Pts',(3.103599827,1.796786772,6.834257277));
#130779=CARTESIAN_POINT('Ctrl Pts',(3.370706649,1.75,6.699875871));
#130780=CARTESIAN_POINT('Ctrl Pts',(3.47157512,1.73233175,6.649128957));
#130781=CARTESIAN_POINT('Ctrl Pts',(3.570870203,1.714550109,6.59536852600001));
#130782=CARTESIAN_POINT('Ctrl Pts',(2.510717817,1.844275173,6.801381922));
#130783=CARTESIAN_POINT('Ctrl Pts',(2.781871425,1.796786772,6.70128605900001));
#130784=CARTESIAN_POINT('Ctrl Pts',(3.044195986,1.75,6.579921793));
#130785=CARTESIAN_POINT('Ctrl Pts',(3.143258515,1.73233175,6.534090586));
#130786=CARTESIAN_POINT('Ctrl Pts',(3.240896457,1.714550109,6.485298001));
#130787=CARTESIAN_POINT('',(3.23664945585214,1.71532338697944,6.48741861781993));
#130788=CARTESIAN_POINT('Ctrl Pts',(3.23664944972825,1.71532338941592,6.48741861962143));
#130789=CARTESIAN_POINT('Ctrl Pts',(3.1728605588578,1.72693520766624,6.51924364726614));
#130790=CARTESIAN_POINT('Ctrl Pts',(3.10869423851655,1.73849644464483,6.55008172375029));
#130791=CARTESIAN_POINT('Ctrl Pts',(3.04419598629713,1.74999999994701,6.57992179286254));
#130792=CARTESIAN_POINT('Ctrl Pts',(2.91016337108299,1.77390532353909,6.64193188382054));
#130793=CARTESIAN_POINT('Ctrl Pts',(2.77377179436078,1.79806000486797,6.70005682492887));
#130794=CARTESIAN_POINT('Ctrl Pts',(2.63536988905111,1.82239926748975,6.75405993082061));
#130795=CARTESIAN_POINT('Ctrl Pts',(2.59399534719788,1.82967536558803,6.77020388317389));
#130796=CARTESIAN_POINT('Ctrl Pts',(2.55244136939087,1.83696793249714,6.78597974788644));
#130797=CARTESIAN_POINT('Ctrl Pts',(2.51071781603781,1.84427517371954,6.80138192202261));
#130798=CARTESIAN_POINT('Ctrl Pts',(3.34654004953954,1.75423096141095,6.71197956579558));
#130799=CARTESIAN_POINT('Ctrl Pts',(3.33397027170787,1.74998153247943,6.68618133683395));
#130800=CARTESIAN_POINT('Ctrl Pts',(3.32141418136706,1.7456671706433,6.66038701106129));
#130801=CARTESIAN_POINT('Ctrl Pts',(3.30883153794968,1.74127713116734,6.63461861631227));
#130802=CARTESIAN_POINT('Ctrl Pts',(3.29683279212067,1.73709081148045,6.61004600396372));
#130803=CARTESIAN_POINT('Ctrl Pts',(3.28481882657189,1.73283723878304,6.58549216656776));
#130804=CARTESIAN_POINT('Ctrl Pts',(3.27278894282203,1.72851290761768,6.56095871051622));
#130805=CARTESIAN_POINT('Ctrl Pts',(3.2607587080534,1.72418845027309,6.53642453860544));
#130806=CARTESIAN_POINT('Ctrl Pts',(3.24871246551558,1.7197931999573,6.51191056533552));
#130807=CARTESIAN_POINT('Ctrl Pts',(3.23664944844862,1.71532338476526,6.48741861973777));
#130808=CARTESIAN_POINT('Ctrl Pts',(3.121976037,1.714555786,6.81933029100001));
#130809=CARTESIAN_POINT('Ctrl Pts',(3.491121217,1.779135389,6.650330939));
#130810=CARTESIAN_POINT('Ctrl Pts',(3.839866164,1.844275173,6.442470632));
#130811=CARTESIAN_POINT('Ctrl Pts',(3.232474826,1.714555786,6.489499711));
#130812=CARTESIAN_POINT('Ctrl Pts',(3.583765559,1.779135389,6.314518819));
#130813=CARTESIAN_POINT('Ctrl Pts',(3.914114695,1.844275173,6.102639278));
#130814=CARTESIAN_POINT('Origin',(-0.111095048004704,1.87498564516303,-0.163700524380229));
#130815=CARTESIAN_POINT('Ctrl Pts',(4.25394605,1.844275173,6.176887809));
#130816=CARTESIAN_POINT('Ctrl Pts',(4.500202683,1.796786772,6.007293919));
#130817=CARTESIAN_POINT('Ctrl Pts',(4.732176666,1.75,5.818634204));
#130818=CARTESIAN_POINT('Ctrl Pts',(4.819777801,1.73233175,5.747389985));
#130819=CARTESIAN_POINT('Ctrl Pts',(4.905194518,1.714550109,5.673540935));
#130820=CARTESIAN_POINT('Ctrl Pts',(3.914114695,1.844275173,6.102639278));
#130821=CARTESIAN_POINT('Ctrl Pts',(4.157411231,1.796786772,5.94659359));
#130822=CARTESIAN_POINT('Ctrl Pts',(4.38751306,1.75,5.771674726));
#130823=CARTESIAN_POINT('Ctrl Pts',(4.474407207,1.73233175,5.705619513));
#130824=CARTESIAN_POINT('Ctrl Pts',(4.559273465,1.714550109,5.636978399));
#130825=CARTESIAN_POINT('',(4.5555816269561,1.7153233868784,5.63996241661938));
#130826=CARTESIAN_POINT('Ctrl Pts',(4.55558162624592,1.71532338859363,5.63996241529551));
#130827=CARTESIAN_POINT('Ctrl Pts',(4.50012551473204,1.7269352089599,5.68475612547429));
#130828=CARTESIAN_POINT('Ctrl Pts',(4.44408864066811,1.73849644619173,5.72866708822583));
#130829=CARTESIAN_POINT('Ctrl Pts',(4.38751306021334,1.7500000000932,5.77167472643996));
#130830=CARTESIAN_POINT('Ctrl Pts',(4.26994398658319,1.77390540532321,5.86104841372417));
#130831=CARTESIAN_POINT('Ctrl Pts',(4.14923589214618,1.79806016925447,5.94713486426133));
#130832=CARTESIAN_POINT('Ctrl Pts',(4.02567838072189,1.82239951533986,6.02962798030087));
#130833=CARTESIAN_POINT('Ctrl Pts',(3.98874204125291,1.82967553068769,6.0542885104683));
#130834=CARTESIAN_POINT('Ctrl Pts',(3.95155133907772,1.83696801443579,6.07862813922019));
#130835=CARTESIAN_POINT('Ctrl Pts',(3.91411469928401,1.84427517216382,6.10263927525232));
#130836=CARTESIAN_POINT('Ctrl Pts',(4.71117700477546,1.75423096141368,5.83565002581548));
#130837=CARTESIAN_POINT('Ctrl Pts',(4.69335524483893,1.74998153250359,5.81315707568662));
#130838=CARTESIAN_POINT('Ctrl Pts',(4.67554769134855,1.7456671706691,5.79066499517674));
#130839=CARTESIAN_POINT('Ctrl Pts',(4.65771977994613,1.74127713119138,5.76820394759273));
#130840=CARTESIAN_POINT('Ctrl Pts',(4.64071917279701,1.73709081150169,5.74678520495294));
#130841=CARTESIAN_POINT('Ctrl Pts',(4.62370773780115,1.73283723880173,5.7253880701201));
#130842=CARTESIAN_POINT('Ctrl Pts',(4.60668513821075,1.72851290765366,5.70401426208977));
#130843=CARTESIAN_POINT('Ctrl Pts',(4.58966204185025,1.72418845030874,5.68263983030815));
#130844=CARTESIAN_POINT('Ctrl Pts',(4.57262765414895,1.71979320001295,5.66128856615154));
#130845=CARTESIAN_POINT('Ctrl Pts',(4.55558161933687,1.71532338483719,5.63996242078891));
#130846=CARTESIAN_POINT('Ctrl Pts',(4.514940407,1.714555786,5.988765576));
#130847=CARTESIAN_POINT('Ctrl Pts',(4.83912531200001,1.779135389,5.744362032));
#130848=CARTESIAN_POINT('Ctrl Pts',(5.135032975,1.844275173,5.466391529));
#130849=CARTESIAN_POINT('Ctrl Pts',(4.55195197,1.714555786,5.64289227800001));
#130850=CARTESIAN_POINT('Ctrl Pts',(4.85741400200001,1.779135389,5.396485218));
#130851=CARTESIAN_POINT('Ctrl Pts',(5.134491921,1.844275173,5.118544003));
#130852=CARTESIAN_POINT('Origin',(-0.143688351757486,1.87498561536551,-0.135991010582247));
#130853=CARTESIAN_POINT('Ctrl Pts',(5.482339447,1.844275173,5.11800295));
#130854=CARTESIAN_POINT('Ctrl Pts',(5.686381063,1.796786772,4.899436174));
#130855=CARTESIAN_POINT('Ctrl Pts',(5.872375362,1.75,4.665319669));
#130856=CARTESIAN_POINT('Ctrl Pts',(5.94261303,1.73233175,4.57690944600001));
#130857=CARTESIAN_POINT('Ctrl Pts',(6.010157388,1.714550109,4.486424876));
#130858=CARTESIAN_POINT('Ctrl Pts',(5.134491921,1.844275173,5.118544003));
#130859=CARTESIAN_POINT('Ctrl Pts',(5.338555108,1.796786772,4.913845014));
#130860=CARTESIAN_POINT('Ctrl Pts',(5.5256749,1.75,4.693550565));
#130861=CARTESIAN_POINT('Ctrl Pts',(5.596337592,1.73233175,4.610360012));
#130862=CARTESIAN_POINT('Ctrl Pts',(5.664463913,1.714550109,4.525079953));
#130863=CARTESIAN_POINT('',(5.66149986270782,1.71532338696423,4.52878784223245));
#130864=CARTESIAN_POINT('Ctrl Pts',(5.66149985801441,1.71532338934311,4.52878784623302));
#130865=CARTESIAN_POINT('Ctrl Pts',(5.61696961119619,1.7269352076431,4.58445571965647));
#130866=CARTESIAN_POINT('Ctrl Pts',(5.57168240855937,1.738496444645,4.63938633858587));
#130867=CARTESIAN_POINT('Ctrl Pts',(5.52567490000935,1.74999999999766,4.69355056498899));
#130868=CARTESIAN_POINT('Ctrl Pts',(5.4300673898056,1.77390536467005,4.80610842695748));
#130869=CARTESIAN_POINT('Ctrl Pts',(5.33068759992327,1.79806008776014,4.91613071518046));
#130870=CARTESIAN_POINT('Ctrl Pts',(5.22775255965428,1.82239939272323,5.02325623196279));
#130871=CARTESIAN_POINT('Ctrl Pts',(5.19698088489966,1.82967544929367,5.05528061891337));
#130872=CARTESIAN_POINT('Ctrl Pts',(5.16589180616078,1.83696797448142,5.08704628471413));
#130873=CARTESIAN_POINT('Ctrl Pts',(5.13449191974758,1.84427517382627,5.11854400418614));
#130874=CARTESIAN_POINT('Ctrl Pts',(5.85552455969772,1.75423096143509,4.68645197657854));
#130875=CARTESIAN_POINT('Ctrl Pts',(5.83328414297991,1.74998153247748,4.66831605084902));
#130876=CARTESIAN_POINT('Ctrl Pts',(5.81105778769197,1.74566717063503,4.65017792033718));
#130877=CARTESIAN_POINT('Ctrl Pts',(5.78881822167231,1.74127713116126,4.63207447348658));
#130878=CARTESIAN_POINT('Ctrl Pts',(5.76761068276119,1.73709081147863,4.61481111712567));
#130879=CARTESIAN_POINT('Ctrl Pts',(5.74639721422484,1.73283723879033,4.59757119101665));
#130880=CARTESIAN_POINT('Ctrl Pts',(5.7251778567166,1.72851290765275,4.58035644644634));
#130881=CARTESIAN_POINT('Ctrl Pts',(5.7039578798872,1.7241884503026,4.56314119943596));
#130882=CARTESIAN_POINT('Ctrl Pts',(5.68273185608999,1.71979320000101,4.5459510057534));
#130883=CARTESIAN_POINT('Ctrl Pts',(5.66149985709962,1.71532338474366,4.52878784834283));
#130884=CARTESIAN_POINT('Ctrl Pts',(5.696791181,1.714555786,4.878172838));
#130885=CARTESIAN_POINT('Ctrl Pts',(5.96085728700001,1.779135389,4.569793141));
#130886=CARTESIAN_POINT('Ctrl Pts',(6.19009135100001,1.844275173,4.234710034));
#130887=CARTESIAN_POINT('Ctrl Pts',(5.6585849,1.714555786,4.532429474));
#130888=CARTESIAN_POINT('Ctrl Pts',(5.903935165,1.779135389,4.226117966));
#130889=CARTESIAN_POINT('Ctrl Pts',(6.114786011,1.844275173,3.895111301));
#130890=CARTESIAN_POINT('Origin',(-0.169562945721984,1.8749856686932,-0.101922792765602));
#130891=CARTESIAN_POINT('Ctrl Pts',(6.454384744,1.844275173,3.819805961));
#130892=CARTESIAN_POINT('Ctrl Pts',(6.606670585,1.796786772,3.562486238));
#130893=CARTESIAN_POINT('Ctrl Pts',(6.737988312,1.75,3.293859971));
#130894=CARTESIAN_POINT('Ctrl Pts',(6.787578278,1.73233175,3.192417707));
#130895=CARTESIAN_POINT('Ctrl Pts',(6.834091979,1.714550109,3.089528577));
#130896=CARTESIAN_POINT('Ctrl Pts',(6.114786011,1.844275173,3.895111301));
#130897=CARTESIAN_POINT('Ctrl Pts',(6.270074082,1.796786772,3.651330506));
#130898=CARTESIAN_POINT('Ctrl Pts',(6.405462322,1.75,3.395961195));
#130899=CARTESIAN_POINT('Ctrl Pts',(6.45658945000001,1.73233175,3.299525202));
#130900=CARTESIAN_POINT('Ctrl Pts',(6.504790324,1.714550109,3.201593798));
#130901=CARTESIAN_POINT('',(6.502692658161,1.715323386995,3.20585218134069));
#130902=CARTESIAN_POINT('Ctrl Pts',(6.5026926542726,1.71532338947817,3.20585218664574));
#130903=CARTESIAN_POINT('Ctrl Pts',(6.47117044720264,1.72693520768658,3.26979126275422));
#130904=CARTESIAN_POINT('Ctrl Pts',(6.43875049337347,1.73849644464479,3.33317304402333));
#130905=CARTESIAN_POINT('Ctrl Pts',(6.40546232232299,1.7499999999346,3.39596119507856));
#130906=CARTESIAN_POINT('Ctrl Pts',(6.33628667717964,1.77390536429521,3.52644030471717));
#130907=CARTESIAN_POINT('Ctrl Pts',(6.26288187152611,1.79806008728388,3.65525404916549));
#130908=CARTESIAN_POINT('Ctrl Pts',(6.1853822153065,1.82239939206309,3.78200302082832));
#130909=CARTESIAN_POINT('Ctrl Pts',(6.1622142610839,1.82967544884116,3.81989369694854));
#130910=CARTESIAN_POINT('Ctrl Pts',(6.13868070620393,1.8369679742302,3.85759993313946));
#130911=CARTESIAN_POINT('Ctrl Pts',(6.11478600965671,1.84427517376166,3.89511130190476));
#130912=CARTESIAN_POINT('Ctrl Pts',(6.72607429382354,1.7542309613994,3.31812064141593));
#130913=CARTESIAN_POINT('Ctrl Pts',(6.70045515785928,1.74998153248024,3.30518975552672));
#130914=CARTESIAN_POINT('Ctrl Pts',(6.67484928050486,1.74566717064617,3.29225369376661));
#130915=CARTESIAN_POINT('Ctrl Pts',(6.64923795717485,1.74127713116247,3.27935434482503));
#130916=CARTESIAN_POINT('Ctrl Pts',(6.62481512732558,1.73709081146471,3.26705359018196));
#130917=CARTESIAN_POINT('Ctrl Pts',(6.60039154325329,1.73283723875166,3.25477699277116));
#130918=CARTESIAN_POINT('Ctrl Pts',(6.57596762111564,1.7285129075842,3.24252625409133));
#130919=CARTESIAN_POINT('Ctrl Pts',(6.55154298624939,1.72418845022592,3.2302751579156));
#130920=CARTESIAN_POINT('Ctrl Pts',(6.52711783144759,1.71979319991006,3.21804982922536));
#130921=CARTESIAN_POINT('Ctrl Pts',(6.50269265332106,1.71532338480411,3.20585218759416));
#130922=CARTESIAN_POINT('Ctrl Pts',(6.61226633200001,1.714555786,3.53948216));
#130923=CARTESIAN_POINT('Ctrl Pts',(6.803866199,1.779135389,3.181545802));
#130924=CARTESIAN_POINT('Ctrl Pts',(6.955707935,1.844275173,2.805018204));
#130925=CARTESIAN_POINT('Ctrl Pts',(6.500628688,1.714555786,3.210035304));
#130926=CARTESIAN_POINT('Ctrl Pts',(6.674394881,1.779135389,2.858142135));
#130927=CARTESIAN_POINT('Ctrl Pts',(6.809159503,1.844275173,2.489547522));
#130928=CARTESIAN_POINT('Origin',(-0.187509082124542,1.87498563387379,-0.0630888866187446));
#130929=CARTESIAN_POINT('Ctrl Pts',(7.124630184,1.844275173,2.34299909));
#130930=CARTESIAN_POINT('Ctrl Pts',(7.218039533,1.796786772,2.058958406));
#130931=CARTESIAN_POINT('Ctrl Pts',(7.288540418,1.75,1.768383042));
#130932=CARTESIAN_POINT('Ctrl Pts',(7.31516391,1.73233175,1.658652065));
#130933=CARTESIAN_POINT('Ctrl Pts',(7.338472024,1.714550109,1.548169354));
#130934=CARTESIAN_POINT('Ctrl Pts',(6.809159503,1.844275173,2.489547522));
#130935=CARTESIAN_POINT('Ctrl Pts',(6.908411361,1.796786772,2.218083843));
#130936=CARTESIAN_POINT('Ctrl Pts',(6.985737446,1.75,1.939580454));
#130937=CARTESIAN_POINT('Ctrl Pts',(7.014938362,1.73233175,1.83440826));
#130938=CARTESIAN_POINT('Ctrl Pts',(7.040959969,1.714550109,1.728404675));
#130939=CARTESIAN_POINT('',(7.03982677265495,1.71532338719604,1.73301443461817));
#130940=CARTESIAN_POINT('Ctrl Pts',(7.03982676947817,1.7153233893999,1.73301444130634));
#130941=CARTESIAN_POINT('Ctrl Pts',(7.02278654487449,1.72693520766041,1.80223500036135));
#130942=CARTESIAN_POINT('Ctrl Pts',(7.00474976112088,1.73849644464533,1.87110428255116));
#130943=CARTESIAN_POINT('Ctrl Pts',(6.98573744584127,1.75000000009604,1.93958045457169));
#130944=CARTESIAN_POINT('Ctrl Pts',(6.9462281097166,1.77390544324813,2.08188022262457));
#130945=CARTESIAN_POINT('Ctrl Pts',(6.90223045660141,1.79806024608469,2.22346269816108));
#130946=CARTESIAN_POINT('Ctrl Pts',(6.85378979382319,1.82239963186884,2.3639089373963));
#130947=CARTESIAN_POINT('Ctrl Pts',(6.83930901925183,1.82967560908574,2.40589371244103));
#130948=CARTESIAN_POINT('Ctrl Pts',(6.82443155112805,1.83696805454724,2.44777695512015));
#130949=CARTESIAN_POINT('Ctrl Pts',(6.80915950245155,1.8442751738645,2.48954752360552));
#130950=CARTESIAN_POINT('Ctrl Pts',(7.28212026958201,1.75423096143692,1.7946376730125));
#130951=CARTESIAN_POINT('Ctrl Pts',(7.25432033648641,1.7499815324715,1.78751646127468));
#130952=CARTESIAN_POINT('Ctrl Pts',(7.22653223945985,1.74566717064373,1.78038734412662));
#130953=CARTESIAN_POINT('Ctrl Pts',(7.19874671596365,1.74127713116593,1.77329525216261));
#130954=CARTESIAN_POINT('Ctrl Pts',(7.17225057973697,1.73709081147826,1.76653226873937));
#130955=CARTESIAN_POINT('Ctrl Pts',(7.14575890002104,1.73283723877416,1.75979303987636));
#130956=CARTESIAN_POINT('Ctrl Pts',(7.11927244903046,1.72851290761131,1.75307913787034));
#130957=CARTESIAN_POINT('Ctrl Pts',(7.09278522507288,1.72418845024939,1.74636503992924));
#130958=CARTESIAN_POINT('Ctrl Pts',(7.06630303261031,1.71979319992597,1.73967621882733));
#130959=CARTESIAN_POINT('Ctrl Pts',(7.03982676944971,1.71532338471622,1.73301444351913));
#130960=CARTESIAN_POINT('Ctrl Pts',(7.218559257,1.714555786,2.03528923));
#130961=CARTESIAN_POINT('Ctrl Pts',(7.32873389,1.779135389,1.644532917));
#130962=CARTESIAN_POINT('Ctrl Pts',(7.396083347,1.844275173,1.24416684));
#130963=CARTESIAN_POINT('Ctrl Pts',(7.038710305,1.714555786,1.737543452));
#130964=CARTESIAN_POINT('Ctrl Pts',(7.13276731100001,1.779135389,1.356522755));
#130965=CARTESIAN_POINT('Ctrl Pts',(7.185144264,1.844275173,0.967575269));
#130966=CARTESIAN_POINT('Origin',(-0.196687366030756,1.87498564470105,-0.0213049812195722));
#130967=CARTESIAN_POINT('Ctrl Pts',(7.461735836,1.844275173,0.756636186000001));
#130968=CARTESIAN_POINT('Ctrl Pts',(7.491900975,1.796786772,0.459155966));
#130969=CARTESIAN_POINT('Ctrl Pts',(7.498288474,1.75,0.160218487));
#130970=CARTESIAN_POINT('Ctrl Pts',(7.500700607,1.73233175,0.047329695));
#130971=CARTESIAN_POINT('Ctrl Pts',(7.499713274,1.714550109,-0.065580547));
#130972=CARTESIAN_POINT('Ctrl Pts',(7.185144264,1.844275173,0.967575269));
#130973=CARTESIAN_POINT('Ctrl Pts',(7.223719002,1.796786772,0.681122044));
#130974=CARTESIAN_POINT('Ctrl Pts',(7.23936725,1.75,0.392507087));
#130975=CARTESIAN_POINT('Ctrl Pts',(7.245276552,1.73233175,0.283516426));
#130976=CARTESIAN_POINT('Ctrl Pts',(7.247902151,1.714550109,0.17439727));
#130977=CARTESIAN_POINT('',(7.2477864108896,1.71532338699242,0.179142860916561));
#130978=CARTESIAN_POINT('Ctrl Pts',(7.24778640962524,1.7153233894705,0.179142867162212));
#130979=CARTESIAN_POINT('Ctrl Pts',(7.24602494966089,1.72693520768405,0.250408232466979));
#130980=CARTESIAN_POINT('Ctrl Pts',(7.24321471541452,1.7384964446451,0.321544764467899));
#130981=CARTESIAN_POINT('Ctrl Pts',(7.23936725011237,1.75000000002696,0.392507087301587));
#130982=CARTESIAN_POINT('Ctrl Pts',(7.23137187607232,1.77390540851427,0.539973091694986));
#130983=CARTESIAN_POINT('Ctrl Pts',(7.21883893532828,1.7980601762294,0.687703429362648));
#130984=CARTESIAN_POINT('Ctrl Pts',(7.20172261620258,1.822399526404,0.835279211927122));
#130985=CARTESIAN_POINT('Ctrl Pts',(7.19660585891261,1.82967553864264,0.87939555818794));
#130986=CARTESIAN_POINT('Ctrl Pts',(7.19107985214801,1.83696801928899,0.923498023146735));
#130987=CARTESIAN_POINT('Ctrl Pts',(7.18514426436052,1.84427517391947,0.967575271034647));
#130988=CARTESIAN_POINT('Ctrl Pts',(7.4976623948633,1.75423096140896,0.187239441348413));
#130989=CARTESIAN_POINT('Ctrl Pts',(7.46898155867245,1.74998153245423,0.186260883320029));
#130990=CARTESIAN_POINT('Ctrl Pts',(7.4403105823626,1.7456671706257,0.185272060355469));
#130991=CARTESIAN_POINT('Ctrl Pts',(7.41165007873351,1.74127713114288,0.184318843757033));
#130992=CARTESIAN_POINT('Ctrl Pts',(7.38431956598644,1.7370908114746,0.183409861181869));
#130993=CARTESIAN_POINT('Ctrl Pts',(7.35699851208546,1.73283723878819,0.182523119811445));
#130994=CARTESIAN_POINT('Ctrl Pts',(7.32968800914164,1.72851290763471,0.181659989172753));
#130995=CARTESIAN_POINT('Ctrl Pts',(7.30237670927953,1.72418845029759,0.180796833347977));
#130996=CARTESIAN_POINT('Ctrl Pts',(7.27507575700033,1.71979319999011,0.179957281808602));
#130997=CARTESIAN_POINT('Ctrl Pts',(7.24778640920089,1.7153233848652,0.179142868459304));
#130998=CARTESIAN_POINT('Ctrl Pts',(7.487320375,1.714555786,0.435928437));
#130999=CARTESIAN_POINT('Ctrl Pts',(7.510918129,1.779135389,0.030623501));
#131000=CARTESIAN_POINT('Ctrl Pts',(7.490626122,1.844275173,-0.374860382));
#131001=CARTESIAN_POINT('Ctrl Pts',(7.24766965,1.714555786,0.183805999));
#131002=CARTESIAN_POINT('Ctrl Pts',(7.257619468,1.779135389,-0.208526122));
#131003=CARTESIAN_POINT('Ctrl Pts',(7.225159666,1.844275173,-0.599639729));
#131004=CARTESIAN_POINT('Origin',(-0.196669206806751,1.87498565714627,0.0214751056292038));
#131005=CARTESIAN_POINT('Ctrl Pts',(7.449939012,1.844275173,-0.865106183999999));
#131006=CARTESIAN_POINT('Ctrl Pts',(7.41544945400001,1.796786772,-1.162116095));
#131007=CARTESIAN_POINT('Ctrl Pts',(7.357424895,1.75,-1.455437707));
#131008=CARTESIAN_POINT('Ctrl Pts',(7.335512881,1.73233175,-1.566205758));
#131009=CARTESIAN_POINT('Ctrl Pts',(7.310276266,1.714550109,-1.676263974));
#131010=CARTESIAN_POINT('Ctrl Pts',(7.225159666,1.844275173,-0.599639729));
#131011=CARTESIAN_POINT('Ctrl Pts',(7.201253572,1.796786772,-0.887688265));
#131012=CARTESIAN_POINT('Ctrl Pts',(7.154492288,1.75,-1.172919475));
#131013=CARTESIAN_POINT('Ctrl Pts',(7.136833664,1.73233175,-1.28063232));
#131014=CARTESIAN_POINT('Ctrl Pts',(7.11594048400001,1.714550109,-1.387764758));
#131015=CARTESIAN_POINT('',(7.11684761175525,1.71532338698871,-1.38310523484352));
#131016=CARTESIAN_POINT('Ctrl Pts',(7.11684761179474,1.71532338938623,-1.38310522861952));
#131017=CARTESIAN_POINT('Ctrl Pts',(7.13044728108712,1.72693520765624,-1.31312734623891));
#131018=CARTESIAN_POINT('Ctrl Pts',(7.14299500024421,1.7384964446449,-1.24304982945737));
#131019=CARTESIAN_POINT('Ctrl Pts',(7.15449228822887,1.74999999996677,-1.17291947501433));
#131020=CARTESIAN_POINT('Ctrl Pts',(7.17838464095599,1.77390537580904,-1.02718257393111));
#131021=CARTESIAN_POINT('Ctrl Pts',(7.19790234835856,1.79806011041741,-0.880212078894142));
#131022=CARTESIAN_POINT('Ctrl Pts',(7.21291062193433,1.822399427013,-0.732407236428844));
#131023=CARTESIAN_POINT('Ctrl Pts',(7.21739722597261,1.82967547216072,-0.688222154131791));
#131024=CARTESIAN_POINT('Ctrl Pts',(7.22148116085493,1.83696798586838,-0.643962651336697));
#131025=CARTESIAN_POINT('Ctrl Pts',(7.22515966590222,1.84427517368027,-0.599639727699752));
#131026=CARTESIAN_POINT('Ctrl Pts',(7.36262215969342,1.75423096149365,-1.42891389841392));
#131027=CARTESIAN_POINT('Ctrl Pts',(7.33440150456365,1.74998153254278,-1.42370404627898));
#131028=CARTESIAN_POINT('Ctrl Pts',(7.30618827216476,1.74566717068936,-1.41850633850759));
#131029=CARTESIAN_POINT('Ctrl Pts',(7.27799292189134,1.74127713120157,-1.4132761082767));
#131030=CARTESIAN_POINT('Ctrl Pts',(7.25110597695037,1.73709081151225,-1.40828858689877));
#131031=CARTESIAN_POINT('Ctrl Pts',(7.22423305089781,1.73283723881738,-1.40328137776424));
#131032=CARTESIAN_POINT('Ctrl Pts',(7.1973755047234,1.72851290767054,-1.39825337815015));
#131033=CARTESIAN_POINT('Ctrl Pts',(7.17051717483185,1.72418845033747,-1.39322523181642));
#131034=CARTESIAN_POINT('Ctrl Pts',(7.14367402481404,1.7197932000495,-1.38817625758044));
#131035=CARTESIAN_POINT('Ctrl Pts',(7.11684761220601,1.71532338486886,-1.38310522694114));
#131036=CARTESIAN_POINT('Ctrl Pts',(7.405982713,1.714555786,-1.183815884));
#131037=CARTESIAN_POINT('Ctrl Pts',(7.34190018500001,1.779135389,-1.584717836));
#131038=CARTESIAN_POINT('Ctrl Pts',(7.234915544,1.844275173,-1.976359549));
#131039=CARTESIAN_POINT('Ctrl Pts',(7.11773601800001,1.714555786,-1.378526018));
#131040=CARTESIAN_POINT('Ctrl Pts',(7.043113406,1.779135389,-1.763824549));
#131041=CARTESIAN_POINT('Ctrl Pts',(6.92733463100001,1.844275173,-2.138816239));
#131042=CARTESIAN_POINT('Origin',(-0.187454516868641,1.87498563159744,0.0632510508886766));
#131043=CARTESIAN_POINT('Ctrl Pts',(7.089791321,1.844275173,-2.446397152));
#131044=CARTESIAN_POINT('Ctrl Pts',(6.992259758,1.796786772,-2.7290489));
#131045=CARTESIAN_POINT('Ctrl Pts',(6.872536305,1.75,-3.00303925));
#131046=CARTESIAN_POINT('Ctrl Pts',(6.827324725,1.73233175,-3.106507171));
#131047=CARTESIAN_POINT('Ctrl Pts',(6.779018865,1.714550109,-3.208567161));
#131048=CARTESIAN_POINT('Ctrl Pts',(6.927334631,1.844275173,-2.138816239));
#131049=CARTESIAN_POINT('Ctrl Pts',(6.842065528,1.796786772,-2.414991257));
#131050=CARTESIAN_POINT('Ctrl Pts',(6.735081219,1.75,-2.683501626));
#131051=CARTESIAN_POINT('Ctrl Pts',(6.69468036500001,1.73233175,-2.784900123));
#131052=CARTESIAN_POINT('Ctrl Pts',(6.651245349,1.714550109,-2.885036447));
#131053=CARTESIAN_POINT('',(6.65313292778536,1.71532338722933,-2.88068086811694));
#131054=CARTESIAN_POINT('Ctrl Pts',(6.65313292980567,1.71532338938004,-2.88068086059141));
#131055=CARTESIAN_POINT('Ctrl Pts',(6.68145782268044,1.7269352076563,-2.81526254923147));
#131056=CARTESIAN_POINT('Ctrl Pts',(6.70877677796881,1.73849644464498,-2.74952079466792));
#131057=CARTESIAN_POINT('Ctrl Pts',(6.73508121897836,1.74999999999054,-2.68350162605432));
#131058=CARTESIAN_POINT('Ctrl Pts',(6.78974406744588,1.77390535875619,-2.54630822084171));
#131059=CARTESIAN_POINT('Ctrl Pts',(6.84039974034393,1.79806007584213,-2.40696964593335));
#131060=CARTESIAN_POINT('Ctrl Pts',(6.88683077358647,1.82239937471913,-2.26584683728512));
#131061=CARTESIAN_POINT('Ctrl Pts',(6.90071100498353,1.82967543723296,-2.22365916445846));
#131062=CARTESIAN_POINT('Ctrl Pts',(6.91421397780518,1.83696796839194,-2.18131224827326));
#131063=CARTESIAN_POINT('Ctrl Pts',(6.92733463124804,1.84427517373051,-2.13881623783067));
#131064=CARTESIAN_POINT('Ctrl Pts',(6.88331389536588,1.75423096141576,-2.97825281206678));
#131065=CARTESIAN_POINT('Ctrl Pts',(6.85687298763967,1.74998153248078,-2.96709815684415));
#131066=CARTESIAN_POINT('Ctrl Pts',(6.83043671842837,1.74566717062983,-2.95595695765252));
#131067=CARTESIAN_POINT('Ctrl Pts',(6.80402490463477,1.74127713115002,-2.94478784049848));
#131068=CARTESIAN_POINT('Ctrl Pts',(6.77883873113512,1.73709081146473,-2.93413702625764));
#131069=CARTESIAN_POINT('Ctrl Pts',(6.75367048106214,1.73283723877631,-2.92346999819169));
#131070=CARTESIAN_POINT('Ctrl Pts',(6.72852172072704,1.72851290764213,-2.91278597190329));
#131071=CARTESIAN_POINT('Ctrl Pts',(6.70337222640133,1.72418845029822,-2.90210163379136));
#131072=CARTESIAN_POINT('Ctrl Pts',(6.67824203453034,1.71979320000627,-2.89140021791908));
#131073=CARTESIAN_POINT('Ctrl Pts',(6.65313293024291,1.71532338480356,-2.88068085923549));
#131074=CARTESIAN_POINT('Ctrl Pts',(6.978349531,1.714555786,-2.748206291));
#131075=CARTESIAN_POINT('Ctrl Pts',(6.829583148,1.779135389,-3.125959528));
#131076=CARTESIAN_POINT('Ctrl Pts',(6.640908357,1.844275173,-3.485446341));
#131077=CARTESIAN_POINT('Ctrl Pts',(6.65498496,1.714555786,-2.876399691));
#131078=CARTESIAN_POINT('Ctrl Pts',(6.499279189,1.779135389,-3.236648501));
#131079=CARTESIAN_POINT('Ctrl Pts',(6.30559512900001,1.844275173,-3.577984079));
#131080=CARTESIAN_POINT('Origin',(-0.169474786281197,1.87498566159976,0.102069443457045));
#131081=CARTESIAN_POINT('Ctrl Pts',(6.398132867,1.844275173,-3.913297307));
#131082=CARTESIAN_POINT('Ctrl Pts',(6.242119767,1.796786772,-4.168374412));
#131083=CARTESIAN_POINT('Ctrl Pts',(6.066295556,1.75,-4.410222016));
#131084=CARTESIAN_POINT('Ctrl Pts',(5.999898453,1.73233175,-4.501551761));
#131085=CARTESIAN_POINT('Ctrl Pts',(5.930782076,1.714550109,-4.590841313));
#131086=CARTESIAN_POINT('Ctrl Pts',(6.305595129,1.844275173,-3.577984079));
#131087=CARTESIAN_POINT('Ctrl Pts',(6.162950104,1.796786772,-3.829371942));
#131088=CARTESIAN_POINT('Ctrl Pts',(6.000745237,1.75,-4.068606224));
#131089=CARTESIAN_POINT('Ctrl Pts',(5.939491253,1.73233175,-4.158949091));
#131090=CARTESIAN_POINT('Ctrl Pts',(5.875545374,1.714550109,-4.247407039));
#131091=CARTESIAN_POINT('',(5.87832514394337,1.7153233870063,-4.24355906365207));
#131092=CARTESIAN_POINT('Ctrl Pts',(5.87832514675913,1.71532338943757,-4.24355905786656));
#131093=CARTESIAN_POINT('Ctrl Pts',(5.92005082188062,1.72693520767362,-4.18575920521102));
#131094=CARTESIAN_POINT('Ctrl Pts',(5.96086360898721,1.73849644464494,-4.12742722417017));
#131095=CARTESIAN_POINT('Ctrl Pts',(6.00074523693298,1.74999999998067,-4.06860622409885));
#131096=CARTESIAN_POINT('Ctrl Pts',(6.08362259649407,1.77390535047736,-3.94637126312403));
#131097=CARTESIAN_POINT('Ctrl Pts',(6.16304761652092,1.7980600591429,-3.82117986309644));
#131098=CARTESIAN_POINT('Ctrl Pts',(6.23873032669115,1.82239934946658,-3.6933377730755));
#131099=CARTESIAN_POINT('Ctrl Pts',(6.26135517561757,1.8296754203857,-3.65512022025984));
#131100=CARTESIAN_POINT('Ctrl Pts',(6.28364581790097,1.83696795998772,-3.61666604713042));
#131101=CARTESIAN_POINT('Ctrl Pts',(6.30559512927184,1.84427517379952,-3.57798407762311));
#131102=CARTESIAN_POINT('Ctrl Pts',(6.08214952361998,1.75423096141961,-4.38833193459233));
#131103=CARTESIAN_POINT('Ctrl Pts',(6.05872471075126,1.74998153245681,-4.37175405532098));
#131104=CARTESIAN_POINT('Ctrl Pts',(6.03530153526694,1.74566717060285,-4.35519031474403));
#131105=CARTESIAN_POINT('Ctrl Pts',(6.01190824498387,1.74127713111933,-4.33860456609043));
#131106=CARTESIAN_POINT('Ctrl Pts',(5.98960052047753,1.73709081144454,-4.32278847920317));
#131107=CARTESIAN_POINT('Ctrl Pts',(5.96731378585211,1.73283723876601,-4.30696041055451));
#131108=CARTESIAN_POINT('Ctrl Pts',(5.94504973934713,1.72851290762539,-4.29111993073684));
#131109=CARTESIAN_POINT('Ctrl Pts',(5.92278504321281,1.72418845030769,-4.27527898871925));
#131110=CARTESIAN_POINT('Ctrl Pts',(5.9005428693928,1.71979320002457,-4.25942551758569));
#131111=CARTESIAN_POINT('Ctrl Pts',(5.87832514674664,1.71532338488821,-4.24355905666755));
#131112=CARTESIAN_POINT('Ctrl Pts',(6.224416481,1.714555786,-4.184093626));
#131113=CARTESIAN_POINT('Ctrl Pts',(5.997922393,1.779135389,-4.521034827));
#131114=CARTESIAN_POINT('Ctrl Pts',(5.736379676,1.844275173,-4.831557535));
#131115=CARTESIAN_POINT('Ctrl Pts',(5.881054202,1.714555786,-4.239776111));
#131116=CARTESIAN_POINT('Ctrl Pts',(5.6515459,1.779135389,-4.558130366));
#131117=CARTESIAN_POINT('Ctrl Pts',(5.389013006,1.844275173,-4.84984936));
#131118=CARTESIAN_POINT('Origin',(-0.143570649467616,1.87498566364901,0.136115196854825));
#131119=CARTESIAN_POINT('Ctrl Pts',(5.407304832,1.844275173,-5.19721603));
#131120=CARTESIAN_POINT('Ctrl Pts',(5.200105193,1.796786772,-5.412791368));
#131121=CARTESIAN_POINT('Ctrl Pts',(4.976401568,1.75,-5.611187702));
#131122=CARTESIAN_POINT('Ctrl Pts',(4.891923597,1.73233175,-5.686108794));
#131123=CARTESIAN_POINT('Ctrl Pts',(4.805228509,1.714550109,-5.75845282800001));
#131124=CARTESIAN_POINT('Ctrl Pts',(5.389013006,1.844275173,-4.84984936));
#131125=CARTESIAN_POINT('Ctrl Pts',(5.195661984,1.796786772,-5.06469545100001));
#131126=CARTESIAN_POINT('Ctrl Pts',(4.985821077,1.75,-5.263467316));
#131127=CARTESIAN_POINT('Ctrl Pts',(4.906578131,1.73233175,-5.338530221));
#131128=CARTESIAN_POINT('Ctrl Pts',(4.825111428,1.714550109,-5.411173598));
#131129=CARTESIAN_POINT('',(4.82865340810967,1.71532338695943,-5.40801315424955));
#131130=CARTESIAN_POINT('Ctrl Pts',(4.82865341177974,1.71532338935395,-5.40801314937509));
#131131=CARTESIAN_POINT('Ctrl Pts',(4.88182882469613,1.72693520764639,-5.36053441211114));
#131132=CARTESIAN_POINT('Ctrl Pts',(4.93422708346645,1.73849644464463,-5.31233974310289));
#131133=CARTESIAN_POINT('Ctrl Pts',(4.98582107697322,1.74999999988717,-5.26346731649234));
#131134=CARTESIAN_POINT('Ctrl Pts',(5.09303762256744,1.77390532985231,-5.16190641121414));
#131135=CARTESIAN_POINT('Ctrl Pts',(5.19751809382533,1.79806001794096,-5.05671604018305));
#131136=CARTESIAN_POINT('Ctrl Pts',(5.29891357386326,1.8223992873886,-4.94813247038953));
#131137=CARTESIAN_POINT('Ctrl Pts',(5.32922519817982,1.82967537890037,-4.91567200594574));
#131138=CARTESIAN_POINT('Ctrl Pts',(5.35926129425477,1.83696793918965,-4.88290860695238));
#131139=CARTESIAN_POINT('Ctrl Pts',(5.38901300743212,1.84427517375631,-4.84984935964758));
#131140=CARTESIAN_POINT('Ctrl Pts',(4.99659059962593,1.75423096137881,-5.59321753312504));
#131141=CARTESIAN_POINT('Ctrl Pts',(4.9772771996466,1.74998153250547,-5.57199159351297));
#131142=CARTESIAN_POINT('Ctrl Pts',(4.95796235969366,1.7456671706527,-5.5507798136574));
#131143=CARTESIAN_POINT('Ctrl Pts',(4.93868143733802,1.74127713116747,-5.52955296470416));
#131144=CARTESIAN_POINT('Ctrl Pts',(4.92029524621638,1.73709081147187,-5.50931114771194));
#131145=CARTESIAN_POINT('Ctrl Pts',(4.90193212997671,1.73283723877001,-5.4890621412984));
#131146=CARTESIAN_POINT('Ctrl Pts',(4.88359383955079,1.72851290761803,-5.46880589124527));
#131147=CARTESIAN_POINT('Ctrl Pts',(4.86525501387076,1.72418845024839,-5.44854904995705));
#131148=CARTESIAN_POINT('Ctrl Pts',(4.84694087742774,1.71979319992644,-5.42828481420679));
#131149=CARTESIAN_POINT('Ctrl Pts',(4.82865341408233,1.7153233846591,-5.40801314835518));
#131150=CARTESIAN_POINT('Ctrl Pts',(5.179436634,1.714555786,-5.424337393));
#131151=CARTESIAN_POINT('Ctrl Pts',(4.885805454,1.779135389,-5.704711563));
#131152=CARTESIAN_POINT('Ctrl Pts',(4.563624257,1.844275173,-5.951750469));
#131153=CARTESIAN_POINT('Ctrl Pts',(4.832131886,1.714555786,-5.404905313));
#131154=CARTESIAN_POINT('Ctrl Pts',(4.539552606,1.779135389,-5.666479121));
#131155=CARTESIAN_POINT('Ctrl Pts',(4.220446625,1.844275173,-5.894941076));
#131156=CARTESIAN_POINT('Origin',(-0.110953220978337,1.87498565391221,0.163796221188096));
#131157=CARTESIAN_POINT('Ctrl Pts',(4.163637232,1.844275173,-6.238118707));
#131158=CARTESIAN_POINT('Ctrl Pts',(3.91493948,1.796786772,-6.404112217));
#131159=CARTESIAN_POINT('Ctrl Pts',(3.653816575,1.75,-6.549780488));
#131160=CARTESIAN_POINT('Ctrl Pts',(3.555207832,1.73233175,-6.60478969900001));
#131161=CARTESIAN_POINT('Ctrl Pts',(3.454987798,1.714550109,-6.656805489));
#131162=CARTESIAN_POINT('Ctrl Pts',(4.220446625,1.844275173,-5.894941076));
#131163=CARTESIAN_POINT('Ctrl Pts',(3.985430483,1.796786772,-6.06319943));
#131164=CARTESIAN_POINT('Ctrl Pts',(3.737765465,1.75,-6.212214527));
#131165=CARTESIAN_POINT('Ctrl Pts',(3.64423887,1.73233175,-6.268487612));
#131166=CARTESIAN_POINT('Ctrl Pts',(3.549060633,1.714550109,-6.321919694));
#131167=CARTESIAN_POINT('',(3.5531992049754,1.71532338719967,-6.31959456164931));
#131168=CARTESIAN_POINT('Ctrl Pts',(3.55319921057251,1.71532338934942,-6.31959455693109));
#131169=CARTESIAN_POINT('Ctrl Pts',(3.61533793732367,1.72693520764435,-6.28465698753141));
#131170=CARTESIAN_POINT('Ctrl Pts',(3.67687158329099,1.73849644464494,-6.24885315985814));
#131171=CARTESIAN_POINT('Ctrl Pts',(3.73776546488684,1.74999999997862,-6.21221452706809));
#131172=CARTESIAN_POINT('Ctrl Pts',(3.86430804125286,1.77390534937231,-6.13607638508135));
#131173=CARTESIAN_POINT('Ctrl Pts',(3.98895873611091,1.79806005694259,-6.05580545205442));
#131174=CARTESIAN_POINT('Ctrl Pts',(4.11132599884036,1.82239934618419,-5.97155746290186));
#131175=CARTESIAN_POINT('Ctrl Pts',(4.14790689513797,1.8296754181976,-5.94637207519497));
#131176=CARTESIAN_POINT('Ctrl Pts',(4.18428382795472,1.83696795890152,-5.9208316068493));
#131177=CARTESIAN_POINT('Ctrl Pts',(4.22044662639856,1.84427517382187,-5.894941074851));
#131178=CARTESIAN_POINT('Ctrl Pts',(3.67739665300579,1.75423096143411,-6.53657049633415));
#131179=CARTESIAN_POINT('Ctrl Pts',(3.66309773951689,1.74998153247552,-6.51168899697367));
#131180=CARTESIAN_POINT('Ctrl Pts',(3.64879437539372,1.74566717062461,-6.48682101708093));
#131181=CARTESIAN_POINT('Ctrl Pts',(3.63452737529584,1.74127713113628,-6.46194561166913));
#131182=CARTESIAN_POINT('Ctrl Pts',(3.62092243537416,1.7370908114417,-6.4382245495094));
#131183=CARTESIAN_POINT('Ctrl Pts',(3.60734157634775,1.73283723873845,-6.4145014264286));
#131184=CARTESIAN_POINT('Ctrl Pts',(3.59378651978766,1.72851290758898,-6.39077656588435));
#131185=CARTESIAN_POINT('Ctrl Pts',(3.58023106762785,1.72418845023538,-6.36705101293812));
#131186=CARTESIAN_POINT('Ctrl Pts',(3.56670131697463,1.71979319993311,-6.34332354586962));
#131187=CARTESIAN_POINT('Ctrl Pts',(3.5531992128619,1.71532338470336,-6.31959455638273));
#131188=CARTESIAN_POINT('Ctrl Pts',(3.892272087,1.714555786,-6.410945172));
#131189=CARTESIAN_POINT('Ctrl Pts',(3.545233681,1.779135389,-6.621642326));
#131190=CARTESIAN_POINT('Ctrl Pts',(3.177478839,1.844275173,-6.793646166));
#131191=CARTESIAN_POINT('Ctrl Pts',(3.557264453,1.714555786,-6.317307149));
#131192=CARTESIAN_POINT('Ctrl Pts',(3.215294878,1.779135389,-6.50986961));
#131193=CARTESIAN_POINT('Ctrl Pts',(2.85453685,1.844275173,-6.664391898));
#131194=CARTESIAN_POINT('Origin',(-0.0731479700179943,1.87498564855422,
0.183818649927637));
#131195=CARTESIAN_POINT('Ctrl Pts',(2.725282582,1.844275173,-6.987333887));
#131196=CARTESIAN_POINT('Ctrl Pts',(2.446715548,1.796786772,-7.095983895));
#131197=CARTESIAN_POINT('Ctrl Pts',(2.160383179,1.75,-7.182112817));
#131198=CARTESIAN_POINT('Ctrl Pts',(2.052254499,1.73233175,-7.21463797899999));
#131199=CARTESIAN_POINT('Ctrl Pts',(1.943195696,1.714550109,-7.243893324));
#131200=CARTESIAN_POINT('Ctrl Pts',(2.85453685,1.844275173,-6.664391898));
#131201=CARTESIAN_POINT('Ctrl Pts',(2.588844683,1.796786772,-6.778194942));
#131202=CARTESIAN_POINT('Ctrl Pts',(2.314936093,1.75,-6.870485491));
#131203=CARTESIAN_POINT('Ctrl Pts',(2.211499049,1.73233175,-6.905337489));
#131204=CARTESIAN_POINT('Ctrl Pts',(2.107059708,1.714550109,-6.937059852));
#131205=CARTESIAN_POINT('',(2.11160135746148,1.71532338716952,-6.93567875019962));
#131206=CARTESIAN_POINT('Ctrl Pts',(2.11160136389839,1.71532338936648,-6.93567874676857));
#131207=CARTESIAN_POINT('Ctrl Pts',(2.17979786577418,1.72693520764907,-6.91491598770769));
#131208=CARTESIAN_POINT('Ctrl Pts',(2.24758965350799,1.73849644464509,-6.893177148517));
#131209=CARTESIAN_POINT('Ctrl Pts',(2.31493609321961,1.75000000002331,-6.87048549099526));
#131210=CARTESIAN_POINT('Ctrl Pts',(2.45488789203671,1.7739053949493,-6.82333023983162));
#131211=CARTESIAN_POINT('Ctrl Pts',(2.59388046275683,1.79806014881565,-6.77173210473685));
#131212=CARTESIAN_POINT('Ctrl Pts',(2.73149792979389,1.82239948494412,-6.71575900811587));
#131213=CARTESIAN_POINT('Ctrl Pts',(2.77263743592456,1.82967551094163,-6.69902635345241));
#131214=CARTESIAN_POINT('Ctrl Pts',(2.81365408042104,1.83696800541057,-6.68190307860387));
#131215=CARTESIAN_POINT('Ctrl Pts',(2.8545368519287,1.84427517391657,-6.66439189675992));
#131216=CARTESIAN_POINT('Ctrl Pts',(2.18625172552816,1.75423096135723,-7.17428068773433));
#131217=CARTESIAN_POINT('Ctrl Pts',(2.17763589926552,1.74998153246511,-7.14690706044567));
#131218=CARTESIAN_POINT('Ctrl Pts',(2.16901282041771,1.74566717062331,-7.11954567964696));
#131219=CARTESIAN_POINT('Ctrl Pts',(2.16042685174637,1.74127713113718,-7.09218486411791));
#131220=CARTESIAN_POINT('Ctrl Pts',(2.15223931497369,1.73709081144488,-7.06609372730505));
#131221=CARTESIAN_POINT('Ctrl Pts',(2.14407573916766,1.732837238741,-7.04000575443481));
#131222=CARTESIAN_POINT('Ctrl Pts',(2.1359377360913,1.72851290757632,-7.01392163141829));
#131223=CARTESIAN_POINT('Ctrl Pts',(2.12779949554998,1.72418845022869,-6.98783674727334));
#131224=CARTESIAN_POINT('Ctrl Pts',(2.11968676711798,1.71979319991724,-6.96175551874662));
#131225=CARTESIAN_POINT('Ctrl Pts',(2.11160136600415,1.71532338469401,-6.93567874658361));
#131226=CARTESIAN_POINT('Ctrl Pts',(2.423109222,1.714555786,-7.097784281));
#131227=CARTESIAN_POINT('Ctrl Pts',(2.038890722,1.779135389,-7.228952453));
#131228=CARTESIAN_POINT('Ctrl Pts',(1.642758043,1.844275173,-7.317878519));
#131229=CARTESIAN_POINT('Ctrl Pts',(2.116063288,1.714555786,-6.934318724));
#131230=CARTESIAN_POINT('Ctrl Pts',(1.740693535,1.779135389,-7.048865831));
#131231=CARTESIAN_POINT('Ctrl Pts',(1.355152105,1.844275173,-7.122223162));
#131232=CARTESIAN_POINT('Origin',(-0.031922228289937,1.87498560777645,0.195245673609244));
#131233=CARTESIAN_POINT('Ctrl Pts',(1.159496749,1.844275173,-7.4098291));
#131234=CARTESIAN_POINT('Ctrl Pts',(0.864085917,1.796786772,-7.456055254));
#131235=CARTESIAN_POINT('Ctrl Pts',(0.565932667,1.75,-7.478617534));
#131236=CARTESIAN_POINT('Ctrl Pts',(0.453340027,1.73233175,-7.487137805));
#131237=CARTESIAN_POINT('Ctrl Pts',(0.340541924,1.714550109,-7.492264758));
#131238=CARTESIAN_POINT('Ctrl Pts',(1.355152105,1.844275173,-7.122223162));
#131239=CARTESIAN_POINT('Ctrl Pts',(1.071207382,1.796786772,-7.176249592));
#131240=CARTESIAN_POINT('Ctrl Pts',(0.783862884,1.75,-7.207500189));
#131241=CARTESIAN_POINT('Ctrl Pts',(0.67535199,1.73233175,-7.21930146));
#131242=CARTESIAN_POINT('Ctrl Pts',(0.566535013,1.714550109,-7.22783080000001));
#131243=CARTESIAN_POINT('',(0.571267377317762,1.71532338719877,-7.22745830883115));
#131244=CARTESIAN_POINT('Ctrl Pts',(0.571267384531206,1.71532338937434,
-7.22745830685143));
#131245=CARTESIAN_POINT('Ctrl Pts',(0.642332869732959,1.72693520765293,
-7.22184120144342));
#131246=CARTESIAN_POINT('Ctrl Pts',(0.713212931112191,1.73849644464485,
-7.21518383454917));
#131247=CARTESIAN_POINT('Ctrl Pts',(0.783862883888383,1.74999999995389,
-7.20750018916874));
#131248=CARTESIAN_POINT('Ctrl Pts',(0.930679421736194,1.77390535412743,
-7.19153292890536));
#131249=CARTESIAN_POINT('Ctrl Pts',(1.07751424809532,1.79806006666806,-7.17102046623649));
#131250=CARTESIAN_POINT('Ctrl Pts',(1.22394660966233,1.82239936091677,-7.14593973521569));
#131251=CARTESIAN_POINT('Ctrl Pts',(1.26772157230118,1.82967542807154,-7.13844202055999));
#131252=CARTESIAN_POINT('Ctrl Pts',(1.31146051721306,1.83696796389124,-7.13053640196224));
#131253=CARTESIAN_POINT('Ctrl Pts',(1.35515210699587,1.84427517390224,-7.12222316208742));
#131254=CARTESIAN_POINT('Ctrl Pts',(0.592880097673218,1.75423096140348,
-7.47652948817272));
#131255=CARTESIAN_POINT('Ctrl Pts',(0.590350225508527,1.74998153246448,
-7.44794369301217));
#131256=CARTESIAN_POINT('Ctrl Pts',(0.587810637439113,1.74566717063106,
-7.41936829903185));
#131257=CARTESIAN_POINT('Ctrl Pts',(0.585307170438711,1.74127713115372,
-7.3908014346883));
#131258=CARTESIAN_POINT('Ctrl Pts',(0.582919876829699,1.7370908114675,-7.36356021574434));
#131259=CARTESIAN_POINT('Ctrl Pts',(0.580555303863958,1.73283723876916,
-7.33632723766341));
#131260=CARTESIAN_POINT('Ctrl Pts',(0.578214878173422,1.72851290761529,
-7.30910351682742));
#131261=CARTESIAN_POINT('Ctrl Pts',(0.575874384186324,1.724188450272,-7.28187900156907));
#131262=CARTESIAN_POINT('Ctrl Pts',(0.573558020025772,1.71979319997028,
-7.25466354083005));
#131263=CARTESIAN_POINT('Ctrl Pts',(0.571267386158136,1.7153233847658,-7.22745830671902));
#131264=CARTESIAN_POINT('Ctrl Pts',(0.840644464,1.714555786,-7.452738885));
#131265=CARTESIAN_POINT('Ctrl Pts',(0.437211499,1.779135389,-7.49824479800001));
#131266=CARTESIAN_POINT('Ctrl Pts',(0.031223706,1.844275173,-7.499935005));
#131267=CARTESIAN_POINT('Ctrl Pts',(0.575917356,1.714555786,-7.22708926200001));
#131268=CARTESIAN_POINT('Ctrl Pts',(0.184699296,1.779135389,-7.258264921));
#131269=CARTESIAN_POINT('Ctrl Pts',(-0.207598047,1.844275173,-7.247027187));
#131270=CARTESIAN_POINT('Origin',(0.0107961689541792,1.8749856554977,0.19754299577718));
#131271=CARTESIAN_POINT('Ctrl Pts',(-0.460505865,1.844275173,-7.48584894));
#131272=CARTESIAN_POINT('Ctrl Pts',(-0.758947412,1.796786772,-7.467489755));
#131273=CARTESIAN_POINT('Ctrl Pts',(-1.054980228,1.75,-7.425430406));
#131274=CARTESIAN_POINT('Ctrl Pts',(-1.166772121,1.73233175,-7.409547389));
#131275=CARTESIAN_POINT('Ctrl Pts',(-1.27803521,1.714550109,-7.390306218));
#131276=CARTESIAN_POINT('Ctrl Pts',(-0.207598047,1.844275173,-7.247027187));
#131277=CARTESIAN_POINT('Ctrl Pts',(-0.496518385,1.796786772,-7.238750787));
#131278=CARTESIAN_POINT('Ctrl Pts',(-0.783862884,1.75,-7.207500189));
#131279=CARTESIAN_POINT('Ctrl Pts',(-0.892373777000001,1.73233175,-7.19569891800001));
#131280=CARTESIAN_POINT('Ctrl Pts',(-1.00048023,1.714550109,-7.18063641400001));
#131281=CARTESIAN_POINT('',(-0.995778431050306,1.7153233872116,-7.18128994946387));
#131282=CARTESIAN_POINT('Ctrl Pts',(-0.995778423627768,1.71532338936346,
-7.1812899489929));
#131283=CARTESIAN_POINT('Ctrl Pts',(-0.925166898717766,1.72693520764936,
-7.19108114745931));
#131284=CARTESIAN_POINT('Ctrl Pts',(-0.854512836891311,1.7384964446448,
-7.19981654411594));
#131285=CARTESIAN_POINT('Ctrl Pts',(-0.783862883933284,1.74999999993805,
-7.20750018951493));
#131286=CARTESIAN_POINT('Ctrl Pts',(-0.637046086122069,1.77390539626308,
-7.22346747988324));
#131287=CARTESIAN_POINT('Ctrl Pts',(-0.489234340772536,1.79806015189128,
-7.23499974628836));
#131288=CARTESIAN_POINT('Ctrl Pts',(-0.340833606960876,1.82239948974368,
-7.24198401373006));
#131289=CARTESIAN_POINT('Ctrl Pts',(-0.296470552966318,1.82967551413793,
-7.24407189716345));
#131290=CARTESIAN_POINT('Ctrl Pts',(-0.252054988031275,1.8369680069904,
-7.24575367526172));
#131291=CARTESIAN_POINT('Ctrl Pts',(-0.207598045031906,1.84427517385712,
-7.24702718695691));
#131292=CARTESIAN_POINT('Ctrl Pts',(-1.02821394492889,1.75423096140346,
-7.42918407887295));
#131293=CARTESIAN_POINT('Ctrl Pts',(-1.02453956940233,1.7499815325155,-7.40072275602745));
#131294=CARTESIAN_POINT('Ctrl Pts',(-1.0208769182417,1.7456671706696,-7.37226950252867));
#131295=CARTESIAN_POINT('Ctrl Pts',(-1.01718082414328,1.74127713118194,
-7.34383234421274));
#131296=CARTESIAN_POINT('Ctrl Pts',(-1.0136562473036,1.73709081149108,-7.31671481232162));
#131297=CARTESIAN_POINT('Ctrl Pts',(-1.01011125257461,1.73283723879007,
-7.28961021289635));
#131298=CARTESIAN_POINT('Ctrl Pts',(-1.00654466515591,1.72851290763796,
-7.26251984527877));
#131299=CARTESIAN_POINT('Ctrl Pts',(-1.00297797364889,1.72418845028333,
-7.23542868704812));
#131300=CARTESIAN_POINT('Ctrl Pts',(-0.999389662915626,1.71979319997506,
-7.20835155888954));
#131301=CARTESIAN_POINT('Ctrl Pts',(-0.995778421714262,1.71532338474605,
-7.18128994961304));
#131302=CARTESIAN_POINT('Ctrl Pts',(-0.781127895000001,1.714555786,-7.459211702));
#131303=CARTESIAN_POINT('Ctrl Pts',(-1.184911248,1.779135389,-7.41692755));
#131304=CARTESIAN_POINT('Ctrl Pts',(-1.581770616,1.844275173,-7.331302866));
#131305=CARTESIAN_POINT('Ctrl Pts',(-0.991157831999999,1.714555786,-7.181929139));
#131306=CARTESIAN_POINT('Ctrl Pts',(-1.379931276,1.779135389,-7.12827561));
#131307=CARTESIAN_POINT('Ctrl Pts',(-1.760641144,1.844275173,-7.032968275));
#131308=CARTESIAN_POINT('Origin',(0.0530096988521347,1.87498560675979,0.190603958778421));
#131309=CARTESIAN_POINT('Ctrl Pts',(-2.058975735,1.844275173,-7.211838803));
#131310=CARTESIAN_POINT('Ctrl Pts',(-2.346493203,1.796786772,-7.129752735));
#131311=CARTESIAN_POINT('Ctrl Pts',(-2.62656342,1.75,-7.025038406));
#131312=CARTESIAN_POINT('Ctrl Pts',(-2.732327301,1.73233175,-6.98549477199999));
#131313=CARTESIAN_POINT('Ctrl Pts',(-2.836852838,1.714550109,-6.94278517400001));
#131314=CARTESIAN_POINT('Ctrl Pts',(-1.760641144,1.844275173,-7.032968275));
#131315=CARTESIAN_POINT('Ctrl Pts',(-2.041027504,1.796786772,-6.96277604));
#131316=CARTESIAN_POINT('Ctrl Pts',(-2.314936093,1.75,-6.870485491));
#131317=CARTESIAN_POINT('Ctrl Pts',(-2.418373138,1.73233175,-6.835633493));
#131318=CARTESIAN_POINT('Ctrl Pts',(-2.520714129,1.714550109,-6.79768345));
#131319=CARTESIAN_POINT('',(-2.51626274462168,1.71532338697785,-6.79933245394681));
#131320=CARTESIAN_POINT('Ctrl Pts',(-2.51626273833866,1.71532338937276,
-6.79933245505572));
#131321=CARTESIAN_POINT('Ctrl Pts',(-2.44940689025209,1.72693520765307,
-6.82407413079242));
#131322=CARTESIAN_POINT('Ctrl Pts',(-2.38228253315872,1.7384964446447,-6.84779383348064));
#131323=CARTESIAN_POINT('Ctrl Pts',(-2.31493609343453,1.74999999990727,
-6.87048549103555));
#131324=CARTESIAN_POINT('Ctrl Pts',(-2.17498473716275,1.7739053193183,-6.91764059378519));
#131325=CARTESIAN_POINT('Ctrl Pts',(-2.03310830652878,1.79805999654194,
-6.96067827377804));
#131326=CARTESIAN_POINT('Ctrl Pts',(-1.88967898132039,1.82239925498918,
-6.9994009276728));
#131327=CARTESIAN_POINT('Ctrl Pts',(-1.84680148610072,1.82967535725213,
-7.01097687565173));
#131328=CARTESIAN_POINT('Ctrl Pts',(-1.80378540390959,1.83696792834415,
-7.0221674928574));
#131329=CARTESIAN_POINT('Ctrl Pts',(-1.7606411431672,1.8442751737596,-7.03296827530728));
#131330=CARTESIAN_POINT('Ctrl Pts',(-2.60122984628299,1.75423096144644,
-7.03445827945573));
#131331=CARTESIAN_POINT('Ctrl Pts',(-2.5915230321622,1.74998153250533,-7.00745224865434));
#131332=CARTESIAN_POINT('Ctrl Pts',(-2.58182940328121,1.7456671706653,-6.98045157812462));
#131333=CARTESIAN_POINT('Ctrl Pts',(-2.57210657331054,1.74127713117846,
-6.95347381572797));
#131334=CARTESIAN_POINT('Ctrl Pts',(-2.56283493129394,1.73709081148723,
-6.92774795647658));
#131335=CARTESIAN_POINT('Ctrl Pts',(-2.55354612883298,1.73283723878164,
-6.90203911658116));
#131336=CARTESIAN_POINT('Ctrl Pts',(-2.54423929792918,1.72851290762179,
-6.87634881754053));
#131337=CARTESIAN_POINT('Ctrl Pts',(-2.53493219541867,1.72418845026245,
-6.85065776876484));
#131338=CARTESIAN_POINT('Ctrl Pts',(-2.52560699518005,1.71979319994618,
-6.82498506952868));
#131339=CARTESIAN_POINT('Ctrl Pts',(-2.51626273693115,1.71532338472195,
-6.79933245534817));
#131340=CARTESIAN_POINT('Ctrl Pts',(-2.366375582,1.714555786,-7.11690007));
#131341=CARTESIAN_POINT('Ctrl Pts',(-2.751628862,1.779135389,-6.988803013));
#131342=CARTESIAN_POINT('Ctrl Pts',(-3.120803103,1.844275173,-6.819867154));
#131343=CARTESIAN_POINT('Ctrl Pts',(-2.511887581,1.714555786,-6.800949991));
#131344=CARTESIAN_POINT('Ctrl Pts',(-2.880037795,1.779135389,-6.664976053));
#131345=CARTESIAN_POINT('Ctrl Pts',(-3.231358619,1.844275173,-6.49005558300001));
#131346=CARTESIAN_POINT('Origin',(0.0927445948128036,1.87498566366618,0.174752221623834));
#131347=CARTESIAN_POINT('Ctrl Pts',(-3.561170189,1.844275173,-6.600611099));
#131348=CARTESIAN_POINT('Ctrl Pts',(-3.82431958,1.796786772,-6.458636401));
#131349=CARTESIAN_POINT('Ctrl Pts',(-4.075331425,1.75,-6.296163417));
#131350=CARTESIAN_POINT('Ctrl Pts',(-4.170121894,1.73233175,-6.23480818400001));
#131351=CARTESIAN_POINT('Ctrl Pts',(-4.26302238,1.714550109,-6.170627212));
#131352=CARTESIAN_POINT('Ctrl Pts',(-3.231358619,1.844275173,-6.490055583));
#131353=CARTESIAN_POINT('Ctrl Pts',(-3.490100446,1.796786772,-6.361229625));
#131354=CARTESIAN_POINT('Ctrl Pts',(-3.737765465,1.75,-6.212214527));
#131355=CARTESIAN_POINT('Ctrl Pts',(-3.831292059,1.73233175,-6.155941442));
#131356=CARTESIAN_POINT('Ctrl Pts',(-3.923082237,1.714550109,-6.096878362));
#131357=CARTESIAN_POINT('',(-3.9190894118075,1.715323387189,-6.09944572887941));
#131358=CARTESIAN_POINT('Ctrl Pts',(-3.91908940514573,1.71532338929515,
-6.09944573161675));
#131359=CARTESIAN_POINT('Ctrl Pts',(-3.85911533782438,1.72693520762752,
-6.13798099222613));
#131360=CARTESIAN_POINT('Ctrl Pts',(-3.79865934604485,1.7384964446453,-6.17557589414559));
#131361=CARTESIAN_POINT('Ctrl Pts',(-3.73776546454411,1.75000000008612,
-6.2122145272743));
#131362=CARTESIAN_POINT('Ctrl Pts',(-3.6112224337199,1.77390543523616,-6.28835294289181));
#131363=CARTESIAN_POINT('Ctrl Pts',(-3.48191418812186,1.79806022994621,
-6.36088399665844));
#131364=CARTESIAN_POINT('Ctrl Pts',(-3.35016172797745,1.82239960750087,
-6.4295346952108));
#131365=CARTESIAN_POINT('Ctrl Pts',(-3.3107758002692,1.82967559281287,-6.45005705545622));
#131366=CARTESIAN_POINT('Ctrl Pts',(-3.27117169807065,1.83696804640807,
-6.47023289694387));
#131367=CARTESIAN_POINT('Ctrl Pts',(-3.23135861767661,1.8442751738904,-6.49005558383991));
#131368=CARTESIAN_POINT('Ctrl Pts',(-4.05261513068032,1.75423096141826,
-6.31080902862432));
#131369=CARTESIAN_POINT('Ctrl Pts',(-4.03732975837505,1.74998153251284,
-6.28652106195361));
#131370=CARTESIAN_POINT('Ctrl Pts',(-4.02205841514142,1.74566717066447,
-6.26223549580918));
#131371=CARTESIAN_POINT('Ctrl Pts',(-4.00676347813377,1.74127713117592,
-6.23797857957085));
#131372=CARTESIAN_POINT('Ctrl Pts',(-3.99217830271731,1.73709081148113,
-6.21484730559298));
#131373=CARTESIAN_POINT('Ctrl Pts',(-3.97758002674885,1.73283723877757,
-6.19173634204228));
#131374=CARTESIAN_POINT('Ctrl Pts',(-3.96296812961283,1.72851290762974,
-6.16864736146869));
#131375=CARTESIAN_POINT('Ctrl Pts',(-3.9483558060092,1.72418845027056,-6.14555770701255));
#131376=CARTESIAN_POINT('Ctrl Pts',(-3.93372975245047,1.71979319996508,
-6.12248986358579));
#131377=CARTESIAN_POINT('Ctrl Pts',(-3.91908940361339,1.71532338467323,
-6.09944573338996));
#131378=CARTESIAN_POINT('Ctrl Pts',(-3.840974177,1.714555786,-6.4418101));
#131379=CARTESIAN_POINT('Ctrl Pts',(-4.189683368,1.779135389,-6.233889815));
#131380=CARTESIAN_POINT('Ctrl Pts',(-4.513910305,1.844275173,-5.989542033));
#131381=CARTESIAN_POINT('Ctrl Pts',(-3.915164259,1.714555786,-6.101965981));
#131382=CARTESIAN_POINT('Ctrl Pts',(-4.245476948,1.779135389,-5.890029624));
#131383=CARTESIAN_POINT('Ctrl Pts',(-4.550981356,1.844275173,-5.643675106));
#131384=CARTESIAN_POINT('Origin',(0.128142651926348,1.87498565322314,0.150729012321198));
#131385=CARTESIAN_POINT('Ctrl Pts',(-4.896848283,1.844275173,-5.680746157));
#131386=CARTESIAN_POINT('Ctrl Pts',(-5.123325024,1.796786772,-5.485521408));
#131387=CARTESIAN_POINT('Ctrl Pts',(-5.333541463,1.75,-5.272886825));
#131388=CARTESIAN_POINT('Ctrl Pts',(-5.41292622100001,1.73233175,-5.192588894));
#131389=CARTESIAN_POINT('Ctrl Pts',(-5.489857734,1.714550109,-5.109937579));
#131390=CARTESIAN_POINT('Ctrl Pts',(-4.550981356,1.844275173,-5.643675106));
#131391=CARTESIAN_POINT('Ctrl Pts',(-4.77598017,1.796786772,-5.462239182));
#131392=CARTESIAN_POINT('Ctrl Pts',(-4.985821077,1.75,-5.263467316));
#131393=CARTESIAN_POINT('Ctrl Pts',(-5.065064022,1.73233175,-5.188404412));
#131394=CARTESIAN_POINT('Ctrl Pts',(-5.14201138,1.714550109,-5.110990019));
#131395=CARTESIAN_POINT('',(-5.13866381173065,1.71532338696204,-5.11435570193178));
#131396=CARTESIAN_POINT('Ctrl Pts',(-5.13866380664227,1.71532338939167,
-5.11435570540697));
#131397=CARTESIAN_POINT('Ctrl Pts',(-5.08837584222255,1.72693520765757,
-5.16488268446888));
#131398=CARTESIAN_POINT('Ctrl Pts',(-5.03741507052992,1.73849644464497,
-5.21459488956239));
#131399=CARTESIAN_POINT('Ctrl Pts',(-4.98582107705033,1.74999999998741,
-5.26346731617251));
#131400=CARTESIAN_POINT('Ctrl Pts',(-4.8786043022516,1.77390538127784,-5.36502844050722));
#131401=CARTESIAN_POINT('Ctrl Pts',(-4.76791149972737,1.79806012136271,
-5.46366099465171));
#131402=CARTESIAN_POINT('Ctrl Pts',(-4.65399747964481,1.82239944351147,
-5.55902936340484));
#131403=CARTESIAN_POINT('Ctrl Pts',(-4.61994382240916,1.82967548322283,
-5.58753895105952));
#131404=CARTESIAN_POINT('Ctrl Pts',(-4.58560259585709,1.83696799146888,
-5.61575701812922));
#131405=CARTESIAN_POINT('Ctrl Pts',(-4.55098135499805,1.84427517380053,
-5.64367510678222));
#131406=CARTESIAN_POINT('Ctrl Pts',(-5.31450463649893,1.75423096142994,
-5.29207336192635));
#131407=CARTESIAN_POINT('Ctrl Pts',(-5.29435543258047,1.74998153248503,
-5.27163913767342));
#131408=CARTESIAN_POINT('Ctrl Pts',(-5.27422044602439,1.74566717065283,
-5.25120424192191));
#131409=CARTESIAN_POINT('Ctrl Pts',(-5.25406857613305,1.74127713117215,
-5.23080239827337));
#131410=CARTESIAN_POINT('Ctrl Pts',(-5.23485185378547,1.73709081147825,
-5.21134730220106));
#131411=CARTESIAN_POINT('Ctrl Pts',(-5.21562670327365,1.73283723877023,
-5.19191485797558));
#131412=CARTESIAN_POINT('Ctrl Pts',(-5.19639297566802,1.72851290760489,
-5.17250681089194));
#131413=CARTESIAN_POINT('Ctrl Pts',(-5.17715868680678,1.72418845025209,
-5.15309819746591));
#131414=CARTESIAN_POINT('Ctrl Pts',(-5.15791567763788,1.71979319993897,
-5.13371383664131));
#131415=CARTESIAN_POINT('Ctrl Pts',(-5.13866380548064,1.71532338474424,
-5.11435570700624));
#131416=CARTESIAN_POINT('Ctrl Pts',(-5.135973089,1.714555786,-5.46550825));
#131417=CARTESIAN_POINT('Ctrl Pts',(-5.431832937,1.779135389,-5.187486857));
#131418=CARTESIAN_POINT('Ctrl Pts',(-5.695952078,1.844275173,-4.879152583));
#131419=CARTESIAN_POINT('Ctrl Pts',(-5.135372207,1.714555786,-5.117660823));
#131420=CARTESIAN_POINT('Ctrl Pts',(-5.412402317,1.779135389,-4.839671956));
#131421=CARTESIAN_POINT('Ctrl Pts',(-5.657805263,1.844275173,-4.533402653));
#131422=CARTESIAN_POINT('Origin',(0.15754918724798,1.87498566985664,0.119658311091085));
#131423=CARTESIAN_POINT('Ctrl Pts',(-6.003555193,1.844275173,-4.495255837));
#131424=CARTESIAN_POINT('Ctrl Pts',(-6.182769484,1.796786772,-4.25590953));
#131425=CARTESIAN_POINT('Ctrl Pts',(-6.342361029,1.75,-4.003055905));
#131426=CARTESIAN_POINT('Ctrl Pts',(-6.402628134,1.73233175,-3.907569919));
#131427=CARTESIAN_POINT('Ctrl Pts',(-6.45999344200001,1.714550109,-3.810312944));
#131428=CARTESIAN_POINT('Ctrl Pts',(-5.657805263,1.844275173,-4.533402653));
#131429=CARTESIAN_POINT('Ctrl Pts',(-5.838540369,1.796786772,-4.307840506));
#131430=CARTESIAN_POINT('Ctrl Pts',(-6.000745237,1.75,-4.068606224));
#131431=CARTESIAN_POINT('Ctrl Pts',(-6.06199922,1.73233175,-3.978263357));
#131432=CARTESIAN_POINT('Ctrl Pts',(-6.120505785,1.714550109,-3.886117463));
#131433=CARTESIAN_POINT('',(-6.11796000416365,1.71532338699328,-3.89012408614553));
#131434=CARTESIAN_POINT('Ctrl Pts',(-6.11795999984783,1.71532338947478,
-3.89012409082083));
#131435=CARTESIAN_POINT('Ctrl Pts',(-6.07970954685225,1.72693520768515,
-3.95028020283552));
#131436=CARTESIAN_POINT('Ctrl Pts',(-6.04062686434743,1.7384964446451,-4.00978522383035));
#131437=CARTESIAN_POINT('Ctrl Pts',(-6.00074523690707,1.75000000002681,
-4.06860622413707));
#131438=CARTESIAN_POINT('Ctrl Pts',(-5.91786775054758,1.77390538695136,
-4.19084137137646));
#131439=CARTESIAN_POINT('Ctrl Pts',(-5.83096594687763,1.79806013262182,
-4.31096365888321));
#131440=CARTESIAN_POINT('Ctrl Pts',(-5.74021653072587,1.82239946043817,
-4.42859054095511));
#131441=CARTESIAN_POINT('Ctrl Pts',(-5.71308776811837,1.82967549453686,
-4.46375409236191));
#131442=CARTESIAN_POINT('Ctrl Pts',(-5.68561549162366,1.83696799714455,
-4.49869475799346));
#131443=CARTESIAN_POINT('Ctrl Pts',(-5.65780526140172,1.84427517382125,
-4.53340265367153));
#131444=CARTESIAN_POINT('Ctrl Pts',(-6.32789381132842,1.754230961419,-4.02588622636397));
#131445=CARTESIAN_POINT('Ctrl Pts',(-6.3038229304785,1.74998153248991,-4.01026122619341));
#131446=CARTESIAN_POINT('Ctrl Pts',(-6.27976579010753,1.74566717064373,
-3.99463251394121));
#131447=CARTESIAN_POINT('Ctrl Pts',(-6.25569926639605,1.74127713116377,
-3.97903971038985));
#131448=CARTESIAN_POINT('Ctrl Pts',(-6.2327495497864,1.73709081147847,-3.96417049093199));
#131449=CARTESIAN_POINT('Ctrl Pts',(-6.20979647155677,1.73283723878647,
-3.94932520550051));
#131450=CARTESIAN_POINT('Ctrl Pts',(-6.18684026140042,1.72851290763057,
-3.93450559067464));
#131451=CARTESIAN_POINT('Ctrl Pts',(-6.16388338136915,1.7241884502883,-3.91968554340421));
#131452=CARTESIAN_POINT('Ctrl Pts',(-6.14092319847239,1.71979319997889,
-3.90489105636516));
#131453=CARTESIAN_POINT('Ctrl Pts',(-6.11795999885005,1.71532338484833,
-3.89012409187889));
#131454=CARTESIAN_POINT('Ctrl Pts',(-6.190819606,1.714555786,-4.233645309));
#131455=CARTESIAN_POINT('Ctrl Pts',(-6.419996035,1.779135389,-3.898522779));
#131456=CARTESIAN_POINT('Ctrl Pts',(-6.611657462,1.844275173,-3.540619381));
#131457=CARTESIAN_POINT('Ctrl Pts',(-6.115455858,1.714555786,-3.894059533));
#131458=CARTESIAN_POINT('Ctrl Pts',(-6.32624977,1.779135389,-3.563016607));
#131459=CARTESIAN_POINT('Ctrl Pts',(-6.500076484,1.844275173,-3.21115333));
#131460=CARTESIAN_POINT('Origin',(0.179588712885957,1.87498562990572,0.0829923124906845));
#131461=CARTESIAN_POINT('Ctrl Pts',(-6.829542535,1.844275173,-3.099572351));
#131462=CARTESIAN_POINT('Ctrl Pts',(-6.953114514,1.796786772,-2.827296052));
#131463=CARTESIAN_POINT('Ctrl Pts',(-7.054618843,1.75,-2.54604654));
#131464=CARTESIAN_POINT('Ctrl Pts',(-7.092950272,1.73233175,-2.439837317));
#131465=CARTESIAN_POINT('Ctrl Pts',(-7.128067036,1.714550109,-2.332522311));
#131466=CARTESIAN_POINT('Ctrl Pts',(-6.500076484,1.844275173,-3.21115333));
#131467=CARTESIAN_POINT('Ctrl Pts',(-6.62809690900001,1.796786772,-2.952011995));
#131468=CARTESIAN_POINT('Ctrl Pts',(-6.735081219,1.75,-2.683501626));
#131469=CARTESIAN_POINT('Ctrl Pts',(-6.775482072,1.73233175,-2.58210313));
#131470=CARTESIAN_POINT('Ctrl Pts',(-6.812812143,1.714550109,-2.479534373));
#131471=CARTESIAN_POINT('',(-6.81118718672704,1.71532338720686,-2.48399459038574));
#131472=CARTESIAN_POINT('Ctrl Pts',(-6.81118718300311,1.71532338937562,
-2.48399459670162));
#131473=CARTESIAN_POINT('Ctrl Pts',(-6.78676279055767,1.72693520765252,
-2.55096700918865));
#131474=CARTESIAN_POINT('Ctrl Pts',(-6.76138566003139,1.73849644464502,
-2.61748245733183));
#131475=CARTESIAN_POINT('Ctrl Pts',(-6.73508121901305,1.75000000000424,
-2.68350162607721));
#131476=CARTESIAN_POINT('Ctrl Pts',(-6.68041833199122,1.77390537542953,
-2.82069512751682));
#131477=CARTESIAN_POINT('Ctrl Pts',(-6.62137101549202,1.79806010944939,
-2.95669027739262));
#131478=CARTESIAN_POINT('Ctrl Pts',(-6.55802960725091,1.82239942545539,
-3.09107548762239));
#131479=CARTESIAN_POINT('Ctrl Pts',(-6.53909419508274,1.82967547114592,
-3.13124888154695));
#131480=CARTESIAN_POINT('Ctrl Pts',(-6.51977538511073,1.83696798539964,
-3.17127844552307));
#131481=CARTESIAN_POINT('Ctrl Pts',(-6.50007648272107,1.84427517376508,
-3.21115333112861));
#131482=CARTESIAN_POINT('Ctrl Pts',(-7.04539770492697,1.75423096145248,
-2.57145312545857));
#131483=CARTESIAN_POINT('Ctrl Pts',(-7.01853067466854,1.7499815325047,-2.56136795692046));
#131484=CARTESIAN_POINT('Ctrl Pts',(-6.99167626573207,1.74566717065564,
-2.55127620925494));
#131485=CARTESIAN_POINT('Ctrl Pts',(-6.96482041212451,1.7412771311639,-2.5412215479421));
#131486=CARTESIAN_POINT('Ctrl Pts',(-6.93921080451857,1.73709081147356,
-2.53163347323051));
#131487=CARTESIAN_POINT('Ctrl Pts',(-6.91360305898445,1.73283723877157,
-2.52206949564413));
#131488=CARTESIAN_POINT('Ctrl Pts',(-6.88799777319566,1.72851290761252,
-2.5125312617467));
#131489=CARTESIAN_POINT('Ctrl Pts',(-6.86239174019579,1.72418845026124,
-2.5029927495054));
#131490=CARTESIAN_POINT('Ctrl Pts',(-6.83678797627367,1.71979319995007,
-2.49347990990502));
#131491=CARTESIAN_POINT('Ctrl Pts',(-6.81118718266381,1.71532338473148,
-2.48399459871635));
#131492=CARTESIAN_POINT('Ctrl Pts',(-6.95619028,1.714555786,-2.803821818));
#131493=CARTESIAN_POINT('Ctrl Pts',(-7.107967253,1.779135389,-2.42726811));
#131494=CARTESIAN_POINT('Ctrl Pts',(-7.218209092,1.844275173,-2.036530753));
#131495=CARTESIAN_POINT('Ctrl Pts',(-6.809587591,1.714555786,-2.488376347));
#131496=CARTESIAN_POINT('Ctrl Pts',(-6.944288814,1.779135389,-2.119758561));
#131497=CARTESIAN_POINT('Ctrl Pts',(-7.038411352,1.844275173,-1.738754046));
#131498=CARTESIAN_POINT('Origin',(0.193230873444549,1.874985638441,0.0424457232433673));
#131499=CARTESIAN_POINT('Ctrl Pts',(-7.336188059,1.844275173,-1.558956307));
#131500=CARTESIAN_POINT('Ctrl Pts',(-7.39833963800001,1.796786772,-1.266481354));
#131501=CARTESIAN_POINT('Ctrl Pts',(-7.43701052,1.75,-0.969986869));
#131502=CARTESIAN_POINT('Ctrl Pts',(-7.451613939,1.73233175,-0.858020634));
#131503=CARTESIAN_POINT('Ctrl Pts',(-7.462840138,1.714550109,-0.745665527));
#131504=CARTESIAN_POINT('Ctrl Pts',(-7.038411352,1.844275173,-1.738754046));
#131505=CARTESIAN_POINT('Ctrl Pts',(-7.107731005,1.796786772,-1.458150685));
#131506=CARTESIAN_POINT('Ctrl Pts',(-7.154492288,1.75,-1.172919475));
#131507=CARTESIAN_POINT('Ctrl Pts',(-7.172150913,1.73233175,-1.06520663));
#131508=CARTESIAN_POINT('Ctrl Pts',(-7.186558977,1.714550109,-0.957011012));
#131509=CARTESIAN_POINT('',(-7.18593082598847,1.71532338697828,-0.961716270654875));
#131510=CARTESIAN_POINT('Ctrl Pts',(-7.18593082403205,1.71532338941653,
-0.961716276704436));
#131511=CARTESIAN_POINT('Ctrl Pts',(-7.1764745489304,1.72693520766661,-1.03237343373525));
#131512=CARTESIAN_POINT('Ctrl Pts',(-7.16598957642124,1.73849644464473,
-1.1027891205401));
#131513=CARTESIAN_POINT('Ctrl Pts',(-7.15449228845151,1.74999999991563,
-1.17291947499682));
#131514=CARTESIAN_POINT('Ctrl Pts',(-7.13059994450386,1.77390536878919,
-1.31865633427296));
#131515=CARTESIAN_POINT('Ctrl Pts',(-7.10216806696628,1.79806009648014,
-1.46416538209603));
#131516=CARTESIAN_POINT('Ctrl Pts',(-7.06919640414973,1.82239940603252,
-1.6090252331022));
#131517=CARTESIAN_POINT('Ctrl Pts',(-7.05933977535074,1.82967545822364,
-1.6523299880728));
#131518=CARTESIAN_POINT('Ctrl Pts',(-7.04907779246522,1.83696797900477,
-1.69557669487067));
#131519=CARTESIAN_POINT('Ctrl Pts',(-7.03841135156546,1.8442751739085,-1.7387540481104));
#131520=CARTESIAN_POINT('Ctrl Pts',(-7.43346663201529,1.75423096142758,
-0.996781734613964));
#131521=CARTESIAN_POINT('Ctrl Pts',(-7.40505972491879,1.7499815325007,-0.992707968931453));
#131522=CARTESIAN_POINT('Ctrl Pts',(-7.37666372970027,1.74566717065144,
-0.988625064820829));
#131523=CARTESIAN_POINT('Ctrl Pts',(-7.34827429605648,1.74127713115956,
-0.984578690565064));
#131524=CARTESIAN_POINT('Ctrl Pts',(-7.32120227423994,1.73709081147489,
-0.980720088329301));
#131525=CARTESIAN_POINT('Ctrl Pts',(-7.29413725113095,1.73283723877859,
-0.976884619551812));
#131526=CARTESIAN_POINT('Ctrl Pts',(-7.26708016439697,1.72851290762386,
-0.973073763836603));
#131527=CARTESIAN_POINT('Ctrl Pts',(-7.24002228807107,1.72418845027458,
-0.96926279691131));
#131528=CARTESIAN_POINT('Ctrl Pts',(-7.21297214663693,1.71979319996398,
-0.965476414649176));
#131529=CARTESIAN_POINT('Ctrl Pts',(-7.18593082378778,1.71532338478122,
-0.961716278323274));
#131530=CARTESIAN_POINT('Ctrl Pts',(-7.39629722700001,1.714555786,-1.242894736));
#131531=CARTESIAN_POINT('Ctrl Pts',(-7.463577823,1.779135389,-0.842517081));
#131532=CARTESIAN_POINT('Ctrl Pts',(-7.48724528700001,1.844275173,-0.437216209));
#131533=CARTESIAN_POINT('Ctrl Pts',(-7.185310576,1.714555786,-0.966339449));
#131534=CARTESIAN_POINT('Ctrl Pts',(-7.237620632,1.779135389,-0.57738296));
#131535=CARTESIAN_POINT('Ctrl Pts',(-7.24763792900001,1.844275173,-0.185052556));
#131536=CARTESIAN_POINT('Origin',(0.197838004389101,1.87498562398033,-8.55452297409201E-5));
#131537=CARTESIAN_POINT('Ctrl Pts',(-7.499801582,1.844275173,0.054554802));
#131538=CARTESIAN_POINT('Ctrl Pts',(-7.497626623,1.796786772,0.353552605));
#131539=CARTESIAN_POINT('Ctrl Pts',(-7.471655851,1.75,0.651428311));
#131540=CARTESIAN_POINT('Ctrl Pts',(-7.461848419,1.73233175,0.76391614));
#131541=CARTESIAN_POINT('Ctrl Pts',(-7.448659129,1.714550109,0.876057748));
#131542=CARTESIAN_POINT('Ctrl Pts',(-7.247637929,1.844275173,-0.185052556));
#131543=CARTESIAN_POINT('Ctrl Pts',(-7.255015499,1.796786772,0.103892131));
#131544=CARTESIAN_POINT('Ctrl Pts',(-7.23936725,1.75,0.392507087));
#131545=CARTESIAN_POINT('Ctrl Pts',(-7.233457948,1.73233175,0.501497748));
#131546=CARTESIAN_POINT('Ctrl Pts',(-7.2242703,1.714550109,0.610261121));
#131547=CARTESIAN_POINT('',(-7.22466832593348,1.71532338696753,0.605530834702192));
#131548=CARTESIAN_POINT('Ctrl Pts',(-7.22466832530966,1.71532338955417,
0.605530828374252));
#131549=CARTESIAN_POINT('Ctrl Pts',(-7.23062233283012,1.72693520771164,
0.534492776723643));
#131550=CARTESIAN_POINT('Ctrl Pts',(-7.23551978458698,1.73849644464494,
0.463469410197625));
#131551=CARTESIAN_POINT('Ctrl Pts',(-7.23936725010701,1.74999999995834,
0.392507087148465));
#131552=CARTESIAN_POINT('Ctrl Pts',(-7.24736260576629,1.77390535047713,
0.245041440907815));
#131553=CARTESIAN_POINT('Ctrl Pts',(-7.25087559512114,1.79806005925618,
0.0968224154203942));
#131554=CARTESIAN_POINT('Ctrl Pts',(-7.24981538563083,1.82239934968363,
-0.0517385105763896));
#131555=CARTESIAN_POINT('Ctrl Pts',(-7.24949844297524,1.82967542051086,
-0.0961498225221249));
#131556=CARTESIAN_POINT('Ctrl Pts',(-7.24877314242756,1.8369679600195,-0.140591582761845));
#131557=CARTESIAN_POINT('Ctrl Pts',(-7.24763792873457,1.8442751737337,-0.185052557496855));
#131558=CARTESIAN_POINT('Ctrl Pts',(-7.47395492118855,1.75423096142584,
0.624498063269636));
#131559=CARTESIAN_POINT('Ctrl Pts',(-7.44533641265144,1.74998153250237,
0.622369941210248));
#131560=CARTESIAN_POINT('Ctrl Pts',(-7.41672659636858,1.74566717064329,
0.620253089576169));
#131561=CARTESIAN_POINT('Ctrl Pts',(-7.38813104109155,1.7412771311558,0.618101972734666));
#131562=CARTESIAN_POINT('Ctrl Pts',(-7.3608624625947,1.73709081145649,0.616050678473018));
#131563=CARTESIAN_POINT('Ctrl Pts',(-7.33360569219016,1.73283723875479,
0.61397829614577));
#131564=CARTESIAN_POINT('Ctrl Pts',(-7.30636196376475,1.72851290761384,
0.611883582297337));
#131565=CARTESIAN_POINT('Ctrl Pts',(-7.27911744015338,1.72418845025495,
0.609788807308702));
#131566=CARTESIAN_POINT('Ctrl Pts',(-7.25188575564588,1.71979319995443,
0.607671685225234));
#131567=CARTESIAN_POINT('Ctrl Pts',(-7.22466832570712,1.71532338479073,
0.605530826510677));
#131568=CARTESIAN_POINT('Ctrl Pts',(-7.490561537,1.714555786,0.376148724));
#131569=CARTESIAN_POINT('Ctrl Pts',(-7.470199788,1.779135389,0.781629111));
#131570=CARTESIAN_POINT('Ctrl Pts',(-7.406186214,1.844275173,1.182542078));
#131571=CARTESIAN_POINT('Ctrl Pts',(-7.225056424,1.714555786,0.600882408));
#131572=CARTESIAN_POINT('Ctrl Pts',(-7.192529353,1.779135389,0.991990426));
#131573=CARTESIAN_POINT('Ctrl Pts',(-7.117973011,1.844275173,1.377301786));
#131574=CARTESIAN_POINT('Origin',(0.193194100687983,1.87498565212922,-0.0426128425397729));
#131575=CARTESIAN_POINT('Ctrl Pts',(-7.312732719,1.844275173,1.665514988));
#131576=CARTESIAN_POINT('Ctrl Pts',(-7.24633292000001,1.796786772,1.957054837));
#131577=CARTESIAN_POINT('Ctrl Pts',(-7.156934859,1.75,2.242383426));
#131578=CARTESIAN_POINT('Ctrl Pts',(-7.123175161,1.73233175,2.350133045));
#131579=CARTESIAN_POINT('Ctrl Pts',(-7.086187098,1.714550109,2.456817537));
#131580=CARTESIAN_POINT('Ctrl Pts',(-7.117973011,1.844275173,1.377301786));
#131581=CARTESIAN_POINT('Ctrl Pts',(-7.063063531,1.796786772,1.661077066));
#131582=CARTESIAN_POINT('Ctrl Pts',(-6.985737446,1.75,1.939580454));
#131583=CARTESIAN_POINT('Ctrl Pts',(-6.95653653,1.73233175,2.044752649));
#131584=CARTESIAN_POINT('Ctrl Pts',(-6.924182773,1.714550109,2.148998121));
#131585=CARTESIAN_POINT('',(-6.92558836542192,1.71532338722248,2.14446399150146));
#131586=CARTESIAN_POINT('Ctrl Pts',(-6.92558836637386,1.71532338940864,
2.14446398387456));
#131587=CARTESIAN_POINT('Ctrl Pts',(-6.94667425374691,1.72693520766414,
2.07636669827668));
#131588=CARTESIAN_POINT('Ctrl Pts',(-6.96672513021646,1.73849644464487,
2.00805662611619));
#131589=CARTESIAN_POINT('Ctrl Pts',(-6.98573744593035,1.74999999995786,
1.93958045425087));
#131590=CARTESIAN_POINT('Ctrl Pts',(-7.02524659969686,1.77390533277599,
1.79728134347411));
#131591=CARTESIAN_POINT('Ctrl Pts',(-7.06054014363285,1.7980600235061,1.65328289302275));
#131592=CARTESIAN_POINT('Ctrl Pts',(-7.09144091274129,1.8223992956843,1.50796743465552));
#131593=CARTESIAN_POINT('Ctrl Pts',(-7.10067852414962,1.82967538443001,
1.46452619436445));
#131594=CARTESIAN_POINT('Ctrl Pts',(-7.1095238684046,1.83696794194513,1.42096743216677));
#131595=CARTESIAN_POINT('Ctrl Pts',(-7.11797301163307,1.84427517374057,
1.37730178497811));
#131596=CARTESIAN_POINT('Ctrl Pts',(-7.16496938531472,1.75423096140909,
2.21657702477027));
#131597=CARTESIAN_POINT('Ctrl Pts',(-7.1374774448394,1.74998153246282,2.20834652356057));
#131598=CARTESIAN_POINT('Ctrl Pts',(-7.10999157065123,1.74566717061902,
2.20012889801882));
#131599=CARTESIAN_POINT('Ctrl Pts',(-7.08252699007765,1.74127713114131,
2.1918808740247));
#131600=CARTESIAN_POINT('Ctrl Pts',(-7.0563369033927,1.7370908114499,2.18401559959216));
#131601=CARTESIAN_POINT('Ctrl Pts',(-7.03016288205566,1.73283723875281,
2.17613226848579));
#131602=CARTESIAN_POINT('Ctrl Pts',(-7.00400639833485,1.72851290760386,
2.16822993156721));
#131603=CARTESIAN_POINT('Ctrl Pts',(-6.97784915130021,1.72418845025975,
2.16032736403801));
#131604=CARTESIAN_POINT('Ctrl Pts',(-6.95170924709586,1.71979319996095,
2.15240573186988));
#131605=CARTESIAN_POINT('Ctrl Pts',(-6.92558836665804,1.71532338478933,
2.14446398239877));
#131606=CARTESIAN_POINT('Ctrl Pts',(-7.234575514,1.714555786,1.977603887));
#131607=CARTESIAN_POINT('Ctrl Pts',(-7.127523515,1.779135389,2.369227193));
#131608=CARTESIAN_POINT('Ctrl Pts',(-6.978822105,1.844275173,2.747006012));
#131609=CARTESIAN_POINT('Ctrl Pts',(-6.926966664,1.714555786,2.140007671));
#131610=CARTESIAN_POINT('Ctrl Pts',(-6.811123395,1.779135389,2.514979442));
#131611=CARTESIAN_POINT('Ctrl Pts',(-6.655479587,1.844275173,2.875255027));
#131612=CARTESIAN_POINT('Origin',(0.179516811567976,1.87498563076573,-0.0831475948476074));
#131613=CARTESIAN_POINT('Ctrl Pts',(-6.783728602,1.844275173,3.198597545));
#131614=CARTESIAN_POINT('Ctrl Pts',(-6.656208743,1.796786772,3.46904736));
#131615=CARTESIAN_POINT('Ctrl Pts',(-6.507563547,1.75,3.728487185));
#131616=CARTESIAN_POINT('Ctrl Pts',(-6.451430149,1.73233175,3.82646034));
#131617=CARTESIAN_POINT('Ctrl Pts',(-6.392372834,1.714550109,3.922699268));
#131618=CARTESIAN_POINT('Ctrl Pts',(-6.655479587,1.844275173,2.875255027));
#131619=CARTESIAN_POINT('Ctrl Pts',(-6.540850562,1.796786772,3.140591884));
#131620=CARTESIAN_POINT('Ctrl Pts',(-6.405462322,1.75,3.395961195));
#131621=CARTESIAN_POINT('Ctrl Pts',(-6.354335194,1.73233175,3.492397189));
#131622=CARTESIAN_POINT('Ctrl Pts',(-6.300328155,1.714550109,3.587250358));
#131623=CARTESIAN_POINT('',(-6.30267559026525,1.71532338700246,3.58312439402828));
#131624=CARTESIAN_POINT('Ctrl Pts',(-6.30267559237097,1.71532338942935,
3.58312438803456));
#131625=CARTESIAN_POINT('Ctrl Pts',(-6.3379074070704,1.72693520767085,3.52115202098277));
#131626=CARTESIAN_POINT('Ctrl Pts',(-6.37217415129364,1.73849644464501,
3.45874934597489));
#131627=CARTESIAN_POINT('Ctrl Pts',(-6.40546232218141,1.75000000000019,
3.39596119494342));
#131628=CARTESIAN_POINT('Ctrl Pts',(-6.47463803525355,1.77390538761063,
3.26548195919798));
#131629=CARTESIAN_POINT('Ctrl Pts',(-6.54006198665916,1.7980601341064,3.13243687131316));
#131630=CARTESIAN_POINT('Ctrl Pts',(-6.60147896312938,1.82239946276566,
2.9971612401855));
#131631=CARTESIAN_POINT('Ctrl Pts',(-6.61983904091199,1.8296754960881,2.95672175175188));
#131632=CARTESIAN_POINT('Ctrl Pts',(-6.63784129172376,1.83696799791638,
2.91608316627399));
#131633=CARTESIAN_POINT('Ctrl Pts',(-6.65547958721565,1.84427517380786,
2.87525502605794));
#131634=CARTESIAN_POINT('Ctrl Pts',(-6.52095784396122,1.75423096140536,
3.70501130873352));
#131635=CARTESIAN_POINT('Ctrl Pts',(-6.4958779642362,1.7499815324682,3.69106327754831));
#131636=CARTESIAN_POINT('Ctrl Pts',(-6.47080124111415,1.74566717063294,
3.67712912506784));
#131637=CARTESIAN_POINT('Ctrl Pts',(-6.44575184852816,1.74127713116918,
3.66316986236279));
#131638=CARTESIAN_POINT('Ctrl Pts',(-6.4218648730107,1.73709081148772,3.64985837924667));
#131639=CARTESIAN_POINT('Ctrl Pts',(-6.39799746888694,1.73283723880349,
3.63653271520437));
#131640=CARTESIAN_POINT('Ctrl Pts',(-6.37415127804237,1.72851290766362,
3.62319225975418));
#131641=CARTESIAN_POINT('Ctrl Pts',(-6.35030439132123,1.72418845033167,
3.60985141500447));
#131642=CARTESIAN_POINT('Ctrl Pts',(-6.32647854029341,1.71979320004113,
3.59649567952216));
#131643=CARTESIAN_POINT('Ctrl Pts',(-6.30267559296041,1.7153233848871,3.58312438664675));
#131644=CARTESIAN_POINT('Ctrl Pts',(-6.640308781,1.714555786,3.48658849));
#131645=CARTESIAN_POINT('Ctrl Pts',(-6.451572163,1.779135389,3.846042846));
#131646=CARTESIAN_POINT('Ctrl Pts',(-6.225136031,1.844275173,4.183022998));
#131647=CARTESIAN_POINT('Ctrl Pts',(-6.304979642,1.714555786,3.579068554));
#131648=CARTESIAN_POINT('Ctrl Pts',(-6.111236877,1.779135389,3.920370815));
#131649=CARTESIAN_POINT('Ctrl Pts',(-5.881783334,1.844275173,4.238764539));
#131650=CARTESIAN_POINT('Origin',(0.157445675832952,1.87498564300627,-0.11979455520069));
#131651=CARTESIAN_POINT('Ctrl Pts',(-5.937524875,1.844275173,4.582117236));
#131652=CARTESIAN_POINT('Ctrl Pts',(-5.75484764300001,1.796786772,4.818831084));
#131653=CARTESIAN_POINT('Ctrl Pts',(-5.553905796,1.75,5.040251027));
#131654=CARTESIAN_POINT('Ctrl Pts',(-5.478023433,1.73233175,5.123866603));
#131655=CARTESIAN_POINT('Ctrl Pts',(-5.399658321,1.714550109,5.20515994100001));
#131656=CARTESIAN_POINT('Ctrl Pts',(-5.881783334,1.844275173,4.238764539));
#131657=CARTESIAN_POINT('Ctrl Pts',(-5.712794691,1.796786772,4.473256116));
#131658=CARTESIAN_POINT('Ctrl Pts',(-5.5256749,1.75,4.693550565));
#131659=CARTESIAN_POINT('Ctrl Pts',(-5.455012208,1.73233175,4.776741117));
#131660=CARTESIAN_POINT('Ctrl Pts',(-5.38187719599999,1.714550109,4.857766756));
#131661=CARTESIAN_POINT('',(-5.3850567085804,1.7153233869507,4.85424188252398));
#131662=CARTESIAN_POINT('Ctrl Pts',(-5.38505671164049,1.71532338934533,
4.85424187730532));
#131663=CARTESIAN_POINT('Ctrl Pts',(-5.43278705369071,1.72693520764284,
4.80129218921946));
#131664=CARTESIAN_POINT('Ctrl Pts',(-5.47966739144009,1.73849644464498,
4.74771479141373));
#131665=CARTESIAN_POINT('Ctrl Pts',(-5.52567489996523,1.74999999999131,
4.69355056504093));
#131666=CARTESIAN_POINT('Ctrl Pts',(-5.62128238601438,1.77390535875058,
4.58099273040823));
#131667=CARTESIAN_POINT('Ctrl Pts',(-5.713777415179,1.7980600758039,4.46512252189255));
#131668=CARTESIAN_POINT('Ctrl Pts',(-5.80283865954232,1.82239937461986,
4.34621254500967));
#131669=CARTESIAN_POINT('Ctrl Pts',(-5.82946289357073,1.82967543720348,
4.31066524185358));
#131670=CARTESIAN_POINT('Ctrl Pts',(-5.85578046393677,1.83696796843011,
4.27484657200368));
#131671=CARTESIAN_POINT('Ctrl Pts',(-5.88178333413084,1.84427517383409,
4.23876453736655));
#131672=CARTESIAN_POINT('Ctrl Pts',(-5.57203356106891,1.75423096144802,
5.02020338136438));
#131673=CARTESIAN_POINT('Ctrl Pts',(-5.55053844964282,1.74998153248361,
5.00119001457047));
#131674=CARTESIAN_POINT('Ctrl Pts',(-5.52904343725145,1.74566717064368,
4.98219088070449));
#131675=CARTESIAN_POINT('Ctrl Pts',(-5.50758051440559,1.74127713116268,
4.96317309889159));
#131676=CARTESIAN_POINT('Ctrl Pts',(-5.48711357848799,1.73709081146249,
4.94503783723804));
#131677=CARTESIAN_POINT('Ctrl Pts',(-5.46666880488506,1.73283723875101,
4.92689293344726));
#131678=CARTESIAN_POINT('Ctrl Pts',(-5.44624792837025,1.72851290759493,
4.90873814434882));
#131679=CARTESIAN_POINT('Ctrl Pts',(-5.4258264558248,1.72418845022322,4.89058282536075));
#131680=CARTESIAN_POINT('Ctrl Pts',(-5.40542872828474,1.71979319990471,
4.87241748589314));
#131681=CARTESIAN_POINT('Ctrl Pts',(-5.38505671417874,1.71532338465106,
4.85424187602781));
#131682=CARTESIAN_POINT('Ctrl Pts',(-5.735548589,1.714555786,4.83254409));
#131683=CARTESIAN_POINT('Ctrl Pts',(-5.473952467,1.779135389,5.143021809));
#131684=CARTESIAN_POINT('Ctrl Pts',(-5.180369514,1.844275173,5.423446478));
#131685=CARTESIAN_POINT('Ctrl Pts',(-5.388178779,1.714555786,4.85077617));
#131686=CARTESIAN_POINT('Ctrl Pts',(-5.125595715,1.779135389,5.142450006));
#131687=CARTESIAN_POINT('Ctrl Pts',(-4.833061429,1.844275173,5.404074132));
#131688=CARTESIAN_POINT('Origin',(0.128012269137338,1.87498564545476,-0.150839850589362));
#131689=CARTESIAN_POINT('Ctrl Pts',(-4.813689083,1.844275173,5.751382217));
#131690=CARTESIAN_POINT('Ctrl Pts',(-4.584396264,1.796786772,5.943291623));
#131691=CARTESIAN_POINT('Ctrl Pts',(-4.340553583,1.75,6.116338332));
#131692=CARTESIAN_POINT('Ctrl Pts',(-4.24847043,1.73233175,6.181686558));
#131693=CARTESIAN_POINT('Ctrl Pts',(-4.154461786,1.714550109,6.244233121));
#131694=CARTESIAN_POINT('Ctrl Pts',(-4.833061429,1.844275173,5.404074132));
#131695=CARTESIAN_POINT('Ctrl Pts',(-4.61761489,1.796786772,5.596755863));
#131696=CARTESIAN_POINT('Ctrl Pts',(-4.38751306,1.75,5.771674726));
#131697=CARTESIAN_POINT('Ctrl Pts',(-4.300618913,1.73233175,5.83772994));
#131698=CARTESIAN_POINT('Ctrl Pts',(-4.21177564,1.714550109,5.901139378));
#131699=CARTESIAN_POINT('',(-4.21563856057858,1.71532338724087,5.89838041754561));
#131700=CARTESIAN_POINT('Ctrl Pts',(-4.21563856641281,1.71532338948522,
5.89838041212843));
#131701=CARTESIAN_POINT('Ctrl Pts',(-4.27363561602965,1.72693520768896,
5.85692927020594));
#131702=CARTESIAN_POINT('Ctrl Pts',(-4.33093747372644,1.73849644464486,
5.81468236861823));
#131703=CARTESIAN_POINT('Ctrl Pts',(-4.38751305996885,1.7499999999554,5.77167472619238));
#131704=CARTESIAN_POINT('Ctrl Pts',(-4.50508187020585,1.77390535177738,
5.68230124087691));
#131705=CARTESIAN_POINT('Ctrl Pts',(-4.62032305475982,1.79806006190976,
5.58902373835267));
#131706=CARTESIAN_POINT('Ctrl Pts',(-4.73286419640703,1.82239935371937,
5.4920393752814));
#131707=CARTESIAN_POINT('Ctrl Pts',(-4.76650762263189,1.8296754232205,5.46304654460459));
#131708=CARTESIAN_POINT('Ctrl Pts',(-4.79990989018178,1.83696796139774,
5.43372276736845));
#131709=CARTESIAN_POINT('Ctrl Pts',(-4.83306143023905,1.8442751737759,5.40407413082299));
#131710=CARTESIAN_POINT('Ctrl Pts',(-4.36256718214353,1.75423096135179,
6.10065632342319));
#131711=CARTESIAN_POINT('Ctrl Pts',(-4.34566192601552,1.74998153244077,
6.07746666510283));
#131712=CARTESIAN_POINT('Ctrl Pts',(-4.32875370718173,1.74566717061137,
6.05429092807392));
#131713=CARTESIAN_POINT('Ctrl Pts',(-4.31188083645815,1.74127713113457,
6.03110387735127));
#131714=CARTESIAN_POINT('Ctrl Pts',(-4.29579095138311,1.73709081146119,
6.00899282183094));
#131715=CARTESIAN_POINT('Ctrl Pts',(-4.27972478328063,1.73283723877417,
5.98687711382543));
#131716=CARTESIAN_POINT('Ctrl Pts',(-4.26368407855432,1.72851290761985,
5.96475688867575));
#131717=CARTESIAN_POINT('Ctrl Pts',(-4.24764290579709,1.72418845029148,
5.94263601810869));
#131718=CARTESIAN_POINT('Ctrl Pts',(-4.23162707695028,1.71979319999226,
5.92051046568219));
#131719=CARTESIAN_POINT('Ctrl Pts',(-4.21563856675955,1.71532338489521,
5.89838041096121));
#131720=CARTESIAN_POINT('Ctrl Pts',(-4.56260052,1.714555786,5.9525353));
#131721=CARTESIAN_POINT('Ctrl Pts',(-4.240376838,1.779135389,6.199518789));
#131722=CARTESIAN_POINT('Ctrl Pts',(-3.893374677,1.844275173,6.410275628));
#131723=CARTESIAN_POINT('Ctrl Pts',(-4.219432665,1.714555786,5.895666882));
#131724=CARTESIAN_POINT('Ctrl Pts',(-3.900287394,1.779135389,6.124073949));
#131725=CARTESIAN_POINT('Ctrl Pts',(-3.558350943,1.844275173,6.316695225));
#131726=CARTESIAN_POINT('Origin',(0.0925933313251481,1.87498563513127,-0.174832223587613));
#131727=CARTESIAN_POINT('Ctrl Pts',(-3.46477054,1.844275173,6.651718958));
#131728=CARTESIAN_POINT('Ctrl Pts',(-3.19958361,1.796786772,6.78985045));
#131729=CARTESIAN_POINT('Ctrl Pts',(-2.924241908,1.75,6.906432456));
#131730=CARTESIAN_POINT('Ctrl Pts',(-2.820263672,1.73233175,6.95045772));
#131731=CARTESIAN_POINT('Ctrl Pts',(-2.715007236,1.714550109,6.991332899));
#131732=CARTESIAN_POINT('Ctrl Pts',(-3.558350943,1.844275173,6.316695225));
#131733=CARTESIAN_POINT('Ctrl Pts',(-3.306520548,1.796786772,6.45855752700001));
#131734=CARTESIAN_POINT('Ctrl Pts',(-3.044195986,1.75,6.579921793));
#131735=CARTESIAN_POINT('Ctrl Pts',(-2.945133458,1.73233175,6.62575299900001));
#131736=CARTESIAN_POINT('Ctrl Pts',(-2.844736136,1.714550109,6.668581282));
#131737=CARTESIAN_POINT('',(-2.84910183972128,1.7153233869967,6.66671723749229));
#131738=CARTESIAN_POINT('Ctrl Pts',(-2.849101845019,1.71532338948331,6.66671723400881));
#131739=CARTESIAN_POINT('Ctrl Pts',(-2.91465372686627,1.72693520768767,
6.63870284816572));
#131740=CARTESIAN_POINT('Ctrl Pts',(-2.97969773415148,1.73849644464538,
6.60976186158683));
#131741=CARTESIAN_POINT('Ctrl Pts',(-3.04419598661781,1.75000000011019,
6.57992179271417));
#131742=CARTESIAN_POINT('Ctrl Pts',(-3.17822933764657,1.77390545484905,
6.51791136105184));
#131743=CARTESIAN_POINT('Ctrl Pts',(-3.3108287147856,1.79806026946321,6.45158778029257));
#131744=CARTESIAN_POINT('Ctrl Pts',(-3.44158802289031,1.82239966718631,
6.38106353848644));
#131745=CARTESIAN_POINT('Ctrl Pts',(-3.48067692002918,1.82967563268207,
6.35998117828039));
#131746=CARTESIAN_POINT('Ctrl Pts',(-3.51960144497907,1.83696806636762,
6.3385237776968));
#131747=CARTESIAN_POINT('Ctrl Pts',(-3.5583509445948,1.84427517386462,6.31669522442253));
#131748=CARTESIAN_POINT('Ctrl Pts',(-2.94911201020307,1.75423096146604,
6.89584935662685));
#131749=CARTESIAN_POINT('Ctrl Pts',(-2.93758708077107,1.74998153251673,
6.86956772922766));
#131750=CARTESIAN_POINT('Ctrl Pts',(-2.92605626518683,1.7456671706699,6.8432990608362));
#131751=CARTESIAN_POINT('Ctrl Pts',(-2.91456240336107,1.74127713118637,
6.81702694207591));
#131752=CARTESIAN_POINT('Ctrl Pts',(-2.90360191419132,1.7370908114843,6.79197398098211));
#131753=CARTESIAN_POINT('Ctrl Pts',(-2.89266558762335,1.7328372387758,6.76692157463651));
#131754=CARTESIAN_POINT('Ctrl Pts',(-2.88175510013895,1.72851290761327,
6.74187023065704));
#131755=CARTESIAN_POINT('Ctrl Pts',(-2.87084429429732,1.72418845027103,
6.71681815570412));
#131756=CARTESIAN_POINT('Ctrl Pts',(-2.85995924627466,1.71979319997136,
6.69176695657303));
#131757=CARTESIAN_POINT('Ctrl Pts',(-2.8491018461973,1.7153233848865,6.6667172331805));
#131758=CARTESIAN_POINT('Ctrl Pts',(-3.176310322,1.714555786,6.794192575));
#131759=CARTESIAN_POINT('Ctrl Pts',(-2.808525901,1.779135389,6.96613316));
#131760=CARTESIAN_POINT('Ctrl Pts',(-2.424329967,1.844275173,7.097367414));
#131761=CARTESIAN_POINT('Ctrl Pts',(-2.853390569,1.714555786,6.664882764));
#131762=CARTESIAN_POINT('Ctrl Pts',(-2.492605969,1.779135389,6.819343002));
#131763=CARTESIAN_POINT('Ctrl Pts',(-2.117255923,1.844275173,6.933954669));
#131764=CARTESIAN_POINT('Origin',(0.0528448728486269,1.87498564167741,-0.190649775606609));
#131765=CARTESIAN_POINT('Ctrl Pts',(-1.953843178,1.844275173,7.241028714));
#131766=CARTESIAN_POINT('Ctrl Pts',(-1.665161983,1.796786772,7.318923417));
#131767=CARTESIAN_POINT('Ctrl Pts',(-1.371195932,1.75,7.373589473));
#131768=CARTESIAN_POINT('Ctrl Pts',(-1.260184519,1.73233175,7.39423320399999));
#131769=CARTESIAN_POINT('Ctrl Pts',(-1.148601964,1.714550109,7.411525722));
#131770=CARTESIAN_POINT('Ctrl Pts',(-2.117255923,1.844275173,6.933954669));
#131771=CARTESIAN_POINT('Ctrl Pts',(-1.84081698,1.796786772,7.018364219));
#131772=CARTESIAN_POINT('Ctrl Pts',(-1.558535692,1.75,7.080499029));
#131773=CARTESIAN_POINT('Ctrl Pts',(-1.451936835,1.73233175,7.103963212));
#131774=CARTESIAN_POINT('Ctrl Pts',(-1.344679932,1.714550109,7.124207737));
#131775=CARTESIAN_POINT('',(-1.34934428253352,1.71532338697916,7.12332576961706));
#131776=CARTESIAN_POINT('Ctrl Pts',(-1.34934428819312,1.715323389353,7.12332576731145));
#131777=CARTESIAN_POINT('Ctrl Pts',(-1.41938586838029,1.72693520764564,
7.11005805973543));
#131778=CARTESIAN_POINT('Ctrl Pts',(-1.48913063995742,1.73849644464481,
7.09577623625125));
#131779=CARTESIAN_POINT('Ctrl Pts',(-1.55853569163772,1.74999999993995,
7.08049902907975));
#131780=CARTESIAN_POINT('Ctrl Pts',(-1.70276500374618,1.77390531831854,
7.04875175653017));
#131781=CARTESIAN_POINT('Ctrl Pts',(-1.84652107666297,1.79805999435931,
7.01248396251438));
#131782=CARTESIAN_POINT('Ctrl Pts',(-1.98938313034179,1.82239925163071,
6.97171820711546));
#131783=CARTESIAN_POINT('Ctrl Pts',(-2.0320910514752,1.82967535506913,6.95953148137767));
#131784=CARTESIAN_POINT('Ctrl Pts',(-2.07471906307088,1.83696792734425,
6.94694313302838));
#131785=CARTESIAN_POINT('Ctrl Pts',(-2.11725592454464,1.8442751739537,6.93395466887861));
#131786=CARTESIAN_POINT('Ctrl Pts',(-1.39775963841141,1.75423096140856,
7.36860013775094));
#131787=CARTESIAN_POINT('Ctrl Pts',(-1.39215392831724,1.74998153249677,
7.34045544110522));
#131788=CARTESIAN_POINT('Ctrl Pts',(-1.38653968409113,1.74566717064396,
7.31232213507187));
#131789=CARTESIAN_POINT('Ctrl Pts',(-1.38096227129005,1.74127713116199,
7.28419340331715));
#131790=CARTESIAN_POINT('Ctrl Pts',(-1.3756436783369,1.7370908114676,7.25736998539424));
#131791=CARTESIAN_POINT('Ctrl Pts',(-1.37034856376125,1.73283723876874,
7.23055230350191));
#131792=CARTESIAN_POINT('Ctrl Pts',(-1.36507845578425,1.72851290762297,
7.2037412138722));
#131793=CARTESIAN_POINT('Ctrl Pts',(-1.35980819399523,1.72418845026839,
7.17692934174095));
#131794=CARTESIAN_POINT('Ctrl Pts',(-1.35456289953641,1.71979319996468,
7.15012386222506));
#131795=CARTESIAN_POINT('Ctrl Pts',(-1.34934429048395,1.71532338472446,
7.12332576748435));
#131796=CARTESIAN_POINT('Ctrl Pts',(-1.641499383,1.714555786,7.31816095600001));
#131797=CARTESIAN_POINT('Ctrl Pts',(-1.245351414,1.779135389,7.407018888));
#131798=CARTESIAN_POINT('Ctrl Pts',(-0.841926282,1.844275173,7.452594188));
#131799=CARTESIAN_POINT('Ctrl Pts',(-1.353927101,1.714555786,7.122456136));
#131800=CARTESIAN_POINT('Ctrl Pts',(-0.96837306,1.779135389,7.195747154));
#131801=CARTESIAN_POINT('Ctrl Pts',(-0.577160368,1.844275173,7.2269901));
#131802=CARTESIAN_POINT('Origin',(0.0106252857440335,1.87498562053249,-0.197552244875694));
#131803=CARTESIAN_POINT('Ctrl Pts',(-0.35155628,1.844275173,7.491756015));
#131804=CARTESIAN_POINT('Ctrl Pts',(-0.052879233,1.796786772,7.505771659));
#131805=CARTESIAN_POINT('Ctrl Pts',(0.245965642,1.75,7.495965642));
#131806=CARTESIAN_POINT('Ctrl Pts',(0.358819462,1.73233175,7.492262562));
#131807=CARTESIAN_POINT('Ctrl Pts',(0.471510658,1.714550109,7.485163839));
#131808=CARTESIAN_POINT('Ctrl Pts',(-0.577160368,1.844275173,7.2269901));
#131809=CARTESIAN_POINT('Ctrl Pts',(-0.289038857,1.796786772,7.25000000000001));
#131810=CARTESIAN_POINT('Ctrl Pts',(0.,1.75,7.25));
#131811=CARTESIAN_POINT('Ctrl Pts',(0.10915074,1.73233175,7.25));
#131812=CARTESIAN_POINT('Ctrl Pts',(0.218252011,1.714550109,7.246714156));
#131813=CARTESIAN_POINT('Ctrl Pts',(0.213507107014918,1.71532338944195,
7.2468555054415));
#131814=CARTESIAN_POINT('Ctrl Pts',(0.142250895423482,1.72693520767621,
7.24895485834218));
#131815=CARTESIAN_POINT('Ctrl Pts',(0.0710665482432402,1.73849644464489,
7.24999999999807));
#131816=CARTESIAN_POINT('Ctrl Pts',(1.97018677014537E-10,1.74999999996597,
7.2500000000132));
#131817=CARTESIAN_POINT('Ctrl Pts',(-0.147682176765806,1.77390534111371,
7.25000000004464));
#131818=CARTESIAN_POINT('Ctrl Pts',(-0.295873957336015,1.79806004030465,
7.2454834246082));
#131819=CARTESIAN_POINT('Ctrl Pts',(-0.444159548931349,1.82239932104086,
7.23638185097581));
#131820=CARTESIAN_POINT('Ctrl Pts',(-0.488488627306059,1.82967540141882,
7.23366099073213));
#131821=CARTESIAN_POINT('Ctrl Pts',(-0.532826001291235,1.83696795052539,
7.23053072198764));
#131822=CARTESIAN_POINT('Ctrl Pts',(-0.577160369311128,1.84427517387865,
7.22699009993985));
#131823=CARTESIAN_POINT('Ctrl Pts',(-1.356373314,4.042807359,7.121990693));
#131824=CARTESIAN_POINT('Ctrl Pts',(-0.967555641,4.108510123,7.196040483));
#131825=CARTESIAN_POINT('Ctrl Pts',(-0.572987507000001,4.173674111,7.22732214));
#131826=CARTESIAN_POINT('Ctrl Pts',(-1.160767276,4.042807359,7.409630175));
#131827=CARTESIAN_POINT('Ctrl Pts',(-0.756246224,4.108510123,7.473001057));
#131828=CARTESIAN_POINT('Ctrl Pts',(-0.347230585,4.173674111,7.49195775000001));
#131829=CARTESIAN_POINT('',(-0.57767741387148,4.17289950682494,7.2269487950413));
#131830=CARTESIAN_POINT('Ctrl Pts',(-0.577677421570388,4.17289950544926,
7.22694879416544));
#131831=CARTESIAN_POINT('Ctrl Pts',(-0.581165056550137,4.16602041298585,
7.26840987604015));
#131832=CARTESIAN_POINT('Ctrl Pts',(-0.584634097524575,4.15930620363512,
7.30992460671165));
#131833=CARTESIAN_POINT('Ctrl Pts',(-0.5915309518297,4.14619777610803,7.39295902153762));
#131834=CARTESIAN_POINT('Ctrl Pts',(-0.594962596891404,4.13979627490491,
7.43452487823737));
#131835=CARTESIAN_POINT('Ctrl Pts',(-0.598375443565973,4.13354310001741,
7.47609168121553));
#131836=CARTESIAN_POINT('Origin',(0.0411432879379811,4.01786903905992,-0.19371389706037));
#131837=CARTESIAN_POINT('Ctrl Pts',(-2.122257426,4.173681702,6.932425508));
#131838=CARTESIAN_POINT('Ctrl Pts',(-1.744480471,4.108088716,7.04807622));
#131839=CARTESIAN_POINT('Ctrl Pts',(-1.356373314,4.042807359,7.121990693));
#131840=CARTESIAN_POINT('Ctrl Pts',(-1.34295702550999,4.0405506793621,7.12454580664703));
#131841=CARTESIAN_POINT('Ctrl Pts',(-1.32954073702,4.03829399972412,7.1271009202939));
#131842=CARTESIAN_POINT('Ctrl Pts',(-2.43008400264692,4.173681702,7.09595388132405));
#131843=CARTESIAN_POINT('Ctrl Pts',(-2.04339570073195,4.108088716,7.22837935535182));
#131844=CARTESIAN_POINT('Ctrl Pts',(-1.64460712498496,4.042807359,7.31800089883344));
#131845=CARTESIAN_POINT('Ctrl Pts',(-1.63082159569944,4.0405506793621,7.32109898259864));
#131846=CARTESIAN_POINT('Ctrl Pts',(-1.61703606641398,4.03829399972412,
7.32419706636394));
#131847=CARTESIAN_POINT('',(-2.11775200231854,4.17289950637609,6.93380317648907));
#131848=CARTESIAN_POINT('Origin',(0.0562465567860779,4.16071258307181,-0.191024216299545));
#131849=CARTESIAN_POINT('Ctrl Pts',(-2.19152447788009,4.13354310002878,
7.1726717795594));
#131850=CARTESIAN_POINT('Ctrl Pts',(-2.17925578861821,4.13979627445688,
7.13281044940035));
#131851=CARTESIAN_POINT('Ctrl Pts',(-2.16696894385799,4.14619777521132,
7.09295408430292));
#131852=CARTESIAN_POINT('Ctrl Pts',(-2.14238339093939,4.15930620199799,
7.01334359200757));
#131853=CARTESIAN_POINT('Ctrl Pts',(-2.13007101043476,4.16602041351798,
6.97354518103625));
#131854=CARTESIAN_POINT('Ctrl Pts',(-2.11775200767413,4.17289950597958,
6.93380317476033));
#131855=CARTESIAN_POINT('Ctrl Pts',(-2.85697152392,4.042807359,6.66067269852999));
#131856=CARTESIAN_POINT('Ctrl Pts',(-2.49333902583,4.108510123,6.81664608632));
#131857=CARTESIAN_POINT('Ctrl Pts',(-2.11488790018,4.173674111,6.93210619159));
#131858=CARTESIAN_POINT('Ctrl Pts',(-2.855679535,4.042807359,6.66390234));
#131859=CARTESIAN_POINT('Ctrl Pts',(-2.491870718,4.108510123,6.81980519300001));
#131860=CARTESIAN_POINT('Ctrl Pts',(-2.113252,4.173674111,6.935175988));
#131861=CARTESIAN_POINT('Ctrl Pts',(-2.726480643,4.042807359,6.986866487));
#131862=CARTESIAN_POINT('Ctrl Pts',(-2.345039935,4.108510123,7.135715861));
#131863=CARTESIAN_POINT('Ctrl Pts',(-1.949661982,4.173674111,7.242155629));
#131864=CARTESIAN_POINT('Origin',(0.0818241170220929,4.01786906021735,-0.180340324830033));
#131865=CARTESIAN_POINT('Ctrl Pts',(-3.56290679,4.173681702,6.314126639));
#131866=CARTESIAN_POINT('Ctrl Pts',(-3.218823535,4.108088716,6.50828438));
#131867=CARTESIAN_POINT('Ctrl Pts',(-2.855679535,4.042807359,6.66390234));
#131868=CARTESIAN_POINT('Ctrl Pts',(-2.84312618582388,4.04055067936573,
6.66928182194095));
#131869=CARTESIAN_POINT('Ctrl Pts',(-2.83057283664774,4.03829399973139,
6.67466130388175));
#131870=CARTESIAN_POINT('Ctrl Pts',(-3.89869031899568,4.173681702,6.40765819510463));
#131871=CARTESIAN_POINT('Ctrl Pts',(-3.54951013729434,4.108088716,6.62011418952331));
#131872=CARTESIAN_POINT('Ctrl Pts',(-3.17931099982446,4.042807359,6.79336818647261));
#131873=CARTESIAN_POINT('Ctrl Pts',(-3.16651376501578,4.04055067936573,
6.79935732003907));
#131874=CARTESIAN_POINT('Ctrl Pts',(-3.15371653020715,4.03829399973139,
6.80534645360562));
#131875=CARTESIAN_POINT('',(-3.55880278961537,4.17289951177096,6.31644066991972));
#131876=CARTESIAN_POINT('Origin',(0.0959961150006616,4.16071256757818,-0.174466852259469));
#131877=CARTESIAN_POINT('Ctrl Pts',(-3.68220026361106,4.13354309997035,
6.53386571769809));
#131878=CARTESIAN_POINT('Ctrl Pts',(-3.6616494017322,4.13979627441468,6.4975737287741));
#131879=CARTESIAN_POINT('Ctrl Pts',(-3.64108187621462,4.14619777516013,
6.46129049185571));
#131880=CARTESIAN_POINT('Ctrl Pts',(-3.59995721709266,4.15930620195124,
6.38882641575838));
#131881=CARTESIAN_POINT('Ctrl Pts',(-3.57937721046934,4.16602041369041,
6.35260526619195));
#131882=CARTESIAN_POINT('Ctrl Pts',(-3.55880286240089,4.17289950613706,
6.31644062743981));
#131883=CARTESIAN_POINT('Ctrl Pts',(-4.22202485949,4.042807359,5.89078544632999));
#131884=CARTESIAN_POINT('Ctrl Pts',(-3.90042355506,4.108510123,6.1212825017));
#131885=CARTESIAN_POINT('Ctrl Pts',(-3.55564091525,4.173674111,6.31539901854001));
#131886=CARTESIAN_POINT('Ctrl Pts',(-4.221457354,4.042807359,5.89421732));
#131887=CARTESIAN_POINT('Ctrl Pts',(-3.89966869,4.108510123,6.124683393));
#131888=CARTESIAN_POINT('Ctrl Pts',(-3.554703177,4.173674111,6.318748715));
#131889=CARTESIAN_POINT('Ctrl Pts',(-4.164706805,4.042807359,6.237404687));
#131890=CARTESIAN_POINT('Ctrl Pts',(-3.824182184,4.108510123,6.464772523));
#131891=CARTESIAN_POINT('Ctrl Pts',(-3.460929352,4.173674111,6.653718361));
#131892=CARTESIAN_POINT('Origin',(0.118679043510761,4.0178690429932,-0.158534450043609));
#131893=CARTESIAN_POINT('Ctrl Pts',(-4.836958592,4.173681702,5.400586226));
#131894=CARTESIAN_POINT('Ctrl Pts',(-4.54265798800001,4.108088716,5.664172395));
#131895=CARTESIAN_POINT('Ctrl Pts',(-4.221457354,4.042807359,5.89421732));
#131896=CARTESIAN_POINT('Ctrl Pts',(-4.21035392510298,4.04055067943894,
5.90216963141373));
#131897=CARTESIAN_POINT('Ctrl Pts',(-4.19925049620598,4.03829399987781,
5.91012194282748));
#131898=CARTESIAN_POINT('Ctrl Pts',(-5.18499820863676,4.173681702,5.41974753300654));
#131899=CARTESIAN_POINT('Ctrl Pts',(-4.88965342356855,4.108088716,5.70229984158404));
#131900=CARTESIAN_POINT('Ctrl Pts',(-4.5653538246012,4.042807359,5.95108512861541));
#131901=CARTESIAN_POINT('Ctrl Pts',(-4.55414326908762,4.04055067943894,
5.95968526651294));
#131902=CARTESIAN_POINT('Ctrl Pts',(-4.54293271357389,4.03829399987781,
5.96828540441047));
#131903=CARTESIAN_POINT('',(-4.83344804812553,4.17289950636361,5.4037283423453));
#131904=CARTESIAN_POINT('Origin',(0.131257016296314,4.1607126306623,-0.149751590677861));
#131905=CARTESIAN_POINT('Ctrl Pts',(-5.00070045707408,4.13354310000987,
5.5895433562025));
#131906=CARTESIAN_POINT('Ctrl Pts',(-4.97282835816321,4.13979627444877,
5.55851768164219));
#131907=CARTESIAN_POINT('Ctrl Pts',(-4.94494186657699,4.14619777519739,
5.52750413664097));
#131908=CARTESIAN_POINT('Ctrl Pts',(-4.88920104484026,4.15930620198616,
5.46557481653246));
#131909=CARTESIAN_POINT('Ctrl Pts',(-4.86131571175525,4.16602041350881,
5.43462459145768));
#131910=CARTESIAN_POINT('Ctrl Pts',(-4.83344805214332,4.17289950595417,
5.40372833863019));
#131911=CARTESIAN_POINT('Ctrl Pts',(-5.38966100413,4.042807359,4.84545161372));
#131912=CARTESIAN_POINT('Ctrl Pts',(-5.12512861464,4.108510123,5.13969454897));
#131913=CARTESIAN_POINT('Ctrl Pts',(-4.83013611373001,4.173674111,5.40339080558));
#131914=CARTESIAN_POINT('Ctrl Pts',(-5.389844518,4.042807359,4.848925249));
#131915=CARTESIAN_POINT('Ctrl Pts',(-5.125122489,4.108510123,5.143178203));
#131916=CARTESIAN_POINT('Ctrl Pts',(-4.829940385,4.173674111,5.406863774));
#131917=CARTESIAN_POINT('Ctrl Pts',(-5.408195905,4.042807359,5.196288777));
#131918=CARTESIAN_POINT('Ctrl Pts',(-5.124509925,4.108510123,5.491543606));
#131919=CARTESIAN_POINT('Ctrl Pts',(-4.810367512,4.173674111,5.75416061600001));
#131920=CARTESIAN_POINT('Origin',(0.149984530496082,4.0178690506638,-0.129315426812652));
#131921=CARTESIAN_POINT('Ctrl Pts',(-5.88483958600001,4.173681702,4.234520403));
#131922=CARTESIAN_POINT('Ctrl Pts',(-5.654082801,4.108088716,4.555210005));
#131923=CARTESIAN_POINT('Ctrl Pts',(-5.389844518,4.042807359,4.848925249));
#131924=CARTESIAN_POINT('Ctrl Pts',(-5.3807101926145,4.04055067934832,4.85907854919147));
#131925=CARTESIAN_POINT('Ctrl Pts',(-5.37157586722897,4.03829399969656,
4.86923184938294));
#131926=CARTESIAN_POINT('Ctrl Pts',(-6.22886134497027,4.173681702,4.17841550046807));
#131927=CARTESIAN_POINT('Ctrl Pts',(-6.00116195121418,4.108088716,4.51785229157821));
#131928=CARTESIAN_POINT('Ctrl Pts',(-5.73792577853392,4.042807359,4.83053594383522));
#131929=CARTESIAN_POINT('Ctrl Pts',(-5.72882609461528,4.04055067934832,
4.84134495375618));
#131930=CARTESIAN_POINT('Ctrl Pts',(-5.71972641069679,4.03829399969656,
4.85215396367713));
#131931=CARTESIAN_POINT('',(-5.88208653312298,4.17289951178147,4.23834378550683));
#131932=CARTESIAN_POINT('Origin',(0.160380289703171,4.16071263034052,-0.118033961145265));
#131933=CARTESIAN_POINT('Ctrl Pts',(-6.08537345500513,4.13354310000783,
4.38386016046888));
#131934=CARTESIAN_POINT('Ctrl Pts',(-6.05148338734865,4.13979627444683,
4.359551526254));
#131935=CARTESIAN_POINT('Ctrl Pts',(-6.01758187087438,4.14619777522652,
4.33525783186004));
#131936=CARTESIAN_POINT('Ctrl Pts',(-5.94983126543378,4.15930620203592,
4.28675901346378));
#131937=CARTESIAN_POINT('Ctrl Pts',(-5.91594449174928,4.16602041372458,
4.26252690899275));
#131938=CARTESIAN_POINT('Ctrl Pts',(-5.88208658157426,4.17289950620119,
4.23834371608479));
#131939=CARTESIAN_POINT('Ctrl Pts',(-6.30528259168001,4.042807359,3.57354984844));
#131940=CARTESIAN_POINT('Ctrl Pts',(-6.11018835478,4.108510123,3.91778019304));
#131941=CARTESIAN_POINT('Ctrl Pts',(-5.87877951616001,4.173674111,4.23872604476));
#131942=CARTESIAN_POINT('Ctrl Pts',(-6.306208544,4.042807359,3.576902822));
#131943=CARTESIAN_POINT('Ctrl Pts',(-6.110931255,4.108510123,3.921183718));
#131944=CARTESIAN_POINT('Ctrl Pts',(-5.87933494900001,4.173674111,4.242159893));
#131945=CARTESIAN_POINT('Ctrl Pts',(-6.398803776,4.042807359,3.912200178));
#131946=CARTESIAN_POINT('Ctrl Pts',(-6.185221277,4.108510123,4.261536214));
#131947=CARTESIAN_POINT('Ctrl Pts',(-5.934878233,4.173674111,4.585544717));
#131948=CARTESIAN_POINT('Origin',(0.174276787464549,4.01786905587483,-0.094049750877061));
#131949=CARTESIAN_POINT('Ctrl Pts',(-6.657552022,4.173681702,2.870453113));
#131950=CARTESIAN_POINT('Ctrl Pts',(-6.501128988,4.108088716,3.233251058));
#131951=CARTESIAN_POINT('Ctrl Pts',(-6.306208544,4.042807359,3.576902822));
#131952=CARTESIAN_POINT('Ctrl Pts',(-6.29947043335256,4.04055067931237,
3.58878235378487));
#131953=CARTESIAN_POINT('Ctrl Pts',(-6.2927323227051,4.03829399962467,3.60066188556971));
#131954=CARTESIAN_POINT('Ctrl Pts',(-6.98146984730646,4.173681702,2.74170540229433));
#131955=CARTESIAN_POINT('Ctrl Pts',(-6.83206281608218,4.108088716,3.12215498942187));
#131956=CARTESIAN_POINT('Ctrl Pts',(-6.64219870107257,4.042807359,3.48411626705964));
#131957=CARTESIAN_POINT('Ctrl Pts',(-6.63563538021891,4.04055067931237,
3.4966287315747));
#131958=CARTESIAN_POINT('Ctrl Pts',(-6.62907205936524,4.03829399962466,
3.5091411960898));
#131959=CARTESIAN_POINT('',(-6.65568527962966,4.17289950637162,2.87477885958419));
#131960=CARTESIAN_POINT('Origin',(0.18200448439748,4.16071258288865,-0.0807973746653828));
#131961=CARTESIAN_POINT('Ctrl Pts',(-6.88550115417661,4.13354309998774,
2.97319253546826));
#131962=CARTESIAN_POINT('Ctrl Pts',(-6.84717777957122,4.13979627444384,
2.95673758635237));
#131963=CARTESIAN_POINT('Ctrl Pts',(-6.80884643569607,4.14619777519811,
2.94029968905659));
#131964=CARTESIAN_POINT('Ctrl Pts',(-6.73225398929105,4.15930620203543,
2.90749912360423));
#131965=CARTESIAN_POINT('Ctrl Pts',(-6.69395028459455,4.16602041351321,
2.89111820751232));
#131966=CARTESIAN_POINT('Ctrl Pts',(-6.65568528188716,4.17289950599813,
2.87477885414013));
#131967=CARTESIAN_POINT('Ctrl Pts',(-6.92607617273,4.042807359,2.13455286448));
#131968=CARTESIAN_POINT('Ctrl Pts',(-6.80954247911,4.108510123,2.51267478814));
#131969=CARTESIAN_POINT('Ctrl Pts',(-6.65253772200001,4.173674111,2.87586316486001));
#131970=CARTESIAN_POINT('Ctrl Pts',(-6.927701267,4.042807359,2.137628395));
#131971=CARTESIAN_POINT('Ctrl Pts',(-6.810999668,4.108510123,2.515839039));
#131972=CARTESIAN_POINT('Ctrl Pts',(-6.653818345,4.173674111,2.87909733));
#131973=CARTESIAN_POINT('Ctrl Pts',(-7.090210694,4.042807359,2.445181447));
#131974=CARTESIAN_POINT('Ctrl Pts',(-6.956718557,4.108510123,2.832264125));
#131975=CARTESIAN_POINT('Ctrl Pts',(-6.781880645,4.173674111,3.202513844));
#131976=CARTESIAN_POINT('Origin',(0.19042057799295,4.01786904786398,-0.0543866950544405));
#131977=CARTESIAN_POINT('Ctrl Pts',(-7.118964725,4.173681702,1.372166625));
#131978=CARTESIAN_POINT('Ctrl Pts',(-7.044189608,4.108088716,1.760108884));
#131979=CARTESIAN_POINT('Ctrl Pts',(-6.927701267,4.042807359,2.137628395));
#131980=CARTESIAN_POINT('Ctrl Pts',(-6.92367443794669,4.04055067938082,
2.15067868417093));
#131981=CARTESIAN_POINT('Ctrl Pts',(-6.91964760889334,4.03829399976158,
2.16372897334185));
#131982=CARTESIAN_POINT('Ctrl Pts',(-7.4076325789629,4.173681702,1.17679620739295));
#131983=CARTESIAN_POINT('Ctrl Pts',(-7.34350401581941,4.108088716,1.58046918964557));
#131984=CARTESIAN_POINT('Ctrl Pts',(-7.23588979397176,4.042807359,1.97478318634262));
#131985=CARTESIAN_POINT('Ctrl Pts',(-7.23216973004631,4.04055067938082,
1.98841403595727));
#131986=CARTESIAN_POINT('Ctrl Pts',(-7.22844966612089,4.03829399976157,
2.00204488557198));
#131987=CARTESIAN_POINT('',(-7.11807151787488,4.17289951178047,1.37679261006278));
#131988=CARTESIAN_POINT('Origin',(0.195118497292496,4.16071260882338,-0.0397828217243851));
#131989=CARTESIAN_POINT('Ctrl Pts',(-7.36367047159053,4.13354310001364,
1.42350173179299));
#131990=CARTESIAN_POINT('Ctrl Pts',(-7.3227057484912,4.13979627446707,1.41566988296896));
#131991=CARTESIAN_POINT('Ctrl Pts',(-7.28173690833156,4.14619777517845,
1.40785640051236));
#131992=CARTESIAN_POINT('Ctrl Pts',(-7.19988399878459,4.15930620199099,
1.39228780605833));
#131993=CARTESIAN_POINT('Ctrl Pts',(-7.1589543988164,4.16602041376379,1.38452403064383));
#131994=CARTESIAN_POINT('Ctrl Pts',(-7.1180715326786,4.17289950622846,1.37679252684336));
#131995=CARTESIAN_POINT('Ctrl Pts',(-7.22301412936999,4.042807359,0.5957465609));
#131996=CARTESIAN_POINT('Ctrl Pts',(-7.19048996598,4.108510123,0.990079504110001));
#131997=CARTESIAN_POINT('Ctrl Pts',(-7.11523065735001,4.173674111,1.37852811994));
#131998=CARTESIAN_POINT('Ctrl Pts',(-7.225262378,4.042807359,0.59840084));
#131999=CARTESIAN_POINT('Ctrl Pts',(-7.192593307,4.108510123,0.992856524000001));
#132000=CARTESIAN_POINT('Ctrl Pts',(-7.11717659000001,4.173674111,1.381411376));
#132001=CARTESIAN_POINT('Ctrl Pts',(-7.450087241,4.042807359,0.86382875));
#132002=CARTESIAN_POINT('Ctrl Pts',(-7.402927409,4.108510123,1.270558513));
#132003=CARTESIAN_POINT('Ctrl Pts',(-7.311769855,4.173674111,1.669736982));
#132004=CARTESIAN_POINT('Origin',(0.197660024976012,4.01786908484965,-0.0121803578723476));
#132005=CARTESIAN_POINT('Ctrl Pts',(-7.247502549,4.173681702,-0.190280849));
#132006=CARTESIAN_POINT('Ctrl Pts',(-7.257871751,4.108088716,0.204665976));
#132007=CARTESIAN_POINT('Ctrl Pts',(-7.225262378,4.042807359,0.59840084));
#132008=CARTESIAN_POINT('Ctrl Pts',(-7.22413512038967,4.04055067941005,
0.612011669680603));
#132009=CARTESIAN_POINT('Ctrl Pts',(-7.22300786277932,4.03829399982003,
0.625622499361206));
#132010=CARTESIAN_POINT('Ctrl Pts',(-7.48742264462432,4.173681702,-0.443138670805177));
#132011=CARTESIAN_POINT('Ctrl Pts',(-7.51157113006956,4.108088716,-0.0351175931109789));
#132012=CARTESIAN_POINT('Ctrl Pts',(-7.49123872278329,4.042807359,0.373111438402523));
#132013=CARTESIAN_POINT('Ctrl Pts',(-7.4905358616504,4.04055067941005,0.387223309934955));
#132014=CARTESIAN_POINT('Ctrl Pts',(-7.48983300051752,4.03829399982002,
0.401335181467389));
#132015=CARTESIAN_POINT('',(-7.24762467318051,4.17289950634919,-0.185571082546173));
#132016=CARTESIAN_POINT('Origin',(0.199108805722675,4.16071257662121,0.00309198393094883));
#132017=CARTESIAN_POINT('Ctrl Pts',(-7.49752274180161,4.13354309997187,
-0.192750430437809));
#132018=CARTESIAN_POINT('Ctrl Pts',(-7.45583213525102,4.13979627442737,
-0.19159297045491));
#132019=CARTESIAN_POINT('Ctrl Pts',(-7.41414145586947,4.14619777517913,
-0.190416688450836));
#132020=CARTESIAN_POINT('Ctrl Pts',(-7.33085543430957,4.15930620200286,
-0.188025341891005));
#132021=CARTESIAN_POINT('Ctrl Pts',(-7.28921376519328,4.16602041349394,
-0.186808950522999));
#132022=CARTESIAN_POINT('Ctrl Pts',(-7.24762467294151,4.17289950595543,
-0.185571088387518));
#132023=CARTESIAN_POINT('Ctrl Pts',(-7.18221197363,4.042807359,-0.970916189530001));
#132024=CARTESIAN_POINT('Ctrl Pts',(-7.23521813274001,4.108510123,-0.57881079857));
#132025=CARTESIAN_POINT('Ctrl Pts',(-7.24522331535001,4.173674111,-0.18326536814));
#132026=CARTESIAN_POINT('Ctrl Pts',(-7.184978251,4.042807359,-0.968807273));
#132027=CARTESIAN_POINT('Ctrl Pts',(-7.237869276,4.108510123,-0.57655086));
#132028=CARTESIAN_POINT('Ctrl Pts',(-7.247743568,4.173674111,-0.180867839));
#132029=CARTESIAN_POINT('Ctrl Pts',(-7.461605988,4.042807359,-0.75791562));
#132030=CARTESIAN_POINT('Ctrl Pts',(-7.502983602,4.108510123,-0.350557003));
#132031=CARTESIAN_POINT('Ctrl Pts',(-7.499768833,4.173674111,0.058885075));
#132032=CARTESIAN_POINT('Origin',(0.195657217993492,4.01786906992177,0.0305954721080647));
#132033=CARTESIAN_POINT('Ctrl Pts',(-7.037155209,4.173681702,-1.743831002));
#132034=CARTESIAN_POINT('Ctrl Pts',(-7.13218387800001,4.108088716,-1.360346886));
#132035=CARTESIAN_POINT('Ctrl Pts',(-7.18497825100001,4.042807359,-0.968807273));
#132036=CARTESIAN_POINT('Ctrl Pts',(-7.18680327408043,4.04055067942458,
-0.955272329974366));
#132037=CARTESIAN_POINT('Ctrl Pts',(-7.18862829716087,4.03829399984908,
-0.941737386948719));
#132038=CARTESIAN_POINT('Ctrl Pts',(-7.21710914931246,4.173681702,-2.04235287662919));
#132039=CARTESIAN_POINT('Ctrl Pts',(-7.32840552681098,4.108088716,-1.64906231605176));
#132040=CARTESIAN_POINT('Ctrl Pts',(-7.39630565439742,4.042807359,-1.24600658618435));
#132041=CARTESIAN_POINT('Ctrl Pts',(-7.39865286098343,4.04055067942458,
-1.23207354809886));
#132042=CARTESIAN_POINT('Ctrl Pts',(-7.40100006756945,4.03829399984908,
-1.21814051001333));
#132043=CARTESIAN_POINT('',(-7.03828695718376,4.17289951177251,-1.73925752363152));
#132044=CARTESIAN_POINT('Origin',(0.193788930123852,4.16071258056698,0.0458221794985492));
#132045=CARTESIAN_POINT('Ctrl Pts',(-7.28079918183226,4.13354309998201,
-1.7999897968914));
#132046=CARTESIAN_POINT('Ctrl Pts',(-7.24033209814515,4.13979627444535,
-1.78989714956336));
#132047=CARTESIAN_POINT('Ctrl Pts',(-7.19986898956744,4.14619777519187,
-1.77978610465057));
#132048=CARTESIAN_POINT('Ctrl Pts',(-7.11904421763658,4.15930620201941,
-1.75954663372673));
#132049=CARTESIAN_POINT('Ctrl Pts',(-7.07863759428674,4.16602041375186,
-1.74940695265407));
#132050=CARTESIAN_POINT('Ctrl Pts',(-7.03828693559596,4.17289950621262,
-1.73925760568948));
#132051=CARTESIAN_POINT('Ctrl Pts',(-6.80557756794,4.042807359,-2.49217997837));
#132052=CARTESIAN_POINT('Ctrl Pts',(-6.94163554200999,4.108510123,-2.12063655002));
#132053=CARTESIAN_POINT('Ctrl Pts',(-7.03643738356,4.173674111,-1.73648957142));
#132054=CARTESIAN_POINT('Ctrl Pts',(-6.808732526,4.042807359,-2.490715035));
#132055=CARTESIAN_POINT('Ctrl Pts',(-6.944710523,4.108510123,-2.118999365));
#132056=CARTESIAN_POINT('Ctrl Pts',(-7.039414112,4.173674111,-1.734689875));
#132057=CARTESIAN_POINT('Ctrl Pts',(-7.12422833200001,4.042807359,-2.344220698));
#132058=CARTESIAN_POINT('Ctrl Pts',(-7.252208622,4.108510123,-1.955280863));
#132059=CARTESIAN_POINT('Ctrl Pts',(-7.33708695600001,4.173674111,-1.554720233));
#132060=CARTESIAN_POINT('Origin',(0.184505509730328,4.01786907984804,0.0719406205453618));
#132061=CARTESIAN_POINT('Ctrl Pts',(-6.497758313,4.173681702,-3.215841555));
#132062=CARTESIAN_POINT('Ctrl Pts',(-6.67300301300001,4.108088716,-2.86175144));
#132063=CARTESIAN_POINT('Ctrl Pts',(-6.808732526,4.042807359,-2.490715035));
#132064=CARTESIAN_POINT('Ctrl Pts',(-6.81342449392482,4.04055067932614,
-2.47788885687033));
#132065=CARTESIAN_POINT('Ctrl Pts',(-6.81811646184952,4.03829399965221,
-2.46506267874058));
#132066=CARTESIAN_POINT('Ctrl Pts',(-6.60933165069055,4.173681702,-3.54606893239908));
#132067=CARTESIAN_POINT('Ctrl Pts',(-6.80257182679263,4.108088716,-3.1858987174254));
#132068=CARTESIAN_POINT('Ctrl Pts',(-6.95552955382461,4.042807359,-2.80686272653251));
#132069=CARTESIAN_POINT('Ctrl Pts',(-6.96081707555239,4.04055067932614,
-2.793760014585));
#132070=CARTESIAN_POINT('Ctrl Pts',(-6.96610459728,4.03829399965221,-2.7806573026375));
#132071=CARTESIAN_POINT('',(-6.49984676413174,4.17289951180422,-3.21161829486362));
#132072=CARTESIAN_POINT('Origin',(0.179407972082283,4.16071260285053,0.0864098315335438));
#132073=CARTESIAN_POINT('Ctrl Pts',(-6.72363354399547,4.13354310000101,
-3.32306364090028));
#132074=CARTESIAN_POINT('Ctrl Pts',(-6.68628217907727,4.13979627445217,
-3.30450772734517));
#132075=CARTESIAN_POINT('Ctrl Pts',(-6.64893865122487,4.14619777519857,
-3.28593470078994));
#132076=CARTESIAN_POINT('Ctrl Pts',(-6.57435440562825,4.15930620201408,
-3.24879348059528));
#132077=CARTESIAN_POINT('Ctrl Pts',(-6.53707219854965,4.16602041373077,
-3.23020462996973));
#132078=CARTESIAN_POINT('Ctrl Pts',(-6.49984672556043,4.17289950620038,
-3.21161837004206));
#132079=CARTESIAN_POINT('Ctrl Pts',(-6.11072191959001,4.042807359,-3.89691220109));
#132080=CARTESIAN_POINT('Ctrl Pts',(-6.32346978797,4.108510123,-3.56330369453));
#132081=CARTESIAN_POINT('Ctrl Pts',(-6.49863546028999,4.173674111,-3.20851745189));
#132082=CARTESIAN_POINT('Ctrl Pts',(-6.11411803600001,4.042807359,-3.89615973));
#132083=CARTESIAN_POINT('Ctrl Pts',(-6.326824824,4.108510123,-3.562365816));
#132084=CARTESIAN_POINT('Ctrl Pts',(-6.501929476,4.173674111,-3.20739974));
#132085=CARTESIAN_POINT('Ctrl Pts',(-6.453729677,4.042807359,-3.820912621));
#132086=CARTESIAN_POINT('Ctrl Pts',(-6.662328427,4.108510123,-3.468577963));
#132087=CARTESIAN_POINT('Ctrl Pts',(-6.831331047,4.173674111,-3.095628551));
#132088=CARTESIAN_POINT('Origin',(0.164726898386173,4.01786907394915,0.109921998321732));
#132089=CARTESIAN_POINT('Ctrl Pts',(-5.65453346,4.173681702,-4.537482931));
#132090=CARTESIAN_POINT('Ctrl Pts',(-5.901799944,4.108088716,-4.229343677));
#132091=CARTESIAN_POINT('Ctrl Pts',(-6.114118036,4.042807359,-3.89615973));
#132092=CARTESIAN_POINT('Ctrl Pts',(-6.12145755719561,4.04055067941673,
-3.88464205565578));
#132093=CARTESIAN_POINT('Ctrl Pts',(-6.12879707839122,4.03829399983337,
-3.8731243813116));
#132094=CARTESIAN_POINT('Ctrl Pts',(-5.69250915066893,4.173681702,-4.88397474512415));
#132095=CARTESIAN_POINT('Ctrl Pts',(-5.95865742732614,4.108088716,-4.57376603597331));
#132096=CARTESIAN_POINT('Ctrl Pts',(-6.18952062274081,4.042807359,-4.23647308634029));
#132097=CARTESIAN_POINT('Ctrl Pts',(-6.19750122062614,4.04055067941672,
-4.22481336987599));
#132098=CARTESIAN_POINT('Ctrl Pts',(-6.20548181851142,4.03829399983338,
-4.21315365341175));
#132099=CARTESIAN_POINT('',(-5.65748091122045,4.1728995063871,-4.5338074256061));
#132100=CARTESIAN_POINT('Origin',(0.156637907631271,4.16071263150207,0.122957005372363));
#132101=CARTESIAN_POINT('Ctrl Pts',(-5.85207827440955,4.13354310000206,
-4.69075472210398));
#132102=CARTESIAN_POINT('Ctrl Pts',(-5.81958913659606,4.13979627445759,
-4.66460319612005));
#132103=CARTESIAN_POINT('Ctrl Pts',(-5.78711133136791,4.14619777521706,
-4.63843664194184));
#132104=CARTESIAN_POINT('Ctrl Pts',(-5.72225508847915,4.15930620204372,
-4.58613035472719));
#132105=CARTESIAN_POINT('Ctrl Pts',(-5.68984057334137,4.16602041350361,
-4.55996152965675));
#132106=CARTESIAN_POINT('Ctrl Pts',(-5.657480907676,4.17289950597006,-4.53380742988185));
#132107=CARTESIAN_POINT('Ctrl Pts',(-5.13013570587,4.042807359,-5.11942914009));
#132108=CARTESIAN_POINT('Ctrl Pts',(-5.40962561367999,4.108510123,-4.83935471788));
#132109=CARTESIAN_POINT('Ctrl Pts',(-5.65696456552999,4.173674111,-4.5305186224));
#132110=CARTESIAN_POINT('Ctrl Pts',(-5.133614182,4.042807359,-5.119424326));
#132111=CARTESIAN_POINT('Ctrl Pts',(-5.413103827,4.108510123,-4.83916));
#132112=CARTESIAN_POINT('Ctrl Pts',(-5.660421844,4.173674111,-4.530135158));
#132113=CARTESIAN_POINT('Ctrl Pts',(-5.481461795,4.042807359,-5.118942917));
#132114=CARTESIAN_POINT('Ctrl Pts',(-5.760925159,4.108510123,-4.819688212));
#132115=CARTESIAN_POINT('Ctrl Pts',(-6.00614969100001,4.173674111,-4.491788718));
#132116=CARTESIAN_POINT('Origin',(0.137245792838453,4.01786906965473,0.142763576683332));
#132117=CARTESIAN_POINT('Ctrl Pts',(-4.546908906,4.173681702,-5.646956649));
#132118=CARTESIAN_POINT('Ctrl Pts',(-4.854635269,4.108088716,-5.399176504));
#132119=CARTESIAN_POINT('Ctrl Pts',(-5.133614182,4.042807359,-5.119424326));
#132120=CARTESIAN_POINT('Ctrl Pts',(-5.14325806887437,4.0405506793996,-5.10975370850253));
#132121=CARTESIAN_POINT('Ctrl Pts',(-5.15290195574862,4.03829399979913,
-5.10008309100504));
#132122=CARTESIAN_POINT('Ctrl Pts',(-4.50951124921801,4.173681702,-5.99351132775443));
#132123=CARTESIAN_POINT('Ctrl Pts',(-4.83612282993789,4.108088716,-5.7477691379534));
#132124=CARTESIAN_POINT('Ctrl Pts',(-5.13409658570113,4.042807359,-5.46799067275003));
#132125=CARTESIAN_POINT('Ctrl Pts',(-5.14439709609169,4.0405506793996,-5.45831914654295));
#132126=CARTESIAN_POINT('Ctrl Pts',(-5.15469760648239,4.03829399979914,
-5.44864762033589));
#132127=CARTESIAN_POINT('',(-4.55057757302164,4.17289950635597,-5.6440006891764));
#132128=CARTESIAN_POINT('Origin',(0.126543657505769,4.16071261389245,0.153754834376969));
#132129=CARTESIAN_POINT('Ctrl Pts',(-4.7068863288185,4.13354310002961,-5.83911132633498));
#132130=CARTESIAN_POINT('Ctrl Pts',(-4.68077857400211,4.13979627448026,
-5.8065870041996));
#132131=CARTESIAN_POINT('Ctrl Pts',(-4.65468511743214,4.14619777522813,
-5.7740504414094));
#132132=CARTESIAN_POINT('Ctrl Pts',(-4.60258948287892,4.15930620202736,
-5.70902487101796));
#132133=CARTESIAN_POINT('Ctrl Pts',(-4.57655832475415,4.16602041348794,
-5.67649969586828));
#132134=CARTESIAN_POINT('Ctrl Pts',(-4.55057756827482,4.17289950593458,
-5.64400069288196));
#132135=CARTESIAN_POINT('Ctrl Pts',(-3.90967004782,4.042807359,-6.102567263));
#132136=CARTESIAN_POINT('Ctrl Pts',(-4.24283335879,4.108510123,-5.88912289343));
#132137=CARTESIAN_POINT('Ctrl Pts',(-4.55078029527,4.173674111,-5.64067777754));
#132138=CARTESIAN_POINT('Ctrl Pts',(-3.913068234,4.042807359,-6.103310331));
#132139=CARTESIAN_POINT('Ctrl Pts',(-4.246272112,4.108510123,-5.889680441));
#132140=CARTESIAN_POINT('Ctrl Pts',(-4.554239178,4.173674111,-5.641046491));
#132141=CARTESIAN_POINT('Ctrl Pts',(-4.252886852,4.042807359,-6.177617131));
#132142=CARTESIAN_POINT('Ctrl Pts',(-4.590147433,4.108510123,-5.945435198));
#132143=CARTESIAN_POINT('Ctrl Pts',(-4.900127451,4.173674111,-5.677917837));
#132144=CARTESIAN_POINT('Origin',(0.103347005926283,4.01786907058862,0.168929478668518));
#132145=CARTESIAN_POINT('Ctrl Pts',(-3.226675946,4.173681702,-6.49238495));
#132146=CARTESIAN_POINT('Ctrl Pts',(-3.580473244,4.108088716,-6.316549838));
#132147=CARTESIAN_POINT('Ctrl Pts',(-3.913068234,4.042807359,-6.103310331));
#132148=CARTESIAN_POINT('Ctrl Pts',(-3.92456554946237,4.0405506793211,-6.09593895754359));
#132149=CARTESIAN_POINT('Ctrl Pts',(-3.9360628649248,4.03829399964212,-6.08856758408716));
#132150=CARTESIAN_POINT('Ctrl Pts',(-3.11565361346413,4.173681702,-6.82279798221495));
#132151=CARTESIAN_POINT('Ctrl Pts',(-3.48745650442695,4.108088716,-6.65301294327412));
#132152=CARTESIAN_POINT('Ctrl Pts',(-3.83860789814411,4.042807359,-6.44383109203186));
#132153=CARTESIAN_POINT('Ctrl Pts',(-3.85074668095807,4.0405506793211,-6.43659998571625));
#132154=CARTESIAN_POINT('Ctrl Pts',(-3.86288546377205,4.03829399964212,
-6.42936887940052));
#132155=CARTESIAN_POINT('',(-3.2308943560275,4.17289951171542,-6.49028671834694));
#132156=CARTESIAN_POINT('Origin',(0.0905324415274239,4.16071263741196,0.177363367578599));
#132157=CARTESIAN_POINT('Ctrl Pts',(-3.34160561000943,4.13354310003923,
-6.71443757429057));
#132158=CARTESIAN_POINT('Ctrl Pts',(-3.32310000783745,4.1397962744689,-6.67706125735356));
#132159=CARTESIAN_POINT('Ctrl Pts',(-3.30461100089086,4.14619777523478,
-6.6396760594406));
#132160=CARTESIAN_POINT('Ctrl Pts',(-3.26771190878886,4.15930620202176,
-6.56497172952417));
#132161=CARTESIAN_POINT('Ctrl Pts',(-3.24928129517904,4.16602041374647,
-6.52761104404165));
#132162=CARTESIAN_POINT('Ctrl Pts',(-3.23089427937063,4.17289950621232,
-6.49028675509605));
#132163=CARTESIAN_POINT('Ctrl Pts',(-2.50639256418,4.042807359,-6.80035612293));
#132164=CARTESIAN_POINT('Ctrl Pts',(-2.87765093218,4.108510123,-6.6635222283));
#132165=CARTESIAN_POINT('Ctrl Pts',(-3.23180659552,4.173674111,-6.48708510932001));
#132166=CARTESIAN_POINT('Ctrl Pts',(-2.509551565,4.042807359,-6.801812328));
#132167=CARTESIAN_POINT('Ctrl Pts',(-2.880889433,4.108510123,-6.66480597100001));
#132168=CARTESIAN_POINT('Ctrl Pts',(-3.235105349,4.173674111,-6.48818876));
#132169=CARTESIAN_POINT('Ctrl Pts',(-2.825451647,4.042807359,-6.947432835));
#132170=CARTESIAN_POINT('Ctrl Pts',(-3.204739515,4.108510123,-6.793180241));
#132171=CARTESIAN_POINT('Ctrl Pts',(-3.564980697,4.173674111,-6.59855382800001));
#132172=CARTESIAN_POINT('Origin',(0.0646159969929783,4.01786908411667,0.187196633203744));
#132173=CARTESIAN_POINT('Ctrl Pts',(-1.755567205,4.173681702,-7.034236546));
#132174=CARTESIAN_POINT('Ctrl Pts',(-2.13889227,4.108088716,-6.93856832300001));
#132175=CARTESIAN_POINT('Ctrl Pts',(-2.509551565,4.042807359,-6.801812328));
#132176=CARTESIAN_POINT('Ctrl Pts',(-2.5223647071198,4.04055067930441,-6.79708487606959));
#132177=CARTESIAN_POINT('Ctrl Pts',(-2.53517784923958,4.03829399960873,
-6.79235742413929));
#132178=CARTESIAN_POINT('Ctrl Pts',(-1.57611147796785,4.173681702,-7.33305818576814));
#132179=CARTESIAN_POINT('Ctrl Pts',(-1.97572058815388,4.108088716,-7.2471692583663));
#132180=CARTESIAN_POINT('Ctrl Pts',(-2.36363017270524,4.042807359,-7.11836513186759));
#132181=CARTESIAN_POINT('Ctrl Pts',(-2.37703963175169,4.04055067930441,
-7.11391256423821));
#132182=CARTESIAN_POINT('Ctrl Pts',(-2.39044909079814,4.03829399960874,
-7.10945999660886));
#132183=CARTESIAN_POINT('',(-1.7601380483259,4.17289951177404,-7.03309420339446));
#132184=CARTESIAN_POINT('Origin',(0.050287931064856,4.16071264270228,0.192678423367151));
#132185=CARTESIAN_POINT('Ctrl Pts',(-1.82007512674651,4.13354310004032,
-7.27580418456825));
#132186=CARTESIAN_POINT('Ctrl Pts',(-1.81003697857167,4.13979627448677,
-7.23532354751039));
#132187=CARTESIAN_POINT('Ctrl Pts',(-1.80001694685657,4.14619777523088,
-7.19483780481292));
#132188=CARTESIAN_POINT('Ctrl Pts',(-1.78003975777084,4.1593062020288,-7.11394780620897));
#132189=CARTESIAN_POINT('Ctrl Pts',(-1.77007148471205,4.1660204137524,-7.0734985555225));
#132190=CARTESIAN_POINT('Ctrl Pts',(-1.76013796597784,4.17289950621194,
-7.03309422269299));
#132191=CARTESIAN_POINT('Ctrl Pts',(-0.9859189489,4.042807359,-7.1801678884));
#132192=CARTESIAN_POINT('Ctrl Pts',(-1.37791274627,4.108510123,-7.12634266953999));
#132193=CARTESIAN_POINT('Ctrl Pts',(-1.76171721181001,4.173674111,-7.03016355056001));
#132194=CARTESIAN_POINT('Ctrl Pts',(-0.988691053,4.042807359,-7.18226914));
#132195=CARTESIAN_POINT('Ctrl Pts',(-1.380799566,4.108510123,-7.128292581));
#132196=CARTESIAN_POINT('Ctrl Pts',(-1.76470159,4.173674111,-7.031950533));
#132197=CARTESIAN_POINT('Ctrl Pts',(-1.265901463,4.042807359,-7.3923943));
#132198=CARTESIAN_POINT('Ctrl Pts',(-1.669481539,4.108510123,-7.323283727));
#132199=CARTESIAN_POINT('Ctrl Pts',(-2.063139409,4.173674111,-7.210648777));
#132200=CARTESIAN_POINT('Origin',(0.0228636093082184,4.01786908234283,0.196710782424259));
#132201=CARTESIAN_POINT('Ctrl Pts',(-0.202370093,4.173681702,-7.24717506));
#132202=CARTESIAN_POINT('Ctrl Pts',(-0.597299071,4.108088716,-7.236147064));
#132203=CARTESIAN_POINT('Ctrl Pts',(-0.988691053000001,4.042807359,-7.18226914));
#132204=CARTESIAN_POINT('Ctrl Pts',(-1.00222089300913,4.04055067936321,
-7.18040666011983));
#132205=CARTESIAN_POINT('Ctrl Pts',(-1.01575073301826,4.03829399972634,
-7.17854418023955));
#132206=CARTESIAN_POINT('Ctrl Pts',(0.0371278792295015,4.173681702,-7.50043273830741));
#132207=CARTESIAN_POINT('Ctrl Pts',(-0.371602173148536,4.108088716,-7.50245599257189));
#132208=CARTESIAN_POINT('Ctrl Pts',(-0.778131726340653,4.042807359,-7.46005233013564));
#132209=CARTESIAN_POINT('Ctrl Pts',(-0.7921848497224,4.04055067936321,-7.45858649845042));
#132210=CARTESIAN_POINT('Ctrl Pts',(-0.806237973104149,4.03829399972634,
-7.45712066676505));
#132211=CARTESIAN_POINT('',(-0.207079563622813,4.17289950638492,-7.24704202295315));
#132212=CARTESIAN_POINT('Origin',(0.00769208186321351,4.16071261746617,
0.198984214355209));
#132213=CARTESIAN_POINT('Ctrl Pts',(-0.213439952651149,4.13354310325808,
-7.49696225529674));
#132214=CARTESIAN_POINT('Ctrl Pts',(-0.212338631208263,4.13979627774058,
-7.45527012810047));
#132215=CARTESIAN_POINT('Ctrl Pts',(-0.21125610081469,4.14619777521567,
-7.41357693052393));
#132216=CARTESIAN_POINT('Ctrl Pts',(-0.209134926115335,4.15930620200786,
-7.33028359035146));
#132217=CARTESIAN_POINT('Ctrl Pts',(-0.208095099130585,4.16602041357748,
-7.2886371377501));
#132218=CARTESIAN_POINT('Ctrl Pts',(-0.207079557951058,4.172899506042,-7.24704202303491));
#132219=CARTESIAN_POINT('Ctrl Pts',(0.580655139860001,4.042807359,-7.22424298406));
#132220=CARTESIAN_POINT('Ctrl Pts',(0.18625510917,4.108510123,-7.25594324748));
#132221=CARTESIAN_POINT('Ctrl Pts',(-0.20925188932,4.173674111,-7.24451935813));
#132222=CARTESIAN_POINT('Ctrl Pts',(0.578399553,4.042807359,-7.22689103));
#132223=CARTESIAN_POINT('Ctrl Pts',(0.183854955,4.108510123,-7.258468152));
#132224=CARTESIAN_POINT('Ctrl Pts',(-0.211782346,4.173674111,-7.24690611500001));
#132225=CARTESIAN_POINT('Ctrl Pts',(0.352840867,4.042807359,-7.491695624));
#132226=CARTESIAN_POINT('Ctrl Pts',(-0.056160462,4.108510123,-7.510958604));
#132227=CARTESIAN_POINT('Ctrl Pts',(-0.464828014,4.173674111,-7.485581802));
#132228=CARTESIAN_POINT('Origin',(-0.0199579329223511,4.01786909089896,
0.197026828565895));
#132229=CARTESIAN_POINT('Ctrl Pts',(1.360289621,4.173681702,-7.121243722));
#132230=CARTESIAN_POINT('Ctrl Pts',(0.972223169,4.108088716,-7.195371611));
#132231=CARTESIAN_POINT('Ctrl Pts',(0.578399553,4.042807359,-7.22689103));
#132232=CARTESIAN_POINT('Ctrl Pts',(0.564785654758208,4.04055067932115,
-7.22798060956172));
#132233=CARTESIAN_POINT('Ctrl Pts',(0.551171756516431,4.03829399964222,
-7.22907018912331));
#132234=CARTESIAN_POINT('Ctrl Pts',(1.64863117716287,4.173681702,-7.31709539294683));
#132235=CARTESIAN_POINT('Ctrl Pts',(1.24989194723257,4.108088716,-7.40693622353508));
#132236=CARTESIAN_POINT('Ctrl Pts',(0.843751293891402,4.042807359,-7.4529157718641));
#132237=CARTESIAN_POINT('Ctrl Pts',(0.829711613938738,4.04055067932115,
-7.45450521664782));
#132238=CARTESIAN_POINT('Ctrl Pts',(0.815671933986074,4.03829399964222,
-7.45609466143153));
#132239=CARTESIAN_POINT('',(1.35566157838182,4.17289951177391,-7.12212620752211));
#132240=CARTESIAN_POINT('Origin',(-0.0352634846856975,4.16071259653434,
0.19598567199083));
#132241=CARTESIAN_POINT('Ctrl Pts',(1.40317543510752,4.13354310004224,-7.36757074577745));
#132242=CARTESIAN_POINT('Ctrl Pts',(1.39528843329839,4.13979627446409,-7.32661660577024));
#132243=CARTESIAN_POINT('Ctrl Pts',(1.3873828455856,4.14619777522124,-7.28566543866845));
#132244=CARTESIAN_POINT('Ctrl Pts',(1.37154882246648,4.15930620197364,-7.20386346053619));
#132245=CARTESIAN_POINT('Ctrl Pts',(1.36361158256332,4.1660204136406,-7.16296714596945));
#132246=CARTESIAN_POINT('Ctrl Pts',(1.35566166098924,4.17289950607299,-7.12212619048186));
#132247=CARTESIAN_POINT('Ctrl Pts',(2.12007843989,4.042807359,-6.9305205064));
#132248=CARTESIAN_POINT('Ctrl Pts',(1.74171388206,4.108510123,-7.04626398314));
#132249=CARTESIAN_POINT('Ctrl Pts',(1.35299781883,4.173674111,-7.12012949179001));
#132250=CARTESIAN_POINT('Ctrl Pts',(2.118444839,4.042807359,-6.933591527));
#132251=CARTESIAN_POINT('Ctrl Pts',(1.739912622,4.108510123,-7.049245819));
#132252=CARTESIAN_POINT('Ctrl Pts',(1.351039605,4.173674111,-7.12300442100001));
#132253=CARTESIAN_POINT('Ctrl Pts',(1.95508475,4.042807359,-7.240693587));
#132254=CARTESIAN_POINT('Ctrl Pts',(1.559786616,4.108510123,-7.347429405));
#132255=CARTESIAN_POINT('Ctrl Pts',(1.155218222,4.173674111,-7.41049734200001));
#132256=CARTESIAN_POINT('Origin',(-0.0618462821909793,4.01786907401881,
0.188130101067273));
#132257=CARTESIAN_POINT('Ctrl Pts',(2.859343703,4.173681702,-6.662330943));
#132258=CARTESIAN_POINT('Ctrl Pts',(2.496285335,4.108088716,-6.818148579));
#132259=CARTESIAN_POINT('Ctrl Pts',(2.118444839,4.042807359,-6.933591527));
#132260=CARTESIAN_POINT('Ctrl Pts',(2.1053834537122,4.04055067935632,-6.93758221841224));
#132261=CARTESIAN_POINT('Ctrl Pts',(2.09232206842445,4.03829399971256,-6.94157290982447));
#132262=CARTESIAN_POINT('Ctrl Pts',(3.18304631452949,4.173681702,-6.79161879846189));
#132263=CARTESIAN_POINT('Ctrl Pts',(2.81294250805857,4.108088716,-6.96507634840558));
#132264=CARTESIAN_POINT('Ctrl Pts',(2.42618144212599,4.042807359,-7.09728915532336));
#132265=CARTESIAN_POINT('Ctrl Pts',(2.41281168597241,4.04055067935632,-7.10185955587442));
#132266=CARTESIAN_POINT('Ctrl Pts',(2.3994419298189,4.03829399971257,-7.10642995642561));
#132267=CARTESIAN_POINT('',(2.85501356984558,4.17289951177047,-6.6641876880865));
#132268=CARTESIAN_POINT('Origin',(-0.0765701649059569,4.16071261020573,
0.183823023449187));
#132269=CARTESIAN_POINT('Ctrl Pts',(2.95417989991717,4.13354310002489,-6.89367979482904));
#132270=CARTESIAN_POINT('Ctrl Pts',(2.93767336231485,4.13979627446358,-6.85537861209491));
#132271=CARTESIAN_POINT('Ctrl Pts',(2.92114931248078,4.14619777520393,-6.8170843284045));
#132272=CARTESIAN_POINT('Ctrl Pts',(2.888100472612,4.15930620198082,-6.74059868211742));
#132273=CARTESIAN_POINT('Ctrl Pts',(2.87155730183866,4.16602041376059,-6.70236477214455));
#132274=CARTESIAN_POINT('Ctrl Pts',(2.85501364662232,4.17289950620053,-6.66418765381247));
#132275=CARTESIAN_POINT('Ctrl Pts',(3.56036922856,4.042807359,-6.31273459326));
#132276=CARTESIAN_POINT('Ctrl Pts',(3.21573205004,4.108510123,-6.50710924714));
#132277=CARTESIAN_POINT('Ctrl Pts',(2.85198285308,4.173674111,-6.66281028394001));
#132278=CARTESIAN_POINT('Ctrl Pts',(3.559433999,4.042807359,-6.316084991));
#132279=CARTESIAN_POINT('Ctrl Pts',(3.214613909,4.108510123,-6.510408587));
#132280=CARTESIAN_POINT('Ctrl Pts',(2.850688446,4.173674111,-6.66603895700001));
#132281=CARTESIAN_POINT('Ctrl Pts',(3.465911043,4.042807359,-6.651124765));
#132282=CARTESIAN_POINT('Ctrl Pts',(3.102799805,4.108510123,-6.840342573));
#132283=CARTESIAN_POINT('Ctrl Pts',(2.721247738,4.173674111,-6.988906263));
#132284=CARTESIAN_POINT('Origin',(-0.1008426060641,4.01786904378294,0.170436281909311));
#132285=CARTESIAN_POINT('Ctrl Pts',(4.224698052,4.173681702,-5.891894973));
#132286=CARTESIAN_POINT('Ctrl Pts',(3.903623972,4.108088716,-6.122116497));
#132287=CARTESIAN_POINT('Ctrl Pts',(3.559433999,4.042807359,-6.316084991));
#132288=CARTESIAN_POINT('Ctrl Pts',(3.54753586259605,4.04055067940109,-6.32279019388423));
#132289=CARTESIAN_POINT('Ctrl Pts',(3.53563772619209,4.03829399980212,-6.32949539676845));
#132290=CARTESIAN_POINT('Ctrl Pts',(4.56862574298852,4.173681702,-5.94857365764975));
#132291=CARTESIAN_POINT('Ctrl Pts',(4.24446300427223,4.108088716,-6.19753724418816));
#132292=CARTESIAN_POINT('Ctrl Pts',(3.89516604182199,4.042807359,-6.40980118682287));
#132293=CARTESIAN_POINT('Ctrl Pts',(3.88309136437426,4.0405506794011,-6.4171388362061));
#132294=CARTESIAN_POINT('Ctrl Pts',(3.87101668692651,4.03829399980211,-6.42447648558946));
#132295=CARTESIAN_POINT('',(4.22086836463542,4.1728995063624,-5.89463911385087));
#132296=CARTESIAN_POINT('Origin',(-0.114296549845329,4.16071257439138,0.16306507739361));
#132297=CARTESIAN_POINT('Ctrl Pts',(4.36705019567237,4.13354310002302,-6.09744803842827));
#132298=CARTESIAN_POINT('Ctrl Pts',(4.34269594963005,4.13979627447705,-6.06359073367165));
#132299=CARTESIAN_POINT('Ctrl Pts',(4.31832608394857,4.14619777521901,-6.02974393134162));
#132300=CARTESIAN_POINT('Ctrl Pts',(4.26960775467346,4.15930620202782,-5.96215100045011));
#132301=CARTESIAN_POINT('Ctrl Pts',(4.2452321948314,4.16602041350905,-5.92836727220656));
#132302=CARTESIAN_POINT('Ctrl Pts',(4.22086836934866,4.17289950595936,-5.89463911036402));
#132303=CARTESIAN_POINT('Ctrl Pts',(4.83418110893999,4.042807359,-5.39977222598));
#132304=CARTESIAN_POINT('Ctrl Pts',(4.53938616098,4.108510123,-5.6636893146));
#132305=CARTESIAN_POINT('Ctrl Pts',(4.2176123393,4.173674111,-5.89394547327));
#132306=CARTESIAN_POINT('Ctrl Pts',(4.833987981,4.042807359,-5.40324534));
#132307=CARTESIAN_POINT('Ctrl Pts',(4.539003422,4.108510123,-5.667151885));
#132308=CARTESIAN_POINT('Ctrl Pts',(4.217042264,4.173674111,-5.897376921));
#132309=CARTESIAN_POINT('Ctrl Pts',(4.814675187,4.042807359,-5.750556742));
#132310=CARTESIAN_POINT('Ctrl Pts',(4.500729524,4.108510123,-6.013408925));
#132311=CARTESIAN_POINT('Ctrl Pts',(4.160034734,4.173674111,-6.240521694));
#132312=CARTESIAN_POINT('Origin',(-0.135123824914297,4.0178690631926,0.144773525234887));
#132313=CARTESIAN_POINT('Ctrl Pts',(5.392510215,4.173681702,-4.845960543));
#132314=CARTESIAN_POINT('Ctrl Pts',(5.12843349100001,4.108088716,-5.139821051));
#132315=CARTESIAN_POINT('Ctrl Pts',(4.833987981,4.042807359,-5.40324534));
#132316=CARTESIAN_POINT('Ctrl Pts',(4.82380943690371,4.04055067941645,-5.41235152654575));
#132317=CARTESIAN_POINT('Ctrl Pts',(4.81363089280759,4.03829399983284,-5.4214577130914));
#132318=CARTESIAN_POINT('Ctrl Pts',(5.74058131055242,4.173681702,-4.82737982414742));
#132319=CARTESIAN_POINT('Ctrl Pts',(5.47751712737947,4.108088716,-5.14020818726269));
#132320=CARTESIAN_POINT('Ctrl Pts',(5.182017007808,4.042807359,-5.42259803764837));
#132321=CARTESIAN_POINT('Ctrl Pts',(5.17180200742472,4.04055067941645,-5.43235983549166));
#132322=CARTESIAN_POINT('Ctrl Pts',(5.16158700704133,4.03829399983283,-5.44212163333497));
#132323=CARTESIAN_POINT('',(5.38935991988585,4.17289951176709,-4.84946385508664));
#132324=CARTESIAN_POINT('Origin',(-0.146678535111375,4.16071263738005,0.134682317308428));
#132325=CARTESIAN_POINT('Ctrl Pts',(5.57572207796147,4.13354310000542,-5.01610638889035));
#132326=CARTESIAN_POINT('Ctrl Pts',(5.54465890095454,4.13979627444771,-4.98827609211711));
#132327=CARTESIAN_POINT('Ctrl Pts',(5.51358272710208,4.14619777520086,-4.96045940989693));
#132328=CARTESIAN_POINT('Ctrl Pts',(5.45147292314858,4.15930620201029,-4.9049197648852));
#132329=CARTESIAN_POINT('Ctrl Pts',(5.42040474616916,4.16602041376432,-4.87716590519808));
#132330=CARTESIAN_POINT('Ctrl Pts',(5.38935997551831,4.17289950624065,-4.84946379136899));
#132331=CARTESIAN_POINT('Ctrl Pts',(5.88195205285999,4.042807359,-4.23432251066));
#132332=CARTESIAN_POINT('Ctrl Pts',(5.65078362047,4.108510123,-4.55544156500999));
#132333=CARTESIAN_POINT('Ctrl Pts',(5.38603095943,4.173674111,-4.84948632227001));
#132334=CARTESIAN_POINT('Ctrl Pts',(5.882510057,4.042807359,-4.237755942));
#132335=CARTESIAN_POINT('Ctrl Pts',(5.65115418,4.108510123,-4.55890546));
#132336=CARTESIAN_POINT('Ctrl Pts',(5.386211872,4.173674111,-4.85296009400001));
#132337=CARTESIAN_POINT('Ctrl Pts',(5.938310471,4.042807359,-4.581099076));
#132338=CARTESIAN_POINT('Ctrl Pts',(5.688210133,4.108510123,-4.905294959));
#132339=CARTESIAN_POINT('Ctrl Pts',(5.40430312900001,4.173674111,-5.200337267));
#132340=CARTESIAN_POINT('Origin',(-0.163086559530075,4.01786906831046,0.112341029565017));
#132341=CARTESIAN_POINT('Ctrl Pts',(6.30817459400001,4.173681702,-3.573434383));
#132342=CARTESIAN_POINT('Ctrl Pts',(6.11344316000001,4.108088716,-3.917193286));
#132343=CARTESIAN_POINT('Ctrl Pts',(5.882510057,4.042807359,-4.237755942));
#132344=CARTESIAN_POINT('Ctrl Pts',(5.87452704205408,4.04055067928692,-4.24883731769155));
#132345=CARTESIAN_POINT('Ctrl Pts',(5.86654402710806,4.03829399957376,-4.25991869338303));
#132346=CARTESIAN_POINT('Ctrl Pts',(6.64411367476263,4.173681702,-3.48046307510273));
#132347=CARTESIAN_POINT('Ctrl Pts',(6.45444863851461,4.108088716,-3.84252870800095));
#132348=CARTESIAN_POINT('Ctrl Pts',(6.22656261649925,4.042807359,-4.18184023157307));
#132349=CARTESIAN_POINT('Ctrl Pts',(6.21868493462476,4.04055067928692,-4.19356972781599));
#132350=CARTESIAN_POINT('Ctrl Pts',(6.21080725275035,4.03829399957376,-4.20529922405897));
#132351=CARTESIAN_POINT('',(6.30585109886971,4.17289950635719,-3.5775329418795));
#132352=CARTESIAN_POINT('Origin',(-0.172201855024702,4.1607126089196,0.100001893504828));
#132353=CARTESIAN_POINT('Ctrl Pts',(6.52367939274731,4.13354309997313,-3.7002171795232));
#132354=CARTESIAN_POINT('Ctrl Pts',(6.48735976437488,4.13979627442715,-3.67971520436029));
#132355=CARTESIAN_POINT('Ctrl Pts',(6.45103036979152,4.14619777517902,-3.65922931941917));
#132356=CARTESIAN_POINT('Ctrl Pts',(6.37843327653972,4.15930620198339,-3.61833993218304));
#132357=CARTESIAN_POINT('Ctrl Pts',(6.34212519835251,4.16602041343716,-3.59791368279754));
#132358=CARTESIAN_POINT('Ctrl Pts',(6.30585110154139,4.17289950588202,-3.577532936964));
#132359=CARTESIAN_POINT('Ctrl Pts',(6.65468945644,4.042807359,-2.87088058177));
#132360=CARTESIAN_POINT('Ctrl Pts',(6.49795671792,4.108510123,-3.23418643029));
#132361=CARTESIAN_POINT('Ctrl Pts',(6.30260475782,4.173674111,-3.57827058098));
#132362=CARTESIAN_POINT('Ctrl Pts',(6.655972501,4.042807359,-2.874113787));
#132363=CARTESIAN_POINT('Ctrl Pts',(6.499063249,4.108510123,-3.237489682));
#132364=CARTESIAN_POINT('Ctrl Pts',(6.303528199,4.173674111,-3.581624247));
#132365=CARTESIAN_POINT('Ctrl Pts',(6.784276957,4.042807359,-3.19743431));
#132366=CARTESIAN_POINT('Ctrl Pts',(6.609716357,4.108510123,-3.567814853));
#132367=CARTESIAN_POINT('Ctrl Pts',(6.395872317,4.173674111,-3.916990849));
#132368=CARTESIAN_POINT('Origin',(-0.183423764448718,4.0178690710966,0.0746558063975883));
#132369=CARTESIAN_POINT('Ctrl Pts',(6.92887574,4.173681702,-2.133818404));
#132370=CARTESIAN_POINT('Ctrl Pts',(6.812595022,4.108088716,-2.511401917));
#132371=CARTESIAN_POINT('Ctrl Pts',(6.655972501,4.042807359,-2.874113787));
#132372=CARTESIAN_POINT('Ctrl Pts',(6.65055829288174,4.0405506793681,-2.88665219807012));
#132373=CARTESIAN_POINT('Ctrl Pts',(6.64514408476364,4.03829399973613,-2.89919060914025));
#132374=CARTESIAN_POINT('Ctrl Pts',(7.23697466922762,4.173681702,-1.97080374093111));
#132375=CARTESIAN_POINT('Ctrl Pts',(7.1295773034183,4.108088716,-2.36517685756169));
#132376=CARTESIAN_POINT('Ctrl Pts',(6.97996107817811,4.042807359,-2.74554422463711));
#132377=CARTESIAN_POINT('Ctrl Pts',(6.97478906730675,4.0405506793681,-2.7586929600398));
#132378=CARTESIAN_POINT('Ctrl Pts',(6.96961705643524,4.03829399973613,-2.77184169544254));
#132379=CARTESIAN_POINT('',(6.92748761210297,4.17289951179661,-2.13832069848568));
#132380=CARTESIAN_POINT('Origin',(-0.189673230629527,4.16071259632617,0.0606455671723691));
#132381=CARTESIAN_POINT('Ctrl Pts',(7.16659670980132,4.13354310001635,-2.211309927262));
#132382=CARTESIAN_POINT('Ctrl Pts',(7.12671889557544,4.13979627446342,-2.19909492345641));
#132383=CARTESIAN_POINT('Ctrl Pts',(7.08683500233852,4.14619777522031,-2.18689773310916));
#132384=CARTESIAN_POINT('Ctrl Pts',(7.00714517929606,4.1593062020332,-2.16257054614862));
#132385=CARTESIAN_POINT('Ctrl Pts',(6.96729492228005,4.16602041379438,-2.15042701411706));
#132386=CARTESIAN_POINT('Ctrl Pts',(6.92748763585173,4.17289950626471,-2.13832061725355));
#132387=CARTESIAN_POINT('Ctrl Pts',(7.11626097776,4.042807359,-1.37319946697));
#132388=CARTESIAN_POINT('Ctrl Pts',(7.04129258152,4.108510123,-1.76170433195));
#132389=CARTESIAN_POINT('Ctrl Pts',(6.92447576331001,4.173674111,-2.13973888338));
#132390=CARTESIAN_POINT('Ctrl Pts',(7.118209069,4.042807359,-1.376081265));
#132391=CARTESIAN_POINT('Ctrl Pts',(7.043083344,4.108510123,-1.764692484));
#132392=CARTESIAN_POINT('Ctrl Pts',(6.926098554,4.173674111,-2.14281563));
#132393=CARTESIAN_POINT('Ctrl Pts',(7.313018193,4.042807359,-1.664261068));
#132394=CARTESIAN_POINT('Ctrl Pts',(7.222159592,4.108510123,-2.063507689));
#132395=CARTESIAN_POINT('Ctrl Pts',(7.08837762300001,4.173674111,-2.450490292));
#132396=CARTESIAN_POINT('Origin',(-0.19518439295879,4.01786909364984,0.0334797583197854));
#132397=CARTESIAN_POINT('Ctrl Pts',(7.225590357,4.173681702,-0.594427447));
#132398=CARTESIAN_POINT('Ctrl Pts',(7.193197511,4.108088716,-0.988180185000001));
#132399=CARTESIAN_POINT('Ctrl Pts',(7.118209069,4.042807359,-1.376081265));
#132400=CARTESIAN_POINT('Ctrl Pts',(7.11561682978209,4.0405506793131,-1.38949043000508));
#132401=CARTESIAN_POINT('Ctrl Pts',(7.11302459056408,4.03829399962612,-1.40289959501017));
#132402=CARTESIAN_POINT('Ctrl Pts',(7.49144277026395,4.173681702,-0.368991814859853));
#132403=CARTESIAN_POINT('Ctrl Pts',(7.47133485840943,4.108088716,-0.777231965446189));
#132404=CARTESIAN_POINT('Ctrl Pts',(7.40698431742471,4.042807359,-1.18086962076656));
#132405=CARTESIAN_POINT('Ctrl Pts',(7.40475981466687,4.0405506793131,-1.19482277584016));
#132406=CARTESIAN_POINT('Ctrl Pts',(7.40253531190902,4.03829399962611,-1.20877593091373));
#132407=CARTESIAN_POINT('',(7.22520254318857,4.17289951177379,-0.599122887178798));
#132408=CARTESIAN_POINT('Origin',(-0.198275918900978,4.16071258780606,0.0184535848791907));
#132409=CARTESIAN_POINT('Ctrl Pts',(7.47441192954827,4.13354310003169,-0.619004280640486));
#132410=CARTESIAN_POINT('Ctrl Pts',(7.432840571704,4.13979627447792,-0.615647408031067));
#132411=CARTESIAN_POINT('Ctrl Pts',(7.3912671063394,4.14619777523392,-0.612309239198264));
#132412=CARTESIAN_POINT('Ctrl Pts',(7.30821076097249,4.15930620204402,-0.60568176445075));
#132413=CARTESIAN_POINT('Ctrl Pts',(7.26668168060823,4.16602041376777,-0.602388768625244));
#132414=CARTESIAN_POINT('Ctrl Pts',(7.22520254895009,4.17289950623539,-0.599122802339564));
#132415=CARTESIAN_POINT('Ctrl Pts',(7.24508404466,4.042807359,0.18869092816));
#132416=CARTESIAN_POINT('Ctrl Pts',(7.25538543020001,4.108510123,-0.20684689829));
#132417=CARTESIAN_POINT('Ctrl Pts',(7.22256597768,4.173674111,-0.601155374030001));
#132418=CARTESIAN_POINT('Ctrl Pts',(7.247606092,4.042807359,0.186295287));
#132419=CARTESIAN_POINT('Ctrl Pts',(7.25777669,4.108510123,-0.209380228));
#132420=CARTESIAN_POINT('Ctrl Pts',(7.22481223800001,4.173674111,-0.603811336000001));
#132421=CARTESIAN_POINT('Ctrl Pts',(7.49981082600001,4.042807359,-0.053268829));
#132422=CARTESIAN_POINT('Ctrl Pts',(7.49690267000001,4.108510123,-0.462713199));
#132423=CARTESIAN_POINT('Ctrl Pts',(7.44943827000001,4.173674111,-0.869407533));
#132424=CARTESIAN_POINT('Origin',(-0.197818151014114,4.01786906839711,-0.00926186170131144));
#132425=CARTESIAN_POINT('Ctrl Pts',(7.1844444,4.173681702,0.972758276));
#132426=CARTESIAN_POINT('Ctrl Pts',(7.23745408,4.108088716,0.581247754));
#132427=CARTESIAN_POINT('Ctrl Pts',(7.247606092,4.042807359,0.186295287));
#132428=CARTESIAN_POINT('Ctrl Pts',(7.24795703198754,4.04055067937703,0.172642366391681));
#132429=CARTESIAN_POINT('Ctrl Pts',(7.24830797197519,4.038293999754,0.158989445783361));
#132430=CARTESIAN_POINT('Ctrl Pts',(7.39561933502162,4.173681702,1.25007375973637));
#132431=CARTESIAN_POINT('Ctrl Pts',(7.46374109865901,4.108088716,0.847055430001624));
#132432=CARTESIAN_POINT('Ctrl Pts',(7.48766520227535,4.042807359,0.439021134686341));
#132433=CARTESIAN_POINT('Ctrl Pts',(7.48849222302995,4.04055067937703,0.424915994688794));
#132434=CARTESIAN_POINT('Ctrl Pts',(7.48931924378469,4.038293999754,0.410810854691255));
#132435=CARTESIAN_POINT('',(7.18507502384416,4.17289950633231,0.968089322403721));
#132436=CARTESIAN_POINT('Origin',(-0.197607384198897,4.16071259388392,-0.0246013163387804));
#132437=CARTESIAN_POINT('Ctrl Pts',(7.4327319551077,4.13354309998286,1.00224531859311));
#132438=CARTESIAN_POINT('Ctrl Pts',(7.39141088416451,4.13979627442906,0.996587096134489));
#132439=CARTESIAN_POINT('Ctrl Pts',(7.35009177569022,4.14619777518784,0.990910154106153));
#132440=CARTESIAN_POINT('Ctrl Pts',(7.2675525304276,4.15930620198021,0.979528022672306));
#132441=CARTESIAN_POINT('Ctrl Pts',(7.22628648180661,4.16602041341854,0.973816505420604));
#132442=CARTESIAN_POINT('Ctrl Pts',(7.18507502301303,4.17289950585988,0.968089327816833));
#132443=CARTESIAN_POINT('Ctrl Pts',(7.03513503368,4.042807359,1.74175834578));
#132444=CARTESIAN_POINT('Ctrl Pts',(7.13022451851,4.108510123,1.3576824667));
#132445=CARTESIAN_POINT('Ctrl Pts',(7.18293703368,4.173674111,0.965537491470001));
#132446=CARTESIAN_POINT('Ctrl Pts',(7.038113109,4.042807359,1.739960879));
#132447=CARTESIAN_POINT('Ctrl Pts',(7.133104463,4.108510123,1.355722415));
#132448=CARTESIAN_POINT('Ctrl Pts',(7.18570173100001,4.173674111,0.963426504000001));
#132449=CARTESIAN_POINT('Ctrl Pts',(7.335920641,4.042807359,1.560214201));
#132450=CARTESIAN_POINT('Ctrl Pts',(7.421098912,4.108510123,1.159717245));
#132451=CARTESIAN_POINT('Ctrl Pts',(7.462171463,4.173674111,0.752327757));
#132452=CARTESIAN_POINT('Origin',(-0.191202134330626,4.01786908337155,-0.0515703590211958));
#132453=CARTESIAN_POINT('Ctrl Pts',(6.807361808,4.173681702,2.494458903));
#132454=CARTESIAN_POINT('Ctrl Pts',(6.94329534,4.108088716,2.123497195));
#132455=CARTESIAN_POINT('Ctrl Pts',(7.038113109,4.042807359,1.739960879));
#132456=CARTESIAN_POINT('Ctrl Pts',(7.04139081861473,4.04055067933166,1.72670259752172));
#132457=CARTESIAN_POINT('Ctrl Pts',(7.04466852822935,4.03829399966326,1.71344431604344));
#132458=CARTESIAN_POINT('Ctrl Pts',(6.95398495829392,4.173681702,2.81068727388919));
#132459=CARTESIAN_POINT('Ctrl Pts',(7.10715110139243,4.108088716,2.43173545453254));
#132460=CARTESIAN_POINT('Ctrl Pts',(7.21823118476982,4.042807359,2.03838374951113));
#132461=CARTESIAN_POINT('Ctrl Pts',(7.22207105846783,4.04055067933166,2.02478616459523));
#132462=CARTESIAN_POINT('Ctrl Pts',(7.22591093216596,4.03829399966326,2.01118857967941));
#132463=CARTESIAN_POINT('',(6.80898137486375,4.1728995063478,2.49003467242114));
#132464=CARTESIAN_POINT('Origin',(-0.187698734055647,4.16071265495012,-0.0665058597055171));
#132465=CARTESIAN_POINT('Ctrl Pts',(7.04350569533256,4.13354309996481,2.57663104013005));
#132466=CARTESIAN_POINT('Ctrl Pts',(7.00436703867137,4.13979627440061,2.56222229503698));
#132467=CARTESIAN_POINT('Ctrl Pts',(6.96523432263822,4.1461977751729,2.54779568983075));
#132468=CARTESIAN_POINT('Ctrl Pts',(6.88707162095704,4.15930620196764,2.51893616842301));
#132469=CARTESIAN_POINT('Ctrl Pts',(6.8479981567205,4.16602041347153,2.50448720246409));
#132470=CARTESIAN_POINT('Ctrl Pts',(6.8089813728981,4.17289950593006,2.49003467752891));
#132471=CARTESIAN_POINT('Ctrl Pts',(6.49623092821,4.042807359,3.21338307884));
#132472=CARTESIAN_POINT('Ctrl Pts',(6.67166223484,4.108510123,2.85872810885));
#132473=CARTESIAN_POINT('Ctrl Pts',(6.80744193786,4.173674111,2.48708289756));
#132474=CARTESIAN_POINT('Ctrl Pts',(6.49952578,4.042807359,3.212267834));
#132475=CARTESIAN_POINT('Ctrl Pts',(6.674896201,4.108510123,2.857432985));
#132476=CARTESIAN_POINT('Ctrl Pts',(6.810595798,4.173674111,2.485615592));
#132477=CARTESIAN_POINT('Ctrl Pts',(6.829010959,4.042807359,3.10074335));
#132478=CARTESIAN_POINT('Ctrl Pts',(6.998292817,4.108510123,2.7279206));
#132479=CARTESIAN_POINT('Ctrl Pts',(7.125981812,4.173674111,2.338885036));
#132480=CARTESIAN_POINT('Origin',(-0.175646128157292,4.01786907295784,-0.0914676050620089));
#132481=CARTESIAN_POINT('Ctrl Pts',(6.111974543,4.173681702,3.899521405));
#132482=CARTESIAN_POINT('Ctrl Pts',(6.324475827,4.108088716,3.566454266));
#132483=CARTESIAN_POINT('Ctrl Pts',(6.49952578,4.042807359,3.212267834));
#132484=CARTESIAN_POINT('Ctrl Pts',(6.5055769970589,4.04055067938178,3.20002413474375));
#132485=CARTESIAN_POINT('Ctrl Pts',(6.51162821411791,4.0382939997635,3.18778043548744));
#132486=CARTESIAN_POINT('Ctrl Pts',(6.18718997383367,4.173681702,4.23987617474425));
#132487=CARTESIAN_POINT('Ctrl Pts',(6.41823861690002,4.108088716,3.90271023113911));
#132488=CARTESIAN_POINT('Ctrl Pts',(6.61128069909999,4.042807359,3.54243380476379));
#132489=CARTESIAN_POINT('Ctrl Pts',(6.61795387736068,4.04055067938178,3.529979583441));
#132490=CARTESIAN_POINT('Ctrl Pts',(6.62462705562136,4.0382939997635,3.51752536211824));
#132491=CARTESIAN_POINT('',(6.11450736626476,4.17289951176952,3.89554870260983));
#132492=CARTESIAN_POINT('Origin',(-0.169013702511757,4.16071260599231,-0.105300696633516));
#132493=CARTESIAN_POINT('Ctrl Pts',(6.32493293725509,4.13354310001343,4.030536358256));
#132494=CARTESIAN_POINT('Ctrl Pts',(6.28980677482503,4.13979627446321,4.00805082736618));
#132495=CARTESIAN_POINT('Ctrl Pts',(6.25469025369967,4.14619777521526,3.98554913111775));
#132496=CARTESIAN_POINT('Ctrl Pts',(6.18455889639565,4.1593062020154,3.94056165900709));
#132497=CARTESIAN_POINT('Ctrl Pts',(6.14950504726379,4.16602041375794,3.91805086130808));
#132498=CARTESIAN_POINT('Ctrl Pts',(6.11450731972724,4.17289950620169,3.89554877328798));
#132499=CARTESIAN_POINT('Ctrl Pts',(5.65357028333,4.042807359,4.53475359029));
#132500=CARTESIAN_POINT('Ctrl Pts',(5.90114043883001,4.108510123,4.22610280245));
#132501=CARTESIAN_POINT('Ctrl Pts',(6.11363842303001,4.173674111,3.89233507207));
#132502=CARTESIAN_POINT('Ctrl Pts',(5.657027848,4.042807359,4.534372715));
#132503=CARTESIAN_POINT('Ctrl Pts',(5.90457721,4.108510123,4.225533165));
#132504=CARTESIAN_POINT('Ctrl Pts',(6.117033975,4.173674111,3.891580058));
#132505=CARTESIAN_POINT('Ctrl Pts',(6.002784315,4.042807359,4.496285186));
#132506=CARTESIAN_POINT('Ctrl Pts',(6.24825432699999,4.108510123,4.16856942));
#132507=CARTESIAN_POINT('Ctrl Pts',(6.45658917200001,4.173674111,3.816078651));
#132508=CARTESIAN_POINT('Origin',(-0.151876743933352,4.01786908548743,-0.127087835198143));
#132509=CARTESIAN_POINT('Ctrl Pts',(5.13079814199999,4.173681702,5.122246619));
#132510=CARTESIAN_POINT('Ctrl Pts',(5.409930853,4.108088716,4.8426479));
#132511=CARTESIAN_POINT('Ctrl Pts',(5.657027848,4.042807359,4.534372715));
#132512=CARTESIAN_POINT('Ctrl Pts',(5.66556962431573,4.04055067939498,4.52371609947151));
#132513=CARTESIAN_POINT('Ctrl Pts',(5.67411140063149,4.03829399978988,4.51305948394299));
#132514=CARTESIAN_POINT('Ctrl Pts',(5.13108886245636,4.173681702,5.47081317818954));
#132515=CARTESIAN_POINT('Ctrl Pts',(5.42921642824447,4.108088716,5.19119861552039));
#132516=CARTESIAN_POINT('Ctrl Pts',(5.69519407555069,4.042807359,4.88084359396338));
#132517=CARTESIAN_POINT('Ctrl Pts',(5.70438852798938,4.04055067939498,4.87011508157252));
#132518=CARTESIAN_POINT('Ctrl Pts',(5.71358298042812,4.03829399978988,4.85938656918154));
#132519=CARTESIAN_POINT('',(5.13412576263134,4.17289951176391,5.11891127869527));
#132520=CARTESIAN_POINT('Origin',(-0.142425679370615,4.16071261417797,-0.139171734135627));
#132521=CARTESIAN_POINT('Ctrl Pts',(5.31061334460018,4.13354310000474,5.29597827577731));
#132522=CARTESIAN_POINT('Ctrl Pts',(5.28114213686151,4.13979627444847,5.26646735746395));
#132523=CARTESIAN_POINT('Ctrl Pts',(5.25168382007216,4.1461977752049,5.23694272427037));
#132524=CARTESIAN_POINT('Ctrl Pts',(5.19286307176349,4.15930620201472,5.17793086538721));
#132525=CARTESIAN_POINT('Ctrl Pts',(5.16346791838434,4.16602041375355,5.14841081626259));
#132526=CARTESIAN_POINT('Ctrl Pts',(5.13412570209188,4.17289950622626,5.11891133762066));
#132527=CARTESIAN_POINT('Ctrl Pts',(4.54655497634,4.042807359,5.64408406444999));
#132528=CARTESIAN_POINT('Ctrl Pts',(4.85468787541999,4.108510123,5.39586962442));
#132529=CARTESIAN_POINT('Ctrl Pts',(5.13396797045,4.173674111,5.11558598396));
#132530=CARTESIAN_POINT('Ctrl Pts',(4.550013582,4.042807359,5.644455368));
#132531=CARTESIAN_POINT('Ctrl Pts',(4.858166752,4.108510123,5.396052109));
#132532=CARTESIAN_POINT('Ctrl Pts',(5.137446442,4.173674111,5.115578565));
#132533=CARTESIAN_POINT('Ctrl Pts',(4.895874148,4.042807359,5.681585723));
#132534=CARTESIAN_POINT('Ctrl Pts',(5.20605441,4.108510123,5.414300567));
#132535=CARTESIAN_POINT('Ctrl Pts',(5.485293597,4.173674111,5.114836669));
#132536=CARTESIAN_POINT('Origin',(-0.121005699289965,4.01786904130105,-0.156765469005895));
#132537=CARTESIAN_POINT('Ctrl Pts',(3.909711322,4.173681702,6.105461275));
#132538=CARTESIAN_POINT('Ctrl Pts',(4.242423525,4.108088716,5.89240469999999));
#132539=CARTESIAN_POINT('Ctrl Pts',(4.550013582,4.042807359,5.644455368));
#132540=CARTESIAN_POINT('Ctrl Pts',(4.56064651363442,4.04055067940265,5.63588412768856));
#132541=CARTESIAN_POINT('Ctrl Pts',(4.57127944526878,4.03829399980524,5.62731288737714));
#132542=CARTESIAN_POINT('Ctrl Pts',(3.83506373905209,4.173681702,6.4459410374688));
#132543=CARTESIAN_POINT('Ctrl Pts',(4.18633011316431,4.108088716,6.23695232226666));
#132544=CARTESIAN_POINT('Ctrl Pts',(4.51280650719211,4.042807359,5.99103056005124));
#132545=CARTESIAN_POINT('Ctrl Pts',(4.52409231145965,4.04055067940265,5.98252940981719));
#132546=CARTESIAN_POINT('Ctrl Pts',(4.53537811572727,4.03829399980525,5.97402825958322));
#132547=CARTESIAN_POINT('',(3.91367807798151,4.17289950635246,6.10291929574919));
#132548=CARTESIAN_POINT('Origin',(-0.10917812640765,4.16071260748246,-0.166535413895311));
#132549=CARTESIAN_POINT('Ctrl Pts',(4.04797537441707,4.13354309997486,6.31378613519414));
#132550=CARTESIAN_POINT('Ctrl Pts',(4.02553716221962,4.13979627442888,6.27862972721912));
#132551=CARTESIAN_POINT('Ctrl Pts',(4.00311448798317,4.14619777516769,6.24346269633418));
#132552=CARTESIAN_POINT('Ctrl Pts',(3.95835474138069,4.15930620198404,6.1731857797458));
#132553=CARTESIAN_POINT('Ctrl Pts',(3.93599276900521,4.16602041351721,6.13803680496813));
#132554=CARTESIAN_POINT('Ctrl Pts',(3.91367807337261,4.17289950597883,6.10291929860463));
#132555=CARTESIAN_POINT('Ctrl Pts',(3.22694781191,4.042807359,6.48950344034));
#132556=CARTESIAN_POINT('Ctrl Pts',(3.5812355014,4.108510123,6.31333158117999));
#132557=CARTESIAN_POINT('Ctrl Pts',(3.91423888132,4.173674111,6.09963778095));
#132558=CARTESIAN_POINT('Ctrl Pts',(3.230245738,4.042807359,6.490609561));
#132559=CARTESIAN_POINT('Ctrl Pts',(3.584593815,4.108510123,6.314257655));
#132560=CARTESIAN_POINT('Ctrl Pts',(3.917637623,4.173674111,6.100378304));
#132561=CARTESIAN_POINT('Ctrl Pts',(3.560038347,4.042807359,6.601221627));
#132562=CARTESIAN_POINT('Ctrl Pts',(3.920425175,4.108510123,6.406865037));
#132563=CARTESIAN_POINT('Ctrl Pts',(4.25751179100001,4.173674111,6.174430609));
#132564=CARTESIAN_POINT('Origin',(-0.0844766574966155,4.01786906872095,
-0.179112931320975));
#132565=CARTESIAN_POINT('Ctrl Pts',(2.505810746,4.173681702,6.803191347));
#132566=CARTESIAN_POINT('Ctrl Pts',(2.876545188,4.108088716,6.66663920500001));
#132567=CARTESIAN_POINT('Ctrl Pts',(3.230245738,4.042807359,6.490609561));
#132568=CARTESIAN_POINT('Ctrl Pts',(3.2424726411516,4.04055067936057,6.48452447742013));
#132569=CARTESIAN_POINT('Ctrl Pts',(3.25469954430317,4.03829399972108,6.47843939384023));
#132570=CARTESIAN_POINT('Ctrl Pts',(2.35971529781498,4.173681702,7.11966385829063));
#132571=CARTESIAN_POINT('Ctrl Pts',(2.74769565534635,4.108088716,6.99107307035044));
#132572=CARTESIAN_POINT('Ctrl Pts',(3.11940512216221,4.042807359,6.82108359598885));
#132573=CARTESIAN_POINT('Ctrl Pts',(3.13225456684441,4.04055067936057,6.81520731211027));
#132574=CARTESIAN_POINT('Ctrl Pts',(3.14510401152666,4.03829399972108,6.80933102823169));
#132575=CARTESIAN_POINT('',(2.51023128580415,4.1728995117299,6.80156150582057));
#132576=CARTESIAN_POINT('Origin',(-0.0708253644546503,4.16071265875346,
-0.186111902591437));
#132577=CARTESIAN_POINT('Ctrl Pts',(2.59605857474129,4.13354310001904,7.03636837218138));
#132578=CARTESIAN_POINT('Ctrl Pts',(2.58170254394118,4.13979627446724,6.99721034916009));
#132579=CARTESIAN_POINT('Ctrl Pts',(2.56736397139921,4.14619777521901,6.95804529166872));
#132580=CARTESIAN_POINT('Ctrl Pts',(2.53875814241895,4.15930620203028,6.87978938791505));
#132581=CARTESIAN_POINT('Ctrl Pts',(2.52447497067071,4.16602041375511,6.84065501247579));
#132582=CARTESIAN_POINT('Ctrl Pts',(2.51023120599506,4.1728995062256,6.80156153393056));
#132583=CARTESIAN_POINT('Ctrl Pts',(1.75645215384,4.042807359,7.03148084821));
#132584=CARTESIAN_POINT('Ctrl Pts',(2.14032853641,4.108510123,6.93558916912));
#132585=CARTESIAN_POINT('Ctrl Pts',(2.51148433258,4.173674111,6.79847729497001));
#132586=CARTESIAN_POINT('Ctrl Pts',(1.759435193,4.042807359,7.033270065));
#132587=CARTESIAN_POINT('Ctrl Pts',(2.143409256,4.108510123,6.93721553));
#132588=CARTESIAN_POINT('Ctrl Pts',(2.514644423,4.173674111,6.79993113400001));
#132589=CARTESIAN_POINT('Ctrl Pts',(2.057739109,4.042807359,7.212191744));
#132590=CARTESIAN_POINT('Ctrl Pts',(2.451481215,4.108510123,7.099851618));
#132591=CARTESIAN_POINT('Ctrl Pts',(2.830653465,4.173674111,6.945315037));
#132592=CARTESIAN_POINT('Origin',(-0.0439977612037606,4.01786909908604,
-0.193085675719032));
#132593=CARTESIAN_POINT('Ctrl Pts',(0.984741244,4.173681702,7.182811753));
#132594=CARTESIAN_POINT('Ctrl Pts',(1.376162796,4.108088716,7.129149071));
#132595=CARTESIAN_POINT('Ctrl Pts',(1.759435193,4.042807359,7.033270065));
#132596=CARTESIAN_POINT('Ctrl Pts',(1.77268435110923,4.04055067934542,7.02995567001672));
#132597=CARTESIAN_POINT('Ctrl Pts',(1.78593350921839,4.03829399969076,7.02664127503343));
#132598=CARTESIAN_POINT('Ctrl Pts',(0.77402919142123,4.173681702,7.4604791102965));
#132599=CARTESIAN_POINT('Ctrl Pts',(1.18058200259842,4.108088716,7.41829901202046));
#132600=CARTESIAN_POINT('Ctrl Pts',(1.5801438198671,4.042807359,7.3321903451503));
#132601=CARTESIAN_POINT('Ctrl Pts',(1.59395607906664,4.04055067934542,7.32921369629466));
#132602=CARTESIAN_POINT('Ctrl Pts',(1.60776833826625,4.03829399969076,7.32623704743884));
#132603=CARTESIAN_POINT('',(0.989408801939575,4.17289951177892,7.18217030221119));
#132604=CARTESIAN_POINT('Origin',(-0.0291609472063403,4.16071258635768,
-0.196986017737631));
#132605=CARTESIAN_POINT('Ctrl Pts',(1.02275296161709,4.13354310000798,7.42993784453988));
#132606=CARTESIAN_POINT('Ctrl Pts',(1.01715038425056,4.13979627445525,7.3886091920938));
#132607=CARTESIAN_POINT('Ctrl Pts',(1.01156636914356,4.14619777522442,7.34727742251048));
#132608=CARTESIAN_POINT('Ctrl Pts',(1.00045203447617,4.1593062020231,7.26470169062957));
#132609=CARTESIAN_POINT('Ctrl Pts',(0.994915529196611,4.1660204137004,7.22341179562296));
#132610=CARTESIAN_POINT('Ctrl Pts',(0.989408718002346,4.17289950615059,
7.18217031248019));
#132611=CARTESIAN_POINT('Ctrl Pts',(0.20382674536,4.042807359,7.24467402586));
#132612=CARTESIAN_POINT('Ctrl Pts',(0.59934218743,4.108510123,7.23354631689));
#132613=CARTESIAN_POINT('Ctrl Pts',(0.991295567150001,4.173674111,7.17942756589));
#132614=CARTESIAN_POINT('Ctrl Pts',(0.206355414,4.042807359,7.247062677));
#132615=CARTESIAN_POINT('Ctrl Pts',(0.602001262,4.108510123,7.235796918));
#132616=CARTESIAN_POINT('Ctrl Pts',(0.994069244,4.173674111,7.181526741));
#132617=CARTESIAN_POINT('Ctrl Pts',(0.459222278,4.042807359,7.485927791));
#132618=CARTESIAN_POINT('Ctrl Pts',(0.867908719,4.108510123,7.460857029));
#132619=CARTESIAN_POINT('Ctrl Pts',(1.271436929,4.173674111,7.39144425200001));
#132620=CARTESIAN_POINT('Origin',(-0.00146140008758431,4.01786907736225,
-0.19802964222655));
#132621=CARTESIAN_POINT('Ctrl Pts',(-0.579724377070001,4.173681702,7.22431773469001));
#132622=CARTESIAN_POINT('Ctrl Pts',(-0.18604099109,4.108088716,7.25590934798001));
#132623=CARTESIAN_POINT('Ctrl Pts',(0.20874406514,4.042807359,7.24453400836));
#132624=CARTESIAN_POINT('Ctrl Pts',(0.222391198647374,4.04055067937027,
7.2441407797511));
#132625=CARTESIAN_POINT('Ctrl Pts',(0.236038332154748,4.03829399974047,
7.24374755114209));
#132626=CARTESIAN_POINT('Ctrl Pts',(-0.582373663,4.173681702,7.22657186500001));
#132627=CARTESIAN_POINT('Ctrl Pts',(-0.18856744,4.108088716,7.25830784900001));
#132628=CARTESIAN_POINT('Ctrl Pts',(0.206355414,4.042807359,7.247062677));
#132629=CARTESIAN_POINT('Ctrl Pts',(0.220007310971782,4.04055067937027,
7.24667394809255));
#132630=CARTESIAN_POINT('Ctrl Pts',(0.233659207943565,4.03829399974047,
7.24628521918494));
#132631=CARTESIAN_POINT('Ctrl Pts',(-0.847849659089798,4.173681702,7.45245065089739));
#132632=CARTESIAN_POINT('Ctrl Pts',(-0.441734353150908,4.108088716,7.49865353618934));
#132633=CARTESIAN_POINT('Ctrl Pts',(-0.0330032499787613,4.042807359,7.50045202179791));
#132634=CARTESIAN_POINT('Ctrl Pts',(-0.0188740223254308,4.04055067937027,
7.50051419277634));
#132635=CARTESIAN_POINT('Ctrl Pts',(-0.00474479467210093,4.03829399974047,
7.50057636375477));
#132636=CARTESIAN_POINT('Origin',(0.0138668838850882,4.16071273333814,-0.198651015243198));
#132637=CARTESIAN_POINT('Ctrl Pts',(0.213507122,1.715323387,7.246855505));
#132638=CARTESIAN_POINT('Ctrl Pts',(0.605805226,1.779910221,7.235297604));
#132639=CARTESIAN_POINT('Ctrl Pts',(0.994563149000001,1.845052736,7.181458358));
#132640=CARTESIAN_POINT('Ctrl Pts',(0.466609588000001,1.715323387,7.48547096));
#132641=CARTESIAN_POINT('Ctrl Pts',(0.871824797,1.779910221,7.460211721));
#132642=CARTESIAN_POINT('Ctrl Pts',(1.27194527,1.845052736,7.391356792));
#132643=CARTESIAN_POINT('',(0.466609584806905,1.71532338744763,7.48547096129464));
#132644=CARTESIAN_POINT('',(1.0255415441568,1.80506741731045,7.42955345467621));
#132645=CARTESIAN_POINT('Origin',(-0.0371219255234506,1.87497458960283,
-0.186844580707713));
#132646=CARTESIAN_POINT('Ctrl Pts',(0.989922562716042,1.84427517372254,
7.18209950661362));
#132647=CARTESIAN_POINT('Ctrl Pts',(0.995813103391253,1.83740483626466,
7.22328556358072));
#132648=CARTESIAN_POINT('Ctrl Pts',(1.00173105596826,1.83070797850139,7.26452308862856));
#132649=CARTESIAN_POINT('Ctrl Pts',(1.01360302452397,1.81765000112593,7.34699349044738));
#132650=CARTESIAN_POINT('Ctrl Pts',(1.01956408258325,1.81128114572236,7.38827527131803));
#132651=CARTESIAN_POINT('Ctrl Pts',(1.02554154127133,1.8050674173951,7.4295534551068));
#132652=CARTESIAN_POINT('',(0.340058346905326,1.71532338829773,7.36616323287369));
#132653=CARTESIAN_POINT('Origin',(-6.84673671924596E-14,1.80614392400061,
1.4658413372004E-13));
#132654=CARTESIAN_POINT('',(1.0294825429089,1.6256495872185,7.42900839215824));
#132655=CARTESIAN_POINT('Origin',(-0.0480202436087657,1.48225709598333,
-0.179766005105065));
#132656=CARTESIAN_POINT('',(1.58774795233212,1.71532338734617,7.33001067177152));
#132657=CARTESIAN_POINT('Origin',(-0.0635989656301628,1.87485301774001,
-0.1735270144933));
#132658=CARTESIAN_POINT('Ctrl Pts',(1.0255415464473,1.80506741659162,7.42955345421685));
#132659=CARTESIAN_POINT('Ctrl Pts',(1.14143634970523,1.78658581162503,7.41355586629499));
#132660=CARTESIAN_POINT('Ctrl Pts',(1.25671458271972,1.76822051520836,7.39487847462538));
#132661=CARTESIAN_POINT('Ctrl Pts',(1.37119593248245,1.74999999995591,7.37358947262711));
#132662=CARTESIAN_POINT('Ctrl Pts',(1.44347393988503,1.73849644457293,7.36014862272757));
#132663=CARTESIAN_POINT('Ctrl Pts',(1.51567409001699,1.72693520694185,7.34562253447594));
#132664=CARTESIAN_POINT('Ctrl Pts',(1.58774795046836,1.71532338729505,7.33001067089588));
#132665=CARTESIAN_POINT('Ctrl Pts',(0.9851997,1.845058467,7.182748885));
#132666=CARTESIAN_POINT('Ctrl Pts',(1.273922751,1.797173233,7.143147075));
#132667=CARTESIAN_POINT('Ctrl Pts',(1.558535692,1.75,7.080499029));
#132668=CARTESIAN_POINT('Ctrl Pts',(1.662816028,1.732716033,7.057545191));
#132669=CARTESIAN_POINT('Ctrl Pts',(1.766375162,1.715323387,7.03153033));
#132670=CARTESIAN_POINT('Ctrl Pts',(0.774939815000001,1.845058467,7.459857122));
#132671=CARTESIAN_POINT('Ctrl Pts',(1.074801713,1.797173233,7.428707072));
#132672=CARTESIAN_POINT('Ctrl Pts',(1.371195932,1.75,7.373589473));
#132673=CARTESIAN_POINT('Ctrl Pts',(1.479792853,1.732716033,7.353394742));
#132674=CARTESIAN_POINT('Ctrl Pts',(1.587747952,1.715323387,7.330010671));
#132675=CARTESIAN_POINT('',(1.67706156174498,1.71532338778839,7.18077049939182));
#132676=CARTESIAN_POINT('Ctrl Pts',(1.766375162,1.715323387,7.03153033));
#132677=CARTESIAN_POINT('Ctrl Pts',(2.147016947,1.779910221,6.935910151));
#132678=CARTESIAN_POINT('Ctrl Pts',(2.51511208,1.845052736,6.799758174));
#132679=CARTESIAN_POINT('Ctrl Pts',(2.064855503,1.715323387,7.21015754));
#132680=CARTESIAN_POINT('Ctrl Pts',(2.455167015,1.779910221,7.098379556));
#132681=CARTESIAN_POINT('Ctrl Pts',(2.83113112,1.845052736,6.945120343));
#132682=CARTESIAN_POINT('',(2.06485550015272,1.71532338744839,7.21015754195452));
#132683=CARTESIAN_POINT('',(2.59869932952182,1.80506741729831,7.03539350645313));
#132684=CARTESIAN_POINT('Origin',(-0.0764201321297411,1.87497455512894,
-0.174496271270764));
#132685=CARTESIAN_POINT('Ctrl Pts',(2.51071781620877,1.84427517367611,6.80138192209821));
#132686=CARTESIAN_POINT('Ctrl Pts',(2.52532442072709,1.83740483780848,6.84033877097677));
#132687=CARTESIAN_POINT('Ctrl Pts',(2.53996885979272,1.83070798172457,6.8793399903243));
#132688=CARTESIAN_POINT('Ctrl Pts',(2.56929197405064,1.81765000114506,6.95733017689152));
#132689=CARTESIAN_POINT('Ctrl Pts',(2.58398802854539,1.81128114570797,6.99636536159158));
#132690=CARTESIAN_POINT('Ctrl Pts',(2.59869932691265,1.80506741737884,7.03539350744946));
#132691=CARTESIAN_POINT('',(1.9156153246616,1.71532338829994,7.12084393710865));
#132692=CARTESIAN_POINT('Origin',(2.94902990916057E-14,1.806143924,1.23165366794353E-13));
#132693=CARTESIAN_POINT('',(2.60243101765133,1.62564958721911,7.0340139887338));
#132694=CARTESIAN_POINT('Origin',(-0.085541867002264,1.48225708216688,-0.165240028068662));
#132695=CARTESIAN_POINT('',(3.12636290849826,1.7153233873471,6.81732021967138));
#132696=CARTESIAN_POINT('Origin',(-0.0994150821221096,1.87485304671307,
-0.155797783110659));
#132697=CARTESIAN_POINT('Ctrl Pts',(2.59869933156525,1.80506741660997,7.03539350555662));
#132698=CARTESIAN_POINT('Ctrl Pts',(2.70844556999549,1.78658581162499,6.99485597570313));
#132699=CARTESIAN_POINT('Ctrl Pts',(2.81701357488237,1.76822051520318,6.95183383867207));
#132700=CARTESIAN_POINT('Ctrl Pts',(2.92424190825311,1.75000000000266,6.90643245527506));
#132701=CARTESIAN_POINT('Ctrl Pts',(2.99194071041716,1.73849644464936,6.8777682092977));
#132702=CARTESIAN_POINT('Ctrl Pts',(3.05933018184855,1.72693520694185,6.8480608352413));
#132703=CARTESIAN_POINT('Ctrl Pts',(3.12636290648176,1.71532338729505,6.8173202192276));
#132704=CARTESIAN_POINT('Ctrl Pts',(2.506244968,1.845058467,6.803031395));
#132705=CARTESIAN_POINT('Ctrl Pts',(2.779704616,1.797173233,6.702288531));
#132706=CARTESIAN_POINT('Ctrl Pts',(3.044195986,1.75,6.579921793));
#132707=CARTESIAN_POINT('Ctrl Pts',(3.14110391,1.732716033,6.535087413));
#132708=CARTESIAN_POINT('Ctrl Pts',(3.236649463,1.715323387,6.487418613));
#132709=CARTESIAN_POINT('Ctrl Pts',(2.360470923,1.845058467,7.118860655));
#132710=CARTESIAN_POINT('Ctrl Pts',(2.646625875,1.797173233,7.023977432));
#132711=CARTESIAN_POINT('Ctrl Pts',(2.924241908,1.75,6.906432456));
#132712=CARTESIAN_POINT('Ctrl Pts',(3.025958623,1.732716033,6.863364738));
#132713=CARTESIAN_POINT('Ctrl Pts',(3.126362908,1.715323387,6.817320219));
#132714=CARTESIAN_POINT('',(3.18150618989582,1.71532338778839,6.6523694138977));
#132715=CARTESIAN_POINT('Ctrl Pts',(3.236649463,1.715323387,6.487418613));
#132716=CARTESIAN_POINT('Ctrl Pts',(3.587836542,1.779910221,6.312207247));
#132717=CARTESIAN_POINT('Ctrl Pts',(3.918057165,1.845052736,6.100108856));
#132718=CARTESIAN_POINT('Ctrl Pts',(3.566551069,1.715323387,6.597705167));
#132719=CARTESIAN_POINT('Ctrl Pts',(3.923708353,1.779910221,6.40463505300001));
#132720=CARTESIAN_POINT('Ctrl Pts',(4.257936425,1.845052736,6.174137786));
#132721=CARTESIAN_POINT('',(3.56655106664231,1.7153233874486,6.59770516952165));
#132722=CARTESIAN_POINT('',(4.0503448225298,1.80506741733711,6.31226637702187));
#132723=CARTESIAN_POINT('Origin',(-0.112144917130483,1.87497457603044,-0.153988411054592));
#132724=CARTESIAN_POINT('Ctrl Pts',(3.91411469427357,1.84427517371797,6.10263927834585));
#132725=CARTESIAN_POINT('Ctrl Pts',(3.93675437769205,1.83740483719272,6.13754535275076));
#132726=CARTESIAN_POINT('Ctrl Pts',(3.95944054978277,1.83070798041905,6.17248662756391));
#132727=CARTESIAN_POINT('Ctrl Pts',(4.00484368626686,1.81765000114176,6.24234983715179));
#132728=CARTESIAN_POINT('Ctrl Pts',(4.02758756590525,1.81128114575264,6.2773131833951));
#132729=CARTESIAN_POINT('Ctrl Pts',(4.05034482005215,1.80506741742345,6.31226637865036));
#132730=CARTESIAN_POINT('',(3.40160025879484,1.71532338830053,6.5425618937461));
#132731=CARTESIAN_POINT('Origin',(7.93635990259389E-13,1.80614392399917,
1.20693385841086E-12));
#132732=CARTESIAN_POINT('',(4.0536927102926,1.62564958721554,6.31011690930612));
#132733=CARTESIAN_POINT('Origin',(-0.119063806186307,1.48225703862391,-0.142988065447516));
#132734=CARTESIAN_POINT('',(4.51879260962798,1.7153233873466,5.98585945055491));
#132735=CARTESIAN_POINT('Origin',(-0.130582748919531,1.87485301701732,-0.130784038236786));
#132736=CARTESIAN_POINT('Ctrl Pts',(4.05034482445065,1.80506741660596,6.31226637562157));
#132737=CARTESIAN_POINT('Ctrl Pts',(4.14881088633035,1.78658581163939,6.24908439319196));
#132738=CARTESIAN_POINT('Ctrl Pts',(4.24559214392768,1.76822051521793,6.18372917775308));
#132739=CARTESIAN_POINT('Ctrl Pts',(4.34055358295998,1.75000000001201,6.11633833187862));
#132740=CARTESIAN_POINT('Ctrl Pts',(4.40050765881071,1.73849644466465,6.07379100026899));
#132741=CARTESIAN_POINT('Ctrl Pts',(4.45993539460349,1.72693520694186,6.03029142298064));
#132742=CARTESIAN_POINT('Ctrl Pts',(4.51879260756621,1.71532338729505,5.98585945054844));
#132743=CARTESIAN_POINT('Ctrl Pts',(3.910101007,1.845058467,6.105211717));
#132744=CARTESIAN_POINT('Ctrl Pts',(4.155510583,1.797173233,5.948038425));
#132745=CARTESIAN_POINT('Ctrl Pts',(4.38751306,1.75,5.771674726));
#132746=CARTESIAN_POINT('Ctrl Pts',(4.472517264,1.732716033,5.707056211));
#132747=CARTESIAN_POINT('Ctrl Pts',(4.555581632,1.715323387,5.639962411));
#132748=CARTESIAN_POINT('Ctrl Pts',(3.835629033,1.845058467,6.444994175));
#132749=CARTESIAN_POINT('Ctrl Pts',(4.094696754,1.797173233,6.290814413));
#132750=CARTESIAN_POINT('Ctrl Pts',(4.340553583,1.75,6.116338332));
#132751=CARTESIAN_POINT('Ctrl Pts',(4.430633931,1.732716033,6.052411428));
#132752=CARTESIAN_POINT('Ctrl Pts',(4.518792609,1.715323387,5.98585945));
#132753=CARTESIAN_POINT('',(4.53718712434111,1.71532338778839,5.81291092750188));
#132754=CARTESIAN_POINT('Ctrl Pts',(4.555581632,1.715323387,5.639962411));
#132755=CARTESIAN_POINT('Ctrl Pts',(4.860892888,1.779910221,5.393352549));
#132756=CARTESIAN_POINT('Ctrl Pts',(5.137798252,1.845052736,5.115225227));
#132757=CARTESIAN_POINT('Ctrl Pts',(4.901478671,1.715323387,5.676751433));
#132758=CARTESIAN_POINT('Ctrl Pts',(5.208781448,1.779910221,5.41141693200001));
#132759=CARTESIAN_POINT('Ctrl Pts',(5.485645355,1.845052736,5.11445940800001));
#132760=CARTESIAN_POINT('',(4.90147866925435,1.71532338744861,5.67675143596386));
#132761=CARTESIAN_POINT('',(5.31260069305792,1.80506741735431,5.29398468727746));
#132762=CARTESIAN_POINT('Origin',(-0.142626191119171,1.87497457881845,-0.126280623933815));
#132763=CARTESIAN_POINT('Ctrl Pts',(5.13449192012045,1.84427517373959,5.11854400406275));
#132764=CARTESIAN_POINT('Ctrl Pts',(5.16410607728195,1.83740483654798,5.14776713411668));
#132765=CARTESIAN_POINT('Ctrl Pts',(5.1937732038837,1.83070797905741,5.17701464835099));
#132766=CARTESIAN_POINT('Ctrl Pts',(5.2531333385214,1.81765000563682,5.23548413644653));
#132767=CARTESIAN_POINT('Ctrl Pts',(5.28286154154871,1.81128115488623,5.26474077435008));
#132768=CARTESIAN_POINT('Ctrl Pts',(5.31260069112421,1.80506741744112,5.29398468919549));
#132769=CARTESIAN_POINT('',(4.72853014526859,1.71532338830053,5.65835692720741));
#132770=CARTESIAN_POINT('Origin',(-3.70797142990043E-13,1.80614392399972,
-5.24753851482984E-13));
#132771=CARTESIAN_POINT('',(5.3154082369853,1.62564958723406,5.29116577603139));
#132772=CARTESIAN_POINT('Origin',(-0.147018238527079,1.48225708010876,-0.114049756782595));
#132773=CARTESIAN_POINT('',(5.69992859077017,1.71532338735754,4.8745065462909));
#132774=CARTESIAN_POINT('Origin',(-0.155644556101205,1.87485301895261,-0.0996550053948186));
#132775=CARTESIAN_POINT('Ctrl Pts',(5.31260069456111,1.80506741667151,5.29398468568869));
#132776=CARTESIAN_POINT('Ctrl Pts',(5.39518241618632,1.78658581165965,5.21111257035019));
#132777=CARTESIAN_POINT('Ctrl Pts',(5.47565154239998,1.76822051521757,5.12648021422536));
#132778=CARTESIAN_POINT('Ctrl Pts',(5.5539057960115,1.74999999998492,5.04025102627439));
#132779=CARTESIAN_POINT('Ctrl Pts',(5.60331176043689,1.73849644462036,4.9858100722164));
#132780=CARTESIAN_POINT('Ctrl Pts',(5.65199898542071,1.72693520694185,4.93055228506105));
#132781=CARTESIAN_POINT('Ctrl Pts',(5.69992858871765,1.71532338729505,4.87450654684407));
#132782=CARTESIAN_POINT('Ctrl Pts',(5.131125069,1.845058467,5.121919125));
#132783=CARTESIAN_POINT('Ctrl Pts',(5.337009493,1.797173233,4.915664652));
#132784=CARTESIAN_POINT('Ctrl Pts',(5.5256749,1.75,4.693550565));
#132785=CARTESIAN_POINT('Ctrl Pts',(5.594800682,1.732716033,4.612169403));
#132786=CARTESIAN_POINT('Ctrl Pts',(5.661499867,1.715323387,4.528787835));
#132787=CARTESIAN_POINT('Ctrl Pts',(5.131437393,1.845058467,5.469766932));
#132788=CARTESIAN_POINT('Ctrl Pts',(5.351304163,1.797173233,5.263499904));
#132789=CARTESIAN_POINT('Ctrl Pts',(5.553905796,1.75,5.040251027));
#132790=CARTESIAN_POINT('Ctrl Pts',(5.628137721,1.732716033,4.958454085));
#132791=CARTESIAN_POINT('Ctrl Pts',(5.69992859,1.715323387,4.874506546));
#132792=CARTESIAN_POINT('',(5.6807142316068,1.71532338778839,4.70164718674625));
#132793=CARTESIAN_POINT('Ctrl Pts',(5.661499867,1.715323387,4.528787835));
#132794=CARTESIAN_POINT('Ctrl Pts',(5.906659286,1.779910221,4.222310679));
#132795=CARTESIAN_POINT('Ctrl Pts',(6.117301603,1.845052736,3.891159352));
#132796=CARTESIAN_POINT('Ctrl Pts',(6.00721857800001,1.715323387,4.490359112));
#132797=CARTESIAN_POINT('Ctrl Pts',(6.250297713,1.779910221,4.165166971));
#132798=CARTESIAN_POINT('Ctrl Pts',(6.456851606,1.845052736,3.815634592));
#132799=CARTESIAN_POINT('',(6.00721857692768,1.71532338744743,4.4903591152651));
#132800=CARTESIAN_POINT('',(6.32644526003464,1.80506741731562,4.02816215775166));
#132801=CARTESIAN_POINT('Origin',(-0.166438120757657,1.87497456263235,-0.0926677379795166));
#132802=CARTESIAN_POINT('Ctrl Pts',(6.11478601007336,1.84427517366593,3.89511130188059));
#132803=CARTESIAN_POINT('Ctrl Pts',(6.14998991154671,1.83740483692664,3.91728504138385));
#132804=CARTESIAN_POINT('Ctrl Pts',(6.18525078550277,1.83070797992551,3.93947120792344));
#132805=CARTESIAN_POINT('Ctrl Pts',(6.25579235404182,1.81765000111118,3.98381305591478));
#132806=CARTESIAN_POINT('Ctrl Pts',(6.2911148683189,1.81128114571037,4.00599502240091));
#132807=CARTESIAN_POINT('Ctrl Pts',(6.32644525851615,1.80506741739896,4.02816216019523));
#132808=CARTESIAN_POINT('',(5.83435921754669,1.71532338829715,4.50957347990846));
#132809=CARTESIAN_POINT('Origin',(-6.34908792207511E-13,1.80614392400067,
-4.53196508098941E-13));
#132810=CARTESIAN_POINT('',(6.32858118252632,1.62564958718437,4.024805611846));
#132811=CARTESIAN_POINT('Origin',(-0.168098257326036,1.48225710020701,-0.0797786914912602));
#132812=CARTESIAN_POINT('',(6.61454224581474,1.71532338735652,3.53522713313313));
#132813=CARTESIAN_POINT('Origin',(-0.17342861253934,1.87485299658896,-0.0638661794487672));
#132814=CARTESIAN_POINT('Ctrl Pts',(6.32644526115658,1.80506741660584,4.02816215574145));
#132815=CARTESIAN_POINT('Ctrl Pts',(6.38928121287247,1.7865858116304,3.92947491541144));
#132816=CARTESIAN_POINT('Ctrl Pts',(6.44967556073724,1.76822051520956,3.82952273321842));
#132817=CARTESIAN_POINT('Ctrl Pts',(6.50756354678065,1.75000000001832,3.72848718457675));
#132818=CARTESIAN_POINT('Ctrl Pts',(6.54411123116617,1.73849644467496,3.66469820839607));
#132819=CARTESIAN_POINT('Ctrl Pts',(6.57978138511481,1.72693520694185,3.60026600275635));
#132820=CARTESIAN_POINT('Ctrl Pts',(6.61454224392906,1.71532338729505,3.53522713409992));
#132821=CARTESIAN_POINT('Ctrl Pts',(6.112223425,1.845058467,3.899131288));
#132822=CARTESIAN_POINT('Ctrl Pts',(6.268955771,1.797173233,3.653439864));
#132823=CARTESIAN_POINT('Ctrl Pts',(6.405462322,1.75,3.395961195));
#132824=CARTESIAN_POINT('Ctrl Pts',(6.455477438,1.732716033,3.30162268));
#132825=CARTESIAN_POINT('Ctrl Pts',(6.502692661,1.715323387,3.205852173));
#132826=CARTESIAN_POINT('Ctrl Pts',(6.187305443,1.845058467,4.238779465));
#132827=CARTESIAN_POINT('Ctrl Pts',(6.357690537,1.797173233,3.99006999));
#132828=CARTESIAN_POINT('Ctrl Pts',(6.507563547,1.75,3.728487185));
#132829=CARTESIAN_POINT('Ctrl Pts',(6.562476046,1.732716033,3.632644941));
#132830=CARTESIAN_POINT('Ctrl Pts',(6.614542245,1.715323387,3.535227133));
#132831=CARTESIAN_POINT('',(6.55861745522722,1.71532338778839,3.37053964866614));
#132832=CARTESIAN_POINT('Ctrl Pts',(6.502692661,1.715323387,3.205852173));
#132833=CARTESIAN_POINT('Ctrl Pts',(6.676236859,1.779910221,2.853838255));
#132834=CARTESIAN_POINT('Ctrl Pts',(6.810766729,1.845052736,2.48514719));
#132835=CARTESIAN_POINT('Ctrl Pts',(6.832067621,1.715323387,3.094002589));
#132836=CARTESIAN_POINT('Ctrl Pts',(6.999557003,1.779910221,2.724158431));
#132837=CARTESIAN_POINT('Ctrl Pts',(7.126142651,1.845052736,2.338394944));
#132838=CARTESIAN_POINT('',(6.83206762065268,1.71532338744779,3.09400259242416));
#132839=CARTESIAN_POINT('',(7.04447227761881,1.80506741731637,2.57398724268056));
#132840=CARTESIAN_POINT('Origin',(-0.182467701556788,1.87497457397358,-0.0547219325918286));
#132841=CARTESIAN_POINT('Ctrl Pts',(6.80915950284082,1.84427517370896,2.48954752285449));
#132842=CARTESIAN_POINT('Ctrl Pts',(6.84830704640822,1.83740483848713,2.50363505160379));
#132843=CARTESIAN_POINT('Ctrl Pts',(6.88751290039156,1.83070798310218,2.51772246887146));
#132844=CARTESIAN_POINT('Ctrl Pts',(6.96593745123682,1.81765000117452,2.54586328409677));
#132845=CARTESIAN_POINT('Ctrl Pts',(7.00520261195919,1.81128114573483,2.55993335230123));
#132846=CARTESIAN_POINT('Ctrl Pts',(7.04447227667578,1.80506741739832,2.57398724535184));
#132847=CARTESIAN_POINT('',(6.66738013753733,1.71532338829819,3.14992738832937));
#132848=CARTESIAN_POINT('Origin',(-6.5746019739521E-13,1.80614392400017,
-3.50414142147315E-13));
#132849=CARTESIAN_POINT('',(7.04583670518615,1.62564958718578,2.57025001060835));
#132850=CARTESIAN_POINT('Origin',(-0.181318472582188,1.48225706044545,-0.041777424151937));
#132851=CARTESIAN_POINT('',(7.21986725682524,1.71532338735623,2.03064442895894));
#132852=CARTESIAN_POINT('Origin',(-0.183103012008832,1.87485300201219,-0.0250909106018232));
#132853=CARTESIAN_POINT('Ctrl Pts',(7.04447227826771,1.80506741661818,2.57398724050962));
#132854=CARTESIAN_POINT('Ctrl Pts',(7.08462432078263,1.78658581163429,2.46409938080374));
#132855=CARTESIAN_POINT('Ctrl Pts',(7.12211991779882,1.76822051520959,2.3535010254003));
#132856=CARTESIAN_POINT('Ctrl Pts',(7.15693485866943,1.75000000001996,2.24238342560448));
#132857=CARTESIAN_POINT('Ctrl Pts',(7.17891533426046,1.73849644467764,2.17222912820569));
#132858=CARTESIAN_POINT('Ctrl Pts',(7.19990052025176,1.72693520694185,2.10163528313927));
#132859=CARTESIAN_POINT('Ctrl Pts',(7.21986725519057,1.71532338729505,2.03064443030443));
#132860=CARTESIAN_POINT('Ctrl Pts',(6.807521008,1.845058467,2.494024404));
#132861=CARTESIAN_POINT('Ctrl Pts',(6.907772645,1.797173233,2.220384289));
#132862=CARTESIAN_POINT('Ctrl Pts',(6.985737446,1.75,1.939580454));
#132863=CARTESIAN_POINT('Ctrl Pts',(7.014303243,1.732716033,1.83669575));
#132864=CARTESIAN_POINT('Ctrl Pts',(7.039826773,1.715323387,1.733014427));
#132865=CARTESIAN_POINT('Ctrl Pts',(6.953861968,1.845058467,2.809591382));
#132866=CARTESIAN_POINT('Ctrl Pts',(7.06679836700001,1.797173233,2.530068838));
#132867=CARTESIAN_POINT('Ctrl Pts',(7.156934859,1.75,2.242383426));
#132868=CARTESIAN_POINT('Ctrl Pts',(7.18996028500001,1.732716033,2.136977356));
#132869=CARTESIAN_POINT('Ctrl Pts',(7.21986725600001,1.715323387,2.030644429));
#132870=CARTESIAN_POINT('',(7.12984701574349,1.71532338778839,1.88182942328867));
#132871=CARTESIAN_POINT('Ctrl Pts',(7.039826773,1.715323387,1.733014427));
#132872=CARTESIAN_POINT('Ctrl Pts',(7.133641018,1.779910221,1.351923526));
#132873=CARTESIAN_POINT('Ctrl Pts',(7.18576797400001,1.845052736,0.962932308));
#132874=CARTESIAN_POINT('Ctrl Pts',(7.337456775,1.715323387,1.552973944));
#132875=CARTESIAN_POINT('Ctrl Pts',(7.421524787,1.779910221,1.15577127));
#132876=CARTESIAN_POINT('Ctrl Pts',(7.462223187,1.845052736,0.751814547));
#132877=CARTESIAN_POINT('',(7.33745677540195,1.71532338744823,1.55297394741524));
#132878=CARTESIAN_POINT('',(7.43310760101885,1.80506741731817,0.99945554461675));
#132879=CARTESIAN_POINT('Origin',(-0.189965455514084,1.87497461017791,-0.0142174232791398));
#132880=CARTESIAN_POINT('Ctrl Pts',(7.18514426466047,1.84427517372893,0.967575270075705));
#132881=CARTESIAN_POINT('Ctrl Pts',(7.22640497351326,1.83740483668611,0.972917876941878));
#132882=CARTESIAN_POINT('Ctrl Pts',(7.26772260749884,1.83070797936229,0.978247840077157));
#132883=CARTESIAN_POINT('Ctrl Pts',(7.35036305583967,1.81765000113681,0.988871775213704));
#132884=CARTESIAN_POINT('Ctrl Pts',(7.39173486735399,1.8112811457412,0.994172043980483));
#132885=CARTESIAN_POINT('Ctrl Pts',(7.43310760065318,1.80506741740517,0.999455547582473));
#132886=CARTESIAN_POINT('',(7.1886417721921,1.71532338829947,1.64299419341015));
#132887=CARTESIAN_POINT('Origin',(6.38811920028459E-13,1.80614392400006,
-5.39390580811538E-15));
#132888=CARTESIAN_POINT('',(7.43363673487287,1.62564958721554,0.995512375212924));
#132889=CARTESIAN_POINT('Origin',(-0.186060401123735,1.48225706441154,-0.00182260911100379));
#132890=CARTESIAN_POINT('',(7.48759929982863,1.71532338734673,0.43111104887891));
#132891=CARTESIAN_POINT('Origin',(-0.184216316486344,1.87485304405876,0.0148574046167898));
#132892=CARTESIAN_POINT('Ctrl Pts',(7.4331076011919,1.805067416582,0.999455542227304));
#132893=CARTESIAN_POINT('Ctrl Pts',(7.44869826958329,1.78658581162576,0.883505297448109));
#132894=CARTESIAN_POINT('Ctrl Pts',(7.46154186313188,1.76822051521192,0.767432225427406));
#132895=CARTESIAN_POINT('Ctrl Pts',(7.47165585077362,1.74999999996564,0.651428310507613));
#132896=CARTESIAN_POINT('Ctrl Pts',(7.47804133522892,1.73849644458883,0.57818902898479));
#132897=CARTESIAN_POINT('Ctrl Pts',(7.48336030927677,1.72693520694185,0.504734434407505));
#132898=CARTESIAN_POINT('Ctrl Pts',(7.4875992984897,1.71532338729505,0.431111050447745));
#132899=CARTESIAN_POINT('Ctrl Pts',(7.184506474,1.845058467,0.972299712));
#132900=CARTESIAN_POINT('Ctrl Pts',(7.223589747,1.797173233,0.683506012));
#132901=CARTESIAN_POINT('Ctrl Pts',(7.23936725,1.75,0.392507087));
#132902=CARTESIAN_POINT('Ctrl Pts',(7.245148025,1.732716033,0.285886968));
#132903=CARTESIAN_POINT('Ctrl Pts',(7.24778641,1.715323387,0.179142852));
#132904=CARTESIAN_POINT('Ctrl Pts',(7.395263635,1.845058467,1.249029928));
#132905=CARTESIAN_POINT('Ctrl Pts',(7.44547056,1.797173233,0.951764478));
#132906=CARTESIAN_POINT('Ctrl Pts',(7.471655851,1.75,0.651428311));
#132907=CARTESIAN_POINT('Ctrl Pts',(7.481249972,1.732716033,0.541387086));
#132908=CARTESIAN_POINT('Ctrl Pts',(7.487599299,1.715323387,0.431111049));
#132909=CARTESIAN_POINT('',(7.36769285470163,1.71532338778839,0.305126945631507));
#132910=CARTESIAN_POINT('Ctrl Pts',(7.24778641,1.715323387,0.179142852));
#132911=CARTESIAN_POINT('Ctrl Pts',(7.25748405,1.779910221,-0.213205645));
#132912=CARTESIAN_POINT('Ctrl Pts',(7.22477069400001,1.845052736,-0.604308219));
#132913=CARTESIAN_POINT('Ctrl Pts',(7.499754606,1.715323387,-0.060670037));
#132914=CARTESIAN_POINT('Ctrl Pts',(7.496470321,1.779910221,-0.46665847));
#132915=CARTESIAN_POINT('Ctrl Pts',(7.449378459,1.845052736,-0.869919863));
#132916=CARTESIAN_POINT('',(7.49975460711691,1.71532338744859,-0.0606700337169635));
#132917=CARTESIAN_POINT('',(7.47417907449485,1.80506741732727,-0.621809583799175));
#132918=CARTESIAN_POINT('Origin',(-0.188580229757588,1.87497455775272,0.0269519145656917));
#132919=CARTESIAN_POINT('Ctrl Pts',(7.22515966610095,1.84427517370307,-0.599639727402906));
#132920=CARTESIAN_POINT('Ctrl Pts',(7.26660422586505,1.83740483653573,-0.603291860843548));
#132921=CARTESIAN_POINT('Ctrl Pts',(7.30810166197752,1.83070797908474,-0.606968579461518));
#132922=CARTESIAN_POINT('Ctrl Pts',(7.3910938530514,1.81765000112985,-0.614358279513735));
#132923=CARTESIAN_POINT('Ctrl Pts',(7.43263781590535,1.81128114572277,-0.618075644573826));
#132924=CARTESIAN_POINT('Ctrl Pts',(7.47417907476336,1.80506741741021,-0.621809580950034));
#132925=CARTESIAN_POINT('',(7.37377050793477,1.71532338830053,0.0592364156205474));
#132926=CARTESIAN_POINT('Origin',(-3.72531866466019E-13,1.8061439240005,
9.02598308594182E-14));
#132927=CARTESIAN_POINT('',(7.47384817270388,1.6256495872157,-0.625774312001561));
#132928=CARTESIAN_POINT('Origin',(-0.182101997659883,1.48225706935401,0.0382174822994667));
#132929=CARTESIAN_POINT('',(7.40521952078754,1.71532338734622,-1.18858060629072));
#132930=CARTESIAN_POINT('Origin',(-0.176715334484012,1.87485302405344,0.0541110863609406));
#132931=CARTESIAN_POINT('Ctrl Pts',(7.47417907417002,1.80506741662168,-0.621809586066532));
#132932=CARTESIAN_POINT('Ctrl Pts',(7.46447936625317,1.7865858116396,-0.738400511443372));
#132933=CARTESIAN_POINT('Ctrl Pts',(7.45207040425345,1.76822051521369,-0.854520852749165));
#132934=CARTESIAN_POINT('Ctrl Pts',(7.4370105196625,1.750000000046,-0.96998686897824));
#132935=CARTESIAN_POINT('Ctrl Pts',(7.42750243431284,1.7384964447202,-1.04288654643311));
#132936=CARTESIAN_POINT('Ctrl Pts',(7.41690648710136,1.72693520694185,-1.11576723638024));
#132937=CARTESIAN_POINT('Ctrl Pts',(7.40521951981277,1.71532338729505,-1.18858060447645));
#132938=CARTESIAN_POINT('Ctrl Pts',(7.225552402,1.845058467,-0.594888634));
#132939=CARTESIAN_POINT('Ctrl Pts',(7.201639821,1.797173233,-0.885332247));
#132940=CARTESIAN_POINT('Ctrl Pts',(7.154492288,1.75,-1.172919475));
#132941=CARTESIAN_POINT('Ctrl Pts',(7.137217738,1.732716033,-1.278289571));
#132942=CARTESIAN_POINT('Ctrl Pts',(7.116847609,1.715323387,-1.383105243));
#132943=CARTESIAN_POINT('Ctrl Pts',(7.490870995,1.845058467,-0.369934777));
#132944=CARTESIAN_POINT('Ctrl Pts',(7.476000825,1.797173233,-0.67104333));
#132945=CARTESIAN_POINT('Ctrl Pts',(7.43701052,1.75,-0.969986869));
#132946=CARTESIAN_POINT('Ctrl Pts',(7.422724725,1.732716033,-1.079517843));
#132947=CARTESIAN_POINT('Ctrl Pts',(7.40521952,1.715323387,-1.188580606));
#132948=CARTESIAN_POINT('',(7.26103356365033,1.71532338778839,-1.28584292929801));
#132949=CARTESIAN_POINT('Ctrl Pts',(7.116847609,1.715323387,-1.383105243));
#132950=CARTESIAN_POINT('Ctrl Pts',(7.04197519500001,1.779910221,-1.768365556));
#132951=CARTESIAN_POINT('Ctrl Pts',(6.925951166,1.845052736,-2.143291965));
#132952=CARTESIAN_POINT('Ctrl Pts',(7.311372246,1.715323387,-1.671477154));
#132953=CARTESIAN_POINT('Ctrl Pts',(7.220889234,1.779910221,-2.067267779));
#132954=CARTESIAN_POINT('Ctrl Pts',(7.088209075,1.845052736,-2.450977787));
#132955=CARTESIAN_POINT('',(7.31137224780019,1.7153233874486,-1.67147715106331));
#132956=CARTESIAN_POINT('',(7.16576624136519,1.80506741729005,-2.21399958686633));
#132957=CARTESIAN_POINT('Origin',(-0.178377524981393,1.87497455155373,0.0668609764454212));
#132958=CARTESIAN_POINT('Ctrl Pts',(6.92733463178518,1.84427517371465,-2.13881623762417));
#132959=CARTESIAN_POINT('Ctrl Pts',(6.96702514232173,1.83740483617331,-2.15129234207367));
#132960=CARTESIAN_POINT('Ctrl Pts',(7.00676200825457,1.83070797831737,-2.16380382392064));
#132961=CARTESIAN_POINT('Ctrl Pts',(7.08622531640099,1.81765000111462,-2.18886162321189));
#132962=CARTESIAN_POINT('Ctrl Pts',(7.12599888080652,1.81128114571596,-2.20142280227942));
#132963=CARTESIAN_POINT('Ctrl Pts',(7.16576624227572,1.80506741737912,-2.21399958403128));
#132964=CARTESIAN_POINT('',(7.21410992918197,1.71532338830053,-1.52729119055528));
#132965=CARTESIAN_POINT('Origin',(-1.3162214373974E-12,1.80614392400089,
4.32596666821716E-13));
#132966=CARTESIAN_POINT('',(7.1645907762973,1.62564958719313,-2.21780048786883));
#132967=CARTESIAN_POINT('Origin',(-0.169628947985297,1.48225708989375,0.0764705232282592));
#132968=CARTESIAN_POINT('',(6.97657990728278,1.7153233872797,-2.75269555326827));
#132969=CARTESIAN_POINT('Origin',(-0.160951713078892,1.87485303486766,0.0908346270390281));
#132970=CARTESIAN_POINT('Ctrl Pts',(7.16576624052238,1.80506741655413,-2.21399958912398));
#132971=CARTESIAN_POINT('Ctrl Pts',(7.11406920084479,1.77740267790226,-2.38132071423326));
#132972=CARTESIAN_POINT('Ctrl Pts',(7.05461884250418,1.75,-2.54604654021329));
#132973=CARTESIAN_POINT('Ctrl Pts',(7.01712111950104,1.732716033,-2.64994571820598));
#132974=CARTESIAN_POINT('Ctrl Pts',(6.97657990649811,1.715323387,-2.75269555219859));
#132975=CARTESIAN_POINT('Ctrl Pts',(6.92873953,1.845058467,-2.134260649));
#132976=CARTESIAN_POINT('Ctrl Pts',(6.84294922100001,1.797173233,-2.412773354));
#132977=CARTESIAN_POINT('Ctrl Pts',(6.735081219,1.75,-2.683501626));
#132978=CARTESIAN_POINT('Ctrl Pts',(6.695559082,1.732716033,-2.78269471));
#132979=CARTESIAN_POINT('Ctrl Pts',(6.653132924,1.715323387,-2.880680874));
#132980=CARTESIAN_POINT('Ctrl Pts',(7.236213552,1.845058467,-1.971601742));
#132981=CARTESIAN_POINT('Ctrl Pts',(7.1569616,1.797173233,-2.262473898));
#132982=CARTESIAN_POINT('Ctrl Pts',(7.054618843,1.75,-2.54604654));
#132983=CARTESIAN_POINT('Ctrl Pts',(7.01712112,1.732716033,-2.649945718));
#132984=CARTESIAN_POINT('Ctrl Pts',(6.976579907,1.715323387,-2.752695552));
#132985=CARTESIAN_POINT('',(6.81485641363876,1.71532338778839,-2.81668821750318));
#132986=CARTESIAN_POINT('Ctrl Pts',(6.653132924,1.715323387,-2.880680874));
#132987=CARTESIAN_POINT('Ctrl Pts',(6.497191406,1.779910221,-3.24083866));
#132988=CARTESIAN_POINT('Ctrl Pts',(6.303281859,1.845052736,-3.582057761));
#132989=CARTESIAN_POINT('Ctrl Pts',(6.781118246,1.715323387,-3.204127858));
#132990=CARTESIAN_POINT('Ctrl Pts',(6.607667391,1.779910221,-3.571213945));
#132991=CARTESIAN_POINT('Ctrl Pts',(6.395602912,1.845052736,-3.917430713));
#132992=CARTESIAN_POINT('',(6.78111824838966,1.7153233874486,-3.20412785551618));
#132993=CARTESIAN_POINT('',(6.52229014260304,1.80506741731559,-3.70266543055499));
#132994=CARTESIAN_POINT('Origin',(-0.159834165078843,1.87497459574732,0.103643782784949));
#132995=CARTESIAN_POINT('Ctrl Pts',(6.30559512922781,1.84427517371725,-3.57798407800257));
#132996=CARTESIAN_POINT('Ctrl Pts',(6.34167569827233,1.83740483728647,-3.59870078122464));
#132997=CARTESIAN_POINT('Ctrl Pts',(6.37779393284573,1.83070798060367,-3.61946199927444));
#132998=CARTESIAN_POINT('Ctrl Pts',(6.45001275928298,1.81765000115535,-3.66101623075933));
#132999=CARTESIAN_POINT('Ctrl Pts',(6.48615615778852,1.8112811457277,-3.68183387727167));
#133000=CARTESIAN_POINT('Ctrl Pts',(6.52229014402864,1.80506741739754,-3.70266542810664));
#133001=CARTESIAN_POINT('',(6.71712558835053,1.71532338830053,-3.0424043586026));
#133002=CARTESIAN_POINT('Origin',(-7.41594285980085E-13,1.80614392400039,
4.57966997657877E-13));
#133003=CARTESIAN_POINT('',(6.52032507813897,1.62564958718767,-3.70612477802065));
#133004=CARTESIAN_POINT('Origin',(-0.149224148019865,1.48225708657861,0.111147861824504));
#133005=CARTESIAN_POINT('',(6.22172317159653,1.71532338734596,-4.18809751359268));
#133006=CARTESIAN_POINT('Origin',(-0.137661888875984,1.87485299115467,0.123310757861001));
#133007=CARTESIAN_POINT('Ctrl Pts',(6.52229014136684,1.80506741661758,-3.70266543245436));
#133008=CARTESIAN_POINT('Ctrl Pts',(6.46453166599464,1.78658581163406,-3.80440768893434));
#133009=CARTESIAN_POINT('Ctrl Pts',(6.40451193142273,1.76822051520921,-3.90458526841971));
#133010=CARTESIAN_POINT('Ctrl Pts',(6.34236102849571,1.74999999995533,-4.00305590530895));
#133011=CARTESIAN_POINT('Ctrl Pts',(6.30312194351028,1.73849644457198,-4.06522552017018));
#133012=CARTESIAN_POINT('Ctrl Pts',(6.26290351519366,1.72693520694186,-4.12692111936024));
#133013=CARTESIAN_POINT('Ctrl Pts',(6.22172317147024,1.71532338729505,-4.18809751153858));
#133014=CARTESIAN_POINT('Ctrl Pts',(6.307946499,1.845058467,-3.573837008));
#133015=CARTESIAN_POINT('Ctrl Pts',(6.164289921,1.797173233,-3.82739586));
#133016=CARTESIAN_POINT('Ctrl Pts',(6.000745237,1.75,-4.068606224));
#133017=CARTESIAN_POINT('Ctrl Pts',(5.940823524,1.732716033,-4.156984138));
#133018=CARTESIAN_POINT('Ctrl Pts',(5.87832513800001,1.715323387,-4.24355907));
#133019=CARTESIAN_POINT('Ctrl Pts',(6.643198806,1.845058467,-3.481078802));
#133020=CARTESIAN_POINT('Ctrl Pts',(6.503270805,1.797173233,-3.748113702));
#133021=CARTESIAN_POINT('Ctrl Pts',(6.342361029,1.75,-4.003055905));
#133022=CARTESIAN_POINT('Ctrl Pts',(6.28340473,1.732716033,-4.096465076));
#133023=CARTESIAN_POINT('Ctrl Pts',(6.221723171,1.715323387,-4.188097513));
#133024=CARTESIAN_POINT('',(6.05002415171423,1.71532338778839,-4.21582829549779));
#133025=CARTESIAN_POINT('Ctrl Pts',(5.878325138,1.715323387,-4.24355907));
#133026=CARTESIAN_POINT('Ctrl Pts',(5.648606168,1.779910221,-4.56177375));
#133027=CARTESIAN_POINT('Ctrl Pts',(5.385878098,1.845052736,-4.853330517));
#133028=CARTESIAN_POINT('Ctrl Pts',(5.933786694,1.715323387,-4.586957104));
#133029=CARTESIAN_POINT('Ctrl Pts',(5.685478366,1.779910221,-4.908174115));
#133030=CARTESIAN_POINT('Ctrl Pts',(5.403945465,1.845052736,-5.200708934));
#133031=CARTESIAN_POINT('',(5.93378669687623,1.71532338744858,-4.5869571020615));
#133032=CARTESIAN_POINT('',(5.57383900614683,1.80506741730661,-5.01819875357225));
#133033=CARTESIAN_POINT('Origin',(-0.133817050721352,1.8749745499756,0.135580323984583));
#133034=CARTESIAN_POINT('Ctrl Pts',(5.38901300709274,1.84427517363401,-4.84984936019252));
#133035=CARTESIAN_POINT('Ctrl Pts',(5.41979654877647,1.83740483829925,-4.87783796967003));
#133036=CARTESIAN_POINT('Ctrl Pts',(5.45060730516344,1.83070798279121,-4.90587814936565));
#133037=CARTESIAN_POINT('Ctrl Pts',(5.51220477455614,1.81765000115592,-4.96198578808963));
#133038=CARTESIAN_POINT('Ctrl Pts',(5.54302798188949,1.81128114573603,-4.99008649174508));
#133039=CARTESIAN_POINT('Ctrl Pts',(5.57383900811601,1.80506741739091,-5.01819875143265));
#133040=CARTESIAN_POINT('',(5.90605592086241,1.71532338830053,-4.41525808049581));
#133041=CARTESIAN_POINT('Origin',(-7.43329009456062E-13,1.80614392399978,
7.86263415486488E-13));
#133042=CARTESIAN_POINT('',(5.5711762260882,1.62564958718905,-5.02115479264374));
#133043=CARTESIAN_POINT('Origin',(-0.121842006482895,1.48225709229395,0.140628193630493));
#133044=CARTESIAN_POINT('',(5.17594557531704,1.71532338735862,-5.42766869075742));
#133045=CARTESIAN_POINT('Origin',(-0.107935379387698,1.87485296552199,0.150021153472114));
#133046=CARTESIAN_POINT('Ctrl Pts',(5.57383900449109,1.80506741658938,-5.01819875520795));
#133047=CARTESIAN_POINT('Ctrl Pts',(5.49555931254626,1.78658581162276,-5.1051459692823));
#133048=CARTESIAN_POINT('Ctrl Pts',(5.41540758776006,1.76822051520736,-5.19007898388589));
#133049=CARTESIAN_POINT('Ctrl Pts',(5.33354146241272,1.7500000000465,-5.27288682476711));
#133050=CARTESIAN_POINT('Ctrl Pts',(5.28185513600857,1.73849644472102,-5.32516770431212));
#133051=CARTESIAN_POINT('Ctrl Pts',(5.22931426207082,1.72693520694185,-5.37677512226718));
#133052=CARTESIAN_POINT('Ctrl Pts',(5.17594557577341,1.71532338729505,-5.42766868867384));
#133053=CARTESIAN_POINT('Ctrl Pts',(5.392200901,1.845058467,-4.846304721));
#133054=CARTESIAN_POINT('Ctrl Pts',(5.197395276,1.797173233,-5.06305359));
#133055=CARTESIAN_POINT('Ctrl Pts',(4.985821077,1.75,-5.263467316));
#133056=CARTESIAN_POINT('Ctrl Pts',(4.908301662,1.732716033,-5.336897607));
#133057=CARTESIAN_POINT('Ctrl Pts',(4.828653401,1.715323387,-5.40801315900001));
#133058=CARTESIAN_POINT('Ctrl Pts',(5.739555467,1.845058467,-4.827784486));
#133059=CARTESIAN_POINT('Ctrl Pts',(5.54549429500001,1.797173233,-5.05849587400001));
#133060=CARTESIAN_POINT('Ctrl Pts',(5.333541463,1.75,-5.272886825));
#133061=CARTESIAN_POINT('Ctrl Pts',(5.255883319,1.732716033,-5.351438279));
#133062=CARTESIAN_POINT('Ctrl Pts',(5.175945575,1.715323387,-5.42766869));
#133063=CARTESIAN_POINT('',(5.00229948441995,1.71532338778839,-5.41784092780546));
#133064=CARTESIAN_POINT('Ctrl Pts',(4.828653401,1.715323387,-5.408013159));
#133065=CARTESIAN_POINT('Ctrl Pts',(4.535898384,1.779910221,-5.669405369));
#133066=CARTESIAN_POINT('Ctrl Pts',(4.216636664,1.845052736,-5.897666932));
#133067=CARTESIAN_POINT('Ctrl Pts',(4.808997871,1.715323387,-5.755305333));
#133068=CARTESIAN_POINT('Ctrl Pts',(4.497442691,1.779910221,-6.015633519));
#133069=CARTESIAN_POINT('Ctrl Pts',(4.159605534,1.845052736,-6.240807784));
#133070=CARTESIAN_POINT('',(4.80899787421697,1.7153233874486,-5.75530533174012));
#133071=CARTESIAN_POINT('',(4.36476135241826,1.80506741731031,-6.09908667995287));
#133072=CARTESIAN_POINT('Origin',(-0.101542619938455,1.87497458295353,0.161177119256457));
#133073=CARTESIAN_POINT('Ctrl Pts',(4.22044662611338,1.84427517372663,-5.89494107521926));
#133074=CARTESIAN_POINT('Ctrl Pts',(4.24449374406009,1.83740483775101,-5.92889288124366));
#133075=CARTESIAN_POINT('Ctrl Pts',(4.26855635477787,1.83070798156074,-5.96290090268123));
#133076=CARTESIAN_POINT('Ctrl Pts',(4.31665222094061,1.81765000116853,-6.03093840455445));
#133077=CARTESIAN_POINT('Ctrl Pts',(4.34071397812627,1.81128114573728,-6.06500820782899));
#133078=CARTESIAN_POINT('Ctrl Pts',(4.36476135477305,1.80506741739355,-6.0990866783064));
#133079=CARTESIAN_POINT('',(4.81882564214694,1.71532338830053,-5.58165924069315));
#133080=CARTESIAN_POINT('Origin',(5.08707659330199E-13,1.8061439240005,
-7.70217223333702E-13));
#133081=CARTESIAN_POINT('',(4.36152536599515,1.6256495872286,-6.10140118956462));
#133082=CARTESIAN_POINT('Origin',(-0.0887624671539777,1.48225710253061,
0.163532757542503));
#133083=CARTESIAN_POINT('',(3.88814651615066,1.71532338735835,-6.41344811180768));
#133084=CARTESIAN_POINT('Origin',(-0.0731616365055499,1.87485299007194,
0.169716425058697));
#133085=CARTESIAN_POINT('Ctrl Pts',(4.3647613504681,1.805067416603,-6.09908668117183));
#133086=CARTESIAN_POINT('Ctrl Pts',(4.26962071314246,1.78658581162838,-6.16717329779867));
#133087=CARTESIAN_POINT('Ctrl Pts',(4.17308480344671,1.76822051520836,-6.23289037410551));
#133088=CARTESIAN_POINT('Ctrl Pts',(4.07533142468709,1.74999999999323,-6.29616341695472));
#133089=CARTESIAN_POINT('Ctrl Pts',(4.01361465257327,1.73849644463394,-6.33611096694137));
#133090=CARTESIAN_POINT('Ctrl Pts',(3.95120808549899,1.72693520694185,-6.3752170969759));
#133091=CARTESIAN_POINT('Ctrl Pts',(3.88814651704041,1.71532338729505,-6.41344810987111));
#133092=CARTESIAN_POINT('Ctrl Pts',(4.224321981,1.845058467,-5.892164611));
#133093=CARTESIAN_POINT('Ctrl Pts',(3.987476203,1.797173233,-6.061968561));
#133094=CARTESIAN_POINT('Ctrl Pts',(3.737765465,1.75,-6.212214527));
#133095=CARTESIAN_POINT('Ctrl Pts',(3.646273069,1.732716033,-6.267263675));
#133096=CARTESIAN_POINT('Ctrl Pts',(3.553199198,1.715323387,-6.319594564));
#133097=CARTESIAN_POINT('Ctrl Pts',(4.567536894,1.845058467,-5.948748333));
#133098=CARTESIAN_POINT('Ctrl Pts',(4.328416635,1.797173233,-6.13234840100001));
#133099=CARTESIAN_POINT('Ctrl Pts',(4.075331425,1.75,-6.296163417));
#133100=CARTESIAN_POINT('Ctrl Pts',(3.98260264499999,1.732716033,-6.356184177));
#133101=CARTESIAN_POINT('Ctrl Pts',(3.888146516,1.715323387,-6.41344811100001));
#133102=CARTESIAN_POINT('',(3.72067285279307,1.71532338778839,-6.36652133995858));
#133103=CARTESIAN_POINT('Ctrl Pts',(3.553199198,1.715323387,-6.319594564));
#133104=CARTESIAN_POINT('Ctrl Pts',(3.211097032,1.779910221,-6.511941894));
#133105=CARTESIAN_POINT('Ctrl Pts',(2.850229985,1.845052736,-6.66623499700001));
#133106=CARTESIAN_POINT('Ctrl Pts',(3.459345652,1.715323387,-6.654541882));
#133107=CARTESIAN_POINT('Ctrl Pts',(3.099111595,1.779910221,-6.84180858500001));
#133108=CARTESIAN_POINT('Ctrl Pts',(2.720767072,1.845052736,-6.989093399));
#133109=CARTESIAN_POINT('',(3.4593456554125,1.7153233874486,-6.65454188146125));
#133110=CARTESIAN_POINT('',(2.95159230918543,1.80506741736312,-6.89478809203611));
#133111=CARTESIAN_POINT('Origin',(-0.0645203327015181,1.87497455206243,
0.179237619153348));
#133112=CARTESIAN_POINT('Ctrl Pts',(2.85453685143102,1.84427517369847,-6.66439189757178));
#133113=CARTESIAN_POINT('Ctrl Pts',(2.87072312970937,1.83740483635783,-6.70271935640467));
#133114=CARTESIAN_POINT('Ctrl Pts',(2.88691245442373,1.83070797872001,-6.74110504825094));
#133115=CARTESIAN_POINT('Ctrl Pts',(2.91925780734436,1.81765000115226,-6.81789104434923));
#133116=CARTESIAN_POINT('Ctrl Pts',(2.93543301336312,1.81128114575983,-6.85633688103594));
#133117=CARTESIAN_POINT('Ctrl Pts',(2.9515923118759,1.80506741744797,-6.89478809091914));
#133118=CARTESIAN_POINT('',(3.50627243214405,1.71532338830053,-6.48706821913863));
#133119=CARTESIAN_POINT('Origin',(1.26634813746307E-13,1.80614392399972,
-3.70363462121048E-13));
#133120=CARTESIAN_POINT('',(2.94793442701481,1.62564958720091,-6.89635284844599));
#133121=CARTESIAN_POINT('Origin',(-0.0515325910989406,1.48225709321937,
0.178790863984528));
#133122=CARTESIAN_POINT('',(2.41854204810154,1.71532338734699,-7.09934182683035));
#133123=CARTESIAN_POINT('Origin',(-0.0349672952353988,1.87485305299441,
0.18147657222317));
#133124=CARTESIAN_POINT('Ctrl Pts',(2.9515923069852,1.80506741664557,-6.89478809282103));
#133125=CARTESIAN_POINT('Ctrl Pts',(2.844039395054,1.78658581166052,-6.940830457713));
#133126=CARTESIAN_POINT('Ctrl Pts',(2.73563321256291,1.76822051522611,-6.98425873842889));
#133127=CARTESIAN_POINT('Ctrl Pts',(2.62656341956293,1.75000000000633,-7.02503840575027));
#133128=CARTESIAN_POINT('Ctrl Pts',(2.55770200869291,1.73849644465536,-7.05078472224044));
#133129=CARTESIAN_POINT('Ctrl Pts',(2.48834781076598,1.72693520694185,-7.07556100547006));
#133130=CARTESIAN_POINT('Ctrl Pts',(2.41854204925877,1.71532338729505,-7.09934182512115));
#133131=CARTESIAN_POINT('Ctrl Pts',(2.85891846,1.845058467,-6.662513432));
#133132=CARTESIAN_POINT('Ctrl Pts',(2.591107176,1.797173233,-6.777432619));
#133133=CARTESIAN_POINT('Ctrl Pts',(2.314936093,1.75,-6.870485491));
#133134=CARTESIAN_POINT('Ctrl Pts',(2.213748799,1.732716033,-6.90457946));
#133135=CARTESIAN_POINT('Ctrl Pts',(2.11160135,1.715323387,-6.935678751));
#133136=CARTESIAN_POINT('Ctrl Pts',(3.181945371,1.845058467,-6.791555319));
#133137=CARTESIAN_POINT('Ctrl Pts',(2.908947024,1.797173233,-6.919459133));
#133138=CARTESIAN_POINT('Ctrl Pts',(2.62656342,1.75,-7.025038406));
#133139=CARTESIAN_POINT('Ctrl Pts',(2.523099898,1.732716033,-7.063721967));
#133140=CARTESIAN_POINT('Ctrl Pts',(2.418542048,1.715323387,-7.099341826));
#133141=CARTESIAN_POINT('',(2.2650716943629,1.71532338778839,-7.01751028999674));
#133142=CARTESIAN_POINT('Ctrl Pts',(2.11160135,1.715323387,-6.935678751));
#133143=CARTESIAN_POINT('Ctrl Pts',(1.736148353,1.779910221,-7.049987254));
#133144=CARTESIAN_POINT('Ctrl Pts',(1.35054972,1.845052736,-7.123097322));
#133145=CARTESIAN_POINT('Ctrl Pts',(1.947938275,1.715323387,-7.242619448));
#133146=CARTESIAN_POINT('Ctrl Pts',(1.555869484,1.779910221,-7.348068286));
#133147=CARTESIAN_POINT('Ctrl Pts',(1.154708565,1.845052736,-7.410576774));
#133148=CARTESIAN_POINT('',(1.94793827842462,1.71532338744861,-7.24261944822413));
#133149=CARTESIAN_POINT('',(1.40041008981262,1.80506741730835,-7.36809687579697));
#133150=CARTESIAN_POINT('Origin',(-0.0244810838891019,1.87497458259997,
0.188917070257419));
#133151=CARTESIAN_POINT('Ctrl Pts',(1.35515210599349,1.84427517370281,-7.12222316244358));
#133152=CARTESIAN_POINT('Ctrl Pts',(1.36272068687216,1.83740483687102,-7.163134114833));
#133153=CARTESIAN_POINT('Ctrl Pts',(1.37027972446643,1.83070797976688,-7.20410259313213));
#133154=CARTESIAN_POINT('Ctrl Pts',(1.38536214280713,1.81765000114587,-7.28604667632506));
#133155=CARTESIAN_POINT('Ctrl Pts',(1.39289446305999,1.81128114571295,-7.32707086193457));
#133156=CARTESIAN_POINT('Ctrl Pts',(1.40041009257676,1.80506741738948,-7.36809687530289));
#133157=CARTESIAN_POINT('',(2.0297698203071,1.71532338830053,-7.08914909726467));
#133158=CARTESIAN_POINT('Origin',(5.0415401020576E-15,1.80614392400089,
1.70002900645727E-13));
#133159=CARTESIAN_POINT('',(1.39650135063366,1.6256495872356,-7.36883871276101));
#133160=CARTESIAN_POINT('Origin',(-0.0118930177375121,1.48225706706544,
0.185688717421748));
#133161=CARTESIAN_POINT('',(0.835849240922742,1.71532338734683,-7.4532782088336));
#133162=CARTESIAN_POINT('Origin',(0.00486236476819724,1.87485299080187,
0.184750327284376));
#133163=CARTESIAN_POINT('Ctrl Pts',(1.40041008758366,1.80506741661815,-7.36809687607145));
#133164=CARTESIAN_POINT('Ctrl Pts',(1.2854739556344,1.78658581163196,-7.38994209922501));
#133165=CARTESIAN_POINT('Ctrl Pts',(1.17026645276057,1.76822051520721,-7.40905092596894));
#133166=CARTESIAN_POINT('Ctrl Pts',(1.05498022756264,1.7499999999812,-7.42543040576093));
#133167=CARTESIAN_POINT('Ctrl Pts',(0.982194060839949,1.73849644461428,
-7.43577161995214));
#133168=CARTESIAN_POINT('Ctrl Pts',(0.909135157054965,1.72693520694186,
-7.44505954502194));
#133169=CARTESIAN_POINT('Ctrl Pts',(0.83584924241827,1.71532338729505,-7.45327820741229));
#133170=CARTESIAN_POINT('Ctrl Pts',(1.35983509,1.845058467,-7.121330531));
#133171=CARTESIAN_POINT('Ctrl Pts',(1.073580856,1.797173233,-7.175991461));
#133172=CARTESIAN_POINT('Ctrl Pts',(0.783862884,1.75,-7.207500189));
#133173=CARTESIAN_POINT('Ctrl Pts',(0.677712097,1.732716033,-7.21904478299999));
#133174=CARTESIAN_POINT('Ctrl Pts',(0.57126737,1.715323387,-7.227458308));
#133175=CARTESIAN_POINT('Ctrl Pts',(1.64756962,1.845058467,-7.316796727));
#133176=CARTESIAN_POINT('Ctrl Pts',(1.353458284,1.797173233,-7.383023646));
#133177=CARTESIAN_POINT('Ctrl Pts',(1.054980228,1.75,-7.425430406));
#133178=CARTESIAN_POINT('Ctrl Pts',(0.945619802999998,1.732716033,-7.440967968));
#133179=CARTESIAN_POINT('Ctrl Pts',(0.835849241000001,1.715323387,-7.453278208));
#133180=CARTESIAN_POINT('',(0.703558300649563,1.71532338778839,-7.3403682584649));
#133181=CARTESIAN_POINT('Ctrl Pts',(0.57126737,1.715323387,-7.227458308));
#133182=CARTESIAN_POINT('Ctrl Pts',(0.180019305,1.779910221,-7.258383046));
#133183=CARTESIAN_POINT('Ctrl Pts',(-0.212280749,1.845052736,-7.246891532));
#133184=CARTESIAN_POINT('Ctrl Pts',(0.34544747,1.715323387,-7.49204017899999));
#133185=CARTESIAN_POINT('Ctrl Pts',(-0.0601233540000001,1.779910221,-7.510740481));
#133186=CARTESIAN_POINT('Ctrl Pts',(-0.465342831,1.845052736,-7.485549816));
#133187=CARTESIAN_POINT('Ctrl Pts',(-0.207598045964949,1.84427517368269,
-7.24702718706223));
#133188=CARTESIAN_POINT('Ctrl Pts',(-0.209001059456788,1.83740483775766,
-7.28860867995657));
#133189=CARTESIAN_POINT('Ctrl Pts',(-0.210425759463398,1.83070798161786,
-7.33024430134279));
#133190=CARTESIAN_POINT('Ctrl Pts',(-0.213311515592232,1.81765000115136,
-7.41351486354743));
#133191=CARTESIAN_POINT('Ctrl Pts',(-0.214774283997516,1.81128114568937,
-7.45519915300969));
#133192=CARTESIAN_POINT('Ctrl Pts',(-0.216253745842921,1.80506741735323,
-7.49688163937647));
#133193=CARTESIAN_POINT('',(0.458357428105106,1.71532338830053,-7.35974924299522));
#133194=CARTESIAN_POINT('Ctrl Pts',(-0.202832658,1.845058467,-7.247162128));
#133195=CARTESIAN_POINT('Ctrl Pts',(-0.494144911,1.797173233,-7.23900891800001));
#133196=CARTESIAN_POINT('Ctrl Pts',(-0.783862884,1.75,-7.207500189));
#133197=CARTESIAN_POINT('Ctrl Pts',(-0.890013671,1.732716033,-7.195955596));
#133198=CARTESIAN_POINT('Ctrl Pts',(-0.995778438,1.715323387,-7.18128994700001));
#133199=CARTESIAN_POINT('Ctrl Pts',(0.036155345,1.845058467,-7.499912852));
#133200=CARTESIAN_POINT('Ctrl Pts',(-0.265316662,1.797173233,-7.501366179));
#133201=CARTESIAN_POINT('Ctrl Pts',(-0.565932667,1.75,-7.478617534));
#133202=CARTESIAN_POINT('Ctrl Pts',(-0.676076422,1.732716033,-7.470282578));
#133203=CARTESIAN_POINT('Ctrl Pts',(-0.785926947,1.715323387,-7.458707585));
#133204=CARTESIAN_POINT('',(-0.890852697336977,1.71532338778839,-7.31999876541133));
#133205=CARTESIAN_POINT('Ctrl Pts',(-0.995778438,1.715323387,-7.181289947));
#133206=CARTESIAN_POINT('Ctrl Pts',(-1.384527244,1.779910221,-7.127384913));
#133207=CARTESIAN_POINT('Ctrl Pts',(-1.765185206,1.845052736,-7.03182915));
#133208=CARTESIAN_POINT('Ctrl Pts',(-1.273196075,1.715323387,-7.391141438));
#133209=CARTESIAN_POINT('Ctrl Pts',(-1.673304891,1.779910221,-7.322218799));
#133210=CARTESIAN_POINT('Ctrl Pts',(-2.063635314,1.845052736,-7.210506868));
#133211=CARTESIAN_POINT('',(-1.27319607194735,1.71532338744859,-7.39114143963449));
#133212=CARTESIAN_POINT('',(-1.82280580273647,1.8050674173212,-7.27512054905735));
#133213=CARTESIAN_POINT('Origin',(0.0571057831376345,1.87497457696,0.181735794365157));
#133214=CARTESIAN_POINT('Ctrl Pts',(-1.76064114318867,1.84427517368998,
-7.03296827585413));
#133215=CARTESIAN_POINT('Ctrl Pts',(-1.77095014927405,1.83740483626804,
-7.07327601879132));
#133216=CARTESIAN_POINT('Ctrl Pts',(-1.78129197126079,1.83070797853862,
-7.11363196432593));
#133217=CARTESIAN_POINT('Ctrl Pts',(-1.8020109648533,1.81765000112568,-7.19433533587172));
#133218=CARTESIAN_POINT('Ctrl Pts',(-1.81240042460075,1.81128114572588,
-7.23473061744994));
#133219=CARTESIAN_POINT('Ctrl Pts',(-1.82280579992674,1.80506741740548,
-7.27512054979416));
#133220=CARTESIAN_POINT('',(-1.13448724847587,1.71532338830053,-7.28621569374938));
#133221=CARTESIAN_POINT('Origin',(-2.75387351811318E-14,1.80614392399994,
-5.09575021068187E-13));
#133222=CARTESIAN_POINT('',(-1.82666476757934,1.6256495872379,-7.27415258434626));
#133223=CARTESIAN_POINT('Origin',(0.0671749039816039,1.48225703765185,0.173520398716352));
#133224=CARTESIAN_POINT('',(-2.37095406541176,1.71532338734599,-7.11537608473305));
#133225=CARTESIAN_POINT('Origin',(0.081987519381812,1.8748529725513,0.165632892873371));
#133226=CARTESIAN_POINT('Ctrl Pts',(-1.82280580495611,1.80506741660434,
-7.27512054836361));
#133227=CARTESIAN_POINT('Ctrl Pts',(-1.93629158428473,1.78658581163235,
-7.24668630654801));
#133228=CARTESIAN_POINT('Ctrl Pts',(-2.04887467011018,1.76822051521175,
-7.21565463296981));
#133229=CARTESIAN_POINT('Ctrl Pts',(-2.16038317911473,1.750000000003,-7.18211281673717));
#133230=CARTESIAN_POINT('Ctrl Pts',(-2.23078427757153,1.73849644464992,
-7.16093613064846));
#133231=CARTESIAN_POINT('Ctrl Pts',(-2.30099064162491,1.72693520694186,
-7.13868898533399));
#133232=CARTESIAN_POINT('Ctrl Pts',(-2.37095406346605,1.71532338729505,
-7.11537608406213));
#133233=CARTESIAN_POINT('Ctrl Pts',(-1.756016176,1.845058467,-7.034124479));
#133234=CARTESIAN_POINT('Ctrl Pts',(-2.038765011,1.797173233,-6.96353836300001));
#133235=CARTESIAN_POINT('Ctrl Pts',(-2.314936093,1.75,-6.870485491));
#133236=CARTESIAN_POINT('Ctrl Pts',(-2.416123388,1.732716033,-6.836391522));
#133237=CARTESIAN_POINT('Ctrl Pts',(-2.516262752,1.715323387,-6.79933245));
#133238=CARTESIAN_POINT('Ctrl Pts',(-1.576949515,1.845058467,-7.332341388));
#133239=CARTESIAN_POINT('Ctrl Pts',(-1.871685696,1.797173233,-7.268953167));
#133240=CARTESIAN_POINT('Ctrl Pts',(-2.160383179,1.75,-7.182112817));
#133241=CARTESIAN_POINT('Ctrl Pts',(-2.266160065,1.732716033,-7.150295076));
#133242=CARTESIAN_POINT('Ctrl Pts',(-2.370954065,1.715323387,-7.115376084));
#133243=CARTESIAN_POINT('',(-2.44360841309735,1.71532338778839,-6.95735426538529));
#133244=CARTESIAN_POINT('Ctrl Pts',(-2.516262752,1.715323387,-6.79933245));
#133245=CARTESIAN_POINT('Ctrl Pts',(-2.884334839,1.779910221,-6.663118183));
#133246=CARTESIAN_POINT('Ctrl Pts',(-3.235551564,1.845052736,-6.487966251));
#133247=CARTESIAN_POINT('Ctrl Pts',(-2.832306387,1.715323387,-6.944641137));
#133248=CARTESIAN_POINT('Ctrl Pts',(-3.208244551,1.779910221,-6.791318303));
#133249=CARTESIAN_POINT('Ctrl Pts',(-3.565434502,1.845052736,-6.598308633));
#133250=CARTESIAN_POINT('',(-2.83230638441011,1.71532338744861,-6.9446411392509));
#133251=CARTESIAN_POINT('',(-3.34412548260674,1.80506741730588,-6.71318290765383));
#133252=CARTESIAN_POINT('Origin',(0.0948385256196937,1.87497459905246,0.165210909860477));
#133253=CARTESIAN_POINT('Ctrl Pts',(-3.23135861816427,1.8442751737878,-6.49005558377446));
#133254=CARTESIAN_POINT('Ctrl Pts',(-3.25009157661077,1.83740483705531,
-6.52720481882866));
#133255=CARTESIAN_POINT('Ctrl Pts',(-3.26886694551241,1.83070798005969,
-6.56439407438189));
#133256=CARTESIAN_POINT('Ctrl Pts',(-3.30645038374621,1.81765000117055,
-6.63875668311628));
#133257=CARTESIAN_POINT('Ctrl Pts',(-3.32528073507912,1.81128114574275,
-6.67597411881968));
#133258=CARTESIAN_POINT('Ctrl Pts',(-3.34412548002259,1.80506741739003,
-6.71318290897665));
#133259=CARTESIAN_POINT('',(-2.67428456193206,1.71532338830053,-6.87198679644513));
#133260=CARTESIAN_POINT('Origin',(5.24103330179493E-13,1.80614392400078,
1.3240276930393E-12));
#133261=CARTESIAN_POINT('',(-3.3476861434657,1.62564958723185,-6.71140801018691));
#133262=CARTESIAN_POINT('Origin',(0.102905981622565,1.48225706127344,0.155022634375567));
#133263=CARTESIAN_POINT('',(-3.84511800556868,1.7153233873472,-6.43933750761235));
#133264=CARTESIAN_POINT('Origin',(0.115677207984717,1.87485304760366,0.144136193360177));
#133265=CARTESIAN_POINT('Ctrl Pts',(-3.34412548462044,1.80506741659049,
-6.71318290649401));
#133266=CARTESIAN_POINT('Ctrl Pts',(-3.44884550812391,1.78658581162302,
-6.66101735348689));
#133267=CARTESIAN_POINT('Ctrl Pts',(-3.55212557167422,1.76822051520746,
-6.60650914783531));
#133268=CARTESIAN_POINT('Ctrl Pts',(-3.65381657476143,1.75000000007832,
-6.54978048744543));
#133269=CARTESIAN_POINT('Ctrl Pts',(-3.71801937267495,1.73849644477304,
-6.51396474497676));
#133270=CARTESIAN_POINT('Ctrl Pts',(-3.78180187253556,1.72693520694185,
-6.4771454331214));
#133271=CARTESIAN_POINT('Ctrl Pts',(-3.84511800351527,1.71532338729505,
-6.43933750739044));
#133272=CARTESIAN_POINT('Ctrl Pts',(-3.22709033,1.845058467,-6.492178987));
#133273=CARTESIAN_POINT('Ctrl Pts',(-3.488054726,1.797173233,-6.362460494));
#133274=CARTESIAN_POINT('Ctrl Pts',(-3.737765465,1.75,-6.212214527));
#133275=CARTESIAN_POINT('Ctrl Pts',(-3.82925786,1.732716033,-6.157165379));
#133276=CARTESIAN_POINT('Ctrl Pts',(-3.919089417,1.715323387,-6.099445724));
#133277=CARTESIAN_POINT('Ctrl Pts',(-3.116317967,1.845058467,-6.82191779));
#133278=CARTESIAN_POINT('Ctrl Pts',(-3.390536786,1.797173233,-6.69665198300001));
#133279=CARTESIAN_POINT('Ctrl Pts',(-3.653816575,1.75,-6.549780488));
#133280=CARTESIAN_POINT('Ctrl Pts',(-3.750280582,1.732716033,-6.495967724));
#133281=CARTESIAN_POINT('Ctrl Pts',(-3.845118005,1.715323387,-6.439337507));
#133282=CARTESIAN_POINT('',(-3.88210371514274,1.71532338778839,-6.26939161293474));
#133283=CARTESIAN_POINT('Ctrl Pts',(-3.919089417,1.715323387,-6.09944572399999));
#133284=CARTESIAN_POINT('Ctrl Pts',(-4.249274143,1.779910221,-5.887291453));
#133285=CARTESIAN_POINT('Ctrl Pts',(-4.554627128,1.845052736,-5.640733261));
#133286=CARTESIAN_POINT('Ctrl Pts',(-4.2589812,1.715323387,-6.173417136));
#133287=CARTESIAN_POINT('Ctrl Pts',(-4.593170261,1.779910221,-5.942863312));
#133288=CARTESIAN_POINT('Ctrl Pts',(-4.900517936,1.845052736,-5.677580819));
#133289=CARTESIAN_POINT('',(-4.25898119793413,1.7153233874486,-6.17341713876038));
#133290=CARTESIAN_POINT('',(-4.70907757189762,1.80506741732327,-5.83734429464129));
#133291=CARTESIAN_POINT('Origin',(0.128136703404839,1.87497456693746,0.140960870615262));
#133292=CARTESIAN_POINT('Ctrl Pts',(-4.55098135569827,1.84427517364945,
-5.6436751063504));
#133293=CARTESIAN_POINT('Ctrl Pts',(-4.57726232901562,1.83740483857874,
-5.67592877290656));
#133294=CARTESIAN_POINT('Ctrl Pts',(-4.60359332343685,1.83070798334266,
-5.7082124060049));
#133295=CARTESIAN_POINT('Ctrl Pts',(-4.65628385777715,1.81765000116681,
-5.77275714641575));
#133296=CARTESIAN_POINT('Ctrl Pts',(-4.68267461446684,1.81128114574686,
-5.80505649027571));
#133297=CARTESIAN_POINT('Ctrl Pts',(-4.70907756966156,1.80506741740742,
-5.837344296486));
#133298=CARTESIAN_POINT('',(-4.08903530174211,1.71532338830053,-6.13643143450315));
#133299=CARTESIAN_POINT('Origin',(6.15393153102772E-13,1.80614392400067,
8.7733639797527E-13));
#133300=CARTESIAN_POINT('',(-4.71217343633271,1.62564958722512,-5.83484545661086));
#133301=CARTESIAN_POINT('Origin',(0.133825473295058,1.48225708072422,0.129276671077776));
#133302=CARTESIAN_POINT('',(-5.13948850268995,1.71532338734785,-5.46220266446694));
#133303=CARTESIAN_POINT('Origin',(0.143957591572755,1.87485301735426,0.115899004336963));
#133304=CARTESIAN_POINT('Ctrl Pts',(-4.70907757360896,1.80506741660989,
-5.83734429307193));
#133305=CARTESIAN_POINT('Ctrl Pts',(-4.80013524921256,1.78658581163547,
-5.76388663229429));
#133306=CARTESIAN_POINT('Ctrl Pts',(-4.88928302912086,1.76822051521265,
-5.68845063738575));
#133307=CARTESIAN_POINT('Ctrl Pts',(-4.97640156834857,1.74999999992805,
-5.61118770152768));
#133308=CARTESIAN_POINT('Ctrl Pts',(-5.03140401600431,1.73849644452739,
-5.56240760784191));
#133309=CARTESIAN_POINT('Ctrl Pts',(-5.08578025209878,1.72693520694185,
-5.51273775897613));
#133310=CARTESIAN_POINT('Ctrl Pts',(-5.13948850063391,1.71532338729505,
-5.46220266470048));
#133311=CARTESIAN_POINT('Ctrl Pts',(-4.54726932600001,1.845058467,-5.646666422));
#133312=CARTESIAN_POINT('Ctrl Pts',(-4.77424687800001,1.797173233,-5.463881043));
#133313=CARTESIAN_POINT('Ctrl Pts',(-4.985821077,1.75,-5.263467316));
#133314=CARTESIAN_POINT('Ctrl Pts',(-5.063340492,1.732716033,-5.190037026));
#133315=CARTESIAN_POINT('Ctrl Pts',(-5.138663817,1.715323387,-5.114355695));
#133316=CARTESIAN_POINT('Ctrl Pts',(-4.509970855,1.845058467,-5.992508897));
#133317=CARTESIAN_POINT('Ctrl Pts',(-4.75085014500001,1.797173233,-5.811222796));
#133318=CARTESIAN_POINT('Ctrl Pts',(-4.976401568,1.75,-5.611187702));
#133319=CARTESIAN_POINT('Ctrl Pts',(-5.059042148,1.732716033,-5.537896141));
#133320=CARTESIAN_POINT('Ctrl Pts',(-5.139488502,1.715323387,-5.462202664));
#133321=CARTESIAN_POINT('',(-5.13907616299444,1.71532338778839,-5.28827917610415));
#133322=CARTESIAN_POINT('Ctrl Pts',(-5.138663817,1.715323387,-5.114355695));
#133323=CARTESIAN_POINT('Ctrl Pts',(-5.41552211,1.779910221,-4.836181517));
#133324=CARTESIAN_POINT('Ctrl Pts',(-5.660733389,1.845052736,-4.529745854));
#133325=CARTESIAN_POINT('Ctrl Pts',(-5.486510786,1.715323387,-5.11353101));
#133326=CARTESIAN_POINT('Ctrl Pts',(-5.763324435,1.779910221,-4.816526637));
#133327=CARTESIAN_POINT('Ctrl Pts',(-6.006458598,1.845052736,-4.491375636));
#133328=CARTESIAN_POINT('',(-5.48651078462152,1.7153233873907,-5.11353101378422));
#133329=CARTESIAN_POINT('',(-5.85383842782573,1.80506741729938,-4.68855794995681));
#133330=CARTESIAN_POINT('Origin',(0.155443364178303,1.87497454573908,0.110119684231014));
#133331=CARTESIAN_POINT('Ctrl Pts',(-5.65780526184909,1.84427517371848,
-4.53340265369336));
#133332=CARTESIAN_POINT('Ctrl Pts',(-5.69040539293009,1.83740483709969,
-4.55925262052202));
#133333=CARTESIAN_POINT('Ctrl Pts',(-5.72306081876345,1.83070798022868,
-4.58512110127154));
#133334=CARTESIAN_POINT('Ctrl Pts',(-5.78839467371819,1.81765000111874,
-4.63682990163741));
#133335=CARTESIAN_POINT('Ctrl Pts',(-5.82111183336738,1.8112811457063,-4.66270087204328));
#133336=CARTESIAN_POINT('Ctrl Pts',(-5.85383842605123,1.80506741738274,
-4.68855795222277));
#133337=CARTESIAN_POINT('',(-5.31258729586815,1.71532338830053,-5.11394335885062));
#133338=CARTESIAN_POINT('Origin',(3.67327696038089E-13,1.80614392400011,
2.68882138776405E-13));
#133339=CARTESIAN_POINT('',(-5.85632473619675,1.6256495871923,-4.68545201434567));
#133340=CARTESIAN_POINT('Origin',(0.158487672707834,1.48225704678402,0.0974859784145793));
#133341=CARTESIAN_POINT('',(-6.19354222877295,1.71532338734701,-4.2296612953197));
#133342=CARTESIAN_POINT('Origin',(0.165506588390246,1.87485294691966,0.082242575767319));
#133343=CARTESIAN_POINT('Ctrl Pts',(-5.85383842914288,1.80506741659236,
-4.68855794806636));
#133344=CARTESIAN_POINT('Ctrl Pts',(-5.9269760013645,1.78658581162182,-4.5972429780145));
#133345=CARTESIAN_POINT('Ctrl Pts',(-5.99782304696224,1.76822051520559,
-4.50440649736151));
#133346=CARTESIAN_POINT('Ctrl Pts',(-6.06629555573099,1.75000000004347,
-4.41022201567403));
#133347=CARTESIAN_POINT('Ctrl Pts',(-6.10952579750693,1.73849644471606,
-4.35075847315401));
#133348=CARTESIAN_POINT('Ctrl Pts',(-6.15195319866596,1.72693520694185,
-4.29056059386023));
#133349=CARTESIAN_POINT('Ctrl Pts',(-6.19354222681643,1.71532338729505,
-4.22966129597777));
#133350=CARTESIAN_POINT('Ctrl Pts',(-5.654823062,1.845058467,-4.53712201));
#133351=CARTESIAN_POINT('Ctrl Pts',(-5.837200552,1.797173233,-4.309816588));
#133352=CARTESIAN_POINT('Ctrl Pts',(-6.000745237,1.75,-4.068606224));
#133353=CARTESIAN_POINT('Ctrl Pts',(-6.06066694900001,1.732716033,-3.98022831));
#133354=CARTESIAN_POINT('Ctrl Pts',(-6.117960008,1.715323387,-3.890124078));
#133355=CARTESIAN_POINT('Ctrl Pts',(-5.692742518,1.845058467,-4.882896949));
#133356=CARTESIAN_POINT('Ctrl Pts',(-5.889019031,1.797173233,-4.654067289));
#133357=CARTESIAN_POINT('Ctrl Pts',(-6.066295556,1.75,-4.410222016));
#133358=CARTESIAN_POINT('Ctrl Pts',(-6.131248525,1.732716033,-4.320878689));
#133359=CARTESIAN_POINT('Ctrl Pts',(-6.193542228,1.715323387,-4.229661295));
#133360=CARTESIAN_POINT('',(-6.15575112068274,1.71532338778839,-4.05989268243235));
#133361=CARTESIAN_POINT('Ctrl Pts',(-6.117960008,1.715323387,-3.890124078));
#133362=CARTESIAN_POINT('Ctrl Pts',(-6.328546282,1.779910221,-3.558937109));
#133363=CARTESIAN_POINT('Ctrl Pts',(-6.502150048,1.845052736,-3.206952564));
#133364=CARTESIAN_POINT('Ctrl Pts',(-6.457497225,1.715323387,-3.814541858));
#133365=CARTESIAN_POINT('Ctrl Pts',(-6.663991964,1.779910221,-3.46497453));
#133366=CARTESIAN_POINT('Ctrl Pts',(-6.83154393200001,1.845052736,-3.095158721));
#133367=CARTESIAN_POINT('',(-6.45749722428321,1.7153233874486,-3.81454186137344));
#133368=CARTESIAN_POINT('',(-6.72488030527665,1.80506741733644,-3.32053984683611));
#133369=CARTESIAN_POINT('Origin',(0.175481749968587,1.87497455746621,0.0741294710234985));
#133370=CARTESIAN_POINT('Ctrl Pts',(-6.5000764830721,1.84427517365532,-3.21115333069245));
#133371=CARTESIAN_POINT('Ctrl Pts',(-6.53747141464812,1.83740483805641,
-3.22939087266828));
#133372=CARTESIAN_POINT('Ctrl Pts',(-6.57492432724293,1.83070798225605,
-3.24763460848772));
#133373=CARTESIAN_POINT('Ctrl Pts',(-6.64984658819208,1.81765000117118,
-3.28408964401682));
#133374=CARTESIAN_POINT('Ctrl Pts',(-6.6873603328519,1.81128114575583,-3.30232254337401));
#133375=CARTESIAN_POINT('Ctrl Pts',(-6.7248803040286,1.80506741742015,-3.3205398494351));
#133376=CARTESIAN_POINT('',(-6.28772861225752,1.71532338830053,-3.85233297492452));
#133377=CARTESIAN_POINT('Origin',(-4.49293380277993E-13,1.80614392399933,
-2.08600497986211E-13));
#133378=CARTESIAN_POINT('',(-6.72664080054466,1.62564958722407,-3.3169720436542));
#133379=CARTESIAN_POINT('Origin',(0.175738525450879,1.48225710692865,0.0611364500891559));
#133380=CARTESIAN_POINT('',(-6.95799280382239,1.71532338734776,-2.79934566613531));
#133381=CARTESIAN_POINT('Origin',(0.179317325664667,1.87485305229205,0.0447409567436702));
#133382=CARTESIAN_POINT('Ctrl Pts',(-6.72488030617135,1.80506741662604,
-3.32053984470728));
#133383=CARTESIAN_POINT('Ctrl Pts',(-6.77667794310486,1.78658581164461,
-3.21563735165099));
#133384=CARTESIAN_POINT('Ctrl Pts',(-6.82591152482656,1.7682205152171,-3.10974131575523));
#133385=CARTESIAN_POINT('Ctrl Pts',(-6.87253630462811,1.75000000004312,
-3.0030392496445));
#133386=CARTESIAN_POINT('Ctrl Pts',(-6.90197294320774,1.7384964447155,-2.9356727075413));
#133387=CARTESIAN_POINT('Ctrl Pts',(-6.93046765080973,1.72693520694185,
-2.86776158452171));
#133388=CARTESIAN_POINT('Ctrl Pts',(-6.95799280205429,1.71532338729505,
-2.79934566720934));
#133389=CARTESIAN_POINT('Ctrl Pts',(-6.497963557,1.845058467,-3.215426816));
#133390=CARTESIAN_POINT('Ctrl Pts',(-6.627213216,1.797173233,-2.954229899));
#133391=CARTESIAN_POINT('Ctrl Pts',(-6.735081219,1.75,-2.683501626));
#133392=CARTESIAN_POINT('Ctrl Pts',(-6.77460335600001,1.732716033,-2.584308542));
#133393=CARTESIAN_POINT('Ctrl Pts',(-6.811187188,1.715323387,-2.483994583));
#133394=CARTESIAN_POINT('Ctrl Pts',(-6.609327869,1.845058467,-3.544966167));
#133395=CARTESIAN_POINT('Ctrl Pts',(-6.75182393300001,1.797173233,-3.279292768));
#133396=CARTESIAN_POINT('Ctrl Pts',(-6.872536305,1.75,-3.00303925));
#133397=CARTESIAN_POINT('Ctrl Pts',(-6.916764535,1.732716033,-2.901821752));
#133398=CARTESIAN_POINT('Ctrl Pts',(-6.957992803,1.715323387,-2.799345666));
#133399=CARTESIAN_POINT('',(-6.88458999724559,1.71532338778839,-2.64167011995074));
#133400=CARTESIAN_POINT('Ctrl Pts',(-6.811187188,1.715323387,-2.483994583));
#133401=CARTESIAN_POINT('Ctrl Pts',(-6.945654664,1.779910221,-2.115280757));
#133402=CARTESIAN_POINT('Ctrl Pts',(-7.039533398,1.845052736,-1.734205737));
#133403=CARTESIAN_POINT('Ctrl Pts',(-7.126538271,1.715323387,-2.337188968));
#133404=CARTESIAN_POINT('Ctrl Pts',(-7.253058636,1.779910221,-1.951404065));
#133405=CARTESIAN_POINT('Ctrl Pts',(-7.337193864,1.845052736,-1.554215624));
#133406=CARTESIAN_POINT('',(-7.12653827101836,1.71532338744859,-2.33718897145734));
#133407=CARTESIAN_POINT('',(-7.28147425196933,1.80506741742003,-1.79725699571591));
#133408=CARTESIAN_POINT('Origin',(0.18731449796178,1.8749745675529,0.0346728987575037));
#133409=CARTESIAN_POINT('Ctrl Pts',(-7.03841135207602,1.84427517370752,
-1.73875404728259));
#133410=CARTESIAN_POINT('Ctrl Pts',(-7.07885255315508,1.8374048364221,-1.74852640324277));
#133411=CARTESIAN_POINT('Ctrl Pts',(-7.1193517128608,1.83070797883412,-1.75829234444339));
#133412=CARTESIAN_POINT('Ctrl Pts',(-7.20035906684401,1.81765000112338,
-1.7777890052515));
#133413=CARTESIAN_POINT('Ctrl Pts',(-7.24091529479374,1.81128114578685,
-1.78753128332844));
#133414=CARTESIAN_POINT('Ctrl Pts',(-7.28147425231075,1.80506741742304,
-1.79725699429402));
#133415=CARTESIAN_POINT('',(-6.96886272684528,1.71532338830053,-2.41059178317464));
#133416=CARTESIAN_POINT('Ctrl Pts',(-7.037266498,1.845058467,-1.743381837));
#133417=CARTESIAN_POINT('Ctrl Pts',(-7.10734475600001,1.797173233,-1.460506703));
#133418=CARTESIAN_POINT('Ctrl Pts',(-7.154492288,1.75,-1.172919475));
#133419=CARTESIAN_POINT('Ctrl Pts',(-7.171766839,1.732716033,-1.067549379));
#133420=CARTESIAN_POINT('Ctrl Pts',(-7.185930826,1.715323387,-0.961716262));
#133421=CARTESIAN_POINT('Ctrl Pts',(-7.216868393,1.845058467,-2.041276707));
#133422=CARTESIAN_POINT('Ctrl Pts',(-7.298921051,1.797173233,-1.751182163));
#133423=CARTESIAN_POINT('Ctrl Pts',(-7.357424895,1.75,-1.455437707));
#133424=CARTESIAN_POINT('Ctrl Pts',(-7.37886032399999,1.732716033,-1.347078855));
#133425=CARTESIAN_POINT('Ctrl Pts',(-7.397095368,1.715323387,-1.238135744));
#133426=CARTESIAN_POINT('',(-7.39709536883243,1.71532338734766,-1.23813574395633));
#133427=CARTESIAN_POINT('Ctrl Pts',(-7.28147425154384,1.80506741796643,
-1.79725699772192));
#133428=CARTESIAN_POINT('Ctrl Pts',(-7.30950995424651,1.78658581254366,
-1.68367210305473));
#133429=CARTESIAN_POINT('Ctrl Pts',(-7.33482796555722,1.7682205156674,-1.5696680900927));
#133430=CARTESIAN_POINT('Ctrl Pts',(-7.35742489468803,1.74999999998162,
-1.45543770641869));
#133431=CARTESIAN_POINT('Ctrl Pts',(-7.3716915062426,1.73849644461496,-1.38331814875904));
#133432=CARTESIAN_POINT('Ctrl Pts',(-7.38492113915213,1.72693520694185,
-1.31086923046406));
#133433=CARTESIAN_POINT('Ctrl Pts',(-7.39709536733612,1.71532338729505,
-1.23813574538403));
#133434=CARTESIAN_POINT('',(-7.29151309772682,1.71532338778839,-1.09992599818185));
#133435=CARTESIAN_POINT('Origin',(-1.04907402209697E-12,1.80614392399972,
-3.31657444563316E-13));
#133436=CARTESIAN_POINT('',(-7.2824266169875,1.62564958719531,-1.79339414632113));
#133437=CARTESIAN_POINT('Origin',(0.184772441701598,1.48225711658612,0.0219285383639398));
#133438=CARTESIAN_POINT('Origin',(0.184742667814161,1.87485301774908,0.00514695786866456));
#133439=CARTESIAN_POINT('Ctrl Pts',(-7.185930826,1.715323387,-0.961716262));
#133440=CARTESIAN_POINT('Ctrl Pts',(-7.237991953,1.779910221,-0.572716228));
#133441=CARTESIAN_POINT('Ctrl Pts',(-7.24775599,1.845052736,-0.180369377));
#133442=CARTESIAN_POINT('Ctrl Pts',(-7.462350308,1.715323387,-0.750551720000001));
#133443=CARTESIAN_POINT('Ctrl Pts',(-7.502980346,1.779910221,-0.346588114));
#133444=CARTESIAN_POINT('Ctrl Pts',(-7.49976476500001,1.845052736,0.059400869));
#133445=CARTESIAN_POINT('',(-7.46235030875524,1.71532338744859,-0.750551723384883));
#133446=CARTESIAN_POINT('',(-7.32414056605716,1.71532338830053,-0.856133999065891));
#133447=CARTESIAN_POINT('',(-7.49759455823745,1.80506741730981,-0.189936395315711));
#133448=CARTESIAN_POINT('Origin',(0.190388983215062,1.87497459522639,-0.00640480722740908));
#133449=CARTESIAN_POINT('Ctrl Pts',(-7.24763792913635,1.84427517364804,
-0.18505255738451));
#133450=CARTESIAN_POINT('Ctrl Pts',(-7.28923440489062,1.83740483639556,
-0.185902778062715));
#133451=CARTESIAN_POINT('Ctrl Pts',(-7.33088610523764,1.83070797884176,
-0.186734274565161));
#133452=CARTESIAN_POINT('Ctrl Pts',(-7.41419075820685,1.81765000112243,
-0.188360927322157));
#133453=CARTESIAN_POINT('Ctrl Pts',(-7.45589310646488,1.81128114570684,
-0.189157046000084));
#133454=CARTESIAN_POINT('Ctrl Pts',(-7.49759455819688,1.80506741739137,
-0.189936398137077));
#133455=CARTESIAN_POINT('Origin',(-8.14452671971111E-13,1.80614392400033,
-4.03052157621486E-14));
#133456=CARTESIAN_POINT('',(-7.49031797585143,1.71532338730065,0.380968029371306));
#133457=CARTESIAN_POINT('Ctrl Pts',(-7.49759455815538,1.80506741661502,
-0.189936393060656));
#133458=CARTESIAN_POINT('Ctrl Pts',(-7.50055740688098,1.78658581163115,
-0.0729802056970346));
#133459=CARTESIAN_POINT('Ctrl Pts',(-7.50077600416531,1.76822051520785,
0.0438010778798551));
#133460=CARTESIAN_POINT('Ctrl Pts',(-7.49828847350378,1.75000000007189,
0.160218486994678));
#133461=CARTESIAN_POINT('Ctrl Pts',(-7.49671796620267,1.73849644476259,
0.233718828343446));
#133462=CARTESIAN_POINT('Ctrl Pts',(-7.49406392199738,1.72693520698401,
0.307317911773481));
#133463=CARTESIAN_POINT('Ctrl Pts',(-7.49031797471166,1.71532338742604,
0.380968027657659));
#133464=CARTESIAN_POINT('',(-7.49769425871342,1.62564958721909,-0.185959132152087));
#133465=CARTESIAN_POINT('Origin',(0.185166703010033,1.48225708291231,-0.0183047507892071));
#133466=CARTESIAN_POINT('Origin',(0.181530033628547,1.87485303207714,-0.0346875888160002));
#133467=CARTESIAN_POINT('Ctrl Pts',(-7.247514679,1.845058467,-0.189818262));
#133468=CARTESIAN_POINT('Ctrl Pts',(-7.25514475400001,1.797173233,0.101508163));
#133469=CARTESIAN_POINT('Ctrl Pts',(-7.23936725,1.75,0.392507087));
#133470=CARTESIAN_POINT('Ctrl Pts',(-7.233586475,1.732716033,0.499127207));
#133471=CARTESIAN_POINT('Ctrl Pts',(-7.224668324,1.715323387,0.605530844));
#133472=CARTESIAN_POINT('Ctrl Pts',(-7.486956173,1.845058467,-0.442139416));
#133473=CARTESIAN_POINT('Ctrl Pts',(-7.504728734,1.797173233,-0.141188225));
#133474=CARTESIAN_POINT('Ctrl Pts',(-7.498288474,1.75,0.160218487));
#133475=CARTESIAN_POINT('Ctrl Pts',(-7.49592880400001,1.732716033,0.270651952));
#133476=CARTESIAN_POINT('Ctrl Pts',(-7.490317975,1.715323387,0.38096803));
#133477=CARTESIAN_POINT('',(-7.35749314923284,1.71532338764623,0.493249440985084));
#133478=CARTESIAN_POINT('Ctrl Pts',(-7.224668324,1.715323387,0.605530843));
#133479=CARTESIAN_POINT('Ctrl Pts',(-7.191888783,1.779910221,0.996627876));
#133480=CARTESIAN_POINT('Ctrl Pts',(-7.117081567,1.845052736,1.381900854));
#133481=CARTESIAN_POINT('Ctrl Pts',(-7.449231138,1.715323387,0.871180493));
#133482=CARTESIAN_POINT('Ctrl Pts',(-7.402071035,1.779910221,1.274433911));
#133483=CARTESIAN_POINT('Ctrl Pts',(-7.311655002,1.845052736,1.670239842));
#133484=CARTESIAN_POINT('',(-7.44923113946963,1.71532338744859,0.871180489875332));
#133485=CARTESIAN_POINT('',(-7.36313567458969,1.8050674173157,1.42626541414909));
#133486=CARTESIAN_POINT('Origin',(0.184560763126078,1.8749745822392,-0.0471830341014413));
#133487=CARTESIAN_POINT('Ctrl Pts',(-7.11797301180835,1.84427517372359,
1.37730178494788));
#133488=CARTESIAN_POINT('Ctrl Pts',(-7.15877975547646,1.83740483677234,
1.38541345408613));
#133489=CARTESIAN_POINT('Ctrl Pts',(-7.19963640712206,1.83070797954891,
1.39355528121711));
#133490=CARTESIAN_POINT('Ctrl Pts',(-7.28134313007023,1.81765000113501,
1.40987469709975));
#133491=CARTESIAN_POINT('Ctrl Pts',(-7.32224164240428,1.81128114574182,
1.41806196319935));
#133492=CARTESIAN_POINT('Ctrl Pts',(-7.3631356751902,1.8050674174027,1.42626541122143));
#133493=CARTESIAN_POINT('',(-7.33694973181313,1.71532338830053,0.738355659920048));
#133494=CARTESIAN_POINT('Origin',(3.1788807697275E-13,1.80614392400006,
-9.44340092234874E-14));
#133495=CARTESIAN_POINT('',(-7.36237804979227,1.62564958720817,1.43017112447915));
#133496=CARTESIAN_POINT('Origin',(0.176902554139877,1.48225709057109,-0.0576821485220025));
#133497=CARTESIAN_POINT('',(-7.23330163873855,1.71532338734751,1.98225816138769));
#133498=CARTESIAN_POINT('Origin',(0.169829105003895,1.87485302319861,-0.0729001907297283));
#133499=CARTESIAN_POINT('Ctrl Pts',(-7.36313567399073,1.80506741657942,
1.42626541646893));
#133500=CARTESIAN_POINT('Ctrl Pts',(-7.3408871297091,1.78658581162416,1.54112415805627));
#133501=CARTESIAN_POINT('Ctrl Pts',(-7.31599609245516,1.76822051521171,
1.65522215227455));
#133502=CARTESIAN_POINT('Ctrl Pts',(-7.28854041727265,1.75000000006627,
1.76838304205611));
#133503=CARTESIAN_POINT('Ctrl Pts',(-7.27120622654293,1.73849644475334,
1.83982737395459));
#133504=CARTESIAN_POINT('Ctrl Pts',(-7.25279260523698,1.72693520694185,
1.91113521043703));
#133505=CARTESIAN_POINT('Ctrl Pts',(-7.23330163797866,1.71532338729505,
1.9822581594651));
#133506=CARTESIAN_POINT('Ctrl Pts',(-7.118877129,1.845058467,1.372621005));
#133507=CARTESIAN_POINT('Ctrl Pts',(-7.063702247,1.797173233,1.65877662));
#133508=CARTESIAN_POINT('Ctrl Pts',(-6.985737446,1.75,1.939580454));
#133509=CARTESIAN_POINT('Ctrl Pts',(-6.957171648,1.732716033,2.042465159));
#133510=CARTESIAN_POINT('Ctrl Pts',(-6.92558836200001,1.715323387,2.144463998));
#133511=CARTESIAN_POINT('Ctrl Pts',(-7.406962203,1.845058467,1.177671822));
#133512=CARTESIAN_POINT('Ctrl Pts',(-7.359623641,1.797173233,1.475407516));
#133513=CARTESIAN_POINT('Ctrl Pts',(-7.288540418,1.75,1.768383042));
#133514=CARTESIAN_POINT('Ctrl Pts',(-7.262495985,1.732716033,1.875727375));
#133515=CARTESIAN_POINT('Ctrl Pts',(-7.23330163800001,1.715323387,1.982258161));
#133516=CARTESIAN_POINT('',(-7.07944499863658,1.71532338778837,2.06336108417793));
#133517=CARTESIAN_POINT('Ctrl Pts',(-6.925588362,1.715323387,2.144463998));
#133518=CARTESIAN_POINT('Ctrl Pts',(-6.809500887,1.779910221,2.519370767));
#133519=CARTESIAN_POINT('Ctrl Pts',(-6.65362032,1.845052736,2.879554937));
#133520=CARTESIAN_POINT('Ctrl Pts',(-7.0877942,1.715323387,2.452177274));
#133521=CARTESIAN_POINT('Ctrl Pts',(-6.955049108,1.779910221,2.835864823));
#133522=CARTESIAN_POINT('Ctrl Pts',(-6.781660377,1.845052736,3.202980258));
#133523=CARTESIAN_POINT('',(-7.08779420210665,1.71532338744858,2.45217727124133));
#133524=CARTESIAN_POINT('',(-6.88438475017486,1.80506741732249,2.97577663915184));
#133525=CARTESIAN_POINT('Origin',(0.170103244568237,1.87497457945223,-0.0857551769196505));
#133526=CARTESIAN_POINT('Ctrl Pts',(-6.65547958725748,1.8442751737515,2.8752550263023));
#133527=CARTESIAN_POINT('Ctrl Pts',(-6.69358851776623,1.83740483771236,
2.89194929058825));
#133528=CARTESIAN_POINT('Ctrl Pts',(-6.73173970549045,1.83070798145379,
2.90868373622113));
#133529=CARTESIAN_POINT('Ctrl Pts',(-6.80802798945147,1.81765000117156,
2.94218614845364));
#133530=CARTESIAN_POINT('Ctrl Pts',(-6.84621029723544,1.81128114574425,
2.95897397223806));
#133531=CARTESIAN_POINT('Ctrl Pts',(-6.88438475134653,1.80506741740601,
2.97577663652078));
#133532=CARTESIAN_POINT('',(-7.00669128353107,1.71532338830053,2.29832062828375));
#133533=CARTESIAN_POINT('Origin',(-1.26634813746307E-13,1.80614392400033,
1.52655665885959E-13));
#133534=CARTESIAN_POINT('',(-6.88280522652421,1.62564958718962,2.97942816863293));
#133535=CARTESIAN_POINT('Origin',(0.160366736514282,1.48225709015059,-0.0943624016382039));
#133536=CARTESIAN_POINT('',(-6.63806415663428,1.71532338734785,3.49086010453999));
#133537=CARTESIAN_POINT('Origin',(0.150187169775896,1.87485301589997,-0.107704045557256));
#133538=CARTESIAN_POINT('Ctrl Pts',(-6.88438474913271,1.80506741661292,
2.97577664120878));
#133539=CARTESIAN_POINT('Ctrl Pts',(-6.83796512925141,1.78658581163562,
3.08316726987123));
#133540=CARTESIAN_POINT('Ctrl Pts',(-6.78912833450483,1.76822051521236,
3.18924687890002));
#133541=CARTESIAN_POINT('Ctrl Pts',(-6.73798831140334,1.75000000001485,
3.29385997111074));
#133542=CARTESIAN_POINT('Ctrl Pts',(-6.70570096511747,1.73849644466928,
3.35990763580892));
#133543=CARTESIAN_POINT('Ctrl Pts',(-6.67238876701024,1.72693520694185,
3.42558995016916));
#133544=CARTESIAN_POINT('Ctrl Pts',(-6.63806415630943,1.71532338729505,
3.49086010249632));
#133545=CARTESIAN_POINT('Ctrl Pts',(-6.657368796,1.845058467,2.870878039));
#133546=CARTESIAN_POINT('Ctrl Pts',(-6.541968873,1.797173233,3.138482526));
#133547=CARTESIAN_POINT('Ctrl Pts',(-6.405462322,1.75,3.395961195));
#133548=CARTESIAN_POINT('Ctrl Pts',(-6.355447207,1.732716033,3.49029971));
#133549=CARTESIAN_POINT('Ctrl Pts',(-6.302675585,1.715323387,3.583124401));
#133550=CARTESIAN_POINT('Ctrl Pts',(-6.980626913,1.845058467,2.742416435));
#133551=CARTESIAN_POINT('Ctrl Pts',(-6.87039072700001,1.797173233,3.023014843));
#133552=CARTESIAN_POINT('Ctrl Pts',(-6.737988312,1.75,3.293859971));
#133553=CARTESIAN_POINT('Ctrl Pts',(-6.689476925,1.732716033,3.39309587));
#133554=CARTESIAN_POINT('Ctrl Pts',(-6.638064156,1.715323387,3.490860104));
#133555=CARTESIAN_POINT('',(-6.47036986816281,1.71532338778839,3.53699225677551));
#133556=CARTESIAN_POINT('Ctrl Pts',(-6.30267558499999,1.715323387,3.583124401));
#133557=CARTESIAN_POINT('Ctrl Pts',(-6.108708297,1.779910221,3.924310682));
#133558=CARTESIAN_POINT('Ctrl Pts',(-5.879043182,1.845052736,4.242564232));
#133559=CARTESIAN_POINT('Ctrl Pts',(-6.394939882,1.715323387,3.918512972));
#133560=CARTESIAN_POINT('Ctrl Pts',(-6.182816816,1.779910221,4.264693848));
#133561=CARTESIAN_POINT('Ctrl Pts',(-5.93456285000001,1.845052736,4.585952876));
#133562=CARTESIAN_POINT('',(-6.39493988465156,1.71532338744858,3.9185129697532));
#133563=CARTESIAN_POINT('',(-6.08372764672891,1.80506741727164,4.386143855119));
#133564=CARTESIAN_POINT('Origin',(0.147691334341582,1.8749745505013,-0.120317322450024));
#133565=CARTESIAN_POINT('Ctrl Pts',(-5.88178333421817,1.84427517375015,
4.23876453771839));
#133566=CARTESIAN_POINT('Ctrl Pts',(-5.9154125277128,1.83740483730708,4.26326079454293));
#133567=CARTESIAN_POINT('Ctrl Pts',(-5.94907435305998,1.83070798061871,
4.2878053775091));
#133568=CARTESIAN_POINT('Ctrl Pts',(-6.01637702711119,1.81765000111501,
4.33692424505133));
#133569=CARTESIAN_POINT('Ctrl Pts',(-6.050057767914,1.81128114569571,4.36152764629411));
#133570=CARTESIAN_POINT('Ctrl Pts',(-6.08372764844526,1.80506741735516,
4.38614385279247));
#133571=CARTESIAN_POINT('',(-6.34880773763066,1.71532338830053,3.75081867950825));
#133572=CARTESIAN_POINT('Origin',(-1.50487261540988E-13,1.80614392399994,
-3.46944695195361E-15));
#133573=CARTESIAN_POINT('',(-6.08140007977468,1.6256495872305,4.38937046332154));
#133574=CARTESIAN_POINT('Origin',(0.13633236409473,1.48225708328908,-0.126630402607792));
#133575=CARTESIAN_POINT('',(-5.73243817153204,1.71532338734572,4.83623330865244));
#133576=CARTESIAN_POINT('Origin',(0.123522468779412,1.87485301057633,-0.137471620468915));
#133577=CARTESIAN_POINT('Ctrl Pts',(-6.08372764527108,1.80506741655844,
4.38614385691246));
#133578=CARTESIAN_POINT('Ctrl Pts',(-6.0153074796744,1.7865858116006,4.48104490613826));
#133579=CARTESIAN_POINT('Ctrl Pts',(-5.94480848178056,1.76822051519547,
4.57414596570128));
#133580=CARTESIAN_POINT('Ctrl Pts',(-5.87237536131294,1.75000000001473,
4.66531966898703));
#133581=CARTESIAN_POINT('Ctrl Pts',(-5.8266445793839,1.73849644466908,4.72288235120746));
#133582=CARTESIAN_POINT('Ctrl Pts',(-5.77999144574739,1.72693520694185,
4.77986791146979));
#133583=CARTESIAN_POINT('Ctrl Pts',(-5.73243817162547,1.71532338729505,
4.83623330659798));
#133584=CARTESIAN_POINT('Ctrl Pts',(-5.884569297,1.845058467,4.234896006));
#133585=CARTESIAN_POINT('Ctrl Pts',(-5.714340306,1.797173233,4.471436477));
#133586=CARTESIAN_POINT('Ctrl Pts',(-5.5256749,1.75,4.693550565));
#133587=CARTESIAN_POINT('Ctrl Pts',(-5.456549118,1.732716033,4.774931727));
#133588=CARTESIAN_POINT('Ctrl Pts',(-5.385056702,1.715323387,4.854241888));
#133589=CARTESIAN_POINT('Ctrl Pts',(-6.227885267,1.845058467,4.178928703));
#133590=CARTESIAN_POINT('Ctrl Pts',(-6.05990597900001,1.797173233,4.429269354));
#133591=CARTESIAN_POINT('Ctrl Pts',(-5.872375362,1.75,4.665319669));
#133592=CARTESIAN_POINT('Ctrl Pts',(-5.803665359,1.732716033,4.751806974));
#133593=CARTESIAN_POINT('Ctrl Pts',(-5.732438171,1.715323387,4.836233308));
#133594=CARTESIAN_POINT('',(-5.55874743329838,1.71532338778837,4.84523760167309));
#133595=CARTESIAN_POINT('Ctrl Pts',(-5.385056702,1.715323387,4.854241888));
#133596=CARTESIAN_POINT('Ctrl Pts',(-5.122279297,1.779910221,5.145754191));
#133597=CARTESIAN_POINT('Ctrl Pts',(-4.829568519,1.845052736,5.407195939));
#133598=CARTESIAN_POINT('Ctrl Pts',(-5.403065283,1.715323387,5.201623357));
#133599=CARTESIAN_POINT('Ctrl Pts',(-5.121482881,1.779910221,5.494110528));
#133600=CARTESIAN_POINT('Ctrl Pts',(-4.80997176,1.845052736,5.754491434));
#133601=CARTESIAN_POINT('',(-5.40306528606363,1.71532338744859,5.2016233553958));
#133602=CARTESIAN_POINT('',(-4.99860219952518,1.80506741735075,5.59141985937217));
#133603=CARTESIAN_POINT('Origin',(0.118373688949022,1.87497455816666,-0.149253604198235));
#133604=CARTESIAN_POINT('Ctrl Pts',(-4.83306143014279,1.84427517370204,
5.40407413113599));
#133605=CARTESIAN_POINT('Ctrl Pts',(-4.86063842297015,1.83740483668169,
5.4352269642911));
#133606=CARTESIAN_POINT('Ctrl Pts',(-4.88823689644891,1.83070797937978,
5.46643400908832));
#133607=CARTESIAN_POINT('Ctrl Pts',(-4.94340696136198,1.81765000116022,
5.52887258420017));
#133608=CARTESIAN_POINT('Ctrl Pts',(-4.97101126108887,1.81128114575866,
5.5601411352121));
#133609=CARTESIAN_POINT('Ctrl Pts',(-4.9986022017135,1.80506741743534,5.59141985745866));
#133610=CARTESIAN_POINT('',(-5.39406099803711,1.71532338830053,5.02793261655969));
#133611=CARTESIAN_POINT('Origin',(7.46364775539021E-13,1.80614392399945,
-7.6588041464376E-13));
#133612=CARTESIAN_POINT('',(-4.99563542483045,1.62564958722827,5.59407067324546));
#133613=CARTESIAN_POINT('Origin',(0.105923124203066,1.48225704987208,-0.152977207608697));
#133614=CARTESIAN_POINT('',(-4.55876974925633,1.715323387357,5.95546961878356));
#133615=CARTESIAN_POINT('Origin',(0.0910824517940872,1.87485302966038,-0.160811540123007));
#133616=CARTESIAN_POINT('Ctrl Pts',(-4.99860219769392,1.80506741663509,
5.59141986081333));
#133617=CARTESIAN_POINT('Ctrl Pts',(-4.91138073706177,1.78658581165296,
5.66939386310148));
#133618=CARTESIAN_POINT('Ctrl Pts',(-4.82251599075879,1.76822051522225,
5.74516307094973));
#133619=CARTESIAN_POINT('Ctrl Pts',(-4.73217666580145,1.75000000003504,
5.81863420380799));
#133620=CARTESIAN_POINT('Ctrl Pts',(-4.67514077019381,1.73849644470229,
5.86502033598252));
#133621=CARTESIAN_POINT('Ctrl Pts',(-4.6173281493075,1.72693520694185,5.91064456103527));
#133622=CARTESIAN_POINT('Ctrl Pts',(-4.55876974991222,1.71532338729505,
5.95546961676522));
#133623=CARTESIAN_POINT('Ctrl Pts',(-4.836613879,1.845058467,5.400894943));
#133624=CARTESIAN_POINT('Ctrl Pts',(-4.619515538,1.797173233,5.59531102800001));
#133625=CARTESIAN_POINT('Ctrl Pts',(-4.38751306,1.75,5.771674726));
#133626=CARTESIAN_POINT('Ctrl Pts',(-4.302508856,1.732716033,5.836293242));
#133627=CARTESIAN_POINT('Ctrl Pts',(-4.215638554,1.715323387,5.898380421));
#133628=CARTESIAN_POINT('Ctrl Pts',(-5.183934627,1.845058467,5.42003891));
#133629=CARTESIAN_POINT('Ctrl Pts',(-4.966066761,1.797173233,5.62841615400001));
#133630=CARTESIAN_POINT('Ctrl Pts',(-4.732176666,1.75,5.818634204));
#133631=CARTESIAN_POINT('Ctrl Pts',(-4.646480852,1.732716033,5.888328864));
#133632=CARTESIAN_POINT('Ctrl Pts',(-4.558769749,1.715323387,5.95546961800001));
#133633=CARTESIAN_POINT('',(-4.38720414758359,1.71532338778839,5.92692502239899));
#133634=CARTESIAN_POINT('Ctrl Pts',(-4.215638554,1.715323387,5.898380421));
#133635=CARTESIAN_POINT('Ctrl Pts',(-3.89633821,1.779910221,6.126587953));
#133636=CARTESIAN_POINT('Ctrl Pts',(-3.554268599,1.845052736,6.318993173));
#133637=CARTESIAN_POINT('Ctrl Pts',(-4.158549356,1.715323387,6.241511616));
#133638=CARTESIAN_POINT('Ctrl Pts',(-3.820674098,1.779910221,6.466628707));
#133639=CARTESIAN_POINT('Ctrl Pts',(-3.460471736,1.845052736,6.653956369));
#133640=CARTESIAN_POINT('',(-4.15854935933182,1.71532338744847,6.24151161509755));
#133641=CARTESIAN_POINT('',(-3.6797476691896,1.80506741728958,6.53524728577702));
#133642=CARTESIAN_POINT('Origin',(0.0835210239221201,1.87497457238564,-0.17121091276438));
#133643=CARTESIAN_POINT('Ctrl Pts',(-3.55835094392698,1.84427517370894,
6.31669522493168));
#133644=CARTESIAN_POINT('Ctrl Pts',(-3.57858625937572,1.83740483824043,
6.35304795193762));
#133645=CARTESIAN_POINT('Ctrl Pts',(-3.59883089848952,1.8307079825938,6.38945823950481));
#133646=CARTESIAN_POINT('Ctrl Pts',(-3.63928868009485,1.81765000115139,
6.46229698630404));
#133647=CARTESIAN_POINT('Ctrl Pts',(-3.659525792586,1.81128114571434,6.4987686045792));
#133648=CARTESIAN_POINT('Ctrl Pts',(-3.6797476716983,1.80506741737228,6.53524728440042));
#133649=CARTESIAN_POINT('',(-4.18709396168286,1.71532338830019,6.06994601389012));
#133650=CARTESIAN_POINT('Origin',(1.49403059368503E-13,1.8061439239995,
-3.35235311732518E-13));
#133651=CARTESIAN_POINT('',(-3.67628040958788,1.62564958722685,6.53719835590227));
#133652=CARTESIAN_POINT('Origin',(0.0705612289384649,1.48225705527937,-0.172171196500804));
#133653=CARTESIAN_POINT('',(-3.17193832019193,1.71532338734682,6.79623478881418));
#133654=CARTESIAN_POINT('Origin',(0.0543832873494848,1.87485296704309,-0.176631898520114));
#133655=CARTESIAN_POINT('Ctrl Pts',(-3.67974766713166,1.80506741658449,
6.53524728677746));
#133656=CARTESIAN_POINT('Ctrl Pts',(-3.57780329029907,1.78658581161492,
6.59264826446448));
#133657=CARTESIAN_POINT('Ctrl Pts',(-3.47472801243772,1.76822051520117,
6.64754273669236));
#133658=CARTESIAN_POINT('Ctrl Pts',(-3.37070664861048,1.74999999999575,
6.69987587087804));
#133659=CARTESIAN_POINT('Ctrl Pts',(-3.30503257263167,1.73849644463805,
6.73291648972614));
#133660=CARTESIAN_POINT('Ctrl Pts',(-3.23876371927812,1.72693520694185,
6.76504604108847));
#133661=CARTESIAN_POINT('Ctrl Pts',(-3.17193832115523,1.71532338729505,
6.79623478698976));
#133662=CARTESIAN_POINT('Ctrl Pts',(-3.56250377,1.845058467,6.314354036));
#133663=CARTESIAN_POINT('Ctrl Pts',(-3.308687357,1.797173233,6.457555054));
#133664=CARTESIAN_POINT('Ctrl Pts',(-3.044195986,1.75,6.579921793));
#133665=CARTESIAN_POINT('Ctrl Pts',(-2.947288063,1.732716033,6.62475617200001));
#133666=CARTESIAN_POINT('Ctrl Pts',(-2.849101831,1.715323387,6.66671724));
#133667=CARTESIAN_POINT('Ctrl Pts',(-3.897588966,1.845058467,6.40771412100001));
#133668=CARTESIAN_POINT('Ctrl Pts',(-3.640019782,1.797173233,6.56438447000001));
#133669=CARTESIAN_POINT('Ctrl Pts',(-3.370706649,1.75,6.699875871));
#133670=CARTESIAN_POINT('Ctrl Pts',(-3.272032063,1.732716033,6.74951904200001));
#133671=CARTESIAN_POINT('Ctrl Pts',(-3.17193832,1.715323387,6.796234788));
#133672=CARTESIAN_POINT('',(-3.01052007105196,1.71532338778838,6.7314760159893));
#133673=CARTESIAN_POINT('Ctrl Pts',(-2.849101831,1.715323387,6.66671724));
#133674=CARTESIAN_POINT('Ctrl Pts',(-2.488208678,1.779910221,6.820949271));
#133675=CARTESIAN_POINT('Ctrl Pts',(-2.11277503,1.845052736,6.93532131));
#133676=CARTESIAN_POINT('Ctrl Pts',(-2.719584283,1.715323387,6.989553729));
#133677=CARTESIAN_POINT('Ctrl Pts',(-2.341214841,1.779910221,7.136774514));
#133678=CARTESIAN_POINT('Ctrl Pts',(-1.949163901,1.845052736,7.242289699));
#133679=CARTESIAN_POINT('',(-2.71958428645445,1.71532338744809,6.98955372882641));
#133680=CARTESIAN_POINT('',(-2.1888322280156,1.80506741730229,7.17349381209083));
#133681=CARTESIAN_POINT('Origin',(0.0447630880302707,1.87497458410537,-0.185162737521352));
#133682=CARTESIAN_POINT('Ctrl Pts',(-2.11725592328195,1.84427517370612,
6.93395466941367));
#133683=CARTESIAN_POINT('Ctrl Pts',(-2.12920338796688,1.83740483743912,
6.9738074892125));
#133684=CARTESIAN_POINT('Ctrl Pts',(-2.14114758477622,1.83070798093934,
7.01371852897689));
#133685=CARTESIAN_POINT('Ctrl Pts',(-2.16500130557034,1.81765000112972,
7.0935515635659));
#133686=CARTESIAN_POINT('Ctrl Pts',(-2.17692496579604,1.81128114571579,
7.1335208765333));
#133687=CARTESIAN_POINT('Ctrl Pts',(-2.18883223079566,1.80506741738623,
7.17349381127575));
#133688=CARTESIAN_POINT('',(-2.78434306451125,1.71532338829908,6.8281354814371));
#133689=CARTESIAN_POINT('Origin',(1.44632569809566E-13,1.8061439240005,
-3.90746462963776E-13));
#133690=CARTESIAN_POINT('',(-2.18502660827602,1.62564958721219,7.17465390913889));
#133691=CARTESIAN_POINT('Origin',(0.0318997603712604,1.48225709287231,-0.183314302122269));
#133692=CARTESIAN_POINT('',(-1.63679058102413,1.71532338734606,7.31921557284011));
#133693=CARTESIAN_POINT('Origin',(0.0151411834314741,1.8748529928791,-0.184193113374613));
#133694=CARTESIAN_POINT('Ctrl Pts',(-2.18883222576068,1.80506741658859,
7.17349381263113));
#133695=CARTESIAN_POINT('Ctrl Pts',(-2.07693173832936,1.78658581162109,
7.20763775979279));
#133696=CARTESIAN_POINT('Ctrl Pts',(-1.96446561443443,1.76822051520548,
7.23909069180446));
#133697=CARTESIAN_POINT('Ctrl Pts',(-1.85162613527359,1.749999999943,7.26783878785127));
#133698=CARTESIAN_POINT('Ctrl Pts',(-1.78038472563909,1.73849644455183,
7.28598895035891));
#133699=CARTESIAN_POINT('Ctrl Pts',(-1.70875829796959,1.72693520694185,
7.30312148604251));
#133700=CARTESIAN_POINT('Ctrl Pts',(-1.63679058234637,1.71532338729505,
7.3192155712624));
#133701=CARTESIAN_POINT('Ctrl Pts',(-2.121814945,1.845058467,6.932560951));
#133702=CARTESIAN_POINT('Ctrl Pts',(-1.843148632,1.797173233,7.01785098300001));
#133703=CARTESIAN_POINT('Ctrl Pts',(-1.558535692,1.75,7.080499029));
#133704=CARTESIAN_POINT('Ctrl Pts',(-1.454255355,1.732716033,7.103452867));
#133705=CARTESIAN_POINT('Ctrl Pts',(-1.349344274,1.715323387,7.12332577));
#133706=CARTESIAN_POINT('Ctrl Pts',(-2.428996377,1.845058467,7.095771741));
#133707=CARTESIAN_POINT('Ctrl Pts',(-2.143769523,1.797173233,7.193409464));
#133708=CARTESIAN_POINT('Ctrl Pts',(-1.851626136,1.75,7.267838788));
#133709=CARTESIAN_POINT('Ctrl Pts',(-1.744586692,1.732716033,7.29510921));
#133710=CARTESIAN_POINT('Ctrl Pts',(-1.636790581,1.715323387,7.319215572));
#133711=CARTESIAN_POINT('',(-1.49306742272831,1.71532338778839,7.2212706719866));
#133712=CARTESIAN_POINT('Ctrl Pts',(-1.349344274,1.715323387,7.12332577));
#133713=CARTESIAN_POINT('Ctrl Pts',(-0.963733275,1.779910221,7.196370583));
#133714=CARTESIAN_POINT('Ctrl Pts',(-0.572490449,1.845052736,7.22736153));
#133715=CARTESIAN_POINT('Ctrl Pts',(-1.153454472,1.715323387,7.41077207700001));
#133716=CARTESIAN_POINT('Ctrl Pts',(-0.75228298,1.779910221,7.473212677));
#133717=CARTESIAN_POINT('Ctrl Pts',(-0.346715327,1.845052736,7.491981613));
#133718=CARTESIAN_POINT('',(-1.15345447538118,1.71532338744759,7.41077207758618));
#133719=CARTESIAN_POINT('',(-0.595569424149683,1.80506741729189,7.4763157408475));
#133720=CARTESIAN_POINT('Origin',(0.00391204345537494,1.87497458607747,
-0.190456472670194));
#133721=CARTESIAN_POINT('Ctrl Pts',(-0.577160368713407,1.84427517375144,
7.22699010014981));
#133722=CARTESIAN_POINT('Ctrl Pts',(-0.58026133036698,1.83740483693944,
7.26847953832023));
#133723=CARTESIAN_POINT('Ctrl Pts',(-0.583346585006129,1.83070797985232,
7.31002513333623));
#133724=CARTESIAN_POINT('Ctrl Pts',(-0.589480875960759,1.81765000113372,
7.39311955382139));
#133725=CARTESIAN_POINT('Ctrl Pts',(-0.592533546807837,1.81128114573694,
7.43471764077701));
#133726=CARTESIAN_POINT('Ctrl Pts',(-0.595569427165579,1.80506741737982,
7.47631574064053));
#133727=CARTESIAN_POINT('',(-1.25139938098489,1.71532338829759,7.26704892212499));
#133728=CARTESIAN_POINT('Origin',(4.1165801236559E-16,1.80614392399939,
-6.8434841127285E-13));
#133729=CARTESIAN_POINT('',(-0.591603391254012,1.62564958716999,7.47663061959824));
#133730=CARTESIAN_POINT('Origin',(-0.00825319872770208,1.48225709597672,
-0.185885931764933));
#133731=CARTESIAN_POINT('',(-0.0251083328437023,1.715323387346,7.49995797182605));
#133732=CARTESIAN_POINT('Origin',(-0.0248088887949483,1.87485302402727,
-0.183141684585254));
#133733=CARTESIAN_POINT('Ctrl Pts',(-0.595569421727552,1.80506741654646,
7.47631574089619));
#133734=CARTESIAN_POINT('Ctrl Pts',(-0.478945166287782,1.78658581160554,
7.4856061244765));
#133735=CARTESIAN_POINT('Ctrl Pts',(-0.362346987204218,1.76822051520377,
7.49214681237726));
#133736=CARTESIAN_POINT('Ctrl Pts',(-0.24596564175084,1.75000000004052,
7.49596564148352));
#133737=CARTESIAN_POINT('Ctrl Pts',(-0.17248806913491,1.73849644471125,
7.49837666576198));
#133738=CARTESIAN_POINT('Ctrl Pts',(-0.0988532380978183,1.72693520694185,
7.49971108777194));
#133739=CARTESIAN_POINT('Ctrl Pts',(-0.0251083344734459,1.71532338729505,
7.49995797056906));
#133740=CARTESIAN_POINT('Ctrl Pts',(-0.581912411,1.845058467,7.226609021));
#133741=CARTESIAN_POINT('Ctrl Pts',(-0.291426326,1.797173233,7.25));
#133742=CARTESIAN_POINT('Ctrl Pts',(0.,1.75,7.25));
#133743=CARTESIAN_POINT('Ctrl Pts',(0.106776717,1.732716033,7.25));
#133744=CARTESIAN_POINT('Ctrl Pts',(0.213507122,1.715323387,7.246855505));
#133745=CARTESIAN_POINT('Ctrl Pts',(-0.846826616,1.845058467,7.452038961));
#133746=CARTESIAN_POINT('Ctrl Pts',(-0.547278984,1.797173233,7.48607862600001));
#133747=CARTESIAN_POINT('Ctrl Pts',(-0.245965642,1.75,7.495965642));
#133748=CARTESIAN_POINT('Ctrl Pts',(-0.135566387,1.732716033,7.49958818));
#133749=CARTESIAN_POINT('Ctrl Pts',(-0.025108333,1.715323387,7.499957971));
#133750=CARTESIAN_POINT('',(0.094199399372222,1.71532338778839,7.37340673793776));
#133751=CARTESIAN_POINT('Ctrl Pts',(-1.648780528,4.042023177,7.316523954));
#133752=CARTESIAN_POINT('Ctrl Pts',(-1.249332754,4.10772842,7.406539611));
#133753=CARTESIAN_POINT('Ctrl Pts',(-0.842459476,4.172899507,7.452533934));
#133754=CARTESIAN_POINT('Ctrl Pts',(-1.361013652,4.042023177,7.12110538));
#133755=CARTESIAN_POINT('Ctrl Pts',(-0.972234813,4.10772842,7.19541032));
#133756=CARTESIAN_POINT('Ctrl Pts',(-0.577677420999999,4.172899507,7.226948789));
#133757=CARTESIAN_POINT('',(-0.84245946624551,4.17289950600422,7.45253393658569));
#133758=CARTESIAN_POINT('',(-0.710068431037417,4.17289950413623,7.33974136318938));
#133759=CARTESIAN_POINT('',(-1.40346520264162,4.08221031165715,7.36751555261981));
#133760=CARTESIAN_POINT('Origin',(0.045787793001877,4.01787921770315,-0.185145958812898));
#133761=CARTESIAN_POINT('Ctrl Pts',(-1.35637331540347,4.0428073592789,7.12199069258409));
#133762=CARTESIAN_POINT('Ctrl Pts',(-1.36425141320857,4.04969801218673,
7.16284458526961));
#133763=CARTESIAN_POINT('Ctrl Pts',(-1.37211768790064,4.05642175344562,
7.20375431976348));
#133764=CARTESIAN_POINT('Ctrl Pts',(-1.38781116925284,4.0695455071114,7.28558294300322));
#133765=CARTESIAN_POINT('Ctrl Pts',(-1.39564719791905,4.07595289336076,
7.32654784736749));
#133766=CARTESIAN_POINT('Ctrl Pts',(-1.40346520397192,4.08221031165702,
7.36751555236596));
#133767=CARTESIAN_POINT('Ctrl Pts',(-1.954361232,4.172899507,7.240888908));
#133768=CARTESIAN_POINT('Ctrl Pts',(-1.55978046,4.107307013,7.347388728));
#133769=CARTESIAN_POINT('Ctrl Pts',(-1.155963477,4.04203077,7.410381126));
#133770=CARTESIAN_POINT('Ctrl Pts',(-2.117752007,4.172899507,6.933803173));
#133771=CARTESIAN_POINT('Ctrl Pts',(-1.739905385,4.107307013,7.049206714));
#133772=CARTESIAN_POINT('Ctrl Pts',(-1.351755947,4.04203077,7.122868513));
#133773=CARTESIAN_POINT('',(-1.95436122762896,4.17289950692266,7.24088891073579));
#133774=CARTESIAN_POINT('Origin',(0.0483827730459563,4.16071411101886,-0.186743460649631));
#133775=CARTESIAN_POINT('',(-2.03605662078521,4.17289950678353,7.08734604013078));
#133776=CARTESIAN_POINT('Origin',(6.59737021957429E-14,4.26419218499978,
-5.49039980146659E-13));
#133777=CARTESIAN_POINT('',(-1.39881673462662,4.26310680662278,7.36839953685386));
#133778=CARTESIAN_POINT('Origin',(0.0196658883634099,4.16071717757456,-0.19146588038788));
#133779=CARTESIAN_POINT('Origin',(0.0716636017910904,4.01799492241726,-0.170731827707776));
#133780=CARTESIAN_POINT('Ctrl Pts',(-3.183069331,4.042023177,6.791028614));
#133781=CARTESIAN_POINT('Ctrl Pts',(-2.812311129,4.10772842,6.964809219));
#133782=CARTESIAN_POINT('Ctrl Pts',(-2.424837742,4.172899507,7.09719394700001));
#133783=CARTESIAN_POINT('Ctrl Pts',(-2.860021067,4.042023177,6.66204019));
#133784=CARTESIAN_POINT('Ctrl Pts',(-2.496305027,4.10772842,6.81818388));
#133785=CARTESIAN_POINT('Ctrl Pts',(-2.117752007,4.172899507,6.933803173));
#133786=CARTESIAN_POINT('',(-2.42483773306114,4.17289950600422,7.09719395161998));
#133787=CARTESIAN_POINT('',(-2.27129485780885,4.17289950413623,7.01549856540382));
#133788=CARTESIAN_POINT('',(-2.95445102732462,4.08221031165033,6.89356360063074));
#133789=CARTESIAN_POINT('Origin',(0.0845180867257572,4.01787922293851,-0.170974027477583));
#133790=CARTESIAN_POINT('Ctrl Pts',(-2.85567953540613,4.04280735926973,
6.66390233981684));
#133791=CARTESIAN_POINT('Ctrl Pts',(-2.87215582770793,4.04969801251677,
6.7021075347925));
#133792=CARTESIAN_POINT('Ctrl Pts',(-2.88863257781732,4.05642175415592,
6.74036980808426));
#133793=CARTESIAN_POINT('Ctrl Pts',(-2.92154988751123,4.06954550710655,
6.81691168458022));
#133794=CARTESIAN_POINT('Ctrl Pts',(-2.93800895763356,4.07595289335613,
6.85523433760006));
#133795=CARTESIAN_POINT('Ctrl Pts',(-2.95445102856625,4.08221031165021,
6.89356360009814));
#133796=CARTESIAN_POINT('Ctrl Pts',(-3.465246429,4.172899507,6.651471054));
#133797=CARTESIAN_POINT('Ctrl Pts',(-3.102785048,4.107307013,6.84030417));
#133798=CARTESIAN_POINT('Ctrl Pts',(-2.721950586,4.04203077,6.988632556));
#133799=CARTESIAN_POINT('Ctrl Pts',(-3.558802862,4.172899507,6.316440627));
#133800=CARTESIAN_POINT('Ctrl Pts',(-3.214598434,4.107307013,6.510371952));
#133801=CARTESIAN_POINT('Ctrl Pts',(-2.851358824,4.04203077,6.665752235));
#133802=CARTESIAN_POINT('',(-3.46524642532133,4.17289950685238,6.65147105763285));
#133803=CARTESIAN_POINT('Origin',(0.0873959770846583,4.16071398744577,-0.171976766965011));
#133804=CARTESIAN_POINT('',(-3.5120246466758,4.17289950678353,6.48395583986313));
#133805=CARTESIAN_POINT('Origin',(-4.71411104596697E-13,4.26419218499956,
8.28330459778925E-13));
#133806=CARTESIAN_POINT('',(-2.95010126897283,4.26310680661376,6.89542620135548));
#133807=CARTESIAN_POINT('Origin',(0.0603656250039425,4.16071714725873,-0.182762002467465));
#133808=CARTESIAN_POINT('Origin',(0.106690365472132,4.01799501511567,-0.151334504317661));
#133809=CARTESIAN_POINT('Ctrl Pts',(-4.568521349,4.042023177,5.947992324));
#133810=CARTESIAN_POINT('Ctrl Pts',(-4.243788962,4.10772842,6.197412088));
#133811=CARTESIAN_POINT('Ctrl Pts',(-3.89383329,4.172899507,6.40999706));
#133812=CARTESIAN_POINT('Ctrl Pts',(-4.225297077,4.042023177,5.891465405));
#133813=CARTESIAN_POINT('Ctrl Pts',(-3.903650793,4.10772842,6.122146739));
#133814=CARTESIAN_POINT('Ctrl Pts',(-3.558802862,4.172899507,6.31644062700001));
#133815=CARTESIAN_POINT('',(-3.89383328225289,4.17289950600423,6.40999706643631));
#133816=CARTESIAN_POINT('',(-3.72631806086074,4.17289950413623,6.36321885236559));
#133817=CARTESIAN_POINT('',(-4.36729000625335,4.0822103116468,6.0972762766455));
#133818=CARTESIAN_POINT('Origin',(0.119296556422939,4.01787916433398,-0.148807985082576));
#133819=CARTESIAN_POINT('Ctrl Pts',(-4.22145735396844,4.04280735933467,
5.89421731982391));
#133820=CARTESIAN_POINT('Ctrl Pts',(-4.24576142183867,4.04969801097169,
5.92798737493316));
#133821=CARTESIAN_POINT('Ctrl Pts',(-4.27007820568629,4.05642175081999,
5.96181307371015));
#133822=CARTESIAN_POINT('Ctrl Pts',(-4.31868018038231,4.06954550707837,
6.0294892121902));
#133823=CARTESIAN_POINT('Ctrl Pts',(-4.34299268432752,4.07595289333869,
6.06337768937981));
#133824=CARTESIAN_POINT('Ctrl Pts',(-4.36729000735009,4.08221031164667,
6.09727627585942));
#133825=CARTESIAN_POINT('Ctrl Pts',(-4.814100554,4.172899507,5.751037807));
#133826=CARTESIAN_POINT('Ctrl Pts',(-4.500706857,4.107307013,6.01337459200001));
#133827=CARTESIAN_POINT('Ctrl Pts',(-4.160662311,4.04203077,6.240103295));
#133828=CARTESIAN_POINT('Ctrl Pts',(-4.83344805100001,4.172899507,5.403728337));
#133829=CARTESIAN_POINT('Ctrl Pts',(-4.538980434,4.107307013,5.667119433));
#133830=CARTESIAN_POINT('Ctrl Pts',(-4.217635331,4.04203077,5.89695279));
#133831=CARTESIAN_POINT('',(-4.81410055117865,4.17289950692264,5.75103781132326));
#133832=CARTESIAN_POINT('Origin',(0.122322701494825,4.16071408995026,-0.149168563028286));
#133833=CARTESIAN_POINT('',(-4.82377430351141,4.17289950678353,5.57738307112526));
#133834=CARTESIAN_POINT('Origin',(-1.34441069388203E-13,4.26419218500022,
1.7650811368064E-13));
#133835=CARTESIAN_POINT('',(-4.36344234637331,4.26310680660557,6.10003040005731));
#133836=CARTESIAN_POINT('Origin',(0.0982427970437966,4.16071715899573,-0.165512377509088));
#133837=CARTESIAN_POINT('Origin',(0.136728528293678,4.01799496612477,-0.124861216573521));
#133838=CARTESIAN_POINT('Ctrl Pts',(-5.74035438700001,4.042023177,4.826834523));
#133839=CARTESIAN_POINT('Ctrl Pts',(-5.476831939,4.10772842,5.140230856));
#133840=CARTESIAN_POINT('Ctrl Pts',(-5.180757521,4.172899507,5.423075834));
#133841=CARTESIAN_POINT('Ctrl Pts',(-5.39300289,4.042023177,4.845412245));
#133842=CARTESIAN_POINT('Ctrl Pts',(-5.128466186,4.10772842,5.139844821));
#133843=CARTESIAN_POINT('Ctrl Pts',(-4.83344805100001,4.172899507,5.403728337));
#133844=CARTESIAN_POINT('',(-5.18075751483706,4.17289950600424,5.42307584194055));
#133845=CARTESIAN_POINT('',(-5.00710277312053,4.17289950413623,5.41340209741281));
#133846=CARTESIAN_POINT('',(-5.57591935849747,4.08221031169378,5.01588709046708));
#133847=CARTESIAN_POINT('Origin',(0.148496838195578,4.01787919839837,-0.119683774713932));
#133848=CARTESIAN_POINT('Ctrl Pts',(-5.38984451854537,4.04280735924304,
4.84892524811203));
#133849=CARTESIAN_POINT('Ctrl Pts',(-5.42083994034192,4.04969801218734,
4.87668112718648));
#133850=CARTESIAN_POINT('Ctrl Pts',(-5.4518597438633,4.05642175349626,4.90448861664555));
#133851=CARTESIAN_POINT('Ctrl Pts',(-5.51387378821012,4.06954550710964,
4.96013452549735));
#133852=CARTESIAN_POINT('Ctrl Pts',(-5.54490290021431,4.0759528933765,4.98800423927055));
#133853=CARTESIAN_POINT('Ctrl Pts',(-5.57591935941457,4.08221031169365,
5.01588708944694));
#133854=CARTESIAN_POINT('Ctrl Pts',(-5.937852687,4.172899507,4.58169242400001));
#133855=CARTESIAN_POINT('Ctrl Pts',(-5.688180615,4.107307013,4.905266302));
#133856=CARTESIAN_POINT('Ctrl Pts',(-5.404826091,4.04203077,5.199793739));
#133857=CARTESIAN_POINT('Ctrl Pts',(-5.882086581,4.172899507,4.238343716));
#133858=CARTESIAN_POINT('Ctrl Pts',(-5.651124753,4.107307013,4.558878708));
#133859=CARTESIAN_POINT('Ctrl Pts',(-5.38669989800001,4.04203077,4.852418387));
#133860=CARTESIAN_POINT('',(-5.93785268519229,4.17289950685237,4.58169242882394));
#133861=CARTESIAN_POINT('Origin',(0.151529528601895,4.16071399372597,-0.119385194429135));
#133862=CARTESIAN_POINT('',(-5.90996963479971,4.17289950678353,4.41001806892829));
#133863=CARTESIAN_POINT('Origin',(3.14418630020796E-13,4.26419218500067,
-4.08961059461532E-13));
#133864=CARTESIAN_POINT('',(-5.57275370974783,4.26310680605755,5.01940395734865));
#133865=CARTESIAN_POINT('Origin',(0.131526048152067,4.16071715478734,-0.140523359004434));
#133866=CARTESIAN_POINT('Origin',(0.160373400530025,4.0179949732781,-0.0925494642866742));
#133867=CARTESIAN_POINT('Ctrl Pts',(-6.643774834,4.042023177,3.479979305));
#133868=CARTESIAN_POINT('Ctrl Pts',(-6.453784342,4.10772842,3.842698142));
#133869=CARTESIAN_POINT('Ctrl Pts',(-6.225435289,4.172899507,4.18257761));
#133870=CARTESIAN_POINT('Ctrl Pts',(-6.308537883,4.042023177,3.572792994));
#133871=CARTESIAN_POINT('Ctrl Pts',(-6.113480201,4.10772842,3.917209472));
#133872=CARTESIAN_POINT('Ctrl Pts',(-5.882086581,4.172899507,4.238343716));
#133873=CARTESIAN_POINT('',(-6.22543528466732,4.17289950600422,4.18257761909796));
#133874=CARTESIAN_POINT('',(-6.05376092498255,4.17289950413623,4.210460677403));
#133875=CARTESIAN_POINT('',(-6.52382491778054,4.08221031166323,3.69996059879415));
#133876=CARTESIAN_POINT('Origin',(0.170753419546019,4.01787914189447,-0.0849631041525056));
#133877=CARTESIAN_POINT('Ctrl Pts',(-6.30620854436298,4.04280735921502,
3.57690282142814));
#133878=CARTESIAN_POINT('Ctrl Pts',(-6.34244600490884,4.04969801238145,
3.59734668483609));
#133879=CARTESIAN_POINT('Ctrl Pts',(-6.37871837213589,4.05642175393434,
3.61783571071886));
#133880=CARTESIAN_POINT('Ctrl Pts',(-6.451244785248,4.06954550708461,3.6588494613919));
#133881=CARTESIAN_POINT('Ctrl Pts',(-6.48753961835998,4.07595289334855,
3.67939725488016));
#133882=CARTESIAN_POINT('Ctrl Pts',(-6.52382491844971,4.08221031166311,
3.6999605976134));
#133883=CARTESIAN_POINT('Ctrl Pts',(-6.783957428,4.172899507,3.198112195));
#133884=CARTESIAN_POINT('Ctrl Pts',(-6.609681369,4.107307013,3.567793211));
#133885=CARTESIAN_POINT('Ctrl Pts',(-6.396266209,4.04203077,3.916347607));
#133886=CARTESIAN_POINT('Ctrl Pts',(-6.65568528000001,4.172899507,2.874778854));
#133887=CARTESIAN_POINT('Ctrl Pts',(-6.499028759,4.107307013,3.237469881));
#133888=CARTESIAN_POINT('Ctrl Pts',(-6.303888365,4.04203077,3.580990293));
#133889=CARTESIAN_POINT('',(-6.78395742727015,4.17289950685237,3.19811220011488));
#133890=CARTESIAN_POINT('Origin',(0.173651161295976,4.16071398741859,-0.0840196800174137));
#133891=CARTESIAN_POINT('',(-6.71982135455063,4.17289950678353,3.03644552328143));
#133892=CARTESIAN_POINT('Origin',(1.86049092798513E-13,4.26419218500022,
-1.0321604682062E-13));
#133893=CARTESIAN_POINT('',(-6.52148930308317,4.26310680659818,3.70407576406289));
#133894=CARTESIAN_POINT('Origin',(0.158659732795933,4.16071715051203,-0.108963977755514));
#133895=CARTESIAN_POINT('Origin',(0.176518966636331,4.01799497241305,-0.0559099629043863));
#133896=CARTESIAN_POINT('Ctrl Pts',(-7.236539753,4.042023177,1.970404122));
#133897=CARTESIAN_POINT('Ctrl Pts',(-7.128964961,4.10772842,2.365485134));
#133898=CARTESIAN_POINT('Ctrl Pts',(-6.979018621,4.172899507,2.746506705));
#133899=CARTESIAN_POINT('Ctrl Pts',(-6.929092656,4.042023177,2.133113913));
#133900=CARTESIAN_POINT('Ctrl Pts',(-6.812634675,4.10772842,2.511409761));
#133901=CARTESIAN_POINT('Ctrl Pts',(-6.65568528,4.172899507,2.874778854));
#133902=CARTESIAN_POINT('',(-6.97901861874018,4.17289950600424,2.74650671479494));
#133903=CARTESIAN_POINT('',(-6.81735194381297,4.17289950413623,2.81064279571972));
#133904=CARTESIAN_POINT('',(-7.16668367558851,4.08221031168703,2.21102806139634));
#133905=CARTESIAN_POINT('Origin',(0.185026142951854,4.01787919238931,-0.0462698970781572));
#133906=CARTESIAN_POINT('Ctrl Pts',(-6.92770126735829,4.04280735924753,
2.13762839408099));
#133907=CARTESIAN_POINT('Ctrl Pts',(-6.96748634201239,4.04969801232502,
2.14980430828143));
#133908=CARTESIAN_POINT('Ctrl Pts',(-7.00731521574551,4.05642175377696,
2.16201682517382));
#133909=CARTESIAN_POINT('Ctrl Pts',(-7.08696274687549,4.06954550711632,
2.18648066255977));
#133910=CARTESIAN_POINT('Ctrl Pts',(-7.12682619520053,4.07595289337755,
2.19874574381524));
#133911=CARTESIAN_POINT('Ctrl Pts',(-7.16668367599155,4.0822103116869,2.21102806008848));
#133912=CARTESIAN_POINT('Ctrl Pts',(-7.31285186,4.172899507,1.664991795));
#133913=CARTESIAN_POINT('Ctrl Pts',(-7.222120769,4.107307013,2.063494074));
#133914=CARTESIAN_POINT('Ctrl Pts',(-7.088624029,4.04203077,2.449777414));
#133915=CARTESIAN_POINT('Ctrl Pts',(-7.118071532,4.172899507,1.376792527));
#133916=CARTESIAN_POINT('Ctrl Pts',(-7.043045404,4.107307013,1.764680561));
#133917=CARTESIAN_POINT('Ctrl Pts',(-6.926314018,4.04203077,2.142119073));
#133918=CARTESIAN_POINT('',(-7.31285186038333,4.17289950685237,1.66499180012521));
#133919=CARTESIAN_POINT('Origin',(0.187653197368192,4.16071405450739,-0.0447255136504804));
#133920=CARTESIAN_POINT('',(-7.2154616962758,4.17289950678353,1.52089215969156));
#133921=CARTESIAN_POINT('Origin',(6.40112962635442E-13,4.26419218500022,
-2.50992802930394E-13));
#133922=CARTESIAN_POINT('',(-7.16528730476381,4.26310680663001,2.21554910444215));
#133923=CARTESIAN_POINT('Origin',(0.178374116608985,4.16071715854707,-0.0723092164665737));
#133924=CARTESIAN_POINT('Origin',(0.184411326266831,4.01799491751039,-0.0166565351205841));
#133925=CARTESIAN_POINT('Ctrl Pts',(-7.490932116,4.042023177,0.368695032));
#133926=CARTESIAN_POINT('Ctrl Pts',(-7.470803103,4.10772842,0.77766467));
#133927=CARTESIAN_POINT('Ctrl Pts',(-7.4062708,4.172899507,1.182012199));
#133928=CARTESIAN_POINT('Ctrl Pts',(-7.225650757,4.042023177,0.593692797));
#133929=CARTESIAN_POINT('Ctrl Pts',(-7.193237924,4.10772842,0.988179322000001));
#133930=CARTESIAN_POINT('Ctrl Pts',(-7.118071532,4.172899507,1.376792527));
#133931=CARTESIAN_POINT('',(-7.40627079988748,4.17289950600422,1.18201220907727));
#133932=CARTESIAN_POINT('',(-7.26217116295607,4.17289950413623,1.27940238027803));
#133933=CARTESIAN_POINT('',(-7.47443626910764,4.08221031167934,0.618710309512847));
#133934=CARTESIAN_POINT('Origin',(0.190646650037835,4.01787918147397,-0.00541292423114959));
#133935=CARTESIAN_POINT('Ctrl Pts',(-7.22526237813834,4.04280735921943,
0.598400839381963));
#133936=CARTESIAN_POINT('Ctrl Pts',(-7.26673476055614,4.04969801214614,
0.601739472284816));
#133937=CARTESIAN_POINT('Ctrl Pts',(-7.30825778633643,4.05642175343086,
0.605104436638636));
#133938=CARTESIAN_POINT('Ctrl Pts',(-7.39130220628258,4.06954550709366,
0.611874458356977));
#133939=CARTESIAN_POINT('Ctrl Pts',(-7.43287029924927,4.07595289336291,
0.615283325785464));
#133940=CARTESIAN_POINT('Ctrl Pts',(-7.47443626921981,4.08221031167921,
0.61871030815259));
#133941=CARTESIAN_POINT('Ctrl Pts',(-7.49980546600001,4.172899507,0.054018228));
#133942=CARTESIAN_POINT('Ctrl Pts',(-7.49686182800001,4.107307013,0.462708249));
#133943=CARTESIAN_POINT('Ctrl Pts',(-7.449525667,4.04203077,0.868658351));
#133944=CARTESIAN_POINT('Ctrl Pts',(-7.247624671,4.172899507,-0.185571088));
#133945=CARTESIAN_POINT('Ctrl Pts',(-7.257737073,4.107307013,0.209376739));
#133946=CARTESIAN_POINT('Ctrl Pts',(-7.224872925,4.04203077,0.603084746));
#133947=CARTESIAN_POINT('',(-7.49980546748518,4.17289950685237,0.0540182329483246));
#133948=CARTESIAN_POINT('Origin',(0.192880559441947,4.16071398945195,-0.00333997202822588));
#133949=CARTESIAN_POINT('',(-7.37371506848807,4.17289950678353,-0.0657764313371442));
#133950=CARTESIAN_POINT('Origin',(8.59555482346508E-13,4.264192185,1.95698492133634E-14));
#133951=CARTESIAN_POINT('',(-7.47404443556447,4.26310680659394,0.623425831355525));
#133952=CARTESIAN_POINT('Origin',(0.1897483654665,4.16071713900448,-0.0322735214081868));
#133953=CARTESIAN_POINT('Origin',(0.183680685919455,4.01799491410986,0.0233758684203914));
#133954=CARTESIAN_POINT('Ctrl Pts',(-7.39505682,4.042023177,-1.250253828));
#133955=CARTESIAN_POINT('Ctrl Pts',(-7.463314795,4.10772842,-0.846518529));
#133956=CARTESIAN_POINT('Ctrl Pts',(-7.487213987,4.172899507,-0.437751883));
#133957=CARTESIAN_POINT('Ctrl Pts',(-7.18434546000001,4.042023177,-0.973488735));
#133958=CARTESIAN_POINT('Ctrl Pts',(-7.237493363,4.10772842,-0.581257285));
#133959=CARTESIAN_POINT('Ctrl Pts',(-7.247624671,4.172899507,-0.185571088));
#133960=CARTESIAN_POINT('',(-7.48721398905837,4.17289950600422,-0.437751873144494));
#133961=CARTESIAN_POINT('',(-7.3674193297415,4.17289950413623,-0.311661467971566));
#133962=CARTESIAN_POINT('',(-7.43269253070425,4.08221031161394,-1.00253764896776));
#133963=CARTESIAN_POINT('Origin',(0.187352954992916,4.01787920562906,0.0356969993917453));
#133964=CARTESIAN_POINT('Ctrl Pts',(-7.18497825126012,4.04280735926989,
-0.968807273831972));
#133965=CARTESIAN_POINT('Ctrl Pts',(-7.22619874119893,4.04969801241923,
-0.974462032846668));
#133966=CARTESIAN_POINT('Ctrl Pts',(-7.26747435131031,4.05642175395236,
-0.980101962884917));
#133967=CARTESIAN_POINT('Ctrl Pts',(-7.35003259022942,4.06954550707542,
-0.991342315626475));
#133968=CARTESIAN_POINT('Ctrl Pts',(-7.39136164998044,4.07595289332165,
-0.99694905686827));
#133969=CARTESIAN_POINT('Ctrl Pts',(-7.43269253052555,4.08221031161382,
-1.00253765028944));
#133970=CARTESIAN_POINT('Ctrl Pts',(-7.336076504,4.172899507,-1.55948117));
#133971=CARTESIAN_POINT('Ctrl Pts',(-7.421057961,4.107307013,-1.159713301));
#133972=CARTESIAN_POINT('Ctrl Pts',(-7.462095765,4.04203077,-0.753078211));
#133973=CARTESIAN_POINT('Ctrl Pts',(-7.03828693500001,4.172899507,-1.739257605));
#133974=CARTESIAN_POINT('Ctrl Pts',(-7.133065024,4.107307013,-1.355717306));
#133975=CARTESIAN_POINT('Ctrl Pts',(-7.185604805,4.04203077,-0.964149153));
#133976=CARTESIAN_POINT('',(-7.33607650652361,4.17289950685235,-1.55948116547139));
#133977=CARTESIAN_POINT('Origin',(0.18908886836307,4.16071403517206,0.0382017074795551));
#133978=CARTESIAN_POINT('',(-7.1871817192009,4.17289950678353,-1.64936938880332));
#133979=CARTESIAN_POINT('Origin',(3.62123525610158E-13,4.26419218500022,
3.63749828868887E-14));
#133980=CARTESIAN_POINT('',(-7.43332355565574,4.26310680663769,-0.997848140298518));
#133981=CARTESIAN_POINT('Origin',(0.192249680943634,4.16071712908807,0.00927126714342946));
#133982=CARTESIAN_POINT('Origin',(0.174360938573022,4.01799497386905,0.0623152207350958));
#133983=CARTESIAN_POINT('Ctrl Pts',(-6.953396885,4.042023177,-2.810742208));
#133984=CARTESIAN_POINT('Ctrl Pts',(-7.106850181,4.10772842,-2.431119463));
#133985=CARTESIAN_POINT('Ctrl Pts',(-7.21806337,4.172899507,-2.037047174));
#133986=CARTESIAN_POINT('Ctrl Pts',(-6.807108153,4.042023177,-2.495151015));
#133987=CARTESIAN_POINT('Ctrl Pts',(-6.94333165600001,4.10772842,-2.123514947));
#133988=CARTESIAN_POINT('Ctrl Pts',(-7.038286935,4.172899507,-1.739257605));
#133989=CARTESIAN_POINT('',(-7.21806337412925,4.17289950600421,-2.03704716480384));
#133990=CARTESIAN_POINT('',(-7.12817515699226,4.17289950413623,-1.88815237254077));
#133991=CARTESIAN_POINT('',(-7.04340435027309,4.08221031169495,-2.57690806135675));
#133992=CARTESIAN_POINT('Origin',(0.175299420682953,4.0178792215071,0.0751379209236386));
#133993=CARTESIAN_POINT('Ctrl Pts',(-6.80873252634046,4.04280735930085,
-2.49071503621283));
#133994=CARTESIAN_POINT('Ctrl Pts',(-6.84777370212766,4.04969801315263,
-2.50509877828202));
#133995=CARTESIAN_POINT('Ctrl Pts',(-6.88687189803305,4.05642175546742,
-2.5194798876564));
#133996=CARTESIAN_POINT('Ctrl Pts',(-6.96508361896581,4.06954550714206,
-2.54820502489215));
#133997=CARTESIAN_POINT('Ctrl Pts',(-7.00424114463182,4.0759528933933,-2.56256520981103));
#133998=CARTESIAN_POINT('Ctrl Pts',(-7.04340434980117,4.08221031169484,
-2.5769080626454));
#133999=CARTESIAN_POINT('Ctrl Pts',(-6.829320759,4.172899507,-3.100060963));
#134000=CARTESIAN_POINT('Ctrl Pts',(-6.998253671,4.107307013,-2.727907945));
#134001=CARTESIAN_POINT('Ctrl Pts',(-7.125746559,4.04203077,-2.339601672));
#134002=CARTESIAN_POINT('Ctrl Pts',(-6.499846725,4.172899507,-3.21161837));
#134003=CARTESIAN_POINT('Ctrl Pts',(-6.67485878100001,4.107307013,-2.857419517));
#134004=CARTESIAN_POINT('Ctrl Pts',(-6.81034579,4.04203077,-2.48630051));
#134005=CARTESIAN_POINT('',(-6.82932076240721,4.17289950685237,-3.10006095915154));
#134006=CARTESIAN_POINT('Origin',(0.176456086776277,4.16071403607459,0.0779571854405042));
#134007=CARTESIAN_POINT('',(-6.6645837414277,4.17289950678353,-3.15583966770859));
#134008=CARTESIAN_POINT('Origin',(8.87744738831131E-13,4.26419218500111,
3.38921599118969E-13));
#134009=CARTESIAN_POINT('',(-7.0450287277557,4.26310680662765,-2.57246384257894));
#134010=CARTESIAN_POINT('Origin',(0.185761950671148,4.16071713387759,0.0503825143463937));
#134011=CARTESIAN_POINT('Origin',(0.156888685719833,4.01799496418505,0.0983408227819893));
#134012=CARTESIAN_POINT('Ctrl Pts',(-6.18660384,4.042023177,-4.239803406));
#134013=CARTESIAN_POINT('Ctrl Pts',(-6.418077152,4.10772842,-3.902043953));
#134014=CARTESIAN_POINT('Ctrl Pts',(-6.611404132,4.172899507,-3.541092403));
#134015=CARTESIAN_POINT('Ctrl Pts',(-6.111578035,4.042023177,-3.900142807));
#134016=CARTESIAN_POINT('Ctrl Pts',(-6.324507477,4.10772842,-3.56647941));
#134017=CARTESIAN_POINT('Ctrl Pts',(-6.499846725,4.172899507,-3.21161837));
#134018=CARTESIAN_POINT('',(-6.61140413801019,4.17289950600422,-3.54109239490403));
#134019=CARTESIAN_POINT('',(-6.55562543653299,4.17289950413623,-3.37635537090293));
#134020=CARTESIAN_POINT('',(-6.32477440992221,4.08221031163205,-4.03078511625019));
#134021=CARTESIAN_POINT('Origin',(0.155048372953193,4.01787918526179,0.111065323303753));
#134022=CARTESIAN_POINT('Ctrl Pts',(-6.11411803582838,4.04280735932927,
-3.89615973118788));
#134023=CARTESIAN_POINT('Ctrl Pts',(-6.14915437016196,4.04969801296718,
-3.91859988748003));
#134024=CARTESIAN_POINT('Ctrl Pts',(-6.1842469572818,4.05642175505077,-3.94104973009006));
#134025=CARTESIAN_POINT('Ctrl Pts',(-6.25445507828098,4.06954550710154,
-3.98591649891152));
#134026=CARTESIAN_POINT('Ctrl Pts',(-6.28961010744197,4.07595289334218,
-4.00835866113015));
#134027=CARTESIAN_POINT('Ctrl Pts',(-6.32477440920043,4.08221031163192,
-4.03078511738196));
#134028=CARTESIAN_POINT('Ctrl Pts',(-6.00323356500001,4.172899507,-4.49568535));
#134029=CARTESIAN_POINT('Ctrl Pts',(-6.248218817,4.107307013,-4.168548645));
#134030=CARTESIAN_POINT('Ctrl Pts',(-6.456205362,4.04203077,-3.81672796));
#134031=CARTESIAN_POINT('Ctrl Pts',(-5.657480906,4.172899507,-4.533807429));
#134032=CARTESIAN_POINT('Ctrl Pts',(-5.904543561,4.107307013,-4.225511967));
#134033=CARTESIAN_POINT('Ctrl Pts',(-6.116642575,4.04203077,-3.892195218));
#134034=CARTESIAN_POINT('',(-6.00323356915964,4.17289950685237,-4.49568534697083));
#134035=CARTESIAN_POINT('Origin',(0.155572222910411,4.16071401278495,0.114067469851924));
#134036=CARTESIAN_POINT('',(-5.83035723468127,4.17289950678352,-4.51474639055731));
#134037=CARTESIAN_POINT('Origin',(9.14632952708772E-13,4.26419218500022,
5.24970691917481E-13));
#134038=CARTESIAN_POINT('',(-6.32731618628048,4.26310680660589,-4.02679399416042));
#134039=CARTESIAN_POINT('Origin',(0.170588519435007,4.16071713402905,0.0891381260390134));
#134040=CARTESIAN_POINT('Origin',(0.132080173369563,4.01799495212349,0.129767979784806));
#134041=CARTESIAN_POINT('Ctrl Pts',(-5.130532076,4.042023177,-5.47061610999999));
#134042=CARTESIAN_POINT('Ctrl Pts',(-5.429201969,4.10772842,-5.190513205));
#134043=CARTESIAN_POINT('Ctrl Pts',(-5.695602984,4.172899507,-4.879560087));
#134044=CARTESIAN_POINT('Ctrl Pts',(-5.130277321,4.042023177,-5.122768257));
#134045=CARTESIAN_POINT('Ctrl Pts',(-5.409956358,4.10772842,-4.84267926));
#134046=CARTESIAN_POINT('Ctrl Pts',(-5.657480906,4.172899507,-4.533807429));
#134047=CARTESIAN_POINT('',(-5.69560299159702,4.17289950600423,-4.87956008041204));
#134048=CARTESIAN_POINT('',(-5.67654195619809,4.17289950413623,-4.70668374449444));
#134049=CARTESIAN_POINT('',(-5.31040504833037,4.08221031160588,-5.29618713926893));
#134050=CARTESIAN_POINT('Origin',(0.127547362614432,4.01787918058668,0.141799201134928));
#134051=CARTESIAN_POINT('Ctrl Pts',(-5.13361418158609,4.04280735933178,
-5.11942432679469));
#134052=CARTESIAN_POINT('Ctrl Pts',(-5.16300740977581,4.04969801160511,
-5.14887161527873));
#134053=CARTESIAN_POINT('Ctrl Pts',(-5.1924534920505,4.05642175216957,-5.17834045498303));
#134054=CARTESIAN_POINT('Ctrl Pts',(-5.25137516991062,4.06954550705694,
-5.23725094732631));
#134055=CARTESIAN_POINT('Ctrl Pts',(-5.28088389259553,4.07595289330727,
-5.26672571649307));
#134056=CARTESIAN_POINT('Ctrl Pts',(-5.31040504739098,4.08221031160576,
-5.29618714021025));
#134057=CARTESIAN_POINT('Ctrl Pts',(-4.896441841,4.172899507,-5.681096487));
#134058=CARTESIAN_POINT('Ctrl Pts',(-5.206024196,4.107307013,-5.414272644));
#134059=CARTESIAN_POINT('Ctrl Pts',(-5.484779179,4.04203077,-5.11538829));
#134060=CARTESIAN_POINT('Ctrl Pts',(-4.550577568,4.172899507,-5.64400069100001));
#134061=CARTESIAN_POINT('Ctrl Pts',(-4.85813844599999,4.107307013,-5.396024174));
#134062=CARTESIAN_POINT('Ctrl Pts',(-5.136931951,4.04203077,-5.116095203));
#134063=CARTESIAN_POINT('',(-4.89644184573234,4.17289950685235,-5.68109648492861));
#134064=CARTESIAN_POINT('Origin',(0.127413845258664,4.16071401356712,0.144844019211612));
#134065=CARTESIAN_POINT('',(-4.72350970347312,4.17289950678353,-5.66254858985659));
#134066=CARTESIAN_POINT('Origin',(7.67615138119737E-13,4.26419218499978,
8.51315545835618E-13));
#134067=CARTESIAN_POINT('',(-5.31374537261658,4.26310680661091,-5.29283573454961));
#134068=CARTESIAN_POINT('Origin',(0.14743797145068,4.16071715078108,0.12372539659845));
#134069=CARTESIAN_POINT('Origin',(0.101096018227911,4.01799493201509,0.155127520179251));
#134070=CARTESIAN_POINT('Ctrl Pts',(-3.834562334,4.042023177,-6.445628884));
#134071=CARTESIAN_POINT('Ctrl Pts',(-4.186463335,4.10772842,-6.236279827));
#134072=CARTESIAN_POINT('Ctrl Pts',(-4.513481772,4.172899507,-5.989864965));
#134073=CARTESIAN_POINT('Ctrl Pts',(-3.909090541,4.042023177,-6.105858756));
#134074=CARTESIAN_POINT('Ctrl Pts',(-4.242441693,4.10772842,-5.89244081));
#134075=CARTESIAN_POINT('Ctrl Pts',(-4.550577568,4.172899507,-5.64400069100001));
#134076=CARTESIAN_POINT('',(-4.51348178085793,4.17289950600422,-5.98986496017105));
#134077=CARTESIAN_POINT('',(-4.53202968383958,4.17289950413623,-5.81693281721745));
#134078=CARTESIAN_POINT('',(-4.0477270485313,4.08221031162645,-6.31394533827614));
#134079=CARTESIAN_POINT('Origin',(0.0940831213956261,4.01787919159973,0.16590348653861));
#134080=CARTESIAN_POINT('Ctrl Pts',(-3.91306823383849,4.04280735934069,
-6.10331033138982));
#134081=CARTESIAN_POINT('Ctrl Pts',(-3.93544396832325,4.04969801166272,
-6.13838783415081));
#134082=CARTESIAN_POINT('Ctrl Pts',(-3.95786668829155,4.05642175228402,
-6.17349774639542));
#134083=CARTESIAN_POINT('Ctrl Pts',(-4.00274679512569,4.06954550706758,
-6.24369736271112));
#134084=CARTESIAN_POINT('Ctrl Pts',(-4.02522941608651,4.07595289331948,
-6.27882653129195));
#134085=CARTESIAN_POINT('Ctrl Pts',(-4.04772704740326,4.08221031162632,
-6.31394533899881));
#134086=CARTESIAN_POINT('Ctrl Pts',(-3.560697939,4.172899507,-6.600865866));
#134087=CARTESIAN_POINT('Ctrl Pts',(-3.92040167,4.107307013,-6.406831272));
#134088=CARTESIAN_POINT('Ctrl Pts',(-4.256890817,4.04203077,-6.174858749));
#134089=CARTESIAN_POINT('Ctrl Pts',(-3.23089428,4.172899507,-6.49028675400001));
#134090=CARTESIAN_POINT('Ctrl Pts',(-3.584572177,4.107307013,-6.314224288));
#134091=CARTESIAN_POINT('Ctrl Pts',(-3.917024099,4.04203077,-6.100772263));
#134092=CARTESIAN_POINT('',(-3.56069794407931,4.17289950685236,-6.60086586499261));
#134093=CARTESIAN_POINT('Origin',(0.0932976583525053,4.16071400382663,0.168847627684026));
#134094=CARTESIAN_POINT('',(-3.39579610831299,4.17289950678352,-6.54557631061581));
#134095=CARTESIAN_POINT('Origin',(4.91360424570431E-13,4.26419218500067,
7.63278329429795E-13));
#134096=CARTESIAN_POINT('',(-4.05170973090138,4.2631068066114,-6.31139035807637));
#134097=CARTESIAN_POINT('Origin',(0.11739369948572,4.16071712351179,0.152527655333695));
#134098=CARTESIAN_POINT('Origin',(0.0653845985702356,4.01799498159655,0.17323333309049));
#134099=CARTESIAN_POINT('Ctrl Pts',(-2.359292718,4.042023177,-7.119251215));
#134100=CARTESIAN_POINT('Ctrl Pts',(-2.747970329,4.10772842,-6.990444937));
#134101=CARTESIAN_POINT('Ctrl Pts',(-3.120315168,4.172899507,-6.820090414));
#134102=CARTESIAN_POINT('Ctrl Pts',(-2.505119032,4.042023177,-6.803446085));
#134103=CARTESIAN_POINT('Ctrl Pts',(-2.876555169,4.10772842,-6.666678376));
#134104=CARTESIAN_POINT('Ctrl Pts',(-3.23089428,4.172899507,-6.490286754));
#134105=CARTESIAN_POINT('',(-3.12031517768316,4.17289950600422,-6.82009041119266));
#134106=CARTESIAN_POINT('',(-3.17560473983395,4.17289950413623,-6.65518857644464));
#134107=CARTESIAN_POINT('',(-2.59578183050533,4.08221031170026,-7.03647047076548));
#134108=CARTESIAN_POINT('Origin',(0.0562190675631685,4.01787921877911,0.182249585017943));
#134109=CARTESIAN_POINT('Ctrl Pts',(-2.50955156393116,4.04280735929469,
-6.80181232839606));
#134110=CARTESIAN_POINT('Ctrl Pts',(-2.52386354156956,4.04969801243914,
-6.84087986467192));
#134111=CARTESIAN_POINT('Ctrl Pts',(-2.53821443956852,4.05642175397371,
-6.87998915422951));
#134112=CARTESIAN_POINT('Ctrl Pts',(-2.56695442848329,4.06954550713191,
-6.95819542901028));
#134113=CARTESIAN_POINT('Ctrl Pts',(-2.58135968549397,4.0759528933911,-6.99733639606272));
#134114=CARTESIAN_POINT('Ctrl Pts',(-2.59578182921528,4.08221031170013,
-7.03647047124092));
#134115=CARTESIAN_POINT('Ctrl Pts',(-2.058459759,4.172899507,-7.211986094));
#134116=CARTESIAN_POINT('Ctrl Pts',(-2.451465519,4.107307013,-7.09981359));
#134117=CARTESIAN_POINT('Ctrl Pts',(-2.829954972,4.04203077,-6.945599676));
#134118=CARTESIAN_POINT('Ctrl Pts',(-1.760137966,4.172899507,-7.033094222));
#134119=CARTESIAN_POINT('Ctrl Pts',(-2.143395296,4.107307013,-6.937178292));
#134120=CARTESIAN_POINT('Ctrl Pts',(-2.513960553,4.04203077,-6.800183993));
#134121=CARTESIAN_POINT('',(-2.05845976415483,4.17289950685236,-7.21198609410644));
#134122=CARTESIAN_POINT('Origin',(0.0548191946948218,4.16071399001688,0.184956388900183));
#134123=CARTESIAN_POINT('',(-1.90929886120836,4.17289950678353,-7.12254015834624));
#134124=CARTESIAN_POINT('Origin',(2.99239799605999E-14,4.26419218500089,
5.03069808033274E-14));
#134125=CARTESIAN_POINT('',(-2.60022064544648,4.26310680662107,-7.03483138298938));
#134126=CARTESIAN_POINT('Origin',(0.0818601306484634,4.16071714532607,0.174197752453119));
#134127=CARTESIAN_POINT('Origin',(0.0266158912002012,4.01799497142736,0.18323895048609));
#134128=CARTESIAN_POINT('Ctrl Pts',(-0.773705198,4.042023177,-7.459985273));
#134129=CARTESIAN_POINT('Ctrl Pts',(-1.180985284,4.10772842,-7.41774461));
#134130=CARTESIAN_POINT('Ctrl Pts',(-1.581246094,4.172899507,-7.331416015));
#134131=CARTESIAN_POINT('Ctrl Pts',(-0.984010941,4.042023177,-7.18291183800001));
#134132=CARTESIAN_POINT('Ctrl Pts',(-1.376164122,4.10772842,-7.129189471));
#134133=CARTESIAN_POINT('Ctrl Pts',(-1.760137966,4.172899507,-7.033094222));
#134134=CARTESIAN_POINT('',(-1.58124610403693,4.17289950600423,-7.33141601435202));
#134135=CARTESIAN_POINT('',(-1.67069204708794,4.17289950413623,-7.18225511452511));
#134136=CARTESIAN_POINT('',(-1.02246073937731,4.08221031165689,-7.429978063712));
#134137=CARTESIAN_POINT('Origin',(0.0157264105232788,4.01787917543695,0.190074088263203));
#134138=CARTESIAN_POINT('Ctrl Pts',(-0.988691052623827,4.04280735930237,
-7.1822691405059));
#134139=CARTESIAN_POINT('Ctrl Pts',(-0.994270058771183,4.04969801240803,
-7.22349995134818));
#134140=CARTESIAN_POINT('Ctrl Pts',(-0.999878099569674,4.05642175390003,
-7.26477990599238));
#134141=CARTESIAN_POINT('Ctrl Pts',(-1.01113412626995,4.06954550710363,
-7.34733600980363));
#134142=CARTESIAN_POINT('Ctrl Pts',(-1.0167884454357,4.07595289335518,-7.38865858715136));
#134143=CARTESIAN_POINT('Ctrl Pts',(-1.02246073803572,4.08221031165677,
-7.42997806389619));
#134144=CARTESIAN_POINT('Ctrl Pts',(-0.459970288,4.172899507,-7.485881867));
#134145=CARTESIAN_POINT('Ctrl Pts',(-0.867901564,4.107307013,-7.46081651499999));
#134146=CARTESIAN_POINT('Ctrl Pts',(-1.270693578,4.04203077,-7.391572081));
#134147=CARTESIAN_POINT('Ctrl Pts',(-0.207079558,4.172899507,-7.247042021));
#134148=CARTESIAN_POINT('Ctrl Pts',(-0.601995634,4.107307013,-7.23575754900001));
#134149=CARTESIAN_POINT('Ctrl Pts',(-0.993347006,4.04203077,-7.181626677));
#134150=CARTESIAN_POINT('',(-0.459970293037299,4.17289950685236,-7.48588186821977));
#134151=CARTESIAN_POINT('Origin',(0.0137773947320928,4.16071402757819,0.192416766574395));
#134152=CARTESIAN_POINT('',(-0.333524921664125,4.17289950678352,-7.36646194406049));
#134153=CARTESIAN_POINT('Origin',(-1.62386380384016E-13,4.26419218499956,
-1.11802928026705E-12));
#134154=CARTESIAN_POINT('',(-1.02714813218712,4.26310680660984,-7.42933151171826));
#134155=CARTESIAN_POINT('Origin',(0.0424989310837132,4.1607171084661,0.187722585433427));
#134156=CARTESIAN_POINT('Origin',(-0.0133973344608364,4.0179949710456,0.184676628010878));
#134157=CARTESIAN_POINT('Ctrl Pts',(0.848059918,4.042023177,-7.451898709));
#134158=CARTESIAN_POINT('Ctrl Pts',(0.441221319,4.10772842,-7.49819879));
#134159=CARTESIAN_POINT('Ctrl Pts',(0.031760289,4.172899507,-7.499932752));
#134160=CARTESIAN_POINT('Ctrl Pts',(0.583108408,4.042023177,-7.22651261599999));
#134161=CARTESIAN_POINT('Ctrl Pts',(0.188574829,4.10772842,-7.25834759));
#134162=CARTESIAN_POINT('Ctrl Pts',(-0.207079558,4.172899507,-7.247042021));
#134163=CARTESIAN_POINT('',(0.0317602790403005,4.17289950600422,-7.4999327535199));
#134164=CARTESIAN_POINT('',(-0.0876596520429175,4.17289950413623,-7.37348738629144));
#134165=CARTESIAN_POINT('',(0.598669479685729,4.08221031163955,-7.47606814066269));
#134166=CARTESIAN_POINT('Origin',(-0.0255015617587158,4.01787924343035,
0.189010783131128));
#134167=CARTESIAN_POINT('Ctrl Pts',(0.578399553974621,4.0428073592547,-7.22689102994081));
#134168=CARTESIAN_POINT('Ctrl Pts',(0.581814387242482,4.04969801196833,
-7.2683572062548));
#134169=CARTESIAN_POINT('Ctrl Pts',(0.585211429059266,4.05642175301284,
-7.30987761848275));
#134170=CARTESIAN_POINT('Ctrl Pts',(0.591965684311098,4.06954550708528,
-7.39292332495118));
#134171=CARTESIAN_POINT('Ctrl Pts',(0.595326692553784,4.07595289334113,
-7.43449531494571));
#134172=CARTESIAN_POINT('Ctrl Pts',(0.598669481027308,4.08221031163943,
-7.47606814055483));
#134173=CARTESIAN_POINT('Ctrl Pts',(1.160026882,4.172899507,-7.409746125));
#134174=CARTESIAN_POINT('Ctrl Pts',(0.756244503,4.107307013,-7.472959952));
#134175=CARTESIAN_POINT('Ctrl Pts',(0.347984036,4.04203077,-7.49192279100001));
#134176=CARTESIAN_POINT('Ctrl Pts',(1.355661661,4.172899507,-7.12212619));
#134177=CARTESIAN_POINT('Ctrl Pts',(0.967552675,4.107307013,-7.196000825));
#134178=CARTESIAN_POINT('Ctrl Pts',(0.573714344,4.04203077,-7.227264479));
#134179=CARTESIAN_POINT('',(1.16002687738136,4.17289950685236,-7.40974612725279));
#134180=CARTESIAN_POINT('Origin',(-0.0279086400380241,4.16071403958437,
0.190880066307909));
#134181=CARTESIAN_POINT('',(1.25784427281764,4.17289950678353,-7.2659361572719));
#134182=CARTESIAN_POINT('Origin',(1.11986225956491E-13,4.26419218500089,
-5.11309744544164E-13));
#134183=CARTESIAN_POINT('',(0.59395268554274,4.26310680660941,-7.47644435575336));
#134184=CARTESIAN_POINT('Origin',(0.001150519444039,4.16071710816118,0.192469726632061));
#134185=CARTESIAN_POINT('Origin',(-0.0527841183711129,4.01799497364709,
0.17747896038271));
#134186=CARTESIAN_POINT('Ctrl Pts',(2.430170694,4.042023177,-7.09536964500001));
#134187=CARTESIAN_POINT('Ctrl Pts',(2.042796905,4.10772842,-7.228045528));
#134188=CARTESIAN_POINT('Ctrl Pts',(1.643281596,4.172899507,-7.317760969));
#134189=CARTESIAN_POINT('Ctrl Pts',(2.122962255,4.042023177,-6.932209696));
#134190=CARTESIAN_POINT('Ctrl Pts',(1.744496231,4.10772842,-7.048113443));
#134191=CARTESIAN_POINT('Ctrl Pts',(1.355661661,4.172899507,-7.12212619));
#134192=CARTESIAN_POINT('',(1.64328158659124,4.17289950600421,-7.31776097262514));
#134193=CARTESIAN_POINT('',(1.49947161132239,4.17289950413623,-7.21994358306752));
#134194=CARTESIAN_POINT('',(2.19180657900837,4.08221031164392,-7.1725855806994));
#134195=CARTESIAN_POINT('Origin',(-0.0655370874021338,4.01787918223643,
0.17910972065395));
#134196=CARTESIAN_POINT('Ctrl Pts',(2.11844483962398,4.04280735919209,-6.93359152718499));
#134197=CARTESIAN_POINT('Ctrl Pts',(2.13069383942245,4.04969801264247,-6.97335416331008));
#134198=CARTESIAN_POINT('Ctrl Pts',(2.14293712315487,4.05642175450617,-7.0131735929134));
#134199=CARTESIAN_POINT('Ctrl Pts',(2.16738583696148,4.06954550708139,-7.09282576247492));
#134200=CARTESIAN_POINT('Ctrl Pts',(2.17960501571345,4.07595289334154,-7.13270330499154));
#134201=CARTESIAN_POINT('Ctrl Pts',(2.19180658029741,4.0822103116438,-7.17258558030506));
#134202=CARTESIAN_POINT('Ctrl Pts',(2.725782484,4.172899507,-6.987138889));
#134203=CARTESIAN_POINT('Ctrl Pts',(2.345029417,4.107307013,-7.135676088));
#134204=CARTESIAN_POINT('Ctrl Pts',(1.950390303,4.04203077,-7.241959518));
#134205=CARTESIAN_POINT('Ctrl Pts',(2.855013647,4.172899507,-6.664187653));
#134206=CARTESIAN_POINT('Ctrl Pts',(2.491859296,4.107307013,-6.8197671));
#134207=CARTESIAN_POINT('Ctrl Pts',(2.113949448,4.04203077,-6.934963427));
#134208=CARTESIAN_POINT('',(2.72578247997462,4.17289950685236,-6.98713889219217));
#134209=CARTESIAN_POINT('Origin',(-0.0682896670251204,4.16071402437646,
0.180417702860357));
#134210=CARTESIAN_POINT('',(2.79039806673785,4.17289950678351,-6.82566327049396));
#134211=CARTESIAN_POINT('Origin',(-3.10732342634346E-13,4.26419218500044,
8.50014503228635E-13));
#134212=CARTESIAN_POINT('',(2.18728093607448,4.26310680608004,-7.17396697094151));
#134213=CARTESIAN_POINT('Origin',(-0.0402517053402771,4.16071713026298,
0.188217278569863));
#134214=CARTESIAN_POINT('Origin',(-0.0897029231216462,4.01799491305414,
0.161982952090527));
#134215=CARTESIAN_POINT('Ctrl Pts',(3.89864939,4.042023177,-6.407068982));
#134216=CARTESIAN_POINT('Ctrl Pts',(3.548853577,4.10772842,-6.61991689));
#134217=CARTESIAN_POINT('Ctrl Pts',(3.177964882,4.172899507,-6.793418816));
#134218=CARTESIAN_POINT('Ctrl Pts',(3.563548747,4.042023177,-6.313764355));
#134219=CARTESIAN_POINT('Ctrl Pts',(3.218846929,4.10772842,-6.508317345));
#134220=CARTESIAN_POINT('Ctrl Pts',(2.855013647,4.172899507,-6.664187653));
#134221=CARTESIAN_POINT('',(3.17796487359751,4.17289950600422,-6.79341882156139));
#134222=CARTESIAN_POINT('',(3.01648924849091,4.17289950413623,-6.7288032416768));
#134223=CARTESIAN_POINT('',(3.68245723873874,4.0822103116389,-6.53372089046924));
#134224=CARTESIAN_POINT('Origin',(-0.102508252357332,4.01787918946685,0.160833875721125));
#134225=CARTESIAN_POINT('Ctrl Pts',(3.55943399894128,4.04280735921392,-6.31608499055302));
#134226=CARTESIAN_POINT('Ctrl Pts',(3.57994441221785,4.04969801158654,-6.35228481986496));
#134227=CARTESIAN_POINT('Ctrl Pts',(3.60046145125465,4.05642175224883,-6.38854134233796));
#134228=CARTESIAN_POINT('Ctrl Pts',(3.6414614367487,4.06954550705898,-6.46107555004328));
#134229=CARTESIAN_POINT('Ctrl Pts',(3.66196743080507,4.07595289332575,-6.49739401557589));
#134230=CARTESIAN_POINT('Ctrl Pts',(3.68245723991077,4.08221031163877,-6.53372088980819));
#134231=CARTESIAN_POINT('Ctrl Pts',(4.164083527,4.172899507,-6.23782080400001));
#134232=CARTESIAN_POINT('Ctrl Pts',(3.824163362,4.107307013,-6.46473594));
#134233=CARTESIAN_POINT('Ctrl Pts',(3.461598487,4.04203077,-6.653370267));
#134234=CARTESIAN_POINT('Ctrl Pts',(4.220868368,4.172899507,-5.894639109));
#134235=CARTESIAN_POINT('Ctrl Pts',(3.899649346,4.107307013,-6.124648645));
#134236=CARTESIAN_POINT('Ctrl Pts',(3.555338625,4.04203077,-6.318391192));
#134237=CARTESIAN_POINT('',(4.1640835237513,4.17289950685234,-6.23782080798759));
#134238=CARTESIAN_POINT('Origin',(-0.105477635539921,4.16071403000556,0.161519491255585));
#134239=CARTESIAN_POINT('',(4.19247594860009,4.17289950678352,-6.06622995573972));
#134240=CARTESIAN_POINT('Origin',(3.38921599118969E-13,4.26419218499978,
-6.4098032437343E-13));
#134241=CARTESIAN_POINT('',(3.67833436109936,4.26310680662289,-6.53604286388211));
#134242=CARTESIAN_POINT('Origin',(-0.0797718658867791,4.16071714068479,
0.175164068949367));
#134243=CARTESIAN_POINT('Origin',(-0.122427020027684,4.01799493636923,0.138912015982894));
#134244=CARTESIAN_POINT('Ctrl Pts',(5.184831573,4.042023177,-5.419180894));
#134245=CARTESIAN_POINT('Ctrl Pts',(4.88896980099999,4.10772842,-5.702248296));
#134246=CARTESIAN_POINT('Ctrl Pts',(4.56405006300001,4.172899507,-5.951423949));
#134247=CARTESIAN_POINT('Ctrl Pts',(4.837507661,4.042023177,-5.40009441));
#134248=CARTESIAN_POINT('Ctrl Pts',(4.542687921,4.10772842,-5.66419956100001));
#134249=CARTESIAN_POINT('Ctrl Pts',(4.220868368,4.172899507,-5.894639109));
#134250=CARTESIAN_POINT('',(4.56405005599778,4.17289950600422,-5.95142395623466));
#134251=CARTESIAN_POINT('',(4.39245920140799,4.17289950413623,-5.92303153945049));
#134252=CARTESIAN_POINT('',(5.00092029153408,4.08221031166126,-5.58934667322293));
#134253=CARTESIAN_POINT('Origin',(-0.134686198386177,4.01787920240881,0.135037443744226));
#134254=CARTESIAN_POINT('Ctrl Pts',(4.83398798137622,4.0428073592445,-5.40324533971125));
#134255=CARTESIAN_POINT('Ctrl Pts',(4.86180076688022,4.04969801186075,-5.43418970570736));
#134256=CARTESIAN_POINT('Ctrl Pts',(4.8896322108278,4.05642175280369,-5.46518801533919));
#134257=CARTESIAN_POINT('Ctrl Pts',(4.94526634776557,4.06954550707249,-5.52721262610302));
#134258=CARTESIAN_POINT('Ctrl Pts',(4.97310031961993,4.07595289334174,-5.55827380351772));
#134259=CARTESIAN_POINT('Ctrl Pts',(5.00092029254455,4.08221031166114,-5.58934667231826));
#134260=CARTESIAN_POINT('Ctrl Pts',(5.407676652,4.172899507,-5.19682915100001));
#134261=CARTESIAN_POINT('Ctrl Pts',(5.12448367900001,4.107307013,-5.491511925));
#134262=CARTESIAN_POINT('Ctrl Pts',(4.810946174,4.04203077,-5.753676817));
#134263=CARTESIAN_POINT('Ctrl Pts',(5.389359975,4.172899507,-4.84946379100001));
#134264=CARTESIAN_POINT('Ctrl Pts',(5.125096127,4.107307013,-5.143148427));
#134265=CARTESIAN_POINT('Ctrl Pts',(4.83048412,4.04203077,-5.406378008));
#134266=CARTESIAN_POINT('',(5.40767664967603,4.17289950685236,-5.19682915561212));
#134267=CARTESIAN_POINT('Origin',(-0.13773348277981,4.16071402875705,0.135068604265487));
#134268=CARTESIAN_POINT('',(5.39851831441093,4.17289950678353,-5.023146470021));
#134269=CARTESIAN_POINT('Origin',(-1.61762964134837E-13,4.26419218499978,
1.77375475418629E-13));
#134270=CARTESIAN_POINT('',(4.99739295983041,4.26310680661695,-5.59250065718638));
#134271=CARTESIAN_POINT('Origin',(-0.115561917034222,4.1607171309572,0.153920221420748));
#134272=CARTESIAN_POINT('Origin',(-0.149426904978411,4.0179949497126,0.109346319510427));
#134273=CARTESIAN_POINT('Ctrl Pts',(6.228576794,4.042023177,-4.17789793));
#134274=CARTESIAN_POINT('Ctrl Pts',(6.00048323,4.10772842,-4.517948909));
#134275=CARTESIAN_POINT('Ctrl Pts',(5.736725335,4.172899507,-4.831147114));
#134276=CARTESIAN_POINT('Ctrl Pts',(5.88527009200001,4.042023177,-4.233922052));
#134277=CARTESIAN_POINT('Ctrl Pts',(5.654117875,4.10772842,-4.555230101));
#134278=CARTESIAN_POINT('Ctrl Pts',(5.389359975,4.172899507,-4.849463791));
#134279=CARTESIAN_POINT('',(5.73672532969533,4.17289950600421,-4.8311471225858));
#134280=CARTESIAN_POINT('',(5.563042643484,4.17289950413623,-4.84030546573553));
#134281=CARTESIAN_POINT('',(6.08554586918542,4.08221031174222,-4.38362081754647));
#134282=CARTESIAN_POINT('Origin',(-0.160566649509389,4.01787920792561,0.102927005237378));
#134283=CARTESIAN_POINT('Ctrl Pts',(5.88251005789048,4.0428073592437,-4.23775594170643));
#134284=CARTESIAN_POINT('Ctrl Pts',(5.91632472470477,4.04969801284624,-4.26199792235454));
#134285=CARTESIAN_POINT('Ctrl Pts',(5.95016921108538,4.05642175488811,-4.28628857520854));
#134286=CARTESIAN_POINT('Ctrl Pts',(6.01783610026202,4.06954550714686,-4.33490338265932));
#134287=CARTESIAN_POINT('Ctrl Pts',(6.05169656428838,4.0759528934186,-4.35925488582192));
#134288=CARTESIAN_POINT('Ctrl Pts',(6.08554587000034,4.08221031174209,-4.38362081641441));
#134289=CARTESIAN_POINT('Ctrl Pts',(6.39841282800001,4.172899507,-3.912839543));
#134290=CARTESIAN_POINT('Ctrl Pts',(6.18518883400001,4.107307013,-4.261510916));
#134291=CARTESIAN_POINT('Ctrl Pts',(5.935339364,4.04203077,-4.584947834));
#134292=CARTESIAN_POINT('Ctrl Pts',(6.30585110000001,4.172899507,-3.577532936));
#134293=CARTESIAN_POINT('Ctrl Pts',(6.110899109,4.107307013,-3.921160304));
#134294=CARTESIAN_POINT('Ctrl Pts',(5.879761546,4.04203077,-4.241568597));
#134295=CARTESIAN_POINT('',(6.3984128267292,4.17289950685238,-3.91283954796789));
#134296=CARTESIAN_POINT('Origin',(-0.163549219894527,4.16071400496938,0.102302234735868));
#134297=CARTESIAN_POINT('',(6.35213196467917,4.17289950678353,-3.74518623834807));
#134298=CARTESIAN_POINT('Origin',(-4.0766001685455E-13,4.26419218500044,
3.18321757841744E-13));
#134299=CARTESIAN_POINT('',(6.082779017676,4.26310680662323,-4.3874593349363));
#134300=CARTESIAN_POINT('Origin',(-0.145948342705643,4.16071718925756,0.125479155657017));
#134301=CARTESIAN_POINT('Origin',(-0.169439547415214,4.01799495272587,0.0746674649441564));
#134302=CARTESIAN_POINT('Ctrl Pts',(6.98108068700001,4.042023177,-2.741261103));
#134303=CARTESIAN_POINT('Ctrl Pts',(6.831420733,4.10772842,-3.122395253));
#134304=CARTESIAN_POINT('Ctrl Pts',(6.641157706,4.172899507,-3.484971208));
#134305=CARTESIAN_POINT('Ctrl Pts',(6.657843835,4.042023177,-2.869776205));
#134306=CARTESIAN_POINT('Ctrl Pts',(6.501167561,4.10772842,-3.233263144));
#134307=CARTESIAN_POINT('Ctrl Pts',(6.3058511,4.172899507,-3.577532936));
#134308=CARTESIAN_POINT('',(6.64115770268627,4.17289950600422,-3.48497121750205));
#134309=CARTESIAN_POINT('',(6.47350439459849,4.17289950413623,-3.53125208740169));
#134310=CARTESIAN_POINT('',(6.88561808514311,4.08221031165632,-2.97292172430832));
#134311=CARTESIAN_POINT('Origin',(-0.178938489425086,4.01787919383781,0.066003326674286));
#134312=CARTESIAN_POINT('Ctrl Pts',(6.65597250213183,4.04280735929249,-2.87411378637647));
#134313=CARTESIAN_POINT('Ctrl Pts',(6.69420791073327,4.0496980130125,-2.89051984944257));
#134314=CARTESIAN_POINT('Ctrl Pts',(6.73248290502452,4.05642175518567,-2.90696703653915));
#134315=CARTESIAN_POINT('Ctrl Pts',(6.80901852467154,4.06954550710853,-2.93989887499767));
#134316=CARTESIAN_POINT('Ctrl Pts',(6.8473222031756,4.07595289335837,-2.95640205462647));
#134317=CARTESIAN_POINT('Ctrl Pts',(6.8856180856794,4.0822103116562,-2.97292172306514));
#134318=CARTESIAN_POINT('Ctrl Pts',(7.08996633,4.172899507,-2.445889906));
#134319=CARTESIAN_POINT('Ctrl Pts',(6.95668143399999,4.107307013,-2.832246392));
#134320=CARTESIAN_POINT('Ctrl Pts',(6.782202682,4.04203077,-3.201831785));
#134321=CARTESIAN_POINT('Ctrl Pts',(6.927487635,4.172899507,-2.138320617));
#134322=CARTESIAN_POINT('Ctrl Pts',(6.81096324000001,4.107307013,-2.515823084));
#134323=CARTESIAN_POINT('Ctrl Pts',(6.654107857,4.04203077,-2.878428153));
#134324=CARTESIAN_POINT('',(7.08996632982761,4.17289950685234,-2.44588991117874));
#134325=CARTESIAN_POINT('Origin',(-0.181717264224633,4.16071400914111,0.0647521217746));
#134326=CARTESIAN_POINT('',(7.00872698291568,4.17289950678351,-2.29210526022896));
#134327=CARTESIAN_POINT('Origin',(3.30898503042576E-13,4.26419218499911,
-1.23599047663348E-13));
#134328=CARTESIAN_POINT('',(6.88374108936043,4.26310680610879,-2.97726529079439));
#134329=CARTESIAN_POINT('Origin',(-0.169510333814914,4.16071715532136,0.0911709032238156));
#134330=CARTESIAN_POINT('Origin',(-0.181529238467207,4.01799496167259,0.0364971912151618));
#134331=CARTESIAN_POINT('Ctrl Pts',(7.407157006,4.042023177,-1.176445953));
#134332=CARTESIAN_POINT('Ctrl Pts',(7.342928594,4.10772842,-1.580841865));
#134333=CARTESIAN_POINT('Ctrl Pts',(7.235056924,4.172899507,-1.975841922));
#134334=CARTESIAN_POINT('Ctrl Pts',(7.1191042,4.042023177,-1.371442812));
#134335=CARTESIAN_POINT('Ctrl Pts',(7.044229877,4.10772842,-1.760112396));
#134336=CARTESIAN_POINT('Ctrl Pts',(6.92748763500001,4.172899507,-2.138320617));
#134337=CARTESIAN_POINT('',(7.23505692281089,4.17289950600423,-1.97584193198538));
#134338=CARTESIAN_POINT('',(7.08127227460583,4.17289950413623,-2.05708128634764));
#134339=CARTESIAN_POINT('',(7.36372645293057,4.08221031170477,-1.42321211529242));
#134340=CARTESIAN_POINT('Origin',(-0.188944138865323,4.01787924544133,0.0259938208454624));
#134341=CARTESIAN_POINT('Ctrl Pts',(7.11820906946345,4.04280735927478,-1.37608126440439));
#134342=CARTESIAN_POINT('Ctrl Pts',(7.15907737229309,4.04969801268933,-1.38388427975716));
#134343=CARTESIAN_POINT('Ctrl Pts',(7.19999317533954,4.05642175451896,-1.39171894787107));
#134344=CARTESIAN_POINT('Ctrl Pts',(7.2818188109592,4.06954550713737,-1.40742796310531));
#134345=CARTESIAN_POINT('Ctrl Pts',(7.32277466663668,4.07595289339688,-1.41531114890485));
#134346=CARTESIAN_POINT('Ctrl Pts',(7.36372645319145,4.08221031170464,-1.42321211394033));
#134347=CARTESIAN_POINT('Ctrl Pts',(7.450000887,4.172899507,-0.864573176000001));
#134348=CARTESIAN_POINT('Ctrl Pts',(7.402887342,4.107307013,-1.270549175));
#134349=CARTESIAN_POINT('Ctrl Pts',(7.31193774100001,4.04203077,-1.669001641));
#134350=CARTESIAN_POINT('Ctrl Pts',(7.225202548,4.172899507,-0.599122803));
#134351=CARTESIAN_POINT('Ctrl Pts',(7.1925543,4.107307013,-0.992848772000001));
#134352=CARTESIAN_POINT('Ctrl Pts',(7.11731548,4.04203077,-1.380695607));
#134353=CARTESIAN_POINT('',(7.45000088794504,4.17289950685238,-0.864573181094501));
#134354=CARTESIAN_POINT('Origin',(-0.191388568438923,4.16071400365763,0.0241744027929161));
#134355=CARTESIAN_POINT('',(7.33760171763272,4.17289950678353,-0.731847988169358));
#134356=CARTESIAN_POINT('Origin',(-1.65752828129584E-12,4.264192185,3.55780942901118E-13));
#134357=CARTESIAN_POINT('',(7.36282707779088,4.26310680606226,-1.42785763063805));
#134358=CARTESIAN_POINT('Origin',(-0.185146489275991,4.16071714815283,0.0525997026355554));
#134359=CARTESIAN_POINT('Origin',(-0.18513120911127,4.01799500061643,-0.00337946912520898));
#134360=CARTESIAN_POINT('Ctrl Pts',(7.486882896,4.042023177,0.443378502));
#134361=CARTESIAN_POINT('Ctrl Pts',(7.511089276,4.10772842,0.034629932));
#134362=CARTESIAN_POINT('Ctrl Pts',(7.49065292200001,4.172899507,-0.374324464));
#134363=CARTESIAN_POINT('Ctrl Pts',(7.247483165,4.042023177,0.191017723));
#134364=CARTESIAN_POINT('Ctrl Pts',(7.25791183400001,4.10772842,-0.204660748));
#134365=CARTESIAN_POINT('Ctrl Pts',(7.225202548,4.172899507,-0.599122803));
#134366=CARTESIAN_POINT('',(7.49065292297682,4.17289950600421,-0.374324474032694));
#134367=CARTESIAN_POINT('',(7.35792773384199,4.17289950413623,-0.486723651005898));
#134368=CARTESIAN_POINT('',(7.49751515522338,4.08221031172839,0.193045309743851));
#134369=CARTESIAN_POINT('Origin',(-0.190114426969782,4.01787920023827,-0.0152313257799268));
#134370=CARTESIAN_POINT('Ctrl Pts',(7.24760609256059,4.04280735932244,0.186295288436253));
#134371=CARTESIAN_POINT('Ctrl Pts',(7.28919633568094,4.04969801290351,0.187460180072133));
#134372=CARTESIAN_POINT('Ctrl Pts',(7.33083977311272,4.05642175490914,0.188604370186818));
#134373=CARTESIAN_POINT('Ctrl Pts',(7.41412934245488,4.06954550718391,0.190852715569519));
#134374=CARTESIAN_POINT('Ctrl Pts',(7.45582232480963,4.07595289343287,0.191958132496257));
#134375=CARTESIAN_POINT('Ctrl Pts',(7.49751515518722,4.08221031172826,0.193045311131656));
#134376=CARTESIAN_POINT('Ctrl Pts',(7.461681683,4.172899507,0.757170034));
#134377=CARTESIAN_POINT('Ctrl Pts',(7.502942465,4.107307013,0.350557509));
#134378=CARTESIAN_POINT('Ctrl Pts',(7.499774717,4.04203077,-0.058130836));
#134379=CARTESIAN_POINT('Ctrl Pts',(7.185075021,4.172899507,0.968089328));
#134380=CARTESIAN_POINT('Ctrl Pts',(7.237829515,4.107307013,0.576550044));
#134381=CARTESIAN_POINT('Ctrl Pts',(7.247725342,4.04203077,0.181596731));
#134382=CARTESIAN_POINT('',(7.46168168499956,4.17289950692262,0.757170029229101));
#134383=CARTESIAN_POINT('Origin',(-0.192110981246819,4.16071410180708,-0.0175336851590434));
#134384=CARTESIAN_POINT('',(7.32337835184357,4.17289950678352,0.862629682328062));
#134385=CARTESIAN_POINT('Origin',(-1.01394587170844E-12,4.264192185,-4.13352078260099E-14));
#134386=CARTESIAN_POINT('',(7.49763545621552,4.26310680660134,0.188315065718333));
#134387=CARTESIAN_POINT('Origin',(-0.192125296875894,4.16071714821591,0.0115689275453297));
#134388=CARTESIAN_POINT('Origin',(-0.18007633025845,4.01799492518908,-0.0430982007787728));
#134389=CARTESIAN_POINT('Ctrl Pts',(7.216530463,4.042023177,2.042471071));
#134390=CARTESIAN_POINT('Ctrl Pts',(7.328039771,4.10772842,1.648482471));
#134391=CARTESIAN_POINT('Ctrl Pts',(7.395994314,4.172899507,1.24469599));
#134392=CARTESIAN_POINT('Ctrl Pts',(7.036977872,4.042023177,1.744546481));
#134393=CARTESIAN_POINT('Ctrl Pts',(7.1322219,4.10772842,1.360360608));
#134394=CARTESIAN_POINT('Ctrl Pts',(7.185075021,4.172899507,0.968089328));
#134395=CARTESIAN_POINT('',(7.39599431711138,4.17289950600422,1.24469598041833));
#134396=CARTESIAN_POINT('',(7.29053467013232,4.17289950413623,1.10639264165444));
#134397=CARTESIAN_POINT('',(7.28072838184259,4.0822103116604,1.80027615080325));
#134398=CARTESIAN_POINT('Origin',(-0.18239528671673,4.01787920662655,-0.0557441918224923));
#134399=CARTESIAN_POINT('Ctrl Pts',(7.03811310959639,4.04280735930236,1.73996088057068));
#134400=CARTESIAN_POINT('Ctrl Pts',(7.07848058142537,4.04969801334083,1.75003921115477));
#134401=CARTESIAN_POINT('Ctrl Pts',(7.11890445475128,4.05642175586792,1.76010875955354));
#134402=CARTESIAN_POINT('Ctrl Pts',(7.19976342610926,4.06954550711907,1.78020933350753));
#134403=CARTESIAN_POINT('Ctrl Pts',(7.24024401768039,4.07595289336593,1.79025166508122));
#134404=CARTESIAN_POINT('Ctrl Pts',(7.28072838151672,4.08221031166027,1.80027615211935));
#134405=CARTESIAN_POINT('Ctrl Pts',(7.124462536,4.172899507,2.343508816));
#134406=CARTESIAN_POINT('Ctrl Pts',(7.252168337,4.107307013,1.955272514));
#134407=CARTESIAN_POINT('Ctrl Pts',(7.336930563,4.04203077,1.555458103));
#134408=CARTESIAN_POINT('Ctrl Pts',(6.80898137100001,4.172899507,2.490034677));
#134409=CARTESIAN_POINT('Ctrl Pts',(6.944671867,4.107307013,2.118990022));
#134410=CARTESIAN_POINT('Ctrl Pts',(7.039239622,4.04203077,1.735397808));
#134411=CARTESIAN_POINT('',(7.12446253898564,4.17289950685236,2.34350881178721));
#134412=CARTESIAN_POINT('Origin',(-0.18385034724122,4.16071403008887,-0.058421934317176));
#134413=CARTESIAN_POINT('',(6.96672195306173,4.17289950678352,2.41677174776338));
#134414=CARTESIAN_POINT('Origin',(9.11163505756818E-13,4.264192185,2.70183181383388E-13));
#134415=CARTESIAN_POINT('',(7.28186273324354,4.26310680661245,1.79568235838605));
#134416=CARTESIAN_POINT('Origin',(-0.190120374725622,4.16071715608105,-0.0300027826587959));
#134417=CARTESIAN_POINT('Origin',(-0.166601488256943,4.01799499817148,-0.0808016891777477));
#134418=CARTESIAN_POINT('Ctrl Pts',(6.608741086,4.042023177,3.546059963));
#134419=CARTESIAN_POINT('Ctrl Pts',(6.802339271,4.10772842,3.185253802));
#134420=CARTESIAN_POINT('Ctrl Pts',(6.95550723200001,4.172899507,2.805515843));
#134421=CARTESIAN_POINT('Ctrl Pts',(6.497431315,4.042023177,3.216502185));
#134422=CARTESIAN_POINT('Ctrl Pts',(6.673037196,4.10772842,2.861773014));
#134423=CARTESIAN_POINT('Ctrl Pts',(6.808981371,4.172899507,2.490034677));
#134424=CARTESIAN_POINT('',(6.95550723709794,4.17289950600422,2.80551583431232));
#134425=CARTESIAN_POINT('',(6.88224430779956,4.17289950413623,2.64777524362585));
#134426=CARTESIAN_POINT('',(6.72350284208098,4.08221031170637,3.32332808042156));
#134427=CARTESIAN_POINT('Origin',(-0.166147856588221,4.01787924998038,-0.0936506027297385));
#134428=CARTESIAN_POINT('Ctrl Pts',(6.49952577937696,4.04280735929061,3.21226783447011));
#134429=CARTESIAN_POINT('Ctrl Pts',(6.53678293033991,4.04969801171788,3.23078834846234));
#134430=CARTESIAN_POINT('Ctrl Pts',(6.57409705013473,4.05642175244788,3.24931240921773));
#134431=CARTESIAN_POINT('Ctrl Pts',(6.64874457416989,4.06954550713273,3.28632534165753));
#134432=CARTESIAN_POINT('Ctrl Pts',(6.68611994776028,4.07595289339519,3.30483501987673));
#134433=CARTESIAN_POINT('Ctrl Pts',(6.72350284147008,4.08221031170624,3.32332808165651));
#134434=CARTESIAN_POINT('Ctrl Pts',(6.45411144,4.172899507,3.82026773));
#134435=CARTESIAN_POINT('Ctrl Pts',(6.662290879,4.107307013,3.468561149));
#134436=CARTESIAN_POINT('Ctrl Pts',(6.83101969100001,4.04203077,3.09631555));
#134437=CARTESIAN_POINT('Ctrl Pts',(6.114507319,4.172899507,3.895548773));
#134438=CARTESIAN_POINT('Ctrl Pts',(6.32678908000001,4.107307013,3.562348381));
#134439=CARTESIAN_POINT('Ctrl Pts',(6.50160688,4.04203077,3.208053611));
#134440=CARTESIAN_POINT('',(6.45411144382979,4.17289950685223,3.82026772651186));
#134441=CARTESIAN_POINT('Origin',(-0.166993061533895,4.16071401829543,-0.0965784589115737));
#134442=CARTESIAN_POINT('',(6.28430937880036,4.17289950678351,3.85790825263968));
#134443=CARTESIAN_POINT('Origin',(2.77555756156289E-13,4.26419218499978,
1.33790548084711E-13));
#134444=CARTESIAN_POINT('',(6.72559820178816,4.26310680658169,3.31908553998013));
#134445=CARTESIAN_POINT('Origin',(-0.179225866214101,4.16071716216026,-0.0701716498773386));
#134446=CARTESIAN_POINT('Origin',(-0.145336718269771,4.01799492185903,-0.114727121590696));
#134447=CARTESIAN_POINT('Ctrl Pts',(5.691934321,4.042023177,4.883839032));
#134448=CARTESIAN_POINT('Ctrl Pts',(5.95856894700001,4.10772842,4.573086206));
#134449=CARTESIAN_POINT('Ctrl Pts',(6.189788363,4.172899507,4.235152893));
#134450=CARTESIAN_POINT('Ctrl Pts',(5.654072091,4.042023177,4.538057821));
#134451=CARTESIAN_POINT('Ctrl Pts',(5.90182869,4.10772842,4.229372095));
#134452=CARTESIAN_POINT('Ctrl Pts',(6.114507319,4.172899507,3.895548773));
#134453=CARTESIAN_POINT('',(6.18978836985319,4.17289950600421,4.23515288559372));
#134454=CARTESIAN_POINT('',(6.15214785067221,4.17289950413623,4.06535081836292));
#134455=CARTESIAN_POINT('',(5.85189378122471,4.08221031161528,4.69098488189386));
#134456=CARTESIAN_POINT('Origin',(-0.142131104059078,4.01787918315488,-0.127177865467208));
#134457=CARTESIAN_POINT('Ctrl Pts',(5.65702784793379,4.04280735922081,4.53437271583437));
#134458=CARTESIAN_POINT('Ctrl Pts',(5.6894325894266,4.04969801272765,4.56046942051071));
#134459=CARTESIAN_POINT('Ctrl Pts',(5.72189220651359,4.05642175465624,4.58658183659266));
#134460=CARTESIAN_POINT('Ctrl Pts',(5.78683781525976,4.06954550706718,4.63877642906093));
#134461=CARTESIAN_POINT('Ctrl Pts',(5.8193603396521,4.07595289331887,4.66488796167648));
#134462=CARTESIAN_POINT('Ctrl Pts',(5.8518937803898,4.08221031161516,4.69098488293473));
#134463=CARTESIAN_POINT('Ctrl Pts',(5.481973265,4.172899507,5.11839517));
#134464=CARTESIAN_POINT('Ctrl Pts',(5.760892103,4.107307013,4.81966372));
#134465=CARTESIAN_POINT('Ctrl Pts',(6.005697929,4.04203077,4.492392723));
#134466=CARTESIAN_POINT('Ctrl Pts',(5.134125702,4.172899507,5.118911337));
#134467=CARTESIAN_POINT('Ctrl Pts',(5.413072667,4.107307013,4.839135289));
#134468=CARTESIAN_POINT('Ctrl Pts',(5.659966227,4.04203077,4.530704394));
#134469=CARTESIAN_POINT('',(5.48197326948944,4.17289950685236,5.11839516742479));
#134470=CARTESIAN_POINT('Origin',(-0.14232717713363,4.16071403116877,-0.130218946123016));
#134471=CARTESIAN_POINT('',(5.30804948257176,4.17289950678352,5.11865325446259));
#134472=CARTESIAN_POINT('Origin',(-5.24753851482984E-14,4.26419218500022,
2.34187669256869E-14));
#134473=CARTESIAN_POINT('',(5.85485217362851,4.26310680661815,4.68729197077568));
#134474=CARTESIAN_POINT('Origin',(-0.159950766863188,4.16071718815307,-0.107059299983618));
#134475=CARTESIAN_POINT('Origin',(-0.117275699508936,4.01799490700237,-0.143287822644464));
#134476=CARTESIAN_POINT('Ctrl Pts',(4.508979033,4.042023177,5.993255216));
#134477=CARTESIAN_POINT('Ctrl Pts',(4.836182561,4.10772842,5.747086181));
#134478=CARTESIAN_POINT('Ctrl Pts',(5.134641869,4.172899507,5.466758901));
#134479=CARTESIAN_POINT('Ctrl Pts',(4.54633474,4.042023177,5.647418918));
#134480=CARTESIAN_POINT('Ctrl Pts',(4.854657234,4.10772842,5.399210438));
#134481=CARTESIAN_POINT('Ctrl Pts',(5.134125702,4.172899507,5.118911337));
#134482=CARTESIAN_POINT('',(5.13464187728293,4.17289950600421,5.46675889524292));
#134483=CARTESIAN_POINT('',(5.13438379809265,4.17289950413623,5.29283510678433));
#134484=CARTESIAN_POINT('',(4.70665667160418,4.0822103116914,5.83929644515874));
#134485=CARTESIAN_POINT('Origin',(-0.111469018216903,4.01787921396925,-0.154758873994295));
#134486=CARTESIAN_POINT('Ctrl Pts',(4.55001358209104,4.0428073593046,5.64445536825661));
#134487=CARTESIAN_POINT('Ctrl Pts',(4.57605069418501,4.049698011634,5.67690800270813));
#134488=CARTESIAN_POINT('Ctrl Pts',(4.60213802041595,4.05642175225397,5.70938777661076));
#134489=CARTESIAN_POINT('Ctrl Pts',(4.6543449520232,4.06954550710832,5.77432348696933));
#134490=CARTESIAN_POINT('Ctrl Pts',(4.68049391020144,4.07595289337418,5.80681592801612));
#134491=CARTESIAN_POINT('Ctrl Pts',(4.70665667053675,4.08221031169127,5.83929644601857));
#134492=CARTESIAN_POINT('Ctrl Pts',(4.253504114,4.172899507,6.177192142));
#134493=CARTESIAN_POINT('Ctrl Pts',(4.590120416,4.107307013,5.94540417200001));
#134494=CARTESIAN_POINT('Ctrl Pts',(4.899556408,4.04203077,5.678410606));
#134495=CARTESIAN_POINT('Ctrl Pts',(3.913678072,4.172899507,6.102919297));
#134496=CARTESIAN_POINT('Ctrl Pts',(4.246246993,4.107307013,5.889649609));
#134497=CARTESIAN_POINT('Ctrl Pts',(4.553671844,4.04203077,5.641504474));
#134498=CARTESIAN_POINT('',(4.25350411889082,4.17289950685237,6.1771921404623));
#134499=CARTESIAN_POINT('Origin',(-0.111006536517217,4.16071400427737,-0.157770777196192));
#134500=CARTESIAN_POINT('',(4.08359109188653,4.17289950678353,6.14005572024055));
#134501=CARTESIAN_POINT('Origin',(8.32667268468867E-14,4.26419218500044,
1.6002824065886E-13));
#134502=CARTESIAN_POINT('',(4.71033976528965,4.26310680660776,5.83632583827294));
#134503=CARTESIAN_POINT('Origin',(-0.133196765032976,4.16071716528115,-0.138941155871057));
#134504=CARTESIAN_POINT('Origin',(-0.0837313970627712,4.01799493508786,
-0.165148863663684));
#134505=CARTESIAN_POINT('Ctrl Pts',(3.115188897,4.042023177,6.822433447));
#134506=CARTESIAN_POINT('Ctrl Pts',(3.487661654,4.10772842,6.652358794));
#134507=CARTESIAN_POINT('Ctrl Pts',(3.839405228,4.172899507,6.442745339));
#134508=CARTESIAN_POINT('Ctrl Pts',(3.226015829,4.042023177,6.492712982));
#134509=CARTESIAN_POINT('Ctrl Pts',(3.580487401,4.10772842,6.316587701));
#134510=CARTESIAN_POINT('Ctrl Pts',(3.913678072,4.172899507,6.102919297));
#134511=CARTESIAN_POINT('',(3.8394052373347,4.17289950600421,6.44274533515021));
#134512=CARTESIAN_POINT('',(3.87654166492425,4.17289950413623,6.27283230877697));
#134513=CARTESIAN_POINT('',(3.34134152675702,4.08221031164381,6.71456899555679));
#134514=CARTESIAN_POINT('Origin',(-0.0755942808618143,4.01787919564236,
-0.175103132993055));
#134515=CARTESIAN_POINT('Ctrl Pts',(3.23024573729236,4.04280735935761,6.49060956175588));
#134516=CARTESIAN_POINT('Ctrl Pts',(3.24869776186493,4.04969801266095,6.52790068627852));
#134517=CARTESIAN_POINT('Ctrl Pts',(3.26719299297759,4.05642175437212,6.56522911152584));
#134518=CARTESIAN_POINT('Ctrl Pts',(3.30422009156699,4.0695455071151,6.63986959601397));
#134519=CARTESIAN_POINT('Ctrl Pts',(3.32277278728129,4.0759528933535,6.67722363469553));
#134520=CARTESIAN_POINT('Ctrl Pts',(3.34134152555005,4.08221031164368,6.71456899615694));
#134521=CARTESIAN_POINT('Ctrl Pts',(2.826145837,4.172899507,6.947150474));
#134522=CARTESIAN_POINT('Ctrl Pts',(3.204719799,4.107307013,6.793144133));
#134523=CARTESIAN_POINT('Ctrl Pts',(3.564317074,4.04203077,6.598912319));
#134524=CARTESIAN_POINT('Ctrl Pts',(2.510231206,4.172899507,6.801561533));
#134525=CARTESIAN_POINT('Ctrl Pts',(2.880871529,4.107307013,6.66477046000001));
#134526=CARTESIAN_POINT('Ctrl Pts',(3.234452827,4.04203077,6.488514076));
#134527=CARTESIAN_POINT('',(2.82614584213299,4.17289950685239,6.9471504735488));
#134528=CARTESIAN_POINT('Origin',(-0.0744951406898375,4.16071401400292,
-0.177945158959567));
#134529=CARTESIAN_POINT('',(2.66818852025341,4.17289950678353,6.87435600398385));
#134530=CARTESIAN_POINT('Origin',(1.83880688453542E-13,4.26419218500044,
1.34007388519208E-13));
#134531=CARTESIAN_POINT('',(3.34557710444455,4.26310680660674,6.71245959639363));
#134532=CARTESIAN_POINT('Origin',(-0.100214494169487,4.16071715590041,-0.164326227237381));
#134533=CARTESIAN_POINT('Origin',(-0.0462715741382319,4.01799497278107,
-0.179287317113798));
#134534=CARTESIAN_POINT('Ctrl Pts',(1.57573599,4.042023177,7.332602273));
#134535=CARTESIAN_POINT('Ctrl Pts',(1.976061564,4.10772842,7.24657450400001));
#134536=CARTESIAN_POINT('Ctrl Pts',(2.364642265,4.172899507,7.117476165));
#134537=CARTESIAN_POINT('Ctrl Pts',(1.754852004,4.042023177,7.034415004));
#134538=CARTESIAN_POINT('Ctrl Pts',(2.138897957,4.10772842,6.938608343));
#134539=CARTESIAN_POINT('Ctrl Pts',(2.510231206,4.172899507,6.801561533));
#134540=CARTESIAN_POINT('',(2.36464227492406,4.17289950600422,7.11747616326049));
#134541=CARTESIAN_POINT('',(2.43743675205796,4.17289950413623,6.95951884320089));
#134542=CARTESIAN_POINT('',(1.8197889658224,4.08221031167589,7.27587576289585));
#134543=CARTESIAN_POINT('Origin',(-0.0361848468469295,4.0178791970496,-0.187259532776093));
#134544=CARTESIAN_POINT('Ctrl Pts',(1.75943519295772,4.04280735931344,7.03327006476682));
#134545=CARTESIAN_POINT('Ctrl Pts',(1.76943932797021,4.04969801137569,7.0736559761413));
#134546=CARTESIAN_POINT('Ctrl Pts',(1.77947764045624,4.0564217516996,7.11408760265159));
#134547=CARTESIAN_POINT('Ctrl Pts',(1.79959357205713,4.06954550710117,7.19494278222298));
#134548=CARTESIAN_POINT('Ctrl Pts',(1.80968250185344,4.07595289336307,7.23541178557499));
#134549=CARTESIAN_POINT('Ctrl Pts',(1.81978896449978,4.08221031167577,7.27587576322622));
#134550=CARTESIAN_POINT('Ctrl Pts',(1.266640122,4.172899507,7.392267771));
#134551=CARTESIAN_POINT('Ctrl Pts',(1.669470046,4.107307013,7.323244224));
#134552=CARTESIAN_POINT('Ctrl Pts',(2.062414236,4.04203077,7.210856227));
#134553=CARTESIAN_POINT('Ctrl Pts',(0.989408718000001,4.172899507,7.18217031200001));
#134554=CARTESIAN_POINT('Ctrl Pts',(1.380789714,4.107307013,7.128254051));
#134555=CARTESIAN_POINT('Ctrl Pts',(1.76399439,4.04203077,7.03212797));
#134556=CARTESIAN_POINT('',(1.26664012712354,4.1728995068524,7.39226777166522));
#134557=CARTESIAN_POINT('Origin',(-0.0345005551398,4.16071403657584,-0.189799287105015));
#134558=CARTESIAN_POINT('',(1.12802441867854,4.17289950678353,7.28721904170456));
#134559=CARTESIAN_POINT('Origin',(1.58293517182884E-14,4.26419218500133,
-3.62557206479153E-13));
#134560=CARTESIAN_POINT('',(1.8243789766821,4.26310680660485,7.27472620408612));
#134561=CARTESIAN_POINT('Origin',(-0.0625461994119189,4.16071710752316,
-0.182027287696495));
#134562=CARTESIAN_POINT('Origin',(-0.00664832895622192,4.0179949497113,
-0.185042884422192));
#134563=CARTESIAN_POINT('Ctrl Pts',(-0.03739658,4.042023177,7.499906766));
#134564=CARTESIAN_POINT('Ctrl Pts',(0.372063032,4.10772842,7.50194844300001));
#134565=CARTESIAN_POINT('Ctrl Pts',(0.779311259,4.172899507,7.459401716));
#134566=CARTESIAN_POINT('Ctrl Pts',(0.201633249,4.042023177,7.247195598));
#134567=CARTESIAN_POINT('Ctrl Pts',(0.597296021,4.10772842,7.236187371));
#134568=CARTESIAN_POINT('Ctrl Pts',(0.989408718,4.172899507,7.18217031200001));
#134569=CARTESIAN_POINT('',(0.779311269060809,4.17289950600422,7.4594017164365));
#134570=CARTESIAN_POINT('',(0.884360005917485,4.17289950413623,7.32078601189595));
#134571=CARTESIAN_POINT('',(0.21314509586863,4.08221031164964,7.49697066538411));
#134572=CARTESIAN_POINT('Origin',(0.00491640757449785,4.01787918214174,
-0.190660168586786));
#134573=CARTESIAN_POINT('Ctrl Pts',(0.206355413397366,4.04280735932038,
7.24706267725279));
#134574=CARTESIAN_POINT('Ctrl Pts',(0.207443880494177,4.04969801231471,
7.28865498727906));
#134575=CARTESIAN_POINT('Ctrl Pts',(0.208555898644855,4.05642175367949,
7.33029929207554));
#134576=CARTESIAN_POINT('Ctrl Pts',(0.210820057400983,4.06954550711118,
7.41358844048726));
#134577=CARTESIAN_POINT('Ctrl Pts',(0.211973474311316,4.07595289335646,
7.45528012253599));
#134578=CARTESIAN_POINT('Ctrl Pts',(0.213145094518449,4.08221031164952,
7.49697066542207));
#134579=CARTESIAN_POINT('Ctrl Pts',(-0.352092277,4.172899507,7.49173084300001));
#134580=CARTESIAN_POINT('Ctrl Pts',(0.0561577300000001,4.107307013,7.510917554));
#134581=CARTESIAN_POINT('Ctrl Pts',(0.4640752,4.04203077,7.485628511));
#134582=CARTESIAN_POINT('Ctrl Pts',(-0.577677421000001,4.172899507,7.226948789));
#134583=CARTESIAN_POINT('Ctrl Pts',(-0.183856294,4.107307013,7.258428405));
#134584=CARTESIAN_POINT('Ctrl Pts',(0.211053536,4.04203077,7.246927377));
#134585=CARTESIAN_POINT('',(-0.352092272134449,4.17289950685238,7.49173084475307));
#134586=CARTESIAN_POINT('Origin',(0.00710727529755324,4.160714013686,-0.192778466708976));
#134587=CARTESIAN_POINT('',(-0.464884850334537,4.17289950678353,7.3593398159157));
#134588=CARTESIAN_POINT('Origin',(-3.27700106633744E-14,4.26419218499956,
2.03830008427275E-13));
#134589=CARTESIAN_POINT('',(0.217874915136567,4.26310680605619,7.49683469969476));
#134590=CARTESIAN_POINT('Origin',(-0.0219534128396459,4.16071715851607,
-0.191217207783373));
#134591=CARTESIAN_POINT('Origin',(0.0332858491263909,4.01799497996062,-0.182145603627001));
#134592=CARTESIAN_POINT('Ctrl Pts',(0.458515569029856,1.71660033198358,
7.48597550365515));
#134593=CARTESIAN_POINT('Ctrl Pts',(0.462562578514928,1.71596185949179,
7.48572323182757));
#134594=CARTESIAN_POINT('Ctrl Pts',(0.466609588,1.715323387,7.48547096));
#134595=CARTESIAN_POINT('Ctrl Pts',(0.873461406,1.651136808,7.46010970200001));
#134596=CARTESIAN_POINT('Ctrl Pts',(1.275167733,1.585954698,7.39080153));
#134597=CARTESIAN_POINT('Ctrl Pts',(0.205671117258217,1.71660033198358,
7.24708636966053));
#134598=CARTESIAN_POINT('Ctrl Pts',(0.209589119629109,1.71596185949179,
7.24697093733027));
#134599=CARTESIAN_POINT('Ctrl Pts',(0.213507122,1.715323387,7.246855505));
#134600=CARTESIAN_POINT('Ctrl Pts',(0.607389665,1.651136808,7.235250923));
#134601=CARTESIAN_POINT('Ctrl Pts',(0.997694124000001,1.585954698,7.18102405200001));
#134602=CARTESIAN_POINT('',(0.993027300490256,1.58673401522208,7.18167089043044));
#134603=CARTESIAN_POINT('Origin',(-0.043636971062415,1.48222902514883,-0.188849083665119));
#134604=CARTESIAN_POINT('Ctrl Pts',(1.02948254309185,1.62564958676913,7.42900839219714));
#134605=CARTESIAN_POINT('Ctrl Pts',(1.02534588378697,1.62139779886715,7.40060352041928));
#134606=CARTESIAN_POINT('Ctrl Pts',(1.02118591211148,1.61707840871591,7.37221205908516));
#134607=CARTESIAN_POINT('Ctrl Pts',(1.01700107867271,1.61268792538597,7.34383535412214));
#134608=CARTESIAN_POINT('Ctrl Pts',(1.01301187494507,1.60850268534662,7.3167851838172));
#134609=CARTESIAN_POINT('Ctrl Pts',(1.00899401265604,1.60425381504717,7.28974898488846));
#134610=CARTESIAN_POINT('Ctrl Pts',(1.00499516686957,1.59993003804733,7.26272204028933));
#134611=CARTESIAN_POINT('Ctrl Pts',(1.00099621028148,1.59560614124254,7.2356943468168));
#134612=CARTESIAN_POINT('Ctrl Pts',(0.99700672008524,1.59120881937225,7.208676889702));
#134613=CARTESIAN_POINT('Ctrl Pts',(0.993027296840828,1.5867340161625,7.18167089110788));
#134614=CARTESIAN_POINT('Ctrl Pts',(0.778213576,1.585967065,7.45951631300001));
#134615=CARTESIAN_POINT('Ctrl Pts',(0.845381055,1.59657582,7.45250907));
#134616=CARTESIAN_POINT('Ctrl Pts',(0.912411464,1.607142857,7.444293474));
#134617=CARTESIAN_POINT('Ctrl Pts',(1.252691653,1.660786473,7.402586957));
#134618=CARTESIAN_POINT('Ctrl Pts',(1.587747952,1.715323387,7.330010671));
#134619=CARTESIAN_POINT('Ctrl Pts',(1.59177351427215,1.71597862537066,7.32913869706712));
#134620=CARTESIAN_POINT('Ctrl Pts',(1.59579907654429,1.71663386374133,7.32826672313425));
#134621=CARTESIAN_POINT('Ctrl Pts',(0.988351829,1.585967065,7.182315829));
#134622=CARTESIAN_POINT('Ctrl Pts',(1.053023321,1.59657582,7.173416445));
#134623=CARTESIAN_POINT('Ctrl Pts',(1.117524075,1.607142857,7.163353959));
#134624=CARTESIAN_POINT('Ctrl Pts',(1.444962461,1.660786473,7.112271703));
#134625=CARTESIAN_POINT('Ctrl Pts',(1.766375162,1.715323387,7.03153033));
#134626=CARTESIAN_POINT('Ctrl Pts',(1.77023680210883,1.71597862537066,7.03056025593805));
#134627=CARTESIAN_POINT('Ctrl Pts',(1.77409844221766,1.71663386374133,7.02959018187611));
#134628=CARTESIAN_POINT('Ctrl Pts',(1.7663751461876,1.71532338431697,7.0315303339722));
#134629=CARTESIAN_POINT('Ctrl Pts',(1.62199423020245,1.69082500709975,7.0677999438676));
#134630=CARTESIAN_POINT('Ctrl Pts',(1.47679252529511,1.66647815902139,7.09954383997699));
#134631=CARTESIAN_POINT('Ctrl Pts',(1.33119287040896,1.64234940160257,7.12674017636573));
#134632=CARTESIAN_POINT('Ctrl Pts',(1.26004864791652,1.63055938954785,7.14002909664876));
#134633=CARTESIAN_POINT('Ctrl Pts',(1.18880939776744,1.61882139759851,7.15223304210549));
#134634=CARTESIAN_POINT('Ctrl Pts',(1.1175240745291,1.60714285692684,7.16335395910296));
#134635=CARTESIAN_POINT('Ctrl Pts',(1.07611863033894,1.60035948101443,7.16981344483863));
#134636=CARTESIAN_POINT('Ctrl Pts',(1.03461671586149,1.59355605143323,7.17592022024356));
#134637=CARTESIAN_POINT('Ctrl Pts',(0.993027300662214,1.58673401459539,
7.18167089093061));
#134638=CARTESIAN_POINT('Ctrl Pts',(2.05705917966293,1.71660033198358,7.21239026252005));
#134639=CARTESIAN_POINT('Ctrl Pts',(2.06095734133147,1.71596185949179,7.21127390126003));
#134640=CARTESIAN_POINT('Ctrl Pts',(2.064855503,1.715323387,7.21015754));
#134641=CARTESIAN_POINT('Ctrl Pts',(2.456743431,1.651136808,7.0979281));
#134642=CARTESIAN_POINT('Ctrl Pts',(2.834158878,1.585954698,6.94388532800001));
#134643=CARTESIAN_POINT('Ctrl Pts',(1.75877198777081,1.71660033198358,7.03344030656226));
#134644=CARTESIAN_POINT('Ctrl Pts',(1.7625735748854,1.71596185949179,7.03248531828113));
#134645=CARTESIAN_POINT('Ctrl Pts',(1.766375162,1.715323387,7.03153033));
#134646=CARTESIAN_POINT('Ctrl Pts',(2.148554308,1.651136808,6.93552395300001));
#134647=CARTESIAN_POINT('Ctrl Pts',(2.518076491,1.585954698,6.798660955));
#134648=CARTESIAN_POINT('',(2.51365782700824,1.5867340152172,6.80029590006137));
#134649=CARTESIAN_POINT('Origin',(-0.0832136971996106,1.48222899362148,
-0.175053107338738));
#134650=CARTESIAN_POINT('Ctrl Pts',(2.60243101783764,1.62564958677363,7.03401398873212));
#134651=CARTESIAN_POINT('Ctrl Pts',(2.59228486354879,1.62139779887973,7.00716246659475));
#134652=CARTESIAN_POINT('Ctrl Pts',(2.58211882471485,1.6170784087356,6.98032905281386));
#134653=CARTESIAN_POINT('Ctrl Pts',(2.57193167755893,1.61268792541243,6.95351539495929));
#134654=CARTESIAN_POINT('Ctrl Pts',(2.56222075215246,1.60850268538428,6.92795520354208));
#134655=CARTESIAN_POINT('Ctrl Pts',(2.55248484170892,1.60425381508471,6.90241481758498));
#134656=CARTESIAN_POINT('Ctrl Pts',(2.54276949248601,1.59993003809904,6.87687938164382));
#134657=CARTESIAN_POINT('Ctrl Pts',(2.53305387406628,1.59560614130841,6.85134323815648));
#134658=CARTESIAN_POINT('Ctrl Pts',(2.52334970118557,1.59120881945939,6.82581505672652));
#134659=CARTESIAN_POINT('Ctrl Pts',(2.51365782285346,1.58673401618092,6.80029590129333));
#134660=CARTESIAN_POINT('Ctrl Pts',(2.363594881,1.585967065,7.117824052));
#134661=CARTESIAN_POINT('Ctrl Pts',(2.427685672,1.59657582,7.096541612));
#134662=CARTESIAN_POINT('Ctrl Pts',(2.491382836,1.607142857,7.074108535));
#134663=CARTESIAN_POINT('Ctrl Pts',(2.814741796,1.660786473,6.96022691200001));
#134664=CARTESIAN_POINT('Ctrl Pts',(3.126362908,1.715323387,6.817320219));
#134665=CARTESIAN_POINT('Ctrl Pts',(3.13010690623377,1.71597862537066,6.81560325443765));
#134666=CARTESIAN_POINT('Ctrl Pts',(3.13385090446755,1.71663386374133,6.81388628987529));
#134667=CARTESIAN_POINT('Ctrl Pts',(2.509230308,1.585967065,6.801930848));
#134668=CARTESIAN_POINT('Ctrl Pts',(2.570476711,1.59657582,6.779337068));
#134669=CARTESIAN_POINT('Ctrl Pts',(2.631306337,1.607142857,6.755644082));
#134670=CARTESIAN_POINT('Ctrl Pts',(2.940108221,1.660786473,6.635366527));
#134671=CARTESIAN_POINT('Ctrl Pts',(3.236649463,1.715323387,6.487418613));
#134672=CARTESIAN_POINT('Ctrl Pts',(3.24021228285891,1.71597862537066,6.48564108026112));
#134673=CARTESIAN_POINT('Ctrl Pts',(3.24377510271782,1.71663386374133,6.48386354752224));
#134674=CARTESIAN_POINT('Ctrl Pts',(3.23664944837323,1.71532338430999,6.48741862029747));
#134675=CARTESIAN_POINT('Ctrl Pts',(3.10344096466667,1.69082500573501,6.55387789944305));
#134676=CARTESIAN_POINT('Ctrl Pts',(2.96845798684327,1.66647815635029,6.61609371823778));
#134677=CARTESIAN_POINT('Ctrl Pts',(2.83210877192866,1.64234939768718,6.67395384374131));
#134678=CARTESIAN_POINT('Ctrl Pts',(2.7654845940745,1.6305593869447,6.70222597786856));
#134679=CARTESIAN_POINT('Ctrl Pts',(2.6985343728361,1.61882139630545,6.72945893164121));
#134680=CARTESIAN_POINT('Ctrl Pts',(2.63130633664155,1.60714285693915,6.75564408215498));
#134681=CARTESIAN_POINT('Ctrl Pts',(2.59225752655057,1.60035948100455,6.7708534952413));
#134682=CARTESIAN_POINT('Ctrl Pts',(2.55303868056522,1.5935560515235,6.78573918205019));
#134683=CARTESIAN_POINT('Ctrl Pts',(2.51365782710389,1.58673401460554,6.80029590003346));
#134684=CARTESIAN_POINT('Ctrl Pts',(3.55941698871103,1.71660033198358,6.6015616687789));
#134685=CARTESIAN_POINT('Ctrl Pts',(3.56298402885552,1.71596185949179,6.59963341788945));
#134686=CARTESIAN_POINT('Ctrl Pts',(3.566551069,1.715323387,6.59770516700001));
#134687=CARTESIAN_POINT('Ctrl Pts',(3.925150863,1.651136808,6.403855268));
#134688=CARTESIAN_POINT('Ctrl Pts',(4.260627904,1.585954698,6.172280767));
#134689=CARTESIAN_POINT('Ctrl Pts',(3.22963463525794,1.71660033198358,6.49091839309238));
#134690=CARTESIAN_POINT('Ctrl Pts',(3.23314204912897,1.71596185949179,6.48916850304618));
#134691=CARTESIAN_POINT('Ctrl Pts',(3.236649463,1.715323387,6.487418613));
#134692=CARTESIAN_POINT('Ctrl Pts',(3.58925494,1.651136808,6.311499592));
#134693=CARTESIAN_POINT('Ctrl Pts',(3.9207164,1.585954698,6.098400028));
#134694=CARTESIAN_POINT('',(3.91675250661477,1.58673401523444,6.10094663162891));
#134695=CARTESIAN_POINT('Origin',(-0.118899482557115,1.48222899061809,-0.153072010682567));
#134696=CARTESIAN_POINT('Ctrl Pts',(4.05369271047275,1.62564958678609,6.31011690926927));
#134697=CARTESIAN_POINT('Ctrl Pts',(4.03801148411028,1.62139779885104,6.28607428389982));
#134698=CARTESIAN_POINT('Ctrl Pts',(4.02231473077999,1.61707840870115,6.26205361824685));
#134699=CARTESIAN_POINT('Ctrl Pts',(4.00660160957958,1.61268792537235,6.23805678428026));
#134700=CARTESIAN_POINT('Ctrl Pts',(3.99162303459156,1.6085026853468,6.21518173784873));
#134701=CARTESIAN_POINT('Ctrl Pts',(3.97662431624528,1.60425381506014,6.1923314048936));
#134702=CARTESIAN_POINT('Ctrl Pts',(3.96164674257624,1.59993003808297,6.16948148613296));
#134703=CARTESIAN_POINT('Ctrl Pts',(3.94666875390263,1.59560614130087,6.14663093423766));
#134704=CARTESIAN_POINT('Ctrl Pts',(3.93170365482691,1.59120881945928,6.12378569777082));
#134705=CARTESIAN_POINT('Ctrl Pts',(3.91675250287728,1.58673401620365,6.10094663327425));
#134706=CARTESIAN_POINT('Ctrl Pts',(3.838457116,1.585967065,6.44331024900001));
#134707=CARTESIAN_POINT('Ctrl Pts',(3.896474404,1.59657582,6.408747755));
#134708=CARTESIAN_POINT('Ctrl Pts',(3.953859916,1.607142857,6.373146144));
#134709=CARTESIAN_POINT('Ctrl Pts',(4.24517774,1.660786473,6.192414392));
#134710=CARTESIAN_POINT('Ctrl Pts',(4.518792609,1.715323387,5.98585945));
#134711=CARTESIAN_POINT('Ctrl Pts',(4.52207997800942,1.71597862537066,5.9833777781612));
#134712=CARTESIAN_POINT('Ctrl Pts',(4.52536734701884,1.71663386374133,5.9808961063224));
#134713=CARTESIAN_POINT('Ctrl Pts',(3.912779966,1.585967065,6.103495141));
#134714=CARTESIAN_POINT('Ctrl Pts',(3.967737468,1.59657582,6.068263424));
#134715=CARTESIAN_POINT('Ctrl Pts',(4.022051639,1.607142857,6.032047796));
#134716=CARTESIAN_POINT('Ctrl Pts',(4.297777787,1.660786473,5.848198986));
#134717=CARTESIAN_POINT('Ctrl Pts',(4.555581632,1.715323387,5.639962411));
#134718=CARTESIAN_POINT('Ctrl Pts',(4.55867903812293,1.71597862537066,5.63746053503914));
#134719=CARTESIAN_POINT('Ctrl Pts',(4.56177644424584,1.71663386374133,5.63495865907829));
#134720=CARTESIAN_POINT('Ctrl Pts',(4.55558161941369,1.71532338433744,5.63996242116637));
#134721=CARTESIAN_POINT('Ctrl Pts',(4.43977427164447,1.69082500902195,5.73350379309277));
#134722=CARTESIAN_POINT('Ctrl Pts',(4.32132169862116,1.66647816281935,5.8232823794762));
#134723=CARTESIAN_POINT('Ctrl Pts',(4.20059848569967,1.64234940725285,5.90910080807064));
#134724=CARTESIAN_POINT('Ctrl Pts',(4.14160960169909,1.63055939331314,5.95103419608245));
#134725=CARTESIAN_POINT('Ctrl Pts',(4.08207890368759,1.61882139949784,5.99202278842587));
#134726=CARTESIAN_POINT('Ctrl Pts',(4.02205163891606,1.60714285698474,6.03204779607983));
#134727=CARTESIAN_POINT('Ctrl Pts',(3.98718534275932,1.6003594810294,6.05529596109391));
#134728=CARTESIAN_POINT('Ctrl Pts',(3.95208339400105,1.59355605150957,6.07826452157217));
#134729=CARTESIAN_POINT('Ctrl Pts',(3.91675250664303,1.58673401458826,6.10094663147859));
#134730=CARTESIAN_POINT('Ctrl Pts',(4.89534041542821,1.71660033198358,5.68205138827747));
#134731=CARTESIAN_POINT('Ctrl Pts',(4.8984095432141,1.71596185949179,5.67940141063874));
#134732=CARTESIAN_POINT('Ctrl Pts',(4.901478671,1.715323387,5.676751433));
#134733=CARTESIAN_POINT('Ctrl Pts',(5.210022603,1.651136808,5.410345282));
#134734=CARTESIAN_POINT('Ctrl Pts',(5.487874705,1.585954698,5.11206721600001));
#134735=CARTESIAN_POINT('Ctrl Pts',(4.54948315630955,1.71660033198358,5.64488834877326));
#134736=CARTESIAN_POINT('Ctrl Pts',(4.55253239415478,1.71596185949179,5.64242537988663));
#134737=CARTESIAN_POINT('Ctrl Pts',(4.555581632,1.715323387,5.639962411));
#134738=CARTESIAN_POINT('Ctrl Pts',(4.862125999,1.651136808,5.392356525));
#134739=CARTESIAN_POINT('Ctrl Pts',(5.140027969,1.585954698,5.112984694));
#134740=CARTESIAN_POINT('',(5.13670419287797,1.58673401524605,5.11632387916256));
#134741=CARTESIAN_POINT('Origin',(-0.149025739088519,1.48222905383165,-0.123933542996065));
#134742=CARTESIAN_POINT('Ctrl Pts',(5.3154082371546,1.62564958678922,5.29116577595053));
#134743=CARTESIAN_POINT('Ctrl Pts',(5.29492517538635,1.6213977988818,5.27105625408232));
#134744=CARTESIAN_POINT('Ctrl Pts',(5.27443167040395,1.61707840872797,5.25097151622125));
#134745=CARTESIAN_POINT('Ctrl Pts',(5.25392730332914,1.61268792539793,5.2309135715011));
#134746=CARTESIAN_POINT('Ctrl Pts',(5.23438146031953,1.60850268536628,5.21179328180062));
#134747=CARTESIAN_POINT('Ctrl Pts',(5.21482125764764,1.6042538150562,5.19270145794555));
#134748=CARTESIAN_POINT('Ctrl Pts',(5.19528179427944,1.59993003806774,5.17360549318183));
#134749=CARTESIAN_POINT('Ctrl Pts',(5.1757417895041,1.59560614127438,5.15450899929958));
#134750=CARTESIAN_POINT('Ctrl Pts',(5.15621551555659,1.59120881943709,5.13541492577162));
#134751=CARTESIAN_POINT('Ctrl Pts',(5.13670419026838,1.58673401624022,5.11632388192909));
#134752=CARTESIAN_POINT('Ctrl Pts',(5.13383736200001,1.585967065,5.46751442));
#134753=CARTESIAN_POINT('Ctrl Pts',(5.18306832399999,1.59657582,5.421287976));
#134754=CARTESIAN_POINT('Ctrl Pts',(5.2314589,1.607142857,5.374182522));
#134755=CARTESIAN_POINT('Ctrl Pts',(5.477113891,1.660786473,5.135051457));
#134756=CARTESIAN_POINT('Ctrl Pts',(5.69992859,1.715323387,4.874506546));
#134757=CARTESIAN_POINT('Ctrl Pts',(5.70260561606592,1.71597862537066,4.87137620710755));
#134758=CARTESIAN_POINT('Ctrl Pts',(5.70528264213185,1.71663386374133,4.86824586821509));
#134759=CARTESIAN_POINT('Ctrl Pts',(5.133372382,1.585967065,5.119666785));
#134760=CARTESIAN_POINT('Ctrl Pts',(5.179471231,1.59657582,5.073444527));
#134761=CARTESIAN_POINT('Ctrl Pts',(5.224730277,1.607142857,5.026399659));
#134762=CARTESIAN_POINT('Ctrl Pts',(5.454488042,1.660786473,4.787576161));
#134763=CARTESIAN_POINT('Ctrl Pts',(5.661499867,1.715323387,4.528787835));
#134764=CARTESIAN_POINT('Ctrl Pts',(5.66398702809828,1.71597862537066,4.52567860074675));
#134765=CARTESIAN_POINT('Ctrl Pts',(5.66647418919657,1.71663386374133,4.5225693664935));
#134766=CARTESIAN_POINT('Ctrl Pts',(5.6614998570788,1.71532338438628,4.52878784740263));
#134767=CARTESIAN_POINT('Ctrl Pts',(5.56850864601704,1.69082500771115,4.64503743717996));
#134768=CARTESIAN_POINT('Ctrl Pts',(5.47212516562663,1.66647816026213,4.75818085749009));
#134769=CARTESIAN_POINT('Ctrl Pts',(5.37267281462158,1.64234940357072,4.86794482593811));
#134770=CARTESIAN_POINT('Ctrl Pts',(5.32407750161806,1.63055939084648,4.92157869531712));
#134771=CARTESIAN_POINT('Ctrl Pts',(5.27474993895569,1.61882139826002,4.97440633186802));
#134772=CARTESIAN_POINT('Ctrl Pts',(5.22473027694185,1.60714285698642,5.02639965906045));
#134773=CARTESIAN_POINT('Ctrl Pts',(5.19567680415667,1.60035948108635,5.05659951771608));
#134774=CARTESIAN_POINT('Ctrl Pts',(5.16633308073874,1.5935560515154,5.08657696779505));
#134775=CARTESIAN_POINT('Ctrl Pts',(5.13670419294588,1.58673401465026,5.11632387909356));
#134776=CARTESIAN_POINT('Ctrl Pts',(6.00236316514702,1.71660033198358,4.49685470076832));
#134777=CARTESIAN_POINT('Ctrl Pts',(6.00479087157351,1.71596185949179,4.49360690638416));
#134778=CARTESIAN_POINT('Ctrl Pts',(6.007218578,1.715323387,4.490359112));
#134779=CARTESIAN_POINT('Ctrl Pts',(6.251279477,1.651136808,4.163853564));
#134780=CARTESIAN_POINT('Ctrl Pts',(6.458514584,1.585954698,3.812819084));
#134781=CARTESIAN_POINT('Ctrl Pts',(5.65660290128854,1.71660033198358,4.53490959909924));
#134782=CARTESIAN_POINT('Ctrl Pts',(5.65905138414427,1.71596185949179,4.53184871704962));
#134783=CARTESIAN_POINT('Ctrl Pts',(5.661499867,1.715323387,4.528787835));
#134784=CARTESIAN_POINT('Ctrl Pts',(5.907649451,1.651136808,4.221072859));
#134785=CARTESIAN_POINT('Ctrl Pts',(6.118997541,1.585954698,3.888491878));
#134786=CARTESIAN_POINT('',(6.11646929978026,1.58673401524938,3.89246750857916));
#134787=CARTESIAN_POINT('Origin',(-0.172183501602985,1.48222899636219,-0.0889997952577576));
#134788=CARTESIAN_POINT('Ctrl Pts',(6.32858118267442,1.62564958672614,4.02480561173429));
#134789=CARTESIAN_POINT('Ctrl Pts',(6.30425405066538,1.62139779884577,4.00956949215637));
#134790=CARTESIAN_POINT('Ctrl Pts',(6.27992204751377,1.61707840870175,3.9943598220441));
#134791=CARTESIAN_POINT('Ctrl Pts',(6.25558519594434,1.61268792537898,3.97917865369961));
#134792=CARTESIAN_POINT('Ctrl Pts',(6.23238602679848,1.60850268535536,3.96470716418705));
#134793=CARTESIAN_POINT('Ctrl Pts',(6.20917895297853,1.60425381506262,3.95026656197384));
#134794=CARTESIAN_POINT('Ctrl Pts',(6.18599124343742,1.59993003808074,3.93581745729565));
#134795=CARTESIAN_POINT('Ctrl Pts',(6.16280289140197,1.59560614129391,3.92136795225588));
#134796=CARTESIAN_POINT('Ctrl Pts',(6.13962846950894,1.59120881944976,3.90691785921443));
#134797=CARTESIAN_POINT('Ctrl Pts',(6.11646929696361,1.58673401627534,3.89246751191927));
#134798=CARTESIAN_POINT('Ctrl Pts',(6.18916508,1.585967065,4.236063694));
#134799=CARTESIAN_POINT('Ctrl Pts',(6.22730773,1.59657582,4.180334797));
#134800=CARTESIAN_POINT('Ctrl Pts',(6.264440681,1.607142857,4.123928098));
#134801=CARTESIAN_POINT('Ctrl Pts',(6.45294628400001,1.660786473,3.837579223));
#134802=CARTESIAN_POINT('Ctrl Pts',(6.614542245,1.715323387,3.535227133));
#134803=CARTESIAN_POINT('Ctrl Pts',(6.61648375335508,1.71597862537066,3.53159449821581));
#134804=CARTESIAN_POINT('Ctrl Pts',(6.61842526171017,1.71663386374133,3.52796186343163));
#134805=CARTESIAN_POINT('Ctrl Pts',(6.113934011,1.585967065,3.896448499));
#134806=CARTESIAN_POINT('Ctrl Pts',(6.149018675,1.59657582,3.841397003));
#134807=CARTESIAN_POINT('Ctrl Pts',(6.183106334,1.607142857,3.785722661));
#134808=CARTESIAN_POINT('Ctrl Pts',(6.35615249700001,1.660786473,3.503091595));
#134809=CARTESIAN_POINT('Ctrl Pts',(6.502692661,1.715323387,3.205852173));
#134810=CARTESIAN_POINT('Ctrl Pts',(6.50445328020731,1.71597862537066,3.20228096479836));
#134811=CARTESIAN_POINT('Ctrl Pts',(6.50621389941464,1.71663386374133,3.19870975659673));
#134812=CARTESIAN_POINT('Ctrl Pts',(6.50269265359969,1.71532338424588,3.20585218801065));
#134813=CARTESIAN_POINT('Ctrl Pts',(6.43686575043932,1.69082500755083,3.33937428870625));
#134814=CARTESIAN_POINT('Ctrl Pts',(6.36705815283194,1.66647816004792,3.47059207839789));
#134815=CARTESIAN_POINT('Ctrl Pts',(6.29352695091531,1.64234940326824,3.59916914265701));
#134816=CARTESIAN_POINT('Ctrl Pts',(6.2575974662105,1.63055939066046,3.66199563730517));
#134817=CARTESIAN_POINT('Ctrl Pts',(6.22077953525197,1.61882139818087,3.72419216051023));
#134818=CARTESIAN_POINT('Ctrl Pts',(6.18310633402413,1.60714285700432,3.78572266101966));
#134819=CARTESIAN_POINT('Ctrl Pts',(6.16122419188576,1.60035948107341,3.82146210164454));
#134820=CARTESIAN_POINT('Ctrl Pts',(6.13901077410713,1.59355605150694,3.85704672843223));
#134821=CARTESIAN_POINT('Ctrl Pts',(6.11646929960905,1.5867340145087,3.89246750832756));
#134822=CARTESIAN_POINT('Ctrl Pts',(6.8287220845867,1.71660033198358,3.10139008475842));
#134823=CARTESIAN_POINT('Ctrl Pts',(6.83039485279336,1.71596185949179,3.09769633687921));
#134824=CARTESIAN_POINT('Ctrl Pts',(6.832067621,1.715323387,3.094002589));
#134825=CARTESIAN_POINT('Ctrl Pts',(7.00023347,1.651136808,2.72266468));
#134826=CARTESIAN_POINT('Ctrl Pts',(7.127161499,1.585954698,2.33528777));
#134827=CARTESIAN_POINT('Ctrl Pts',(6.49922618194217,1.71660033198358,3.21288351652541));
#134828=CARTESIAN_POINT('Ctrl Pts',(6.50095942147109,1.71596185949179,3.2093678447627));
#134829=CARTESIAN_POINT('Ctrl Pts',(6.502692661,1.715323387,3.205852173));
#134830=CARTESIAN_POINT('Ctrl Pts',(6.676937781,1.651136808,2.852416518));
#134831=CARTESIAN_POINT('Ctrl Pts',(6.81184959,1.585954698,2.482177504));
#134832=CARTESIAN_POINT('',(6.81023510037855,1.5867340152209,2.48660368285477));
#134833=CARTESIAN_POINT('Origin',(-0.187290311837918,1.48222900552861,-0.0499046892512461));
#134834=CARTESIAN_POINT('Ctrl Pts',(7.0458367053091,1.6256495867156,2.57025001046618));
#134835=CARTESIAN_POINT('Ctrl Pts',(7.01880301281208,1.62139779885643,2.56059971734374));
#134836=CARTESIAN_POINT('Ctrl Pts',(6.9917702488842,1.61707840870187,2.5509763023171));
#134837=CARTESIAN_POINT('Ctrl Pts',(6.96473887695019,1.61268792536728,2.54138176494955));
#134838=CARTESIAN_POINT('Ctrl Pts',(6.93897114900315,1.60850268532848,2.53223574641715));
#134839=CARTESIAN_POINT('Ctrl Pts',(6.91320234107661,1.60425381501464,2.52312159228064));
#134840=CARTESIAN_POINT('Ctrl Pts',(6.8874506169071,1.59993003802148,2.51399497175813));
#134841=CARTESIAN_POINT('Ctrl Pts',(6.86169817919846,1.59560614122338,2.50486809835155));
#134842=CARTESIAN_POINT('Ctrl Pts',(6.83595921954746,1.59120881937249,2.49573765613442));
#134843=CARTESIAN_POINT('Ctrl Pts',(6.81023509907772,1.58673401608377,2.48660368644794));
#134844=CARTESIAN_POINT('Ctrl Pts',(6.955094316,1.585967065,2.806539337));
#134845=CARTESIAN_POINT('Ctrl Pts',(6.980365147,1.59657582,2.743913808));
#134846=CARTESIAN_POINT('Ctrl Pts',(7.004504177,1.607142857,2.68084338));
#134847=CARTESIAN_POINT('Ctrl Pts',(7.127046081,1.660786473,2.36066605));
#134848=CARTESIAN_POINT('Ctrl Pts',(7.219867256,1.715323387,2.030644429));
#134849=CARTESIAN_POINT('Ctrl Pts',(7.22098246386582,1.71597862537066,2.02667935629295));
#134850=CARTESIAN_POINT('Ctrl Pts',(7.22209767173163,1.71663386374133,2.0227142835859));
#134851=CARTESIAN_POINT('Ctrl Pts',(6.808614881,1.585967065,2.491036613));
#134852=CARTESIAN_POINT('Ctrl Pts',(6.83104484,1.59657582,2.429730024));
#134853=CARTESIAN_POINT('Ctrl Pts',(6.852367211,1.607142857,2.368029478));
#134854=CARTESIAN_POINT('Ctrl Pts',(6.96061032600001,1.660786473,2.05480636));
#134855=CARTESIAN_POINT('Ctrl Pts',(7.039826773,1.715323387,1.733014427));
#134856=CARTESIAN_POINT('Ctrl Pts',(7.04077852570941,1.71597862537066,1.7291482305762));
#134857=CARTESIAN_POINT('Ctrl Pts',(7.04173027841881,1.71663386374133,1.7252820341524));
#134858=CARTESIAN_POINT('Ctrl Pts',(7.0398267723587,1.71532338598808,1.73301443434052));
#134859=CARTESIAN_POINT('Ctrl Pts',(7.03674478447241,1.71320157782646,1.74553404158354));
#134860=CARTESIAN_POINT('Ctrl Pts',(7.03578215386801,1.71254943786671,1.74938028347368));
#134861=CARTESIAN_POINT('Ctrl Pts',(7.03187812797395,1.70989962932953,1.76500933389786));
#134862=CARTESIAN_POINT('Ctrl Pts',(7.02986684988547,1.70854407402951,1.77300311029435));
#134863=CARTESIAN_POINT('Ctrl Pts',(7.02379362923113,1.70447938484232,1.79696818020817));
#134864=CARTESIAN_POINT('Ctrl Pts',(7.01969082021462,1.70177120841212,1.81292922855852));
#134865=CARTESIAN_POINT('Ctrl Pts',(7.00722572551858,1.69365497346663,1.86074508438884));
#134866=CARTESIAN_POINT('Ctrl Pts',(6.99870059694122,1.68825095320109,1.89255771623979));
#134867=CARTESIAN_POINT('Ctrl Pts',(6.97250587998078,1.6720751488223,1.98770859903185));
#134868=CARTESIAN_POINT('Ctrl Pts',(6.95419024702157,1.66132115703357,2.0508687956172));
#134869=CARTESIAN_POINT('Ctrl Pts',(6.89678398291717,1.62920290563523,2.23921117229545));
#134870=CARTESIAN_POINT('Ctrl Pts',(6.85518854199609,1.60803075408737,2.36348655623575));
#134871=CARTESIAN_POINT('Ctrl Pts',(6.81023510083827,1.58673401461604,2.486603682918));
#134872=CARTESIAN_POINT('Ctrl Pts',(7.33577754858687,1.71660033198358,1.56090791565573));
#134873=CARTESIAN_POINT('Ctrl Pts',(7.33661716179344,1.71596185949179,1.55694092982786));
#134874=CARTESIAN_POINT('Ctrl Pts',(7.337456775,1.715323387,1.552973944));
#134875=CARTESIAN_POINT('Ctrl Pts',(7.421864326,1.651136808,1.154167022));
#134876=CARTESIAN_POINT('Ctrl Pts',(7.462550264,1.585954698,0.748560994));
#134877=CARTESIAN_POINT('Ctrl Pts',(7.03795286930082,1.71660033198358,1.74062657215131));
#134878=CARTESIAN_POINT('Ctrl Pts',(7.03888982115041,1.71596185949179,1.73682049957566));
#134879=CARTESIAN_POINT('Ctrl Pts',(7.039826773,1.715323387,1.733014427));
#134880=CARTESIAN_POINT('Ctrl Pts',(7.134019921,1.651136808,1.350384351));
#134881=CARTESIAN_POINT('Ctrl Pts',(7.186187123,1.585954698,0.959799268000001));
#134882=CARTESIAN_POINT('',(7.18556187676617,1.58673401523149,0.964469033473924));
#134883=CARTESIAN_POINT('Origin',(-0.19363951953293,1.48222901693015,-0.00847605363484161));
#134884=CARTESIAN_POINT('Ctrl Pts',(7.43363673495881,1.62564958676892,0.995512375047741));
#134885=CARTESIAN_POINT('Ctrl Pts',(7.40516054742324,1.62139779886505,0.991899144976718));
#134886=CARTESIAN_POINT('Ctrl Pts',(7.37669104475956,1.6170784087111,0.988311965239451));
#134887=CARTESIAN_POINT('Ctrl Pts',(7.34822910937733,1.61268792537966,0.984752688798697));
#134888=CARTESIAN_POINT('Ctrl Pts',(7.32109769297018,1.60850268534258,0.981359798964417));
#134889=CARTESIAN_POINT('Ctrl Pts',(7.29397207171134,1.60425381504701,0.977998260824985));
#134890=CARTESIAN_POINT('Ctrl Pts',(7.26686045491275,1.59993003805526,0.974620875143033));
#134891=CARTESIAN_POINT('Ctrl Pts',(7.23974808689459,1.59560614125856,0.971243395879125));
#134892=CARTESIAN_POINT('Ctrl Pts',(7.21264811464815,1.59120881939792,0.967859533782329));
#134893=CARTESIAN_POINT('Ctrl Pts',(7.18556187633388,1.58673401612646,0.964469036847194));
#134894=CARTESIAN_POINT('Ctrl Pts',(7.395811073,1.585967065,1.24578432));
#134895=CARTESIAN_POINT('Ctrl Pts',(7.407028448,1.59657582,1.17919046));
#134896=CARTESIAN_POINT('Ctrl Pts',(7.417044844,1.607142857,1.112405405));
#134897=CARTESIAN_POINT('Ctrl Pts',(7.467893124,1.660786473,0.773370756));
#134898=CARTESIAN_POINT('Ctrl Pts',(7.487599299,1.715323387,0.431111049));
#134899=CARTESIAN_POINT('Ctrl Pts',(7.48783606050798,1.71597862537066,0.426998940772556));
#134900=CARTESIAN_POINT('Ctrl Pts',(7.48807282201595,1.71663386374133,0.422886832545111));
#134901=CARTESIAN_POINT('Ctrl Pts',(7.184932486,1.585967065,0.969146623));
#134902=CARTESIAN_POINT('Ctrl Pts',(7.193658941,1.59657582,0.90445157));
#134903=CARTESIAN_POINT('Ctrl Pts',(7.201219013,1.607142857,0.839609869));
#134904=CARTESIAN_POINT('Ctrl Pts',(7.239597753,1.660786473,0.510440663));
#134905=CARTESIAN_POINT('Ctrl Pts',(7.24778641,1.715323387,0.179142852));
#134906=CARTESIAN_POINT('Ctrl Pts',(7.24788479331283,1.71597862537066,0.175162446400145));
#134907=CARTESIAN_POINT('Ctrl Pts',(7.24798317662565,1.71663386374133,0.17118204080029));
#134908=CARTESIAN_POINT('Ctrl Pts',(7.24778640958819,1.71532338425733,0.179142868661036));
#134909=CARTESIAN_POINT('Ctrl Pts',(7.24410800451256,1.69082500283194,0.327964273211171));
#134910=CARTESIAN_POINT('Ctrl Pts',(7.23584926208652,1.66647815067575,0.47636579160891));
#134911=CARTESIAN_POINT('Ctrl Pts',(7.2231022543405,1.64234938933421,0.623934152985415));
#134912=CARTESIAN_POINT('Ctrl Pts',(7.21687369910933,1.63055938138335,0.69604030585824));
#134913=CARTESIAN_POINT('Ctrl Pts',(7.20957429458728,1.61882139352168,0.767947761171279));
#134914=CARTESIAN_POINT('Ctrl Pts',(7.20121901293751,1.60714285691265,0.839609869535977));
#134915=CARTESIAN_POINT('Ctrl Pts',(7.19636592023945,1.60035948103039,0.881234180183976));
#134916=CARTESIAN_POINT('Ctrl Pts',(7.19114716532452,1.59355605149237,0.922857084704198));
#134917=CARTESIAN_POINT('Ctrl Pts',(7.18556187702628,1.5867340145481,0.964469033396799));
#134918=CARTESIAN_POINT('Ctrl Pts',(7.49982020834237,1.71660033198358,-0.052560573154935));
#134919=CARTESIAN_POINT('Ctrl Pts',(7.49978740717118,1.71596185949179,-0.0566153050774675));
#134920=CARTESIAN_POINT('Ctrl Pts',(7.499754606,1.715323387,-0.060670037));
#134921=CARTESIAN_POINT('Ctrl Pts',(7.496457056,1.651136808,-0.468298203));
#134922=CARTESIAN_POINT('Ctrl Pts',(7.448998472,1.585954698,-0.873167661));
#134923=CARTESIAN_POINT('Ctrl Pts',(7.24759270333538,1.71660033198358,0.186979863312151));
#134924=CARTESIAN_POINT('Ctrl Pts',(7.24768955666769,1.71596185949179,0.183061357656076));
#134925=CARTESIAN_POINT('Ctrl Pts',(7.24778641,1.715323387,0.179142852));
#134926=CARTESIAN_POINT('Ctrl Pts',(7.257523218,1.651136808,-0.214790287));
#134927=CARTESIAN_POINT('Ctrl Pts',(7.224506533,1.585954698,-0.607458115));
#134928=CARTESIAN_POINT('',(7.22489976600227,1.58673401521042,-0.602763116913948));
#134929=CARTESIAN_POINT('Origin',(-0.190934634282323,1.48222905617907,0.0333488860263628));
#134930=CARTESIAN_POINT('Ctrl Pts',(7.47384817275646,1.62564958676686,-0.625774312182214));
#134931=CARTESIAN_POINT('Ctrl Pts',(7.44526100500499,1.6213977988801,-0.623181528288945));
#134932=CARTESIAN_POINT('Ctrl Pts',(7.41668596593912,1.61707840874644,-0.620564740192384));
#134933=CARTESIAN_POINT('Ctrl Pts',(7.38812431561075,1.6126879254332,-0.617922327910765));
#134934=CARTESIAN_POINT('Ctrl Pts',(7.36089784559814,1.60850268540349,-0.615403441294639));
#134935=CARTESIAN_POINT('Ctrl Pts',(7.33368377491949,1.60425381509984,-0.612855181841118));
#134936=CARTESIAN_POINT('Ctrl Pts',(7.30647997453032,1.59993003809602,-0.610325409987345));
#134937=CARTESIAN_POINT('Ctrl Pts',(7.27927542036728,1.59560614128724,-0.607795568037634));
#134938=CARTESIAN_POINT('Ctrl Pts',(7.25208160005015,1.59120881941603,-0.605274624400682));
#134939=CARTESIAN_POINT('Ctrl Pts',(7.22489976652123,1.58673401614243,-0.602763113096493));
#134940=CARTESIAN_POINT('Ctrl Pts',(7.490707924,1.585967065,-0.373222187));
#134941=CARTESIAN_POINT('Ctrl Pts',(7.487347331,1.59657582,-0.440670524));
#134942=CARTESIAN_POINT('Ctrl Pts',(7.482772737,1.607142857,-0.50804741));
#134943=CARTESIAN_POINT('Ctrl Pts',(7.459549785,1.660786473,-0.850086495));
#134944=CARTESIAN_POINT('Ctrl Pts',(7.40521952,1.715323387,-1.188580606));
#134945=CARTESIAN_POINT('Ctrl Pts',(7.40456676443124,1.71597862537066,-1.19264747215549));
#134946=CARTESIAN_POINT('Ctrl Pts',(7.40391400886248,1.71663386374133,-1.19671433831097));
#134947=CARTESIAN_POINT('Ctrl Pts',(7.225290633,1.585967065,-0.598059586));
#134948=CARTESIAN_POINT('Ctrl Pts',(7.219905545,1.59657582,-0.663118034));
#134949=CARTESIAN_POINT('Ctrl Pts',(7.213349817,1.607142857,-0.728068964));
#134950=CARTESIAN_POINT('Ctrl Pts',(7.180069635,1.660786473,-1.057792671));
#134951=CARTESIAN_POINT('Ctrl Pts',(7.116847609,1.715323387,-1.383105243));
#134952=CARTESIAN_POINT('Ctrl Pts',(7.11608802261588,1.71597862537066,-1.38701373843915));
#134953=CARTESIAN_POINT('Ctrl Pts',(7.11532843623176,1.71663386374133,-1.39092223387829));
#134954=CARTESIAN_POINT('Ctrl Pts',(7.11684761207532,1.71532338434715,-1.38310522717576));
#134955=CARTESIAN_POINT('Ctrl Pts',(7.14524739863188,1.69082501198697,-1.23697248985002));
#134956=CARTESIAN_POINT('Ctrl Pts',(7.16908367371738,1.66647816873387,-1.09026518511952));
#134957=CARTESIAN_POINT('Ctrl Pts',(7.18835751572347,1.64234941611947,-0.94340671439929));
#134958=CARTESIAN_POINT('Ctrl Pts',(7.19777528077458,1.63055939921329,-0.871647354092652));
#134959=CARTESIAN_POINT('Ctrl Pts',(7.20610451662223,1.61882140247104,-0.799851844908871));
#134960=CARTESIAN_POINT('Ctrl Pts',(7.2133498171633,1.60714285707959,-0.728068964315511));
#134961=CARTESIAN_POINT('Ctrl Pts',(7.21755818397531,1.60035948117327,-0.686374535307469));
#134962=CARTESIAN_POINT('Ctrl Pts',(7.22140913456291,1.59355605158198,-0.644602873176996));
#134963=CARTESIAN_POINT('Ctrl Pts',(7.22489976573252,1.58673401461327,-0.602763116988815));
#134964=CARTESIAN_POINT('Ctrl Pts',(7.31317960960073,1.71660033198358,-1.66357138748205));
#134965=CARTESIAN_POINT('Ctrl Pts',(7.31227592780037,1.71596185949179,-1.66752427074103));
#134966=CARTESIAN_POINT('Ctrl Pts',(7.311372246,1.715323387,-1.671477154));
#134967=CARTESIAN_POINT('Ctrl Pts',(7.220523785,1.651136808,-2.068866324));
#134968=CARTESIAN_POINT('Ctrl Pts',(7.087139791,1.585954698,-2.454067967));
#134969=CARTESIAN_POINT('Ctrl Pts',(7.11834315687191,1.71660033198358,-1.37540981543085));
#134970=CARTESIAN_POINT('Ctrl Pts',(7.11759538293595,1.71596185949179,-1.37925752921543));
#134971=CARTESIAN_POINT('Ctrl Pts',(7.116847609,1.715323387,-1.383105243));
#134972=CARTESIAN_POINT('Ctrl Pts',(7.04167279500001,1.651136808,-1.769921571));
#134973=CARTESIAN_POINT('Ctrl Pts',(6.925016046,1.585954698,-2.146311431));
#134974=CARTESIAN_POINT('',(6.92640937099897,1.58673401527515,-2.14181073446729));
#134975=CARTESIAN_POINT('Origin',(-0.179301677008858,1.4822289963032,0.0736145282351569));
#134976=CARTESIAN_POINT('Ctrl Pts',(7.16459077630825,1.62564958672988,-2.21780048805578));
#134977=CARTESIAN_POINT('Ctrl Pts',(7.13722933254449,1.62139779886377,-2.20912292591444));
#134978=CARTESIAN_POINT('Ctrl Pts',(7.1098848940126,1.61707840872217,-2.20042452820074));
#134979=CARTESIAN_POINT('Ctrl Pts',(7.08255903964804,1.61268792540122,-2.19170398356328));
#134980=CARTESIAN_POINT('Ctrl Pts',(7.05651059551737,1.60850268537298,-2.18339110094496));
#134981=CARTESIAN_POINT('Ctrl Pts',(7.03048057511913,1.60425381506448,-2.17505219774219));
#134982=CARTESIAN_POINT('Ctrl Pts',(7.00445661063308,1.59993003806697,-2.16673355763766));
#134983=CARTESIAN_POINT('Ctrl Pts',(6.97843192506457,1.59560614126451,-2.15841468703692));
#134984=CARTESIAN_POINT('Ctrl Pts',(6.95241580953442,1.59120881940851,-2.15010681410913));
#134985=CARTESIAN_POINT('Ctrl Pts',(6.92640937246645,1.58673401608731,-2.14181072954637));
#134986=CARTESIAN_POINT('Ctrl Pts',(7.235347597,1.585967065,-1.97477724));
#134987=CARTESIAN_POINT('Ctrl Pts',(7.217566175,1.59657582,-2.039926244));
#134988=CARTESIAN_POINT('Ctrl Pts',(7.198614493,1.607142857,-2.104744493));
#134989=CARTESIAN_POINT('Ctrl Pts',(7.102406188,1.660786473,-2.433794646));
#134990=CARTESIAN_POINT('Ctrl Pts',(6.976579907,1.715323387,-2.752695552));
#134991=CARTESIAN_POINT('Ctrl Pts',(6.97506815649374,1.71597862537066,-2.75652701393514));
#134992=CARTESIAN_POINT('Ctrl Pts',(6.97355640598748,1.71663386374133,-2.76035847587028));
#134993=CARTESIAN_POINT('Ctrl Pts',(6.927802221,1.585967065,-2.137301193));
#134994=CARTESIAN_POINT('Ctrl Pts',(6.90855739,1.59657582,-2.199680976));
#134995=CARTESIAN_POINT('Ctrl Pts',(6.888192401,1.607142857,-2.261704102));
#134996=CARTESIAN_POINT('Ctrl Pts',(6.78480944,1.660786473,-2.576564797));
#134997=CARTESIAN_POINT('Ctrl Pts',(6.653132924,1.715323387,-2.880680874));
#134998=CARTESIAN_POINT('Ctrl Pts',(6.65155088535002,1.71597862537066,-2.88433470235535));
#134999=CARTESIAN_POINT('Ctrl Pts',(6.64996884670004,1.71663386374133,-2.8879885307107));
#135000=CARTESIAN_POINT('Ctrl Pts',(6.65313292612395,1.71532338611517,-2.88068086759738));
#135001=CARTESIAN_POINT('Ctrl Pts',(6.71228296416041,1.69082501192151,-2.7440697389745));
#135002=CARTESIAN_POINT('Ctrl Pts',(6.76709969595371,1.66647816771549,-2.60591645951733));
#135003=CARTESIAN_POINT('Ctrl Pts',(6.81749315660543,1.64234941497924,-2.46663476376996));
#135004=CARTESIAN_POINT('Ctrl Pts',(6.84211688048578,1.6305593982336,-2.39857763942654));
#135005=CARTESIAN_POINT('Ctrl Pts',(6.86568529500849,1.61882140184801,-2.33025121065281));
#135006=CARTESIAN_POINT('Ctrl Pts',(6.88819240103793,1.60714285700126,-2.26170410208723));
#135007=CARTESIAN_POINT('Ctrl Pts',(6.9012654487764,1.60035948085629,-2.22188913820699));
#135008=CARTESIAN_POINT('Ctrl Pts',(6.91400603931158,1.593556051179,-2.18192191381413));
#135009=CARTESIAN_POINT('Ctrl Pts',(6.926409371,1.586734015,-2.141810735));
#135010=CARTESIAN_POINT('Ctrl Pts',(6.78458286054717,1.71660033198358,-3.19679545366646));
#135011=CARTESIAN_POINT('Ctrl Pts',(6.78285055327358,1.71596185949179,-3.20046165583323));
#135012=CARTESIAN_POINT('Ctrl Pts',(6.78111824600001,1.715323387,-3.204127858));
#135013=CARTESIAN_POINT('Ctrl Pts',(6.606966847,1.651136808,-3.572696556));
#135014=CARTESIAN_POINT('Ctrl Pts',(6.39389433,1.585954698,-3.920218782));
#135015=CARTESIAN_POINT('Ctrl Pts',(6.6562477962472,1.71660033198358,-2.87348685982246));
#135016=CARTESIAN_POINT('Ctrl Pts',(6.6546903601236,1.71596185949179,-2.87708386691123));
#135017=CARTESIAN_POINT('Ctrl Pts',(6.653132924,1.715323387,-2.880680874));
#135018=CARTESIAN_POINT('Ctrl Pts',(6.496561579,1.651136808,-3.242293289));
#135019=CARTESIAN_POINT('Ctrl Pts',(6.301719506,1.585954698,-3.58480561));
#135020=CARTESIAN_POINT('',(6.30404777345953,1.58673401521883,-3.58070965999336));
#135021=CARTESIAN_POINT('Origin',(-0.159284671104115,1.48222897082287,0.110437985497804));
#135022=CARTESIAN_POINT('Ctrl Pts',(6.52032507811018,1.62564958671635,-3.70612477820676));
#135023=CARTESIAN_POINT('Ctrl Pts',(6.49546874906344,1.62139779884951,-3.69176819098134));
#135024=CARTESIAN_POINT('Ctrl Pts',(6.47063350665613,1.61707840869391,-3.67739491099258));
#135025=CARTESIAN_POINT('Ctrl Pts',(6.44582117486303,1.61268792535999,-3.6630039969133));
#135026=CARTESIAN_POINT('Ctrl Pts',(6.42216875293301,1.60850268532869,-3.64928581941188));
#135027=CARTESIAN_POINT('Ctrl Pts',(6.39853991765919,1.60425381501957,-3.6355461902282));
#135028=CARTESIAN_POINT('Ctrl Pts',(6.37491264077159,1.5999300380313,-3.62182765219868));
#135029=CARTESIAN_POINT('Ctrl Pts',(6.35128470921003,1.5956061412381,-3.60810873405046));
#135030=CARTESIAN_POINT('Ctrl Pts',(6.32766278316444,1.59120881939816,-3.59440239872991));
#135031=CARTESIAN_POINT('Ctrl Pts',(6.30404777520744,1.58673401614287,-3.58070965616356));
#135032=CARTESIAN_POINT('Ctrl Pts',(6.641670459,1.585967065,-3.483993903));
#135033=CARTESIAN_POINT('Ctrl Pts',(6.610299646,1.59657582,-3.54379728));
#135034=CARTESIAN_POINT('Ctrl Pts',(6.577857036,1.607142857,-3.603026063));
#135035=CARTESIAN_POINT('Ctrl Pts',(6.41316197200001,1.660786473,-3.903701264));
#135036=CARTESIAN_POINT('Ctrl Pts',(6.221723171,1.715323387,-4.188097513));
#135037=CARTESIAN_POINT('Ctrl Pts',(6.21942311331706,1.71597862537066,-4.19151441581224));
#135038=CARTESIAN_POINT('Ctrl Pts',(6.21712305563413,1.71663386374133,-4.1949313186245));
#135039=CARTESIAN_POINT('Ctrl Pts',(6.306377476,1.585967065,-3.576604972));
#135040=CARTESIAN_POINT('Ctrl Pts',(6.274172769,1.59657582,-3.633389281));
#135041=CARTESIAN_POINT('Ctrl Pts',(6.240950764,1.607142857,-3.68958447));
#135042=CARTESIAN_POINT('Ctrl Pts',(6.072299097,1.660786473,-3.974859616));
#135043=CARTESIAN_POINT('Ctrl Pts',(5.878325138,1.715323387,-4.24355907));
#135044=CARTESIAN_POINT('Ctrl Pts',(5.87599462144663,1.71597862537066,-4.24678738233974));
#135045=CARTESIAN_POINT('Ctrl Pts',(5.87366410489327,1.71663386374133,-4.25001569467948));
#135046=CARTESIAN_POINT('Ctrl Pts',(5.87832514762602,1.71532338429359,-4.2435590566657));
#135047=CARTESIAN_POINT('Ctrl Pts',(5.96545964263553,1.6908250109101,-4.12285733223717));
#135048=CARTESIAN_POINT('Ctrl Pts',(6.04869366166071,1.66647816661746,-3.99971797539809));
#135049=CARTESIAN_POINT('Ctrl Pts',(6.12785040151841,1.64234941292913,-3.87452570760659));
#135050=CARTESIAN_POINT('Ctrl Pts',(6.16652870330467,1.63055939708763,-3.81335309838025));
#135051=CARTESIAN_POINT('Ctrl Pts',(6.20423426152324,1.61882140138784,-3.75169061978853));
#135052=CARTESIAN_POINT('Ctrl Pts',(6.24095076432877,1.60714285701179,-3.68958446996873));
#135053=CARTESIAN_POINT('Ctrl Pts',(6.26227721078558,1.60035948109084,-3.6535106782366));
#135054=CARTESIAN_POINT('Ctrl Pts',(6.28331170442055,1.59355605152486,-3.61721671655659));
#135055=CARTESIAN_POINT('Ctrl Pts',(6.30404777321125,1.58673401456331,-3.58070965997483));
#135056=CARTESIAN_POINT('Ctrl Pts',(5.93874655798517,1.71660033198358,-4.5805409169344));
#135057=CARTESIAN_POINT('Ctrl Pts',(5.93626662599258,1.71596185949179,-4.5837490104672));
#135058=CARTESIAN_POINT('Ctrl Pts',(5.933786694,1.715323387,-4.586957104));
#135059=CARTESIAN_POINT('Ctrl Pts',(5.68447548200001,1.651136808,-4.909471467));
#135060=CARTESIAN_POINT('Ctrl Pts',(5.401677476,1.585954698,-5.203064524));
#135061=CARTESIAN_POINT('Ctrl Pts',(5.88291368665965,1.71660033198358,-4.23720285334885));
#135062=CARTESIAN_POINT('Ctrl Pts',(5.88061941232983,1.71596185949179,-4.24038096167442));
#135063=CARTESIAN_POINT('Ctrl Pts',(5.878325138,1.715323387,-4.24355907));
#135064=CARTESIAN_POINT('Ctrl Pts',(5.647678364,1.651136808,-4.563058976));
#135065=CARTESIAN_POINT('Ctrl Pts',(5.383761566,1.585954698,-4.855678264));
#135066=CARTESIAN_POINT('',(5.38691590788117,1.58673401522098,-4.85217858289702));
#135067=CARTESIAN_POINT('Origin',(-0.131819883971023,1.48222899047365,0.142097578797142));
#135068=CARTESIAN_POINT('Ctrl Pts',(5.57117622601978,1.62564958674757,-5.02115479281309));
#135069=CARTESIAN_POINT('Ctrl Pts',(5.54998726590558,1.62139779884887,-5.00179047884981));
#135070=CARTESIAN_POINT('Ctrl Pts',(5.5288224880741,1.61707840870451,-4.98241439515562));
#135071=CARTESIAN_POINT('Ctrl Pts',(5.50768387604366,1.61268792538439,-4.96302601473718));
#135072=CARTESIAN_POINT('Ctrl Pts',(5.48753343727595,1.60850268535182,-4.94454398896063));
#135073=CARTESIAN_POINT('Ctrl Pts',(5.46741064525574,1.60425381505338,-4.92604608340411));
#135074=CARTESIAN_POINT('Ctrl Pts',(5.44728484120158,1.59993003807154,-4.90756911092237));
#135075=CARTESIAN_POINT('Ctrl Pts',(5.42715847949359,1.59560614128475,-4.88909162647329));
#135076=CARTESIAN_POINT('Ctrl Pts',(5.40703527793745,1.59120881944353,-4.87062772170985));
#135077=CARTESIAN_POINT('Ctrl Pts',(5.38691591042844,1.58673401610884,-4.85217858048633));
#135078=CARTESIAN_POINT('Ctrl Pts',(5.737436191,1.585967065,-4.830302884));
#135079=CARTESIAN_POINT('Ctrl Pts',(5.693942853,1.59657582,-4.881964294));
#135080=CARTESIAN_POINT('Ctrl Pts',(5.649526295,1.607142857,-4.932834139));
#135081=CARTESIAN_POINT('Ctrl Pts',(5.42404543,1.660786473,-5.19107515));
#135082=CARTESIAN_POINT('Ctrl Pts',(5.175945575,1.715323387,-5.42766869));
#135083=CARTESIAN_POINT('Ctrl Pts',(5.17296475828653,1.71597862537066,-5.43051126311771));
#135084=CARTESIAN_POINT('Ctrl Pts',(5.16998394157306,1.71663386374133,-5.43335383623542));
#135085=CARTESIAN_POINT('Ctrl Pts',(5.39007353,1.585967065,-4.848670677));
#135086=CARTESIAN_POINT('Ctrl Pts',(5.346414803,1.59657582,-4.89720434));
#135087=CARTESIAN_POINT('Ctrl Pts',(5.301889206,1.607142857,-4.944943968));
#135088=CARTESIAN_POINT('Ctrl Pts',(5.075854798,1.660786473,-5.187294417));
#135089=CARTESIAN_POINT('Ctrl Pts',(4.828653401,1.715323387,-5.408013159));
#135090=CARTESIAN_POINT('Ctrl Pts',(4.82568337888624,1.71597862537066,-5.41066500301309));
#135091=CARTESIAN_POINT('Ctrl Pts',(4.82271335677248,1.71663386374133,-5.41331684702618));
#135092=CARTESIAN_POINT('Ctrl Pts',(4.82865341292025,1.71532338437019,-5.40801314835676));
#135093=CARTESIAN_POINT('Ctrl Pts',(4.93969804922549,1.69082501233844,-5.30886470972604));
#135094=CARTESIAN_POINT('Ctrl Pts',(5.04745741921797,1.66647816940417,-5.20649714239737));
#135095=CARTESIAN_POINT('Ctrl Pts',(5.15167614981874,1.64234941710383,-5.10124816592978));
#135096=CARTESIAN_POINT('Ctrl Pts',(5.20260048333634,1.6305593998735,-5.04982042401502));
#135097=CARTESIAN_POINT('Ctrl Pts',(5.25268012264772,1.61882140281017,-4.99770515434739));
#135098=CARTESIAN_POINT('Ctrl Pts',(5.30188920605868,1.60714285710216,-4.94494396844451));
#135099=CARTESIAN_POINT('Ctrl Pts',(5.33047185070332,1.60035948118248,-4.91429811729116));
#135100=CARTESIAN_POINT('Ctrl Pts',(5.35881669862536,1.5935560516734,-4.88337448286254));
#135101=CARTESIAN_POINT('Ctrl Pts',(5.3869159075036,1.58673401462794,-4.85217858268661));
#135102=CARTESIAN_POINT('Ctrl Pts',(4.81522106667948,1.71660033198358,-5.75010537695528));
#135103=CARTESIAN_POINT('Ctrl Pts',(4.81210946883974,1.71596185949179,-5.75270535497764));
#135104=CARTESIAN_POINT('Ctrl Pts',(4.808997871,1.715323387,-5.755305333));
#135105=CARTESIAN_POINT('Ctrl Pts',(4.496184362,1.651136808,-6.016684949));
#135106=CARTESIAN_POINT('Ctrl Pts',(4.156884187,1.585954698,-6.242620752));
#135107=CARTESIAN_POINT('Ctrl Pts',(4.83450107061284,1.71660033198358,-5.40279194947145));
#135108=CARTESIAN_POINT('Ctrl Pts',(4.83157723580641,1.71596185949179,-5.40540255423573));
#135109=CARTESIAN_POINT('Ctrl Pts',(4.828653401,1.715323387,-5.40801315900001));
#135110=CARTESIAN_POINT('Ctrl Pts',(4.534715986,1.651136808,-5.670461097));
#135111=CARTESIAN_POINT('Ctrl Pts',(4.214064918,1.585954698,-5.899504798));
#135112=CARTESIAN_POINT('',(4.21789784021562,1.5867340152838,-5.89676502875833));
#135113=CARTESIAN_POINT('Origin',(-0.0981910441401429,1.48222903544964,
0.167112545806996));
#135114=CARTESIAN_POINT('Ctrl Pts',(4.36152536588842,1.62564958678343,-6.10140118971835));
#135115=CARTESIAN_POINT('Ctrl Pts',(4.34499454697019,1.62139779888937,-6.07793460252609));
#135116=CARTESIAN_POINT('Ctrl Pts',(4.32848987505951,1.61707840874017,-6.05446171928497));
#135117=CARTESIAN_POINT('Ctrl Pts',(4.31201340060561,1.61268792541011,-6.03098245170926));
#135118=CARTESIAN_POINT('Ctrl Pts',(4.29630715704654,1.60850268537488,-6.00860077678453));
#135119=CARTESIAN_POINT('Ctrl Pts',(4.28063132748528,1.6042538150622,-5.98620953662333));
#135120=CARTESIAN_POINT('Ctrl Pts',(4.26494805633297,1.59993003807245,-5.963838092623));
#135121=CARTESIAN_POINT('Ctrl Pts',(4.24926435062233,1.59560614127776,-5.94146602874581));
#135122=CARTESIAN_POINT('Ctrl Pts',(4.23358081196648,1.59120881943565,-5.91910790639485));
#135123=CARTESIAN_POINT('Ctrl Pts',(4.21789784426445,1.58673401613719,-5.89676502585763));
#135124=CARTESIAN_POINT('Ctrl Pts',(4.564925784,1.585967065,-5.950752271));
#135125=CARTESIAN_POINT('Ctrl Pts',(4.51134362,1.59657582,-5.99185608300001));
#135126=CARTESIAN_POINT('Ctrl Pts',(4.457029984,1.607142857,-6.031988372));
#135127=CARTESIAN_POINT('Ctrl Pts',(4.181306552,1.660786473,-6.235720132));
#135128=CARTESIAN_POINT('Ctrl Pts',(3.888146516,1.715323387,-6.41344811100001));
#135129=CARTESIAN_POINT('Ctrl Pts',(3.88462431992685,1.71597862537066,-6.41558343885118));
#135130=CARTESIAN_POINT('Ctrl Pts',(3.8811021238537,1.71663386374133,-6.41771876670236));
#135131=CARTESIAN_POINT('Ctrl Pts',(4.221735737,1.585967065,-5.894017931));
#135132=CARTESIAN_POINT('Ctrl Pts',(4.168664423,1.59657582,-5.932031568));
#135133=CARTESIAN_POINT('Ctrl Pts',(4.114917201,1.607142857,-5.969083383));
#135134=CARTESIAN_POINT('Ctrl Pts',(3.842069169,1.660786473,-6.157177096));
#135135=CARTESIAN_POINT('Ctrl Pts',(3.553199198,1.715323387,-6.319594564));
#135136=CARTESIAN_POINT('Ctrl Pts',(3.54972854527601,1.71597862537066,-6.32154594242049));
#135137=CARTESIAN_POINT('Ctrl Pts',(3.54625789255202,1.71663386374133,-6.32349732084099));
#135138=CARTESIAN_POINT('Ctrl Pts',(3.55319920437648,1.71532338607709,-6.31959456096104));
#135139=CARTESIAN_POINT('Ctrl Pts',(3.68296167347084,1.69082501162648,-6.24663546560832));
#135140=CARTESIAN_POINT('Ctrl Pts',(3.81020769735712,1.66647816717725,-6.16982626951713));
#135141=CARTESIAN_POINT('Ctrl Pts',(3.93461527411236,1.64234941421584,-6.08944189945254));
#135142=CARTESIAN_POINT('Ctrl Pts',(3.99540446547425,1.6305593977285,-6.05016373825198));
#135143=CARTESIAN_POINT('Ctrl Pts',(4.05551650849235,1.61882140160225,-6.01003253971538));
#135144=CARTESIAN_POINT('Ctrl Pts',(4.11491720092053,1.60714285701562,-5.96908338305479));
#135145=CARTESIAN_POINT('Ctrl Pts',(4.1494195531229,1.60035948087342,-5.94529843739841));
#135146=CARTESIAN_POINT('Ctrl Pts',(4.1837493825457,1.59355605118872,-5.92119108391622));
#135147=CARTESIAN_POINT('Ctrl Pts',(4.21789784,1.586734015,-5.896765029));
#135148=CARTESIAN_POINT('Ctrl Pts',(3.46654118966067,1.71660033198358,-6.65080130115457));
#135149=CARTESIAN_POINT('Ctrl Pts',(3.46294342083033,1.71596185949179,-6.65267159157729));
#135150=CARTESIAN_POINT('Ctrl Pts',(3.459345652,1.715323387,-6.654541882));
#135151=CARTESIAN_POINT('Ctrl Pts',(3.097656658,1.651136808,-6.84256493));
#135152=CARTESIAN_POINT('Ctrl Pts',(2.717719614,1.585954698,-6.990278972));
#135153=CARTESIAN_POINT('Ctrl Pts',(3.56003255805081,1.71660033198358,-6.31575249957073));
#135154=CARTESIAN_POINT('Ctrl Pts',(3.5566158780254,1.71596185949179,-6.31767353178537));
#135155=CARTESIAN_POINT('Ctrl Pts',(3.553199198,1.715323387,-6.319594564));
#135156=CARTESIAN_POINT('Ctrl Pts',(3.209715328,1.651136808,-6.512718759));
#135157=CARTESIAN_POINT('Ctrl Pts',(2.847323279,1.585954698,-6.667477045));
#135158=CARTESIAN_POINT('',(2.85165556048068,1.58673401523959,-6.66562529465689));
#135159=CARTESIAN_POINT('Origin',(-0.0599712233341998,1.48222903854166,
0.184313888207516));
#135160=CARTESIAN_POINT('Ctrl Pts',(2.94793442687893,1.6256495867408,-6.89635284857505));
#135161=CARTESIAN_POINT('Ctrl Pts',(2.93683471205565,1.62139779887027,-6.86988125968827));
#135162=CARTESIAN_POINT('Ctrl Pts',(2.92576188631293,1.61707840873292,-6.84340914287658));
#135163=CARTESIAN_POINT('Ctrl Pts',(2.91471797125889,1.61268792541888,-6.81693685259069));
#135164=CARTESIAN_POINT('Ctrl Pts',(2.90419032953264,1.60850268539221,-6.79170207068234));
#135165=CARTESIAN_POINT('Ctrl Pts',(2.89369444699762,1.6042538150892,-6.76646448526372));
#135166=CARTESIAN_POINT('Ctrl Pts',(2.88318704114662,1.59993003808792,-6.74124463351249));
#135167=CARTESIAN_POINT('Ctrl Pts',(2.8726793441522,1.5956061412817,-6.7160240829595));
#135168=CARTESIAN_POINT('Ctrl Pts',(2.86216881324473,1.5912088194187,-6.69081718391987));
#135169=CARTESIAN_POINT('Ctrl Pts',(2.85165556371443,1.5867340161584,-6.66562529299552));
#135170=CARTESIAN_POINT('Ctrl Pts',(3.178964521,1.585967065,-6.792951095));
#135171=CARTESIAN_POINT('Ctrl Pts',(3.117798973,1.59657582,-6.821575341));
#135172=CARTESIAN_POINT('Ctrl Pts',(3.056127904,1.607142857,-6.849093534));
#135173=CARTESIAN_POINT('Ctrl Pts',(2.743054426,1.660786473,-6.98878977));
#135174=CARTESIAN_POINT('Ctrl Pts',(2.418542048,1.715323387,-7.099341826));
#135175=CARTESIAN_POINT('Ctrl Pts',(2.41464316655942,1.71597862537066,-7.10067006303679));
#135176=CARTESIAN_POINT('Ctrl Pts',(2.41074428511884,1.71663386374133,-7.10199830007359));
#135177=CARTESIAN_POINT('Ctrl Pts',(2.855994272,1.585967065,-6.663767457));
#135178=CARTESIAN_POINT('Ctrl Pts',(2.795991928,1.59657582,-6.689483593));
#135179=CARTESIAN_POINT('Ctrl Pts',(2.735536241,1.607142857,-6.714115092));
#135180=CARTESIAN_POINT('Ctrl Pts',(2.428632656,1.660786473,-6.839157018));
#135181=CARTESIAN_POINT('Ctrl Pts',(2.11160135,1.715323387,-6.935678751));
#135182=CARTESIAN_POINT('Ctrl Pts',(2.10779235053235,1.71597862537066,-6.93683841953322));
#135183=CARTESIAN_POINT('Ctrl Pts',(2.1039833510647,1.71663386374133,-6.93799808806643));
#135184=CARTESIAN_POINT('Ctrl Pts',(2.1116013570794,1.71532338594482,-6.93567874963665));
#135185=CARTESIAN_POINT('Ctrl Pts',(2.12393574773601,1.71320157779459,-6.93192348391174));
#135186=CARTESIAN_POINT('Ctrl Pts',(2.12772423295924,1.71254943784492,-6.93075403377145));
#135187=CARTESIAN_POINT('Ctrl Pts',(2.14311900235626,1.70989962930861,-6.92600959375084));
#135188=CARTESIAN_POINT('Ctrl Pts',(2.15099216679657,1.70854407400994,-6.92356849105429));
#135189=CARTESIAN_POINT('Ctrl Pts',(2.17459329235689,1.70447938482579,-6.91620673459527));
#135190=CARTESIAN_POINT('Ctrl Pts',(2.19030881086288,1.70177120839844,-6.91124582897896));
#135191=CARTESIAN_POINT('Ctrl Pts',(2.23737969405122,1.69365497345755,-6.8962103172014));
#135192=CARTESIAN_POINT('Ctrl Pts',(2.26868412879233,1.68825095319847,-6.88597539031003));
#135193=CARTESIAN_POINT('Ctrl Pts',(2.36227728757173,1.67207515293314,-6.8546677331669));
#135194=CARTESIAN_POINT('Ctrl Pts',(2.42435327818651,1.66132115912265,-6.83295953415283));
#135195=CARTESIAN_POINT('Ctrl Pts',(2.60931157749119,1.62920289813894,-6.76544079017663));
#135196=CARTESIAN_POINT('Ctrl Pts',(2.73115276257568,1.60803074733088,-6.7171782188802));
#135197=CARTESIAN_POINT('Ctrl Pts',(2.8516555605562,1.5867340146619,-6.66562529507205));
#135198=CARTESIAN_POINT('Ctrl Pts',(1.95576969930549,1.71660033198358,-7.24051314774188));
#135199=CARTESIAN_POINT('Ctrl Pts',(1.95185398715275,1.71596185949179,-7.24156629787095));
#135200=CARTESIAN_POINT('Ctrl Pts',(1.947938275,1.715323387,-7.242619448));
#135201=CARTESIAN_POINT('Ctrl Pts',(1.554285971,1.651136808,-7.34849418));
#135202=CARTESIAN_POINT('Ctrl Pts',(1.151477492,1.585954698,-7.41107951600001));
#135203=CARTESIAN_POINT('Ctrl Pts',(2.11910088016766,1.71660033198358,-6.93339548231832));
#135204=CARTESIAN_POINT('Ctrl Pts',(2.11535111508383,1.71596185949179,-6.93453711665916));
#135205=CARTESIAN_POINT('Ctrl Pts',(2.11160135,1.715323387,-6.935678751));
#135206=CARTESIAN_POINT('Ctrl Pts',(1.734631949,1.651136808,-7.050448931));
#135207=CARTESIAN_POINT('Ctrl Pts',(1.347443968,1.585954698,-7.123685476));
#135208=CARTESIAN_POINT('',(1.35207303377562,1.58673401519647,-7.12280833071507));
#135209=CARTESIAN_POINT('Origin',(-0.0189470888890086,1.48222904029177,
0.192896751804501));
#135210=CARTESIAN_POINT('Ctrl Pts',(1.39650135047031,1.6256495867804,-7.36883871285757));
#135211=CARTESIAN_POINT('Ctrl Pts',(1.39135174990273,1.62139779887436,-7.34059990434166));
#135212=CARTESIAN_POINT('Ctrl Pts',(1.38622852329221,1.6170784087104,-7.31236636061691));
#135213=CARTESIAN_POINT('Ctrl Pts',(1.38113356873396,1.61268792536747,-7.28413886241582));
#135214=CARTESIAN_POINT('Ctrl Pts',(1.37627678961722,1.6085026853288,-7.2572309239418));
#135215=CARTESIAN_POINT('Ctrl Pts',(1.3714516299737,1.60425381503388,-7.23032707476029));
#135216=CARTESIAN_POINT('Ctrl Pts',(1.366611404198,1.59993003804022,-7.20343806747254));
#135217=CARTESIAN_POINT('Ctrl Pts',(1.36177104430736,1.59560614124161,-7.17654831513328));
#135218=CARTESIAN_POINT('Ctrl Pts',(1.35692498200514,1.59120881937363,-7.14967128595165));
#135219=CARTESIAN_POINT('Ctrl Pts',(1.35207303748469,1.58673401603004,-7.12280833022491));
#135220=CARTESIAN_POINT('Ctrl Pts',(1.64435841,1.585967065,-7.317519076));
#135221=CARTESIAN_POINT('Ctrl Pts',(1.578469512,1.59657582,-7.332325318));
#135222=CARTESIAN_POINT('Ctrl Pts',(1.51232468,1.607142857,-7.345942694));
#135223=CARTESIAN_POINT('Ctrl Pts',(1.176540125,1.660786473,-7.415071367));
#135224=CARTESIAN_POINT('Ctrl Pts',(0.835849241,1.715323387,-7.453278208));
#135225=CARTESIAN_POINT('Ctrl Pts',(0.831755981529315,1.71597862537066,
-7.453737247326));
#135226=CARTESIAN_POINT('Ctrl Pts',(0.82766272205863,1.71663386374133,-7.45419628665201));
#135227=CARTESIAN_POINT('Ctrl Pts',(1.356709689,1.585967065,-7.121926623));
#135228=CARTESIAN_POINT('Ctrl Pts',(1.292581958,1.59657582,-7.134142799));
#135229=CARTESIAN_POINT('Ctrl Pts',(1.228244647,1.607142857,-7.145202243));
#135230=CARTESIAN_POINT('Ctrl Pts',(0.901635979,1.660786473,-7.201345559));
#135231=CARTESIAN_POINT('Ctrl Pts',(0.57126737,1.715323387,-7.227458308));
#135232=CARTESIAN_POINT('Ctrl Pts',(0.567298128376246,1.71597862537066,
-7.22777204183371));
#135233=CARTESIAN_POINT('Ctrl Pts',(0.563328886752492,1.71663386374133,
-7.22808577566744));
#135234=CARTESIAN_POINT('Ctrl Pts',(0.571267377071571,1.71532338597849,
-7.22745830826502));
#135235=CARTESIAN_POINT('Ctrl Pts',(0.584120668103141,1.71320157775186,
-7.22644236793295));
#135236=CARTESIAN_POINT('Ctrl Pts',(0.58807197768213,1.71254943783057,-7.22611467124006));
#135237=CARTESIAN_POINT('Ctrl Pts',(0.604126740209036,1.70989962930403,
-7.22479057396694));
#135238=CARTESIAN_POINT('Ctrl Pts',(0.612340599370621,1.7085440740024,-7.22409904052771));
#135239=CARTESIAN_POINT('Ctrl Pts',(0.636972503771454,1.70447938481183,
-7.22198294221739));
#135240=CARTESIAN_POINT('Ctrl Pts',(0.653387050275347,1.70177120837809,
-7.2205163917624));
#135241=CARTESIAN_POINT('Ctrl Pts',(0.702589632971672,1.69365497342768,
-7.21595125041875));
#135242=CARTESIAN_POINT('Ctrl Pts',(0.735362394227467,1.68825095315395,
-7.21268513857028));
#135243=CARTESIAN_POINT('Ctrl Pts',(0.833497639285269,1.67207514933648,
-7.20222919738827));
#135244=CARTESIAN_POINT('Ctrl Pts',(0.898788938037303,1.66132115724861,
-7.19437302764026));
#135245=CARTESIAN_POINT('Ctrl Pts',(1.09393752057592,1.62920290096259,-7.16819340536559));
#135246=CARTESIAN_POINT('Ctrl Pts',(1.22330512767297,1.608030754495,-7.14725144361751));
#135247=CARTESIAN_POINT('Ctrl Pts',(1.35207303373849,1.58673401467295,-7.1228083309756));
#135248=CARTESIAN_POINT('Ctrl Pts',(0.353548592258207,1.71660033198358,
-7.49166664761222));
#135249=CARTESIAN_POINT('Ctrl Pts',(0.349498031129103,1.71596185949179,
-7.49185341330611));
#135250=CARTESIAN_POINT('Ctrl Pts',(0.34544747,1.715323387,-7.492040179));
#135251=CARTESIAN_POINT('Ctrl Pts',(-0.0617614,1.651136808,-7.51081600900001));
#135252=CARTESIAN_POINT('Ctrl Pts',(-0.468606438,1.585954698,-7.485346218));
#135253=CARTESIAN_POINT('Ctrl Pts',(0.579082400613263,1.71660033198358,
-7.22684059819051));
#135254=CARTESIAN_POINT('Ctrl Pts',(0.575174885306631,1.71596185949179,
-7.22714945309525));
#135255=CARTESIAN_POINT('Ctrl Pts',(0.57126737,1.715323387,-7.22745830800001));
#135256=CARTESIAN_POINT('Ctrl Pts',(0.178439107,1.651136808,-7.258507946));
#135257=CARTESIAN_POINT('Ctrl Pts',(-0.215440326,1.585954698,-7.246798291));
#135258=CARTESIAN_POINT('',(-0.210730924768195,1.58673401520766,-7.24693676522288));
#135259=CARTESIAN_POINT('Origin',(0.02296298988262,1.48222898981416,0.192460243053221));
#135260=CARTESIAN_POINT('Ctrl Pts',(-0.220230577341825,1.62564958673025,
-7.49676586842819));
#135261=CARTESIAN_POINT('Ctrl Pts',(-0.219189274043533,1.62139779886349,
-7.46808025586321));
#135262=CARTESIAN_POINT('Ctrl Pts',(-0.218123345138537,1.6170784087238,
-7.43940545450373));
#135263=CARTESIAN_POINT('Ctrl Pts',(-0.217031104751607,1.61268792540798,
-7.41074263500274));
#135264=CARTESIAN_POINT('Ctrl Pts',(-0.215989923663357,1.60850268537158,
-7.38341972517653));
#135265=CARTESIAN_POINT('Ctrl Pts',(-0.21491874152865,1.60425381506126,
-7.3561076063082));
#135266=CARTESIAN_POINT('Ctrl Pts',(-0.21386546378962,1.59993003805682,
-7.32880674356716));
#135267=CARTESIAN_POINT('Ctrl Pts',(-0.212812156865946,1.59560614124741,
-7.3015051243628));
#135268=CARTESIAN_POINT('Ctrl Pts',(-0.211767154034744,1.59120881937963,
-7.27421470500947));
#135269=CARTESIAN_POINT('Ctrl Pts',(-0.21073092149889,1.58673401597724,
-7.24693676549605));
#135270=CARTESIAN_POINT('Ctrl Pts',(0.032863927,1.585967065,-7.499927997));
#135271=CARTESIAN_POINT('Ctrl Pts',(-0.03466743,1.59657582,-7.500223913));
#135272=CARTESIAN_POINT('Ctrl Pts',(-0.102193166,1.607142857,-7.499303738));
#135273=CARTESIAN_POINT('Ctrl Pts',(-0.444987886,1.660786473,-7.494632467));
#135274=CARTESIAN_POINT('Ctrl Pts',(-0.785926947,1.715323387,-7.458707585));
#135275=CARTESIAN_POINT('Ctrl Pts',(-0.790023188214287,1.71597862537067,
-7.4582759624636));
#135276=CARTESIAN_POINT('Ctrl Pts',(-0.794119429428574,1.71663386374134,
-7.4578443399272));
#135277=CARTESIAN_POINT('Ctrl Pts',(-0.206013131,1.585967065,-7.247072415));
#135278=CARTESIAN_POINT('Ctrl Pts',(-0.271267708,1.59657582,-7.245217418));
#135279=CARTESIAN_POINT('Ctrl Pts',(-0.336478302,1.607142857,-7.242187677));
#135280=CARTESIAN_POINT('Ctrl Pts',(-0.667520194,1.660786473,-7.226807185));
#135281=CARTESIAN_POINT('Ctrl Pts',(-0.995778438,1.715323387,-7.181289947));
#135282=CARTESIAN_POINT('Ctrl Pts',(-0.999722324464808,1.71597862537067,
-7.18074307629029));
#135283=CARTESIAN_POINT('Ctrl Pts',(-1.00366621092962,1.71663386374134,
-7.18019620558059));
#135284=CARTESIAN_POINT('Ctrl Pts',(-0.995778431195552,1.71532338603152,
-7.18128994909741));
#135285=CARTESIAN_POINT('Ctrl Pts',(-0.983007246198175,1.71320157786637,
-7.18306083844871));
#135286=CARTESIAN_POINT('Ctrl Pts',(-0.979077870701436,1.71254943790544,
-7.18359021791031));
#135287=CARTESIAN_POINT('Ctrl Pts',(-0.963113817753805,1.70989962936613,
-7.18574837665296));
#135288=CARTESIAN_POINT('Ctrl Pts',(-0.954943334809972,1.70854407406466,
-7.1868387477902));
#135289=CARTESIAN_POINT('Ctrl Pts',(-0.930432412067507,1.70447938487425,
-7.19006725398254));
#135290=CARTESIAN_POINT('Ctrl Pts',(-0.914086363547438,1.70177120844069,
-7.19216363292857));
#135291=CARTESIAN_POINT('Ctrl Pts',(-0.865052739460746,1.69365497349035,
-7.19828232285063));
#135292=CARTESIAN_POINT('Ctrl Pts',(-0.832344069660024,1.68825095321702,
-7.20213774575369));
#135293=CARTESIAN_POINT('Ctrl Pts',(-0.734255462670462,1.6720751508552,
-7.21302243439045));
#135294=CARTESIAN_POINT('Ctrl Pts',(-0.668801789500237,1.66132115804658,
-7.21938563741333));
#135295=CARTESIAN_POINT('Ctrl Pts',(-0.47258780643187,1.62920289831347,
-7.23576925835512));
#135296=CARTESIAN_POINT('Ctrl Pts',(-0.341742814072663,1.60803074768566,
-7.24312712082469));
#135297=CARTESIAN_POINT('Ctrl Pts',(-0.210730924864113,1.58673401470343,
-7.2469367657027));
#135298=CARTESIAN_POINT('Ctrl Pts',(-1.26520405425852,1.71660033198358,
-7.39251814139622));
#135299=CARTESIAN_POINT('Ctrl Pts',(-1.26920006462926,1.71596185949179,
-7.39182978969811));
#135300=CARTESIAN_POINT('Ctrl Pts',(-1.273196075,1.715323387,-7.39114143800001));
#135301=CARTESIAN_POINT('Ctrl Pts',(-1.674920877,1.651136808,-7.321940429));
#135302=CARTESIAN_POINT('Ctrl Pts',(-2.066778852,1.585954698,-7.209606451));
#135303=CARTESIAN_POINT('Ctrl Pts',(-0.988013329107109,1.71660033198358,
-7.18236667945575));
#135304=CARTESIAN_POINT('Ctrl Pts',(-0.991895883553554,1.71596185949179,
-7.18182831322788));
#135305=CARTESIAN_POINT('Ctrl Pts',(-0.995778438,1.715323387,-7.181289947));
#135306=CARTESIAN_POINT('Ctrl Pts',(-1.386097349,1.651136808,-7.12716719800001));
#135307=CARTESIAN_POINT('Ctrl Pts',(-1.76825087,1.585954698,-7.031058872));
#135308=CARTESIAN_POINT('',(-1.7636813391673,1.58673401524348,-7.0322064913939));
#135309=CARTESIAN_POINT('Origin',(0.0637993173099696,1.4822290083721,0.183023894089098));
#135310=CARTESIAN_POINT('Ctrl Pts',(-1.82666476776868,1.62564958678102,
-7.27415258436543));
#135311=CARTESIAN_POINT('Ctrl Pts',(-1.81948125070448,1.62139779891109,
-7.24636147483946));
#135312=CARTESIAN_POINT('Ctrl Pts',(-1.81227600790523,1.61707840876749,
-7.21858621756028));
#135313=CARTESIAN_POINT('Ctrl Pts',(-1.80504764454274,1.61268792544544,
-7.19082831818906));
#135314=CARTESIAN_POINT('Ctrl Pts',(-1.79815718774571,1.60850268542199,
-7.16436802603133));
#135315=CARTESIAN_POINT('Ctrl Pts',(-1.7912397511775,1.60425381510532,-7.13792472184617));
#135316=CARTESIAN_POINT('Ctrl Pts',(-1.7843422201044,1.59993003810657,-7.11148856171909));
#135317=CARTESIAN_POINT('Ctrl Pts',(-1.77744449791178,1.5956061413029,-7.08505166908843));
#135318=CARTESIAN_POINT('Ctrl Pts',(-1.77055729322817,1.59120881945812,
-7.05862392934178));
#135319=CARTESIAN_POINT('Ctrl Pts',(-1.7636813350497,1.58673401625577,-7.03220649222103));
#135320=CARTESIAN_POINT('Ctrl Pts',(-1.580167237,1.585967065,-7.331648621));
#135321=CARTESIAN_POINT('Ctrl Pts',(-1.646183361,1.59657582,-7.317420373));
#135322=CARTESIAN_POINT('Ctrl Pts',(-1.711932572,1.607142857,-7.302005674));
#135323=CARTESIAN_POINT('Ctrl Pts',(-2.045708757,1.660786473,-7.223752884));
#135324=CARTESIAN_POINT('Ctrl Pts',(-2.370954065,1.715323387,-7.115376084));
#135325=CARTESIAN_POINT('Ctrl Pts',(-2.37486175229012,1.71597862537066,
-7.11407398176059));
#135326=CARTESIAN_POINT('Ctrl Pts',(-2.37876943958024,1.71663386374133,
-7.11277187952119));
#135327=CARTESIAN_POINT('Ctrl Pts',(-1.759103005,1.585967065,-7.033353156));
#135328=CARTESIAN_POINT('Ctrl Pts',(-1.822433198,1.59657582,-7.017513722));
#135329=CARTESIAN_POINT('Ctrl Pts',(-1.885467899,1.607142857,-7.000536465));
#135330=CARTESIAN_POINT('Ctrl Pts',(-2.205463864,1.660786473,-6.914351339));
#135331=CARTESIAN_POINT('Ctrl Pts',(-2.516262752,1.715323387,-6.79933245));
#135332=CARTESIAN_POINT('Ctrl Pts',(-2.51999687155391,1.71597862537066,
-6.79795054581994));
#135333=CARTESIAN_POINT('Ctrl Pts',(-2.52373099110783,1.71663386374133,
-6.79656864163989));
#135334=CARTESIAN_POINT('Ctrl Pts',(-2.5162627369183,1.71532338435357,-6.79933245558136));
#135335=CARTESIAN_POINT('Ctrl Pts',(-2.37664964043737,1.69082501025532,
-6.85099976765249));
#135336=CARTESIAN_POINT('Ctrl Pts',(-2.23573125128583,1.66647816528029,
-6.89825663970194));
#135337=CARTESIAN_POINT('Ctrl Pts',(-2.09392556770815,1.64234941096584,
-6.94103563718671));
#135338=CARTESIAN_POINT('Ctrl Pts',(-2.02463516259193,1.63055939579003,
-6.96193870673513));
#135339=CARTESIAN_POINT('Ctrl Pts',(-1.95513298040099,1.61882140076076,
-6.98177343537018));
#135340=CARTESIAN_POINT('Ctrl Pts',(-1.88546789921594,1.60714285706073,
-7.00053646515667));
#135341=CARTESIAN_POINT('Ctrl Pts',(-1.84500356901233,1.60035948112099,
-7.01143480091374));
#135342=CARTESIAN_POINT('Ctrl Pts',(-1.80440519902882,1.59355605149649,
-7.0219929241046));
#135343=CARTESIAN_POINT('Ctrl Pts',(-1.76368133918351,1.58673401465524,
-7.03220649106564));
#135344=CARTESIAN_POINT('Ctrl Pts',(-2.82479716579741,1.71660033198358,
-6.94770370202509));
#135345=CARTESIAN_POINT('Ctrl Pts',(-2.8285517763987,1.71596185949179,-6.94617241951255));
#135346=CARTESIAN_POINT('Ctrl Pts',(-2.832306387,1.715323387,-6.944641137));
#135347=CARTESIAN_POINT('Ctrl Pts',(-3.209762915,1.651136808,-6.790699053));
#135348=CARTESIAN_POINT('Ctrl Pts',(-3.568310983,1.585954698,-6.596753499));
#135349=CARTESIAN_POINT('Ctrl Pts',(-2.50891065267966,1.71660033198358,
-6.80205327793971));
#135350=CARTESIAN_POINT('Ctrl Pts',(-2.51258670233983,1.71596185949179,
-6.80069286396985));
#135351=CARTESIAN_POINT('Ctrl Pts',(-2.516262752,1.715323387,-6.79933245));
#135352=CARTESIAN_POINT('Ctrl Pts',(-2.885821433,1.651136808,-6.662568032));
#135353=CARTESIAN_POINT('Ctrl Pts',(-3.238379968,1.585954698,-6.486554955));
#135354=CARTESIAN_POINT('',(-3.23416397512505,1.58673401528033,-6.48865805732195));
#135355=CARTESIAN_POINT('Origin',(0.101652530209534,1.48222898518188,0.16503009862893));
#135356=CARTESIAN_POINT('Ctrl Pts',(-3.3476861436547,1.62564958677245,-6.71140801016537));
#135357=CARTESIAN_POINT('Ctrl Pts',(-3.33469630621779,1.62139779889616,
-6.68581088513764));
#135358=CARTESIAN_POINT('Ctrl Pts',(-3.32168865877955,1.61707840874773,
-6.66023391214072));
#135359=CARTESIAN_POINT('Ctrl Pts',(-3.30866216274858,1.6126879254223,-6.63467886147285));
#135360=CARTESIAN_POINT('Ctrl Pts',(-3.29624462038393,1.60850268538805,
-6.61031844071623));
#135361=CARTESIAN_POINT('Ctrl Pts',(-3.28380438072982,1.6042538150954,-6.58598041070878));
#135362=CARTESIAN_POINT('Ctrl Pts',(-3.27138511704215,1.59993003810284,
-6.56164507859974));
#135363=CARTESIAN_POINT('Ctrl Pts',(-3.2589655092365,1.59560614130533,-6.53730907219748));
#135364=CARTESIAN_POINT('Ctrl Pts',(-3.24655814078463,1.59120881943997,
-6.51297974367117));
#135365=CARTESIAN_POINT('Ctrl Pts',(-3.2341639711417,1.58673401616681,-6.48865805919337));
#135366=CARTESIAN_POINT('Ctrl Pts',(-3.119311536,1.585967065,-6.820549504));
#135367=CARTESIAN_POINT('Ctrl Pts',(-3.180725587,1.59657582,-6.792462389));
#135368=CARTESIAN_POINT('Ctrl Pts',(-3.241623914,1.607142857,-6.763273941));
#135369=CARTESIAN_POINT('Ctrl Pts',(-3.55077456,1.660786473,-6.615098643));
#135370=CARTESIAN_POINT('Ctrl Pts',(-3.845118005,1.715323387,-6.439337507));
#135371=CARTESIAN_POINT('Ctrl Pts',(-3.84865441924078,1.71597862537066,
-6.43722580995057));
#135372=CARTESIAN_POINT('Ctrl Pts',(-3.85219083348155,1.71663386374133,
-6.43511411290114));
#135373=CARTESIAN_POINT('Ctrl Pts',(-3.229939179,1.585967065,-6.49076212));
#135374=CARTESIAN_POINT('Ctrl Pts',(-3.288383736,1.59657582,-6.461678884));
#135375=CARTESIAN_POINT('Ctrl Pts',(-3.346295113,1.607142857,-6.431547949));
#135376=CARTESIAN_POINT('Ctrl Pts',(-3.640282496,1.660786473,-6.278588109));
#135377=CARTESIAN_POINT('Ctrl Pts',(-3.919089417,1.715323387,-6.09944572399999));
#135378=CARTESIAN_POINT('Ctrl Pts',(-3.92243916635777,1.71597862537066,
-6.09729340264818));
#135379=CARTESIAN_POINT('Ctrl Pts',(-3.92578891571553,1.71663386374133,
-6.09514108129637));
#135380=CARTESIAN_POINT('Ctrl Pts',(-3.9190894113225,1.71532338611378,-6.09944572779726));
#135381=CARTESIAN_POINT('Ctrl Pts',(-3.79384736364693,1.69082501703781,
-6.17991775846372));
#135382=CARTESIAN_POINT('Ctrl Pts',(-3.66638243065307,1.66647817789189,
-6.25636306151695));
#135383=CARTESIAN_POINT('Ctrl Pts',(-3.53708834177104,1.64234943014875,
-6.32862592241045));
#135384=CARTESIAN_POINT('Ctrl Pts',(-3.47391141500436,1.63055940832857,
-6.36393569960209));
#135385=CARTESIAN_POINT('Ctrl Pts',(-3.41029800108025,1.61882140691879,
-6.39824763726708));
#135386=CARTESIAN_POINT('Ctrl Pts',(-3.34629511360955,1.60714285711122,
-6.43154794868285));
#135387=CARTESIAN_POINT('Ctrl Pts',(-3.30911963545218,1.60035948098744,
-6.45089012269899));
#135388=CARTESIAN_POINT('Ctrl Pts',(-3.2717401159293,1.5935560511928,-6.46992885310997));
#135389=CARTESIAN_POINT('Ctrl Pts',(-3.234163976,1.586734015,-6.488658057));
#135390=CARTESIAN_POINT('Ctrl Pts',(-4.25230590117908,1.71660033198358,
-6.17802236055207));
#135391=CARTESIAN_POINT('Ctrl Pts',(-4.25564355058954,1.71596185949179,
-6.17571974827603));
#135392=CARTESIAN_POINT('Ctrl Pts',(-4.2589812,1.715323387,-6.173417136));
#135393=CARTESIAN_POINT('Ctrl Pts',(-4.594520006,1.651136808,-5.941932136));
#135394=CARTESIAN_POINT('Ctrl Pts',(-4.90299285900001,1.585954698,-5.675443685));
#135395=CARTESIAN_POINT('Ctrl Pts',(-3.91249410326131,1.71660033198358,
-6.10368342451692));
#135396=CARTESIAN_POINT('Ctrl Pts',(-3.91579176013065,1.71596185949179,
-6.10156457425846));
#135397=CARTESIAN_POINT('Ctrl Pts',(-3.919089417,1.715323387,-6.09944572400001));
#135398=CARTESIAN_POINT('Ctrl Pts',(-4.250607714,1.651136808,-5.88643459));
#135399=CARTESIAN_POINT('Ctrl Pts',(-4.55708601800001,1.585954698,-5.63874693700001));
#135400=CARTESIAN_POINT('',(-4.55342069719549,1.58673401524202,-5.64170718400532));
#135401=CARTESIAN_POINT('Origin',(0.134752473701915,1.48222900232617,0.139319403200179));
#135402=CARTESIAN_POINT('Ctrl Pts',(-4.71217343650642,1.62564958679273,
-5.83484545654915));
#135403=CARTESIAN_POINT('Ctrl Pts',(-4.69398466915291,1.62139779886915,
-5.81263920890564));
#135404=CARTESIAN_POINT('Ctrl Pts',(-4.67578284009688,1.61707840871869,
-5.79045647096182));
#135405=CARTESIAN_POINT('Ctrl Pts',(-4.65756731577416,1.61268792538905,
-5.76829919469481));
#135406=CARTESIAN_POINT('Ctrl Pts',(-4.64020331825134,1.60850268535374,
-5.74717771153594));
#135407=CARTESIAN_POINT('Ctrl Pts',(-4.62282196747897,1.60425381505011,
-5.72608297484968));
#135408=CARTESIAN_POINT('Ctrl Pts',(-4.60546168216947,1.59993003806062,
-5.7049863638248));
#135409=CARTESIAN_POINT('Ctrl Pts',(-4.58810091583422,1.59560614126618,
-5.68388916824656));
#135410=CARTESIAN_POINT('Ctrl Pts',(-4.57075353820189,1.59120881941508,
-5.66279586335943));
#135411=CARTESIAN_POINT('Ctrl Pts',(-4.55342069426911,1.58673401611734,
-5.64170718630423));
#135412=CARTESIAN_POINT('Ctrl Pts',(-4.512600295,1.585967065,-5.99052907300001));
#135413=CARTESIAN_POINT('Ctrl Pts',(-4.566540621,1.59657582,-5.949896413));
#135414=CARTESIAN_POINT('Ctrl Pts',(-4.619740525,1.607142857,-5.908299035));
#135415=CARTESIAN_POINT('Ctrl Pts',(-4.889810092,1.660786473,-5.697129743));
#135416=CARTESIAN_POINT('Ctrl Pts',(-5.139488502,1.715323387,-5.462202664));
#135417=CARTESIAN_POINT('Ctrl Pts',(-5.14248828439617,1.71597862537066,
-5.45938011271906));
#135418=CARTESIAN_POINT('Ctrl Pts',(-5.14548806679234,1.71663386374133,
-5.45655756143813));
#135419=CARTESIAN_POINT('Ctrl Pts',(-4.549746986,1.585967065,-5.644670262));
#135420=CARTESIAN_POINT('Ctrl Pts',(-4.600573106,1.59657582,-5.603703124));
#135421=CARTESIAN_POINT('Ctrl Pts',(-4.650653287,1.607142857,-5.561827398));
#135422=CARTESIAN_POINT('Ctrl Pts',(-4.904885564,1.660786473,-5.349245077));
#135423=CARTESIAN_POINT('Ctrl Pts',(-5.138663817,1.715323387,-5.114355695));
#135424=CARTESIAN_POINT('Ctrl Pts',(-5.14147256561369,1.71597862537066,
-5.11153359663286));
#135425=CARTESIAN_POINT('Ctrl Pts',(-5.14428131422739,1.71663386374133,
-5.10871149826573));
#135426=CARTESIAN_POINT('Ctrl Pts',(-5.13866380557472,1.71532338433466,
-5.11435570647959));
#135427=CARTESIAN_POINT('Ctrl Pts',(-5.03364892658114,1.69082500890268,
-5.21986971217025));
#135428=CARTESIAN_POINT('Ctrl Pts',(-4.92559750013,1.66647816264222,-5.3219289887372));
#135429=CARTESIAN_POINT('Ctrl Pts',(-4.81486057615405,1.6423494070885,-5.42029682131852));
#135430=CARTESIAN_POINT('Ctrl Pts',(-4.76075128450724,1.63055939320285,
-5.46836221405928));
#135431=CARTESIAN_POINT('Ctrl Pts',(-4.70600120464847,1.61882139945801,
-5.5155469299307));
#135432=CARTESIAN_POINT('Ctrl Pts',(-4.6506532871449,1.60714285703281,-5.56182739798854));
#135433=CARTESIAN_POINT('Ctrl Pts',(-4.61850494796888,1.60035948119918,
-5.58870899100399));
#135434=CARTESIAN_POINT('Ctrl Pts',(-4.58609210673901,1.59355605171779,
-5.61533809689503));
#135435=CARTESIAN_POINT('Ctrl Pts',(-4.55342069759857,1.58673401469568,
-5.64170718436339));
#135436=CARTESIAN_POINT('Ctrl Pts',(-5.48098153912164,1.71660033198358,
-5.11946355990375));
#135437=CARTESIAN_POINT('Ctrl Pts',(-5.48374616256082,1.71596185949179,
-5.11649728545188));
#135438=CARTESIAN_POINT('Ctrl Pts',(-5.486510786,1.715323387,-5.113531011));
#135439=CARTESIAN_POINT('Ctrl Pts',(-5.76444244800001,1.651136808,-4.815327076));
#135440=CARTESIAN_POINT('Ctrl Pts',(-6.008416238,1.585954698,-4.488756433));
#135441=CARTESIAN_POINT('Ctrl Pts',(-5.13313367838099,1.71660033198358,
-5.11991211792546));
#135442=CARTESIAN_POINT('Ctrl Pts',(-5.13589874769049,1.71596185949179,
-5.11713390646273));
#135443=CARTESIAN_POINT('Ctrl Pts',(-5.13866381700001,1.715323387,-5.114355695));
#135444=CARTESIAN_POINT('Ctrl Pts',(-5.416640303,1.651136808,-4.835058009));
#135445=CARTESIAN_POINT('Ctrl Pts',(-5.662707791,1.585954698,-4.52727738));
#135446=CARTESIAN_POINT('',(-5.65976452852026,1.58673401523511,-4.53095635414236));
#135447=CARTESIAN_POINT('Origin',(0.161551673038854,1.48222901763502,0.107094477920148));
#135448=CARTESIAN_POINT('Ctrl Pts',(-5.85632473635433,1.62564958674453,
-4.68545201425031));
#135449=CARTESIAN_POINT('Ctrl Pts',(-5.83378752536501,1.62139779883973,
-4.66767498378072));
#135450=CARTESIAN_POINT('Ctrl Pts',(-5.81124261200344,1.61707840867752,
-4.64992372110351));
#135451=CARTESIAN_POINT('Ctrl Pts',(-5.78868979708449,1.61268792533566,
-4.63220026889469));
#135452=CARTESIAN_POINT('Ctrl Pts',(-5.76719126574319,1.6085026853083,-4.61530534051628));
#135453=CARTESIAN_POINT('Ctrl Pts',(-5.74568153657526,1.60425381501317,
-4.59844026372362));
#135454=CARTESIAN_POINT('Ctrl Pts',(-5.72419197744197,1.5999300380356,-4.5815688279632));
#135455=CARTESIAN_POINT('Ctrl Pts',(-5.70270182286744,1.59560614125309,
-4.56469692472233));
#135456=CARTESIAN_POINT('Ctrl Pts',(-5.68122558035585,1.59120881941638,
-4.54782594303467));
#135457=CARTESIAN_POINT('Ctrl Pts',(-5.65976452599462,1.58673401627607,
-4.53095635732274));
#135458=CARTESIAN_POINT('Ctrl Pts',(-5.69488488000001,1.585967065,-4.88039816));
#135459=CARTESIAN_POINT('Ctrl Pts',(-5.73882929,1.59657582,-4.82911989400001));
#135460=CARTESIAN_POINT('Ctrl Pts',(-5.781843203,1.607142857,-4.777058632));
#135461=CARTESIAN_POINT('Ctrl Pts',(-6.000203538,1.660786473,-4.512769388));
#135462=CARTESIAN_POINT('Ctrl Pts',(-6.193542228,1.715323387,-4.229661295));
#135463=CARTESIAN_POINT('Ctrl Pts',(-6.19586511206018,1.71597862537066,
-4.22625986884708));
#135464=CARTESIAN_POINT('Ctrl Pts',(-6.19818799612036,1.71663386374133,
-4.22285844269416));
#135465=CARTESIAN_POINT('Ctrl Pts',(-5.656813681,1.585967065,-4.53463989500001));
#135466=CARTESIAN_POINT('Ctrl Pts',(-5.697644791,1.59657582,-4.483704433));
#135467=CARTESIAN_POINT('Ctrl Pts',(-5.737552082,1.607142857,-4.43204198));
#135468=CARTESIAN_POINT('Ctrl Pts',(-5.940141634,1.660786473,-4.169777291));
#135469=CARTESIAN_POINT('Ctrl Pts',(-6.117960008,1.715323387,-3.890124078));
#135470=CARTESIAN_POINT('Ctrl Pts',(-6.12009642190956,1.71597862537066,
-3.88676416079535));
#135471=CARTESIAN_POINT('Ctrl Pts',(-6.12223283581911,1.71663386374133,
-3.8834042435907));
#135472=CARTESIAN_POINT('Ctrl Pts',(-6.11795999903966,1.71532338425187,
-3.89012409209184));
#135473=CARTESIAN_POINT('Ctrl Pts',(-6.0380827030761,1.69082500927857,-4.01574633149173));
#135474=CARTESIAN_POINT('Ctrl Pts',(-5.95449718812239,1.66647816346924,
-4.13864737958845));
#135475=CARTESIAN_POINT('Ctrl Pts',(-5.86749540988425,1.64234940833118,
-4.25852059023017));
#135476=CARTESIAN_POINT('Ctrl Pts',(-5.8249838006051,1.6305593940166,-4.31709414122001));
#135477=CARTESIAN_POINT('Ctrl Pts',(-5.78165706483856,1.61882139983996,
-4.37494535553091));
#135478=CARTESIAN_POINT('Ctrl Pts',(-5.73755208192497,1.60714285697828,
-4.43204198016065));
#135479=CARTESIAN_POINT('Ctrl Pts',(-5.71193410050092,1.60035948104102,
-4.46520603929647));
#135480=CARTESIAN_POINT('Ctrl Pts',(-5.68600352387605,1.59355605151279,
-4.49818037433353));
#135481=CARTESIAN_POINT('Ctrl Pts',(-5.6597645284826,1.58673401451738,-4.53095635396281));
#135482=CARTESIAN_POINT('Ctrl Pts',(-6.45337257147076,1.71660033198358,
-3.82152433181392));
#135483=CARTESIAN_POINT('Ctrl Pts',(-6.45543489823538,1.71596185949179,
-3.81803309490696));
#135484=CARTESIAN_POINT('Ctrl Pts',(-6.457497225,1.715323387,-3.814541858));
#135485=CARTESIAN_POINT('Ctrl Pts',(-6.664825969,1.651136808,-3.463562675));
#135486=CARTESIAN_POINT('Ctrl Pts',(-6.832892752,1.585954698,-3.092179918));
#135487=CARTESIAN_POINT('Ctrl Pts',(-6.1137536276454,1.71660033198358,-3.8967394111811));
#135488=CARTESIAN_POINT('Ctrl Pts',(-6.11585681782271,1.71596185949179,
-3.89343174459055));
#135489=CARTESIAN_POINT('Ctrl Pts',(-6.117960008,1.715323387,-3.890124078));
#135490=CARTESIAN_POINT('Ctrl Pts',(-6.329396811,1.651136808,-3.557599489));
#135491=CARTESIAN_POINT('Ctrl Pts',(-6.503547641,1.585954698,-3.204117364));
#135492=CARTESIAN_POINT('',(-6.50146406149294,1.58673401531619,-3.20834303967259));
#135493=CARTESIAN_POINT('Origin',(0.180796891847448,1.48222900349585,0.0698618628709807));
#135494=CARTESIAN_POINT('Ctrl Pts',(-6.72664080068503,1.625649586757,-3.31697204352363));
#135495=CARTESIAN_POINT('Ctrl Pts',(-6.70080896102677,1.6213977988843,-3.3044554644234));
#135496=CARTESIAN_POINT('Ctrl Pts',(-6.67497513854352,1.61707840873839,
-3.29196570633431));
#135497=CARTESIAN_POINT('Ctrl Pts',(-6.64913957764186,1.61268792541326,
-3.27950480713941));
#135498=CARTESIAN_POINT('Ctrl Pts',(-6.62451175980181,1.60850268538798,
-3.26762642150408));
#135499=CARTESIAN_POINT('Ctrl Pts',(-6.59987942312048,1.60425381509443,
-3.25577959675733));
#135500=CARTESIAN_POINT('Ctrl Pts',(-6.57526541791268,1.59993003811615,
-3.24392222576583));
#135501=CARTESIAN_POINT('Ctrl Pts',(-6.5506507306901,1.59560614133292,-3.2320645262255));
#135502=CARTESIAN_POINT('Ctrl Pts',(-6.52604982838255,1.59120881949136,
-3.22020473601114));
#135503=CARTESIAN_POINT('Ctrl Pts',(-6.50146405949292,1.58673401619063,
-3.20834304338622));
#135504=CARTESIAN_POINT('Ctrl Pts',(-6.610882977,1.585967065,-3.542065254));
#135505=CARTESIAN_POINT('Ctrl Pts',(-6.64277668,1.59657582,-3.482539096));
#135506=CARTESIAN_POINT('Ctrl Pts',(-6.673593319,1.607142857,-3.422448278));
#135507=CARTESIAN_POINT('Ctrl Pts',(-6.830034135,1.660786473,-3.117396951));
#135508=CARTESIAN_POINT('Ctrl Pts',(-6.957992803,1.715323387,-2.799345666));
#135509=CARTESIAN_POINT('Ctrl Pts',(-6.95953017325041,1.71597862537066,
-2.7955244119083));
#135510=CARTESIAN_POINT('Ctrl Pts',(-6.96106754350082,1.71663386374133,
-2.7917031578166));
#135511=CARTESIAN_POINT('Ctrl Pts',(-6.499374055,1.585967065,-3.212574807));
#135512=CARTESIAN_POINT('Ctrl Pts',(-6.528300937,1.59657582,-3.154052706));
#135513=CARTESIAN_POINT('Ctrl Pts',(-6.556169318,1.607142857,-3.095019205));
#135514=CARTESIAN_POINT('Ctrl Pts',(-6.697643284,1.660786473,-2.795335353));
#135515=CARTESIAN_POINT('Ctrl Pts',(-6.811187188,1.715323387,-2.483994583));
#135516=CARTESIAN_POINT('Ctrl Pts',(-6.81255137084789,1.71597862537066,
-2.48025395295892));
#135517=CARTESIAN_POINT('Ctrl Pts',(-6.81391555369579,1.71663386374133,
-2.47651332291784));
#135518=CARTESIAN_POINT('Ctrl Pts',(-6.81118718586599,1.71532338609523,
-2.483994589877));
#135519=CARTESIAN_POINT('Ctrl Pts',(-6.7601824533748,1.69082501482219,-2.62385108575496));
#135520=CARTESIAN_POINT('Ctrl Pts',(-6.70497122496998,1.66647817350564,
-2.76184716434788));
#135521=CARTESIAN_POINT('Ctrl Pts',(-6.64577271151913,1.64234942362513,
-2.8976205874493));
#135522=CARTESIAN_POINT('Ctrl Pts',(-6.61684656990636,1.63055940398956,
-2.96396349092682));
#135523=CARTESIAN_POINT('Ctrl Pts',(-6.58696907752558,1.6188214047438,-3.02977617227563));
#135524=CARTESIAN_POINT('Ctrl Pts',(-6.55616931819621,1.6071428570744,-3.09501920458437));
#135525=CARTESIAN_POINT('Ctrl Pts',(-6.53827956256854,1.60035948094352,
-3.13291501639681));
#135526=CARTESIAN_POINT('Ctrl Pts',(-6.52004373512448,1.59355605121258,
-3.17069273876414));
#135527=CARTESIAN_POINT('Ctrl Pts',(-6.501464062,1.586734015,-3.208343039));
#135528=CARTESIAN_POINT('Ctrl Pts',(-7.12401107506173,1.71660033198358,
-2.34489487403908));
#135529=CARTESIAN_POINT('Ctrl Pts',(-7.12527467303087,1.71596185949179,
-2.34104192101954));
#135530=CARTESIAN_POINT('Ctrl Pts',(-7.126538271,1.715323387,-2.337188968));
#135531=CARTESIAN_POINT('Ctrl Pts',(-7.253569634,1.651136808,-1.949845932));
#135532=CARTESIAN_POINT('Ctrl Pts',(-7.337870794,1.585954698,-1.551016507));
#135533=CARTESIAN_POINT('Ctrl Pts',(-6.80850125154208,1.71660033198358,
-2.49135950079383));
#135534=CARTESIAN_POINT('Ctrl Pts',(-6.80984421977104,1.71596185949179,
-2.48767704189691));
#135535=CARTESIAN_POINT('Ctrl Pts',(-6.811187188,1.715323387,-2.483994583));
#135536=CARTESIAN_POINT('Ctrl Pts',(-6.94619776,1.651136808,-2.113791572));
#135537=CARTESIAN_POINT('Ctrl Pts',(-7.040288831,1.585954698,-1.731136382));
#135538=CARTESIAN_POINT('',(-7.03916235977438,1.5867340151941,-1.73571117135257));
#135539=CARTESIAN_POINT('Origin',(0.191587870767866,1.48222903349934,0.0293624495522038));
#135540=CARTESIAN_POINT('Ctrl Pts',(-7.28242661707383,1.62564958676879,
-1.79339414618027));
#135541=CARTESIAN_POINT('Ctrl Pts',(-7.25450801706566,1.62139779883678,
-1.78672327941274));
#135542=CARTESIAN_POINT('Ctrl Pts',(-7.22659324614458,1.61707840868643,
-1.78007903323404));
#135543=CARTESIAN_POINT('Ctrl Pts',(-7.19868298126379,1.61268792535802,
-1.77346334495163));
#135544=CARTESIAN_POINT('Ctrl Pts',(-7.17207744626429,1.60850268532689,
-1.7671569223184));
#135545=CARTESIAN_POINT('Ctrl Pts',(-7.14547428273646,1.60425381502804,
-1.76088229411126));
#135546=CARTESIAN_POINT('Ctrl Pts',(-7.11888675499135,1.59993003803373,
-1.75459342542346));
#135547=CARTESIAN_POINT('Ctrl Pts',(-7.09229849054833,1.59560614123448,
-1.74830438248116));
#135548=CARTESIAN_POINT('Ctrl Pts',(-7.0657232393096,1.59120881937443,-1.74201033436875));
#135549=CARTESIAN_POINT('Ctrl Pts',(-7.03916235886331,1.58673401603955,
-1.73571117489813));
#135550=CARTESIAN_POINT('Ctrl Pts',(-7.21776353400001,1.585967065,-2.038109313));
#135551=CARTESIAN_POINT('Ctrl Pts',(-7.236115215,1.59657582,-1.97311864));
#135552=CARTESIAN_POINT('Ctrl Pts',(-7.253293629,1.607142857,-1.907808045));
#135553=CARTESIAN_POINT('Ctrl Pts',(-7.340499928,1.660786473,-1.576258498));
#135554=CARTESIAN_POINT('Ctrl Pts',(-7.397095368,1.715323387,-1.238135744));
#135555=CARTESIAN_POINT('Ctrl Pts',(-7.39777533870557,1.71597862537066,
-1.23407333954463));
#135556=CARTESIAN_POINT('Ctrl Pts',(-7.39845530941115,1.71663386374133,
-1.23001093508926));
#135557=CARTESIAN_POINT('Ctrl Pts',(-7.038030922,1.585967065,-1.740293292));
#135558=CARTESIAN_POINT('Ctrl Pts',(-7.053700988,1.59657582,-1.67692098));
#135559=CARTESIAN_POINT('Ctrl Pts',(-7.068227363,1.607142857,-1.613276771));
#135560=CARTESIAN_POINT('Ctrl Pts',(-7.141970577,1.660786473,-1.290186641));
#135561=CARTESIAN_POINT('Ctrl Pts',(-7.185930826,1.715323387,-0.961716262));
#135562=CARTESIAN_POINT('Ctrl Pts',(-7.18645899013354,1.71597862537066,
-0.957769826821296));
#135563=CARTESIAN_POINT('Ctrl Pts',(-7.18698715426708,1.71663386374133,
-0.953823391642592));
#135564=CARTESIAN_POINT('Ctrl Pts',(-7.18593082383186,1.7153233843102,-0.96171627820039));
#135565=CARTESIAN_POINT('Ctrl Pts',(-7.16618356659928,1.69082501418126,
-1.10926751150146));
#135566=CARTESIAN_POINT('Ctrl Pts',(-7.14192822398185,1.66647817310497,
-1.25590609992664));
#135567=CARTESIAN_POINT('Ctrl Pts',(-7.11330101035654,1.64234942258282,
-1.40123115002223));
#135568=CARTESIAN_POINT('Ctrl Pts',(-7.09931290954574,1.63055940350657,
-1.47224125522062));
#135569=CARTESIAN_POINT('Ctrl Pts',(-7.08428171779415,1.61882140460229,
-1.54293804795029));
#135570=CARTESIAN_POINT('Ctrl Pts',(-7.06822736322912,1.60714285705965,
-1.61327677087489));
#135571=CARTESIAN_POINT('Ctrl Pts',(-7.05890234030263,1.60035948115203,
-1.65413236680542));
#135572=CARTESIAN_POINT('Ctrl Pts',(-7.04921395033693,1.59355605159159,
-1.69494702943989));
#135573=CARTESIAN_POINT('Ctrl Pts',(-7.03916236003226,1.58673401462371,
-1.7357111713207));
#135574=CARTESIAN_POINT('Ctrl Pts',(-7.46153873851908,1.71660033198358,
-0.758620738679522));
#135575=CARTESIAN_POINT('Ctrl Pts',(-7.46194452325954,1.71596185949179,
-0.754586229339761));
#135576=CARTESIAN_POINT('Ctrl Pts',(-7.462350308,1.715323387,-0.75055172));
#135577=CARTESIAN_POINT('Ctrl Pts',(-7.503144445,1.651136808,-0.34495656));
#135578=CARTESIAN_POINT('Ctrl Pts',(-7.49973815400001,1.585954698,0.062670712));
#135579=CARTESIAN_POINT('Ctrl Pts',(-7.18489092487628,1.71660033198358,
-0.969486389062758));
#135580=CARTESIAN_POINT('Ctrl Pts',(-7.18541087543814,1.71596185949179,
-0.965601325531379));
#135581=CARTESIAN_POINT('Ctrl Pts',(-7.185930826,1.715323387,-0.961716262));
#135582=CARTESIAN_POINT('Ctrl Pts',(-7.23820222100001,1.651136808,-0.571145109));
#135583=CARTESIAN_POINT('Ctrl Pts',(-7.247833941,1.585954698,-0.177209386));
#135584=CARTESIAN_POINT('',(-7.24771725026763,1.58673401517814,-0.18191937719729));
#135585=CARTESIAN_POINT('Origin',(0.193420936396731,1.48222900303388,-0.0125097447096686));
#135586=CARTESIAN_POINT('Ctrl Pts',(-7.49769425876711,1.62564958680033,
-0.185959131992468));
#135587=CARTESIAN_POINT('Ctrl Pts',(-7.46899434096227,1.62139779886003,
-0.185445900051847));
#135588=CARTESIAN_POINT('Ctrl Pts',(-7.4403038853534,1.61707840871034,-0.184957843259731));
#135589=CARTESIAN_POINT('Ctrl Pts',(-7.41162396954117,1.61268792538127,
-0.184496708034791));
#135590=CARTESIAN_POINT('Ctrl Pts',(-7.38428476270878,1.60850268534733,
-0.184057129642196));
#135591=CARTESIAN_POINT('Ctrl Pts',(-7.35695470676653,1.60425381504928,
-0.183648092577493));
#135592=CARTESIAN_POINT('Ctrl Pts',(-7.32963685977038,1.5999300380482,-0.183221786703882));
#135593=CARTESIAN_POINT('Ctrl Pts',(-7.30231825584026,1.59560614124216,
-0.182795469018011));
#135594=CARTESIAN_POINT('Ctrl Pts',(-7.27501128491269,1.59120881936851,
-0.18236146569843));
#135595=CARTESIAN_POINT('Ctrl Pts',(-7.24771725040738,1.58673401593797,
-0.18191938037661));
#135596=CARTESIAN_POINT('Ctrl Pts',(-7.487149489,1.585967065,-0.438853645));
#135597=CARTESIAN_POINT('Ctrl Pts',(-7.491101045,1.59657582,-0.37143735));
#135598=CARTESIAN_POINT('Ctrl Pts',(-7.49383799,1.607142857,-0.303960829));
#135599=CARTESIAN_POINT('Ctrl Pts',(-7.507732102,1.660786473,0.038584051));
#135600=CARTESIAN_POINT('Ctrl Pts',(-7.49031797500001,1.715323387,0.38096803));
#135601=CARTESIAN_POINT('Ctrl Pts',(-7.49010875149683,1.71597862537053,
0.385081631303059));
#135602=CARTESIAN_POINT('Ctrl Pts',(-7.48989952799365,1.71663386374106,
0.389195232606118));
#135603=CARTESIAN_POINT('Ctrl Pts',(-7.247597285,1.585967065,-0.186637596));
#135604=CARTESIAN_POINT('Ctrl Pts',(-7.24927782,1.59657582,-0.121378293));
#135605=CARTESIAN_POINT('Ctrl Pts',(-7.249782953,1.607142857,-0.056099309));
#135606=CARTESIAN_POINT('Ctrl Pts',(-7.252347264,1.660786473,0.275289765));
#135607=CARTESIAN_POINT('Ctrl Pts',(-7.224668324,1.715323387,0.605530844));
#135608=CARTESIAN_POINT('Ctrl Pts',(-7.22433577303198,1.71597862537053,
0.609498553402951));
#135609=CARTESIAN_POINT('Ctrl Pts',(-7.22400322206396,1.71663386374106,
0.613466262805901));
#135610=CARTESIAN_POINT('Ctrl Pts',(-7.2246683254307,1.71532338418104,0.605530826930147));
#135611=CARTESIAN_POINT('Ctrl Pts',(-7.23710190400368,1.69082501017366,
0.457184159018169));
#135612=CARTESIAN_POINT('Ctrl Pts',(-7.24493660034943,1.66647816530689,
0.308759694131952));
#135613=CARTESIAN_POINT('Ctrl Pts',(-7.24821926433237,1.64234941111953,
0.160678235119607));
#135614=CARTESIAN_POINT('Ctrl Pts',(-7.24982326999497,1.63055939589135,
0.0883213018436355));
#135615=CARTESIAN_POINT('Ctrl Pts',(-7.25034121939894,1.6188214008152,0.016046122256376));
#135616=CARTESIAN_POINT('Ctrl Pts',(-7.24978295328257,1.60714285707412,
-0.0560993088255138));
#135617=CARTESIAN_POINT('Ctrl Pts',(-7.24945868958999,1.60035948119099,
-0.0980043278327279));
#135618=CARTESIAN_POINT('Ctrl Pts',(-7.24877075450675,1.59355605165188,
-0.139947483342351));
#135619=CARTESIAN_POINT('Ctrl Pts',(-7.24771725015678,1.58673401461714,
-0.181919377103323));
#135620=CARTESIAN_POINT('Ctrl Pts',(-7.45017314305326,1.71660033198358,
0.863125660047407));
#135621=CARTESIAN_POINT('Ctrl Pts',(-7.44970214052664,1.71596185949179,
0.867153076523704));
#135622=CARTESIAN_POINT('Ctrl Pts',(-7.449231138,1.715323387,0.871180493));
#135623=CARTESIAN_POINT('Ctrl Pts',(-7.401880561,1.651136808,1.276062597));
#135624=CARTESIAN_POINT('Ctrl Pts',(-7.31092609300001,1.585954698,1.673427518));
#135625=CARTESIAN_POINT('Ctrl Pts',(-7.22532308280471,1.71660033198358,
0.597718829193276));
#135626=CARTESIAN_POINT('Ctrl Pts',(-7.22499570340235,1.71596185949179,
0.601624836096638));
#135627=CARTESIAN_POINT('Ctrl Pts',(-7.224668324,1.715323387,0.605530843000001));
#135628=CARTESIAN_POINT('Ctrl Pts',(-7.191756391,1.651136808,0.998207464));
#135629=CARTESIAN_POINT('Ctrl Pts',(-7.116478391,1.585954698,1.385003724));
#135630=CARTESIAN_POINT('',(-7.11737693714463,1.58673401526929,1.38037876528236));
#135631=CARTESIAN_POINT('Origin',(0.18620950884611,1.48222902396052,-0.0537970276721317));
#135632=CARTESIAN_POINT('Ctrl Pts',(-7.36237804982027,1.62564958676894,
1.43017112466105));
#135633=CARTESIAN_POINT('Ctrl Pts',(-7.33423879050121,1.62139779885538,
1.42450272340483));
#135634=CARTESIAN_POINT('Ctrl Pts',(-7.3061141840004,1.61707840869336,1.41881176988085));
#135635=CARTESIAN_POINT('Ctrl Pts',(-7.2780056582292,1.6126879253501,1.41309678996554));
#135636=CARTESIAN_POINT('Ctrl Pts',(-7.25121113052638,1.60850268530843,
1.40764897000841));
#135637=CARTESIAN_POINT('Ctrl Pts',(-7.22443210526534,1.60425381500575,
1.40217328992506));
#135638=CARTESIAN_POINT('Ctrl Pts',(-7.1976612912563,1.59993003802629,1.39671709932095));
#135639=CARTESIAN_POINT('Ctrl Pts',(-7.17088973547085,1.59560614124188,
1.39126075753453));
#135640=CARTESIAN_POINT('Ctrl Pts',(-7.14412788854287,1.59120881940184,
1.38581442237808));
#135641=CARTESIAN_POINT('Ctrl Pts',(-7.11737693823206,1.58673401602446,
1.38037876113075));
#135642=CARTESIAN_POINT('Ctrl Pts',(-7.406444656,1.585967065,1.180922331));
#135643=CARTESIAN_POINT('Ctrl Pts',(-7.395811316,1.59657582,1.247611939));
#135644=CARTESIAN_POINT('Ctrl Pts',(-7.383978815,1.607142857,1.314099258));
#135645=CARTESIAN_POINT('Ctrl Pts',(-7.323911067,1.660786473,1.651622452));
#135646=CARTESIAN_POINT('Ctrl Pts',(-7.233301638,1.715323387,1.982258161));
#135647=CARTESIAN_POINT('Ctrl Pts',(-7.23221300334376,1.71597862537067,
1.98623061171932));
#135648=CARTESIAN_POINT('Ctrl Pts',(-7.23112436868752,1.71663386374133,
1.99020306243864));
#135649=CARTESIAN_POINT('Ctrl Pts',(-7.118274054,1.585967065,1.375745066));
#135650=CARTESIAN_POINT('Ctrl Pts',(-7.105886478,1.59657582,1.439839908));
#135651=CARTESIAN_POINT('Ctrl Pts',(-7.09234675,1.607142857,1.503701295));
#135652=CARTESIAN_POINT('Ctrl Pts',(-7.02361225300001,1.660786473,1.827893927));
#135653=CARTESIAN_POINT('Ctrl Pts',(-6.925588362,1.715323387,2.144463998));
#135654=CARTESIAN_POINT('Ctrl Pts',(-6.9244106456623,1.71597862537067,2.14826745592069));
#135655=CARTESIAN_POINT('Ctrl Pts',(-6.92323292932461,1.71663386374133,
2.15207091384138));
#135656=CARTESIAN_POINT('Ctrl Pts',(-6.92558836451754,1.71532338603359,
2.14446399142624));
#135657=CARTESIAN_POINT('Ctrl Pts',(-6.96962140931418,1.69082500736844,
2.00225841314585));
#135658=CARTESIAN_POINT('Ctrl Pts',(-7.00917981241695,1.66647815876397,
1.85898823668409));
#135659=CARTESIAN_POINT('Ctrl Pts',(-7.04421886888584,1.64234940171621,
1.71507449825301));
#135660=CARTESIAN_POINT('Ctrl Pts',(-7.06133997073513,1.63055938941156,
1.64475406096102));
#135661=CARTESIAN_POINT('Ctrl Pts',(-7.07738283337217,1.6188213974299,1.57427999703851));
#135662=CARTESIAN_POINT('Ctrl Pts',(-7.09234675007792,1.60714285693919,
1.50370129463249));
#135663=CARTESIAN_POINT('Ctrl Pts',(-7.10103840820445,1.60035948078227,
1.46270628192017));
#135664=CARTESIAN_POINT('Ctrl Pts',(-7.10938309562888,1.59355605118676,
1.42159584729182));
#135665=CARTESIAN_POINT('Ctrl Pts',(-7.117376937,1.586734015,1.380378766));
#135666=CARTESIAN_POINT('Ctrl Pts',(-7.09044573248517,1.71660033198358,
2.44451326180714));
#135667=CARTESIAN_POINT('Ctrl Pts',(-7.08911996624259,1.71596185949179,
2.44834526790357));
#135668=CARTESIAN_POINT('Ctrl Pts',(-7.0877942,1.715323387,2.452177274));
#135669=CARTESIAN_POINT('Ctrl Pts',(-6.954512969,1.651136808,2.837414485));
#135670=CARTESIAN_POINT('Ctrl Pts',(-6.780263254,1.585954698,3.205936713));
#135671=CARTESIAN_POINT('Ctrl Pts',(-6.92790716496715,1.71660033198358,
2.13697537852514));
#135672=CARTESIAN_POINT('Ctrl Pts',(-6.92674776348357,1.71596185949179,
2.14071968826257));
#135673=CARTESIAN_POINT('Ctrl Pts',(-6.92558836200001,1.715323387,2.144463998));
#135674=CARTESIAN_POINT('Ctrl Pts',(-6.809032025,1.651136808,2.520884965));
#135675=CARTESIAN_POINT('Ctrl Pts',(-6.65236422,1.585954698,2.882455599));
#135676=CARTESIAN_POINT('',(-6.65423598885696,1.58673401523155,2.87813192899063));
#135677=CARTESIAN_POINT('Origin',(0.170291263072342,1.48222902846579,-0.0925688321982565));
#135678=CARTESIAN_POINT('Ctrl Pts',(-6.88280522651745,1.62564958674772,
2.97942816881734));
#135679=CARTESIAN_POINT('Ctrl Pts',(-6.85654238608057,1.62139779883964,
2.9678431826258));
#135680=CARTESIAN_POINT('Ctrl Pts',(-6.83029870404631,1.61707840869647,
2.95623932143671));
#135681=CARTESIAN_POINT('Ctrl Pts',(-6.80407589172505,1.61268792537165,
2.94461545246392));
#135682=CARTESIAN_POINT('Ctrl Pts',(-6.77907892536435,1.60850268533586,
2.93353496810799));
#135683=CARTESIAN_POINT('Ctrl Pts',(-6.75410308807487,1.60425381503204,
2.92243060758177));
#135684=CARTESIAN_POINT('Ctrl Pts',(-6.72913108036632,1.59993003804053,
2.91134704614054));
#135685=CARTESIAN_POINT('Ctrl Pts',(-6.70415838072451,1.59560614124426,
2.90026317759203));
#135686=CARTESIAN_POINT('Ctrl Pts',(-6.67919301180922,1.59120881939051,
2.88919116886698));
#135687=CARTESIAN_POINT('Ctrl Pts',(-6.6542359904442,1.58673401620649,2.87813192527157));
#135688=CARTESIAN_POINT('Ctrl Pts',(-6.979422703,1.585967065,2.745479691));
#135689=CARTESIAN_POINT('Ctrl Pts',(-6.95470167,1.59657582,2.808324279));
#135690=CARTESIAN_POINT('Ctrl Pts',(-6.928852998,1.607142857,2.870713524));
#135691=CARTESIAN_POINT('Ctrl Pts',(-6.797632091,1.660786473,3.187432823));
#135692=CARTESIAN_POINT('Ctrl Pts',(-6.638064156,1.715323387,3.490860104));
#135693=CARTESIAN_POINT('Ctrl Pts',(-6.63614701353499,1.71597862537066,
3.49450565675749));
#135694=CARTESIAN_POINT('Ctrl Pts',(-6.63422987106999,1.71663386374133,
3.49815120951497));
#135695=CARTESIAN_POINT('Ctrl Pts',(-6.65610824,1.585967065,2.873799418));
#135696=CARTESIAN_POINT('Ctrl Pts',(-6.630231782,1.59657582,2.933732796));
#135697=CARTESIAN_POINT('Ctrl Pts',(-6.603280295,1.607142857,2.993190497));
#135698=CARTESIAN_POINT('Ctrl Pts',(-6.46646094,1.660786473,3.2950278));
#135699=CARTESIAN_POINT('Ctrl Pts',(-6.30267558499999,1.715323387,3.583124401));
#135700=CARTESIAN_POINT('Ctrl Pts',(-6.30070777198533,1.71597862537066,
3.58658576200464));
#135701=CARTESIAN_POINT('Ctrl Pts',(-6.29873995897067,1.71663386374133,
3.59004712300929));
#135702=CARTESIAN_POINT('Ctrl Pts',(-6.3026755931018,1.71532338430228,3.58312438674902));
#135703=CARTESIAN_POINT('Ctrl Pts',(-6.37624917261175,1.69082500352122,
3.45370928555288));
#135704=CARTESIAN_POINT('Ctrl Pts',(-6.44568158368489,1.66647815192422,
3.32229255612157));
#135705=CARTESIAN_POINT('Ctrl Pts',(-6.51083865543083,1.64234939105966,
3.18927578061367));
#135706=CARTESIAN_POINT('Ctrl Pts',(-6.54267628004166,1.63055938254416,
3.1242799474357));
#135707=CARTESIAN_POINT('Ctrl Pts',(-6.57349390040191,1.6188213941053,3.05890228911775));
#135708=CARTESIAN_POINT('Ctrl Pts',(-6.60328029523312,1.6071428569086,2.9931904964857));
#135709=CARTESIAN_POINT('Ctrl Pts',(-6.62058146193252,1.60035948096017,
2.95502237623406));
#135710=CARTESIAN_POINT('Ctrl Pts',(-6.63756858308226,1.59355605142897,
2.91666694263408));
#135711=CARTESIAN_POINT('Ctrl Pts',(-6.65423598891596,1.58673401453857,
2.87813192913883));
#135712=CARTESIAN_POINT('Ctrl Pts',(-6.39917695920962,1.71660033198358,
3.91159814126253));
#135713=CARTESIAN_POINT('Ctrl Pts',(-6.39705842060482,1.71596185949179,
3.91505555663127));
#135714=CARTESIAN_POINT('Ctrl Pts',(-6.394939882,1.715323387,3.918512972));
#135715=CARTESIAN_POINT('Ctrl Pts',(-6.181960079,1.651136808,4.266092026));
#135716=CARTESIAN_POINT('Ctrl Pts',(-5.93256284,1.585954698,4.588539871));
#135717=CARTESIAN_POINT('Ctrl Pts',(-6.30655000747555,1.71660033198358,
3.57630933537954));
#135718=CARTESIAN_POINT('Ctrl Pts',(-6.30461279623777,1.71596185949179,
3.57971686818977));
#135719=CARTESIAN_POINT('Ctrl Pts',(-6.302675585,1.715323387,3.583124401));
#135720=CARTESIAN_POINT('Ctrl Pts',(-6.107924889,1.651136808,3.925688688));
#135721=CARTESIAN_POINT('Ctrl Pts',(-5.87719289300001,1.585954698,4.245127054));
#135722=CARTESIAN_POINT('',(-5.87995036171793,1.58673401520821,4.24130684438252));
#135723=CARTESIAN_POINT('Origin',(0.146410562493575,1.48222898979575,-0.127012328747914));
#135724=CARTESIAN_POINT('Ctrl Pts',(-6.08140007972267,1.62564958678031,
4.38937046350252));
#135725=CARTESIAN_POINT('Ctrl Pts',(-6.05824167964871,1.62139779889533,
4.37241059342073));
#135726=CARTESIAN_POINT('Ctrl Pts',(-6.03510604752352,1.61707840874886,
4.35543640811371));
#135727=CARTESIAN_POINT('Ctrl Pts',(-6.01199509829649,1.61268792542109,
4.33844716915636));
#135728=CARTESIAN_POINT('Ctrl Pts',(-5.98996452384715,1.60850268539175,
4.3222521314705));
#135729=CARTESIAN_POINT('Ctrl Pts',(-5.96795971712767,1.60425381508137,
4.30603831801684));
#135730=CARTESIAN_POINT('Ctrl Pts',(-5.94595417929556,1.59993003808504,
4.28984564058481));
#135731=CARTESIAN_POINT('Ctrl Pts',(-5.92394803172507,1.59560614128375,
4.27365251447949));
#135732=CARTESIAN_POINT('Ctrl Pts',(-5.90194649400798,1.59120881942668,
4.25747254677786));
#135733=CARTESIAN_POINT('Ctrl Pts',(-5.87995036393212,1.58673401603956,
4.24130684150147));
#135734=CARTESIAN_POINT('Ctrl Pts',(-6.22605070100001,1.585967065,4.181661472));
#135735=CARTESIAN_POINT('Ctrl Pts',(-6.188397903,1.59657582,4.237722498));
#135736=CARTESIAN_POINT('Ctrl Pts',(-6.149741715,1.607142857,4.293096416));
#135737=CARTESIAN_POINT('Ctrl Pts',(-5.953503393,1.660786473,4.574202378));
#135738=CARTESIAN_POINT('Ctrl Pts',(-5.73243817100001,1.715323387,4.836233308));
#135739=CARTESIAN_POINT('Ctrl Pts',(-5.72978216417361,1.71597862537067,
4.83938150079355));
#135740=CARTESIAN_POINT('Ctrl Pts',(-5.72712615734723,1.71663386374133,
4.84252969358709));
#135741=CARTESIAN_POINT('Ctrl Pts',(-5.88271020300001,1.585967065,4.237478103));
#135742=CARTESIAN_POINT('Ctrl Pts',(-5.844554817,1.59657582,4.290447598));
#135743=CARTESIAN_POINT('Ctrl Pts',(-5.805451792,1.607142857,4.342721438));
#135744=CARTESIAN_POINT('Ctrl Pts',(-5.6069451,1.660786473,4.608089836));
#135745=CARTESIAN_POINT('Ctrl Pts',(-5.385056702,1.715323387,4.854241888));
#135746=CARTESIAN_POINT('Ctrl Pts',(-5.38239080505587,1.71597862537067,
4.85719930266941));
#135747=CARTESIAN_POINT('Ctrl Pts',(-5.37972490811174,1.71663386374133,
4.86015671733883));
#135748=CARTESIAN_POINT('Ctrl Pts',(-5.38505671266411,1.71532338437892,
4.85424187616975));
#135749=CARTESIAN_POINT('Ctrl Pts',(-5.48473056372628,1.69082501355794,
4.74366861817509));
#135750=CARTESIAN_POINT('Ctrl Pts',(-5.58079035829832,1.66647817182258,
4.63025030234907));
#135751=CARTESIAN_POINT('Ctrl Pts',(-5.67301873404316,1.64234942068528,
4.51435027910742));
#135752=CARTESIAN_POINT('Ctrl Pts',(-5.71808423471452,1.63055940224687,
4.45771811429886));
#135753=CARTESIAN_POINT('Ctrl Pts',(-5.76223565778625,1.61882140398259,
4.40049377946256));
#135754=CARTESIAN_POINT('Ctrl Pts',(-5.80545179213163,1.60714285708149,
4.34272143834067));
#135755=CARTESIAN_POINT('Ctrl Pts',(-5.83055348496221,1.60035948120359,
4.3091649072749));
#135756=CARTESIAN_POINT('Ctrl Pts',(-5.85538874093021,1.59355605170177,
4.27535793163229));
#135757=CARTESIAN_POINT('Ctrl Pts',(-5.87995036172034,1.58673401468259,
4.24130684448956));
#135758=CARTESIAN_POINT('Ctrl Pts',(-5.40868978391049,1.71660033198358,
5.19578103749289));
#135759=CARTESIAN_POINT('Ctrl Pts',(-5.40587753345524,1.71596185949179,
5.19870219724644));
#135760=CARTESIAN_POINT('Ctrl Pts',(-5.40306528300001,1.715323387,5.201623357));
#135761=CARTESIAN_POINT('Ctrl Pts',(-5.120345607,1.651136808,5.495291845));
#135762=CARTESIAN_POINT('Ctrl Pts',(-4.807462382,1.585954698,5.756588004));
#135763=CARTESIAN_POINT('Ctrl Pts',(-5.39030558027708,1.71660033198358,
4.84841904112145));
#135764=CARTESIAN_POINT('Ctrl Pts',(-5.38768114113854,1.71596185949179,
4.85133046456072));
#135765=CARTESIAN_POINT('Ctrl Pts',(-5.385056702,1.715323387,4.854241888));
#135766=CARTESIAN_POINT('Ctrl Pts',(-5.121217974,1.651136808,5.14693157));
#135767=CARTESIAN_POINT('Ctrl Pts',(-4.827210557,1.585954698,5.409301086));
#135768=CARTESIAN_POINT('',(-4.83072478968181,1.58673401528728,5.40616296532268));
#135769=CARTESIAN_POINT('Origin',(0.115683554224224,1.48222901566629,-0.155516667237091));
#135770=CARTESIAN_POINT('Ctrl Pts',(-4.99563542474065,1.62564958676171,
5.59407067341435));
#135771=CARTESIAN_POINT('Ctrl Pts',(-4.9766643259881,1.62139779890127,5.57252894419362));
#135772=CARTESIAN_POINT('Ctrl Pts',(-4.95771854011771,1.61707840875737,
5.55097812899299));
#135773=CARTESIAN_POINT('Ctrl Pts',(-4.93880009614803,1.61268792543274,
5.52941791819071));
#135774=CARTESIAN_POINT('Ctrl Pts',(-4.92076603853601,1.60850268539144,
5.50886558923814));
#135775=CARTESIAN_POINT('Ctrl Pts',(-4.90276118250712,1.60425381508363,
5.4883004627315));
#135776=CARTESIAN_POINT('Ctrl Pts',(-4.88475106888786,1.59993003810558,
5.46775582088404));
#135777=CARTESIAN_POINT('Ctrl Pts',(-4.86674045623727,1.59560614132261,
5.44721060977753));
#135778=CARTESIAN_POINT('Ctrl Pts',(-4.84873151701052,1.59120881949219,
5.42667924040514));
#135779=CARTESIAN_POINT('Ctrl Pts',(-4.83072479286547,1.58673401610626,
5.4061629624154));
#135780=CARTESIAN_POINT('Ctrl Pts',(-5.181555488,1.585967065,5.422313411));
#135781=CARTESIAN_POINT('Ctrl Pts',(-5.13273152800001,1.59657582,5.468969522));
#135782=CARTESIAN_POINT('Ctrl Pts',(-5.083075345,1.607142857,5.514738891));
#135783=CARTESIAN_POINT('Ctrl Pts',(-4.830995493,1.660786473,5.747087313));
#135784=CARTESIAN_POINT('Ctrl Pts',(-4.558769749,1.715323387,5.955469618));
#135785=CARTESIAN_POINT('Ctrl Pts',(-4.5554990697505,1.71597862537066,5.95797324484628));
#135786=CARTESIAN_POINT('Ctrl Pts',(-4.552228390501,1.71663386374133,5.96047687169255));
#135787=CARTESIAN_POINT('Ctrl Pts',(-4.834243174,1.585967065,5.403017021));
#135788=CARTESIAN_POINT('Ctrl Pts',(-4.785592964,1.59657582,5.446545839));
#135789=CARTESIAN_POINT('Ctrl Pts',(-4.736166816,1.607142857,5.489191552));
#135790=CARTESIAN_POINT('Ctrl Pts',(-4.485254739,1.660786473,5.705682713));
#135791=CARTESIAN_POINT('Ctrl Pts',(-4.215638554,1.715323387,5.898380421));
#135792=CARTESIAN_POINT('Ctrl Pts',(-4.21239922751805,1.71597862537066,
5.90069560392768));
#135793=CARTESIAN_POINT('Ctrl Pts',(-4.20915990103609,1.71663386374133,
5.90301078685534));
#135794=CARTESIAN_POINT('Ctrl Pts',(-4.21563855917688,1.71532338609041,
5.89838041591));
#135795=CARTESIAN_POINT('Ctrl Pts',(-4.33675209913449,1.69082500967298,
5.81181921265613));
#135796=CARTESIAN_POINT('Ctrl Pts',(-4.45494767587929,1.66647816324636,
5.7217025528292));
#135797=CARTESIAN_POINT('Ctrl Pts',(-4.56993489988004,1.6423494082958,5.62833856611449));
#135798=CARTESIAN_POINT('Ctrl Pts',(-4.62612101649552,1.63055939378575,
5.58271819488782));
#135799=CARTESIAN_POINT('Ctrl Pts',(-4.68154172496527,1.61882139960798,
5.53632299966429));
#135800=CARTESIAN_POINT('Ctrl Pts',(-4.73616681628953,1.60714285693547,
5.48919155190664));
#135801=CARTESIAN_POINT('Ctrl Pts',(-4.7678953096723,1.60035948077783,5.46181567431286));
#135802=CARTESIAN_POINT('Ctrl Pts',(-4.79941743244761,1.59355605119151,
5.43413793201519));
#135803=CARTESIAN_POINT('Ctrl Pts',(-4.830724789,1.586734015,5.406162966));
#135804=CARTESIAN_POINT('Ctrl Pts',(-4.16529828519659,1.71660033198358,
6.23701498812772));
#135805=CARTESIAN_POINT('Ctrl Pts',(-4.16192382059829,1.71596185949179,
6.23926330206386));
#135806=CARTESIAN_POINT('Ctrl Pts',(-4.158549356,1.715323387,6.241511616));
#135807=CARTESIAN_POINT('Ctrl Pts',(-3.819309465,1.651136808,6.467537924));
#135808=CARTESIAN_POINT('Ctrl Pts',(-3.457570326,1.585954698,6.65546448));
#135809=CARTESIAN_POINT('Ctrl Pts',(-4.22201645637774,1.71660033198358,
5.893822062747));
#135810=CARTESIAN_POINT('Ctrl Pts',(-4.21882750518887,1.71596185949179,
5.8961012418735));
#135811=CARTESIAN_POINT('Ctrl Pts',(-4.215638554,1.715323387,5.898380421));
#135812=CARTESIAN_POINT('Ctrl Pts',(-3.895048599,1.651136808,6.127509652));
#135813=CARTESIAN_POINT('Ctrl Pts',(-3.551513221,1.585954698,6.320542211));
#135814=CARTESIAN_POINT('',(-3.55561989738265,1.58673401525583,6.3182329131868));
#135815=CARTESIAN_POINT('Origin',(0.0795475509393828,1.48222904884081,-0.17674948871494));
#135816=CARTESIAN_POINT('Ctrl Pts',(-3.67628040946491,1.62564958677506,
6.53719835604483));
#135817=CARTESIAN_POINT('Ctrl Pts',(-3.66238367936959,1.62139779888063,
6.51208203505397));
#135818=CARTESIAN_POINT('Ctrl Pts',(-3.64851362369125,1.61707840872687,
6.48696228194679));
#135819=CARTESIAN_POINT('Ctrl Pts',(-3.6346722904589,1.61268792539826,6.46183923059958));
#135820=CARTESIAN_POINT('Ctrl Pts',(-3.62147800234549,1.60850268536232,
6.43789061436456));
#135821=CARTESIAN_POINT('Ctrl Pts',(-3.60831498411565,1.60425381504979,
6.4139357772996));
#135822=CARTESIAN_POINT('Ctrl Pts',(-3.59514242756208,1.59993003806146,
6.38999981577955));
#135823=CARTESIAN_POINT('Ctrl Pts',(-3.58196950601816,1.59560614126824,
6.36606319103251));
#135824=CARTESIAN_POINT('Ctrl Pts',(-3.56879524322245,1.59120881943395,
6.34214044413688));
#135825=CARTESIAN_POINT('Ctrl Pts',(-3.55561990060144,1.58673401625832,
6.31823291137706));
#135826=CARTESIAN_POINT('Ctrl Pts',(-3.894776499,1.585967065,6.409424001));
#135827=CARTESIAN_POINT('Ctrl Pts',(-3.837064332,1.59657582,6.44449361));
#135828=CARTESIAN_POINT('Ctrl Pts',(-3.778730021,1.607142857,6.478518305));
#135829=CARTESIAN_POINT('Ctrl Pts',(-3.482595614,1.660786473,6.651244833));
#135830=CARTESIAN_POINT('Ctrl Pts',(-3.17193832,1.715323387,6.796234788));
#135831=CARTESIAN_POINT('Ctrl Pts',(-3.16820590163919,1.71597862537067,
6.79797678209004));
#135832=CARTESIAN_POINT('Ctrl Pts',(-3.16447348327838,1.71663386374133,
6.79971877618008));
#135833=CARTESIAN_POINT('Ctrl Pts',(-3.559732308,1.585967065,6.315916869));
#135834=CARTESIAN_POINT('Ctrl Pts',(-3.502862104,1.59657582,6.347969651));
#135835=CARTESIAN_POINT('Ctrl Pts',(-3.445423944,1.607142857,6.378993169));
#135836=CARTESIAN_POINT('Ctrl Pts',(-3.153838851,1.660786473,6.536484208));
#135837=CARTESIAN_POINT('Ctrl Pts',(-2.849101831,1.715323387,6.66671724));
#135838=CARTESIAN_POINT('Ctrl Pts',(-2.8454405422724,1.71597862537067,6.66828193578925));
#135839=CARTESIAN_POINT('Ctrl Pts',(-2.84177925354481,1.71663386374133,
6.6698466315785));
#135840=CARTESIAN_POINT('Ctrl Pts',(-2.84910184639505,1.71532338424484,
6.66671723342074));
#135841=CARTESIAN_POINT('Ctrl Pts',(-2.98599189749724,1.69082501201072,
6.60821562268897));
#135842=CARTESIAN_POINT('Ctrl Pts',(-3.1207965283895,1.66647816885366,6.54561440386231));
#135843=CARTESIAN_POINT('Ctrl Pts',(-3.25316589951571,1.64234941630276,
6.47915207685954));
#135844=CARTESIAN_POINT('Ctrl Pts',(-3.31784546089788,1.63055939933424,
6.44667663240888));
#135845=CARTESIAN_POINT('Ctrl Pts',(-3.38194407384616,1.61882140252272,
6.41327993798857));
#135846=CARTESIAN_POINT('Ctrl Pts',(-3.44542394381593,1.60714285705506,
6.37899316919607));
#135847=CARTESIAN_POINT('Ctrl Pts',(-3.48229564501008,1.6003594811509,6.35907801375703));
#135848=CARTESIAN_POINT('Ctrl Pts',(-3.51903069410623,1.59355605158396,
6.33882368660111));
#135849=CARTESIAN_POINT('Ctrl Pts',(-3.55561989734046,1.58673401463352,
6.31823291331802));
#135850=CARTESIAN_POINT('Ctrl Pts',(-2.72714206803972,1.71660033198358,
6.98661305006529));
#135851=CARTESIAN_POINT('Ctrl Pts',(-2.72336317551986,1.71596185949179,
6.98808338953265));
#135852=CARTESIAN_POINT('Ctrl Pts',(-2.719584283,1.715323387,6.989553729));
#135853=CARTESIAN_POINT('Ctrl Pts',(-2.339686658,1.651136808,7.137369119));
#135854=CARTESIAN_POINT('Ctrl Pts',(-1.946006124,1.585954698,7.243138834));
#135855=CARTESIAN_POINT('Ctrl Pts',(-2.85631053383156,1.71660033198358,
6.66363651409478));
#135856=CARTESIAN_POINT('Ctrl Pts',(-2.85270618241578,1.71596185949179,
6.66517687704739));
#135857=CARTESIAN_POINT('Ctrl Pts',(-2.849101831,1.715323387,6.66671724));
#135858=CARTESIAN_POINT('Ctrl Pts',(-2.48675108,1.651136808,6.821572194));
#135859=CARTESIAN_POINT('Ctrl Pts',(-2.109751075,1.585954698,6.936241807));
#135860=CARTESIAN_POINT('',(-2.11425816856513,1.5867340151998,6.93486931357578));
#135861=CARTESIAN_POINT('Origin',(0.0396917784304465,1.48222903682356,-0.189717322672631));
#135862=CARTESIAN_POINT('Ctrl Pts',(-2.18502660812398,1.62564958673401,
7.17465390925617));
#135863=CARTESIAN_POINT('Ctrl Pts',(-2.17685404271359,1.62139779888482,
7.14713740763033));
#135864=CARTESIAN_POINT('Ctrl Pts',(-2.16870826565351,1.61707840873381,
7.11962328841482));
#135865=CARTESIAN_POINT('Ctrl Pts',(-2.160591248555,1.61268792540409,7.09211212254638));
#135866=CARTESIAN_POINT('Ctrl Pts',(-2.15285368017845,1.60850268536363,
7.06588702970223));
#135867=CARTESIAN_POINT('Ctrl Pts',(-2.14514798794446,1.6042538150484,7.03966258355752));
#135868=CARTESIAN_POINT('Ctrl Pts',(-2.1374289226582,1.59993003804401,7.01345452121582));
#135869=CARTESIAN_POINT('Ctrl Pts',(-2.12970964348897,1.59560614123467,
6.9872457326906));
#135870=CARTESIAN_POINT('Ctrl Pts',(-2.12198607104548,1.59120881937031,
6.96105020924954));
#135871=CARTESIAN_POINT('Ctrl Pts',(-2.11425817195538,1.58673401592903,
6.9348693128284));
#135872=CARTESIAN_POINT('Ctrl Pts',(-2.42588209,1.585967065,7.096837048));
#135873=CARTESIAN_POINT('Ctrl Pts',(-2.361980272,1.59657582,7.118680339));
#135874=CARTESIAN_POINT('Ctrl Pts',(-2.297695481,1.607142857,7.139369403));
#135875=CARTESIAN_POINT('Ctrl Pts',(-1.971353434,1.660786473,7.244397537));
#135876=CARTESIAN_POINT('Ctrl Pts',(-1.636790581,1.715323387,7.319215572));
#135877=CARTESIAN_POINT('Ctrl Pts',(-1.6327709472766,1.71597862537066,7.32011447961603));
#135878=CARTESIAN_POINT('Ctrl Pts',(-1.6287513135532,1.71663386374133,7.32101338723207));
#135879=CARTESIAN_POINT('Ctrl Pts',(-2.118772315,1.585967065,6.933491464));
#135880=CARTESIAN_POINT('Ctrl Pts',(-2.056341304,1.59657582,6.952569456));
#135881=CARTESIAN_POINT('Ctrl Pts',(-1.993576877,1.607142857,6.970520155));
#135882=CARTESIAN_POINT('Ctrl Pts',(-1.674952964,1.660786473,7.061646965));
#135883=CARTESIAN_POINT('Ctrl Pts',(-1.349344274,1.715323387,7.12332577));
#135884=CARTESIAN_POINT('Ctrl Pts',(-1.34543222082607,1.71597862537066,
7.12406681522476));
#135885=CARTESIAN_POINT('Ctrl Pts',(-1.34152016765215,1.71663386374133,
7.12480786044952));
#135886=CARTESIAN_POINT('Ctrl Pts',(-1.34934428967406,1.71532338437472,
7.12332576703092));
#135887=CARTESIAN_POINT('Ctrl Pts',(-1.49561004609945,1.69082501186417,
7.09561920558352));
#135888=CARTESIAN_POINT('Ctrl Pts',(-1.64072043248348,1.66647816847583,
7.06346057892067));
#135889=CARTESIAN_POINT('Ctrl Pts',(-1.78428251795239,1.64234941574856,
7.02700760592775));
#135890=CARTESIAN_POINT('Ctrl Pts',(-1.85443116652592,1.63055939897599,
7.00919561341184));
#135891=CARTESIAN_POINT('Ctrl Pts',(-1.92421049037672,1.618821402371,6.99035902258183));
#135892=CARTESIAN_POINT('Ctrl Pts',(-1.99357687675647,1.60714285712086,
6.97052015546866));
#135893=CARTESIAN_POINT('Ctrl Pts',(-2.03386770756363,1.60035948126202,
6.95899693115295));
#135894=CARTESIAN_POINT('Ctrl Pts',(-2.07409799246674,1.5935560517563,6.94711308871186));
#135895=CARTESIAN_POINT('Ctrl Pts',(-2.11425816857299,1.58673401473019,
6.93486931386321));
#135896=CARTESIAN_POINT('Ctrl Pts',(-1.16146771926858,1.71660033198358,
7.40952484987453));
#135897=CARTESIAN_POINT('Ctrl Pts',(-1.15746109563429,1.71596185949179,
7.41014846343726));
#135898=CARTESIAN_POINT('Ctrl Pts',(-1.153454472,1.715323387,7.41077207700001));
#135899=CARTESIAN_POINT('Ctrl Pts',(-0.750662703,1.651136808,7.47346486600001));
#135900=CARTESIAN_POINT('Ctrl Pts',(-0.343448839,1.585954698,7.492132066));
#135901=CARTESIAN_POINT('Ctrl Pts',(-1.35704670638058,1.71660033198358,
7.12186672777106));
#135902=CARTESIAN_POINT('Ctrl Pts',(-1.35319549019029,1.71596185949179,
7.12259624888553));
#135903=CARTESIAN_POINT('Ctrl Pts',(-1.349344274,1.715323387,7.12332577000001));
#135904=CARTESIAN_POINT('Ctrl Pts',(-0.962175844,1.651136808,7.196665601));
#135905=CARTESIAN_POINT('Ctrl Pts',(-0.569339312,1.585954698,7.227610445));
#135906=CARTESIAN_POINT('',(-0.574036078793354,1.58673401524049,7.22723893187494));
#135907=CARTESIAN_POINT('Origin',(-0.00201981579105066,1.48222903402286,
-0.193814356406586));
#135908=CARTESIAN_POINT('Ctrl Pts',(-0.591603391086984,1.62564958670864,
7.47663061967719));
#135909=CARTESIAN_POINT('Ctrl Pts',(-0.589537129951309,1.62139779883426,
7.44800057857977));
#135910=CARTESIAN_POINT('Ctrl Pts',(-0.587496518870869,1.61707840868329,
7.4193786228778));
#135911=CARTESIAN_POINT('Ctrl Pts',(-0.585483360458298,1.61268792535319,
7.39076573401896));
#135912=CARTESIAN_POINT('Ctrl Pts',(-0.583564311790205,1.60850268531728,
7.36349042080358));
#135913=CARTESIAN_POINT('Ctrl Pts',(-0.581676255042661,1.60425381501644,
7.33622259159249));
#135914=CARTESIAN_POINT('Ctrl Pts',(-0.579771615869591,1.59993003803003,
7.30896788832829));
#135915=CARTESIAN_POINT('Ctrl Pts',(-0.577866923922012,1.59560614123866,
7.28171242987984));
#135916=CARTESIAN_POINT('Ctrl Pts',(-0.575955187441002,1.59120881938927,
7.25446900346002));
#135917=CARTESIAN_POINT('Ctrl Pts',(-0.574036082484844,1.58673401613979,
7.22723893149673));
#135918=CARTESIAN_POINT('Ctrl Pts',(-0.84355613,1.585967065,7.452409882));
#135919=CARTESIAN_POINT('Ctrl Pts',(-0.776452639,1.59657582,7.460005487));
#135920=CARTESIAN_POINT('Ctrl Pts',(-0.709223254,1.607142857,7.466391523));
#135921=CARTESIAN_POINT('Ctrl Pts',(-0.367932958,1.660786473,7.498810264));
#135922=CARTESIAN_POINT('Ctrl Pts',(-0.025108333,1.715323387,7.499957971));
#135923=CARTESIAN_POINT('Ctrl Pts',(-0.0209894375174155,1.71597862537066,
7.49997176022292));
#135924=CARTESIAN_POINT('Ctrl Pts',(-0.016870542034831,1.71663386374133,
7.49998554944585));
#135925=CARTESIAN_POINT('Ctrl Pts',(-0.578740883,1.585967065,7.226863704));
#135926=CARTESIAN_POINT('Ctrl Pts',(-0.51366827,1.59657582,7.232074841));
#135927=CARTESIAN_POINT('Ctrl Pts',(-0.448512371,1.607142857,7.236113367));
#135928=CARTESIAN_POINT('Ctrl Pts',(-0.117748137,1.660786473,7.256614959));
#135929=CARTESIAN_POINT('Ctrl Pts',(0.213507122,1.715323387,7.246855505));
#135930=CARTESIAN_POINT('Ctrl Pts',(0.217487016355248,1.71597862537066,
7.24673824921362));
#135931=CARTESIAN_POINT('Ctrl Pts',(0.221466910710496,1.71663386374133,
7.24662099342725));
#135932=CARTESIAN_POINT('Ctrl Pts',(0.213507114912512,1.71532338597331,
7.2468555060868));
#135933=CARTESIAN_POINT('Ctrl Pts',(0.200619328248611,1.71320157779897,
7.24723520642678));
#135934=CARTESIAN_POINT('Ctrl Pts',(0.196655750649506,1.71254943779287,
7.24733664243004));
#135935=CARTESIAN_POINT('Ctrl Pts',(0.180551941733234,1.70989962927072,
7.24775613221961));
#135936=CARTESIAN_POINT('Ctrl Pts',(0.17231146465773,1.70854407397244,7.24795672696019));
#135937=CARTESIAN_POINT('Ctrl Pts',(0.147595163082729,1.70447938479062,
7.2485162106093));
#135938=CARTESIAN_POINT('Ctrl Pts',(0.131118277380395,1.70177120836391,
7.24883298177625));
#135939=CARTESIAN_POINT('Ctrl Pts',(0.081710543770135,1.69365497342894,
7.24961433639062));
#135940=CARTESIAN_POINT('Ctrl Pts',(0.0487767691046939,1.68825095317067,
7.2499107293857));
#135941=CARTESIAN_POINT('Ctrl Pts',(-0.0499137006149773,1.67207514746497,
7.25012636772878));
#135942=CARTESIAN_POINT('Ctrl Pts',(-0.115671654201335,1.66132115636037,
7.24937548198048));
#135943=CARTESIAN_POINT('Ctrl Pts',(-0.312506753462951,1.62920290478646,
7.24444859976342));
#135944=CARTESIAN_POINT('Ctrl Pts',(-0.443380249615298,1.60803075453319,
7.23761650001668));
#135945=CARTESIAN_POINT('Ctrl Pts',(-0.574036078744983,1.58673401461205,
7.22723893255561));
#135946=CARTESIAN_POINT('Ctrl Pts',(-1.354636469,4.302796438,7.122321253));
#135947=CARTESIAN_POINT('Ctrl Pts',(-0.968989539,4.238074114,7.195669727));
#135948=CARTESIAN_POINT('Ctrl Pts',(-0.577677421000001,4.172899507,7.226948789));
#135949=CARTESIAN_POINT('Ctrl Pts',(-0.564250173365847,4.17066314490592,
7.22802207983848));
#135950=CARTESIAN_POINT('Ctrl Pts',(-0.550822925731692,4.16842678281185,
7.22909537067707));
#135951=CARTESIAN_POINT('Ctrl Pts',(-1.64281292560515,4.302796438,7.31839524783626));
#135952=CARTESIAN_POINT('Ctrl Pts',(-1.24654932631986,4.238074114,7.40734739431102));
#135953=CARTESIAN_POINT('Ctrl Pts',(-0.842997787615108,4.172899507,7.45299255686155));
#135954=CARTESIAN_POINT('Ctrl Pts',(-0.829150563892455,4.17066314490592,
7.45455879739607));
#135955=CARTESIAN_POINT('Ctrl Pts',(-0.815303340169794,4.16842678281185,
7.45612503793064));
#135956=CARTESIAN_POINT('',(-1.35005064870962,4.30202682597625,7.12319192827134));
#135957=CARTESIAN_POINT('Origin',(0.0137705755161144,4.16072147847015,-0.198015518509984));
#135958=CARTESIAN_POINT('Ctrl Pts',(-1.39881673453704,4.26310680820179,
7.36839953710498));
#135959=CARTESIAN_POINT('Ctrl Pts',(-1.39323107349379,4.26736775487504,
7.34024242578059));
#135960=CARTESIAN_POINT('Ctrl Pts',(-1.38763724397555,4.27169422775334,
7.3120967623594));
#135961=CARTESIAN_POINT('Ctrl Pts',(-1.38203469282476,4.27608953503156,
7.28396366972715));
#135962=CARTESIAN_POINT('Ctrl Pts',(-1.37669475276436,4.28027881894546,
7.25714927315551));
#135963=CARTESIAN_POINT('Ctrl Pts',(-1.37133665373562,4.28452899137152,
7.23034791613796));
#135964=CARTESIAN_POINT('Ctrl Pts',(-1.36599630035225,4.2888490835118,7.20355436555762));
#135965=CARTESIAN_POINT('Ctrl Pts',(-1.36065581289424,4.2931692841121,7.17676014229977));
#135966=CARTESIAN_POINT('Ctrl Pts',(-1.35534004338375,4.29756059498722,
7.14997233931333));
#135967=CARTESIAN_POINT('Ctrl Pts',(-1.35005064905555,4.30202682552111,
7.12319192419185));
#135968=CARTESIAN_POINT('Ctrl Pts',(-2.1253965081304,4.17158344184794,6.93146835656078));
#135969=CARTESIAN_POINT('Ctrl Pts',(-2.1215742575652,4.17224147442397,6.93263576478039));
#135970=CARTESIAN_POINT('Ctrl Pts',(-2.117752007,4.172899507,6.933803173));
#135971=CARTESIAN_POINT('Ctrl Pts',(-1.787314404,4.229787119,7.034726848));
#135972=CARTESIAN_POINT('Ctrl Pts',(-1.448776863,4.285714286,7.103769816));
#135973=CARTESIAN_POINT('Ctrl Pts',(-1.397161514,4.294241258,7.114296498));
#135974=CARTESIAN_POINT('Ctrl Pts',(-1.345398651,4.302795611,7.12407204299999));
#135975=CARTESIAN_POINT('Ctrl Pts',(-1.96234429440288,4.17158344184794,
7.23873422950782));
#135976=CARTESIAN_POINT('Ctrl Pts',(-1.95835276320144,4.17224147442397,
7.23981156875392));
#135977=CARTESIAN_POINT('Ctrl Pts',(-1.954361232,4.172899507,7.240888908));
#135978=CARTESIAN_POINT('Ctrl Pts',(-1.609289139,4.229787119,7.334026025));
#135979=CARTESIAN_POINT('Ctrl Pts',(-1.256923902,4.285714286,7.393926041));
#135980=CARTESIAN_POINT('Ctrl Pts',(-1.203200304,4.294241258,7.403058737));
#135981=CARTESIAN_POINT('Ctrl Pts',(-1.14934967,4.302795611,7.411409808));
#135982=CARTESIAN_POINT('Ctrl Pts',(-2.11775200214645,4.17289950776325,
6.93380317514373));
#135983=CARTESIAN_POINT('Ctrl Pts',(-2.10540223265424,4.17502562443694,
6.93757509482064));
#135984=CARTESIAN_POINT('Ctrl Pts',(-2.10156372697733,4.1756853482417,6.9387313149784));
#135985=CARTESIAN_POINT('Ctrl Pts',(-2.08608302136244,4.17834651467031,
6.94340162287339));
#135986=CARTESIAN_POINT('Ctrl Pts',(-2.07815766815513,4.17970788576612,
6.94577779488903));
#135987=CARTESIAN_POINT('Ctrl Pts',(-2.05437518968315,4.18379006162331,
6.95286388617765));
#135988=CARTESIAN_POINT('Ctrl Pts',(-2.03850584321999,4.18650992790924,
6.95753315333298));
#135989=CARTESIAN_POINT('Ctrl Pts',(-1.99087453841738,4.19466138435571,
6.97137084369471));
#135990=CARTESIAN_POINT('Ctrl Pts',(-1.95906505357515,4.20008900935301,
6.98037657298076));
#135991=CARTESIAN_POINT('Ctrl Pts',(-1.86356284657613,4.2163361933017,7.0067103780558));
#135992=CARTESIAN_POINT('Ctrl Pts',(-1.79969087995045,4.22713823017249,
7.0233874035499));
#135993=CARTESIAN_POINT('Ctrl Pts',(-1.6077998448799,4.25939963184753,7.07070041929629));
#135994=CARTESIAN_POINT('Ctrl Pts',(-1.47928066971532,4.28067055419012,
7.0986991046817));
#135995=CARTESIAN_POINT('Ctrl Pts',(-1.3500506490493,4.30202682560965,7.12319193038323));
#135996=CARTESIAN_POINT('Ctrl Pts',(-2.854054357,4.302796438,6.664598542));
#135997=CARTESIAN_POINT('Ctrl Pts',(-2.493191391,4.238074114,6.81913486));
#135998=CARTESIAN_POINT('Ctrl Pts',(-2.117752007,4.172899507,6.933803173));
#135999=CARTESIAN_POINT('Ctrl Pts',(-2.10486940628411,4.17066314482125,
6.93773783237272));
#136000=CARTESIAN_POINT('Ctrl Pts',(-2.09198680556821,4.16842678264244,
6.94167249174543));
#136001=CARTESIAN_POINT('Ctrl Pts',(-3.17764352088934,4.302796438,6.79413901620324));
#136002=CARTESIAN_POINT('Ctrl Pts',(-2.80976642583978,4.238074114,6.96619647104542));
#136003=CARTESIAN_POINT('Ctrl Pts',(-2.42546205857017,4.172899507,7.09752612644045));
#136004=CARTESIAN_POINT('Ctrl Pts',(-2.412275270162,4.17066314482125,7.10203249307303));
#136005=CARTESIAN_POINT('Ctrl Pts',(-2.3990884817538,4.16842678264244,7.10653885970545));
#136006=CARTESIAN_POINT('',(-2.84976291967314,4.30202682599171,6.66643467681058));
#136007=CARTESIAN_POINT('Origin',(0.056016144692978,4.16072142213443,-0.190425882582227));
#136008=CARTESIAN_POINT('Ctrl Pts',(-2.95010126893415,4.26310680820208,
6.8954262016237));
#136009=CARTESIAN_POINT('Ctrl Pts',(-2.93859325105434,4.26736775488116,
6.86912813973383));
#136010=CARTESIAN_POINT('Ctrl Pts',(-2.92707971648568,4.27169422776909,
6.84284301422454));
#136011=CARTESIAN_POINT('Ctrl Pts',(-2.91556036655634,4.27608953505766,
6.81657204049201));
#136012=CARTESIAN_POINT('Ctrl Pts',(-2.90458096871979,4.28027881896961,
6.79153247889068));
#136013=CARTESIAN_POINT('Ctrl Pts',(-2.89358663965223,4.28452899140393,
6.76650955559758));
#136014=CARTESIAN_POINT('Ctrl Pts',(-2.88261131919965,4.2888490834973,6.74149044156445));
#136015=CARTESIAN_POINT('Ctrl Pts',(-2.87163572320134,4.29316928405064,
6.71647069940297));
#136016=CARTESIAN_POINT('Ctrl Pts',(-2.86068564753187,4.29756059489377,
6.69145191373861));
#136017=CARTESIAN_POINT('Ctrl Pts',(-2.84976291926378,4.3020268255214,6.66643467296296));
#136018=CARTESIAN_POINT('Ctrl Pts',(-3.56576672243298,4.17158344184794,
6.31251705551099));
#136019=CARTESIAN_POINT('Ctrl Pts',(-3.56228479221649,4.17224147442397,
6.31447884125549));
#136020=CARTESIAN_POINT('Ctrl Pts',(-3.558802862,4.172899507,6.31644062700001));
#136021=CARTESIAN_POINT('Ctrl Pts',(-3.257786313,4.229787119,6.486039079));
#136022=CARTESIAN_POINT('Ctrl Pts',(-2.94200579,4.285714286,6.626243425));
#136023=CARTESIAN_POINT('Ctrl Pts',(-2.893860104,4.294241258,6.647619773));
#136024=CARTESIAN_POINT('Ctrl Pts',(-2.845408881,4.302795611,6.668294257));
#136025=CARTESIAN_POINT('Ctrl Pts',(-3.47257965967507,4.17158344184794,
6.64765062822451));
#136026=CARTESIAN_POINT('Ctrl Pts',(-3.46891304433754,4.17224147442397,
6.64956084111226));
#136027=CARTESIAN_POINT('Ctrl Pts',(-3.465246429,4.172899507,6.651471054));
#136028=CARTESIAN_POINT('Ctrl Pts',(-3.148263656,4.229787119,6.81661097799999));
#136029=CARTESIAN_POINT('Ctrl Pts',(-2.817013256,4.285714286,6.950858675));
#136030=CARTESIAN_POINT('Ctrl Pts',(-2.766508945,4.294241258,6.971326838));
#136031=CARTESIAN_POINT('Ctrl Pts',(-2.715712542,4.302795611,6.99105896000001));
#136032=CARTESIAN_POINT('Ctrl Pts',(-3.55880256580312,4.17289956297677,
6.31644079388295));
#136033=CARTESIAN_POINT('Ctrl Pts',(-3.42907978966191,4.1974152208008,6.3895290666609));
#136034=CARTESIAN_POINT('Ctrl Pts',(-3.29736278114992,4.22178367600239,
6.45847127992605));
#136035=CARTESIAN_POINT('Ctrl Pts',(-3.16405329923453,4.24593816410288,
6.52313319819443));
#136036=CARTESIAN_POINT('Ctrl Pts',(-3.09049910662304,4.259265527203,6.55881074432697));
#136037=CARTESIAN_POINT('Ctrl Pts',(-3.01646035691276,4.27252780772309,
6.59318611782242));
#136038=CARTESIAN_POINT('Ctrl Pts',(-2.94200579035202,4.28571428590791,
6.62624342520531));
#136039=CARTESIAN_POINT('Ctrl Pts',(-2.91137508270563,4.29113922027103,
6.63984324526649));
#136040=CARTESIAN_POINT('Ctrl Pts',(-2.88062613755849,4.29657697957941,
6.65324128930027));
#136041=CARTESIAN_POINT('Ctrl Pts',(-2.8497629196197,4.30202682581219,6.66643467675972));
#136042=CARTESIAN_POINT('Ctrl Pts',(-4.220019834,4.302796438,5.89524661));
#136043=CARTESIAN_POINT('Ctrl Pts',(-3.900814385,4.238074114,6.123744826));
#136044=CARTESIAN_POINT('Ctrl Pts',(-3.558802862,4.172899507,6.316440627));
#136045=CARTESIAN_POINT('Ctrl Pts',(-3.54706728522262,4.17066314490999,
6.3230526743003));
#136046=CARTESIAN_POINT('Ctrl Pts',(-3.53533170844517,4.16842678281997,
6.32966472160044));
#136047=CARTESIAN_POINT('Ctrl Pts',(-4.5638910363296,4.302796438,5.95219639508923));
#136048=CARTESIAN_POINT('Ctrl Pts',(-4.24160196994199,4.238074114,6.19931394307104));
#136049=CARTESIAN_POINT('Ctrl Pts',(-3.89451441912942,4.172899507,6.41018726365446));
#136050=CARTESIAN_POINT('Ctrl Pts',(-3.88260466660029,4.17066314490999,
6.41742304337996));
#136051=CARTESIAN_POINT('Ctrl Pts',(-3.87069491407125,4.16842678281997,
6.42465882310546));
#136052=CARTESIAN_POINT('',(-4.21622344309948,4.30202682597525,5.89796234949526));
#136053=CARTESIAN_POINT('Origin',(0.0956423205124818,4.16072145579759,-0.173931787777442));
#136054=CARTESIAN_POINT('Ctrl Pts',(-4.36344234639725,4.26310680820233,
6.10003040032616));
#136055=CARTESIAN_POINT('Ctrl Pts',(-4.34655007361737,4.26736775485972,
6.07682105633263));
#136056=CARTESIAN_POINT('Ctrl Pts',(-4.32965519414465,4.27169422775199,
6.05362553204985));
#136057=CARTESIAN_POINT('Ctrl Pts',(-4.31275767749974,4.27608953504627,
6.03044507880318));
#136058=CARTESIAN_POINT('Ctrl Pts',(-4.29665220633118,4.28027881897436,
6.0083511741612));
#136059=CARTESIAN_POINT('Ctrl Pts',(-4.28053572977285,4.28452899142628,
5.98627672859719));
#136060=CARTESIAN_POINT('Ctrl Pts',(-4.26443863631163,4.28884908353792,
5.96420191693393));
#136061=CARTESIAN_POINT('Ctrl Pts',(-4.24834113871776,4.29316928410953,
5.94212655106178));
#136062=CARTESIAN_POINT('Ctrl Pts',(-4.23226877044292,4.29756059497319,
5.92004663319214));
#136063=CARTESIAN_POINT('Ctrl Pts',(-4.21622344160556,4.30202682552111,
5.89796234547385));
#136064=CARTESIAN_POINT('Ctrl Pts',(-4.83940564834472,4.17158344184794,
5.39839947227737));
#136065=CARTESIAN_POINT('Ctrl Pts',(-4.83642684967236,4.17224147442397,
5.40106390463868));
#136066=CARTESIAN_POINT('Ctrl Pts',(-4.83344805100001,4.172899507,5.403728337));
#136067=CARTESIAN_POINT('Ctrl Pts',(-4.575927756,4.229787119,5.634071332));
#136068=CARTESIAN_POINT('Ctrl Pts',(-4.297669796,4.285714286,5.838881257));
#136069=CARTESIAN_POINT('Ctrl Pts',(-4.255245012,4.294241258,5.870107737));
#136070=CARTESIAN_POINT('Ctrl Pts',(-4.212370955,4.302795611,5.900714443));
#136071=CARTESIAN_POINT('Ctrl Pts',(-4.82044105921187,4.17158344184794,
5.74573027284353));
#136072=CARTESIAN_POINT('Ctrl Pts',(-4.81727080660594,4.17224147442397,
5.74838403992177));
#136073=CARTESIAN_POINT('Ctrl Pts',(-4.81410055400001,4.172899507,5.751037807));
#136074=CARTESIAN_POINT('Ctrl Pts',(-4.540028864,4.229787119,5.980458777));
#136075=CARTESIAN_POINT('Ctrl Pts',(-4.2453822,4.285714286,6.182776882));
#136076=CARTESIAN_POINT('Ctrl Pts',(-4.200458702,4.294241258,6.213623445));
#136077=CARTESIAN_POINT('Ctrl Pts',(-4.155091715,4.302795611,6.243813966));
#136078=CARTESIAN_POINT('Ctrl Pts',(-4.83344804756002,4.17289950774314,
5.40372834137236));
#136079=CARTESIAN_POINT('Ctrl Pts',(-4.82382348853918,4.17502562436276,
5.41233717634408));
#136080=CARTESIAN_POINT('Ctrl Pts',(-4.82082523943908,4.17568534815515,
5.41499827998668));
#136081=CARTESIAN_POINT('Ctrl Pts',(-4.8087363428629,4.17834651459899,5.42573711625745));
#136082=CARTESIAN_POINT('Ctrl Pts',(-4.80254121582195,4.17970788569747,
5.43122144101507));
#136083=CARTESIAN_POINT('Ctrl Pts',(-4.78393219541999,4.18379006156185,
5.44763860682258));
#136084=CARTESIAN_POINT('Ctrl Pts',(-4.77149014101508,4.18650992785334,
5.45853968456259));
#136085=CARTESIAN_POINT('Ctrl Pts',(-4.73407143490589,4.1946613843129,5.49109829800729));
#136086=CARTESIAN_POINT('Ctrl Pts',(-4.70898333589813,4.20008900932188,
5.51262813258871));
#136087=CARTESIAN_POINT('Ctrl Pts',(-4.63336514813262,4.21633619542157,
5.57662839111951));
#136088=CARTESIAN_POINT('Ctrl Pts',(-4.5823990272295,4.22713823126396,5.61858318778587));
#136089=CARTESIAN_POINT('Ctrl Pts',(-4.42810970281214,4.25939962410648,
5.7420962384294));
#136090=CARTESIAN_POINT('Ctrl Pts',(-4.32322521667029,4.28067054359089,
5.82147094945651));
#136091=CARTESIAN_POINT('Ctrl Pts',(-4.21622344427235,4.30202682562769,
5.89796235123299));
#136092=CARTESIAN_POINT('Ctrl Pts',(-5.388661875,4.302796438,4.85023949900001));
#136093=CARTESIAN_POINT('Ctrl Pts',(-5.126039633,4.238074114,5.142015289));
#136094=CARTESIAN_POINT('Ctrl Pts',(-4.83344805100001,4.172899507,5.403728337));
#136095=CARTESIAN_POINT('Ctrl Pts',(-4.82340824000853,4.17066314486255,
5.41270860060828));
#136096=CARTESIAN_POINT('Ctrl Pts',(-4.81336842901706,4.16842678272508,
5.42168886421645));
#136097=CARTESIAN_POINT('Ctrl Pts',(-5.73673607986641,4.302796438,4.83193568617792));
#136098=CARTESIAN_POINT('Ctrl Pts',(-5.47510492068605,4.238074114,5.1425583858957));
#136099=CARTESIAN_POINT('Ctrl Pts',(-5.181463613887,4.172899507,5.42311516817079));
#136100=CARTESIAN_POINT('Ctrl Pts',(-5.17138778327219,4.17066314486254,
5.43274202430646));
#136101=CARTESIAN_POINT('Ctrl Pts',(-5.1613119526574,4.16842678272508,5.44236888044202));
#136102=CARTESIAN_POINT('',(-5.38553804416647,4.30202682608494,4.85370785869225));
#136103=CARTESIAN_POINT('Origin',(0.130796620685834,4.16072143753726,-0.149305274772075));
#136104=CARTESIAN_POINT('Ctrl Pts',(-5.57275370959191,4.2631068065418,5.0194039576247));
#136105=CARTESIAN_POINT('Ctrl Pts',(-5.55126704606305,4.26736775488585,
5.00036857440293));
#136106=CARTESIAN_POINT('Ctrl Pts',(-5.52978080737595,4.27169422776882,
4.98134724825959));
#136107=CARTESIAN_POINT('Ctrl Pts',(-5.50829523230219,4.27608953519676,
4.96234120710692));
#136108=CARTESIAN_POINT('Ctrl Pts',(-5.4927902460748,4.27926139263606,4.9486255674139));
#136109=CARTESIAN_POINT('Ctrl Pts',(-5.47728190210849,4.2824699864591,4.93492215050233));
#136110=CARTESIAN_POINT('Ctrl Pts',(-5.46178013446649,4.285714286,4.92121979118411));
#136111=CARTESIAN_POINT('Ctrl Pts',(-5.45680768340001,4.2867549492618,4.9168245304209));
#136112=CARTESIAN_POINT('Ctrl Pts',(-5.45183604222683,4.28779988859445,
4.91242936939491));
#136113=CARTESIAN_POINT('Ctrl Pts',(-5.44686554586364,4.28884908281018,
4.90803394274152));
#136114=CARTESIAN_POINT('Ctrl Pts',(-5.42639884426299,4.29316928412718,
4.88993516967156));
#136115=CARTESIAN_POINT('Ctrl Pts',(-5.40595570935508,4.29756059498149,
4.87182655211498));
#136116=CARTESIAN_POINT('Ctrl Pts',(-5.38553804287315,4.30202682632576,
4.85370785966905));
#136117=CARTESIAN_POINT('Ctrl Pts',(-5.88675934464407,4.17158344184794,
4.23185872984859));
#136118=CARTESIAN_POINT('Ctrl Pts',(-5.88442296282203,4.17224147442397,
4.23510122292429));
#136119=CARTESIAN_POINT('Ctrl Pts',(-5.882086581,4.172899507,4.238343716));
#136120=CARTESIAN_POINT('Ctrl Pts',(-5.680103902,4.229787119,4.518660671));
#136121=CARTESIAN_POINT('Ctrl Pts',(-5.452379538,4.285714286,4.77849949));
#136122=CARTESIAN_POINT('Ctrl Pts',(-5.417659393,4.294241258,4.818115986));
#136123=CARTESIAN_POINT('Ctrl Pts',(-5.382367244,4.302795611,4.85722378));
#136124=CARTESIAN_POINT('Ctrl Pts',(-5.942903991763,4.17158344184794,4.57514595584757));
#136125=CARTESIAN_POINT('Ctrl Pts',(-5.9403783393815,4.17224147442397,4.57841918992378));
#136126=CARTESIAN_POINT('Ctrl Pts',(-5.937852687,4.172899507,4.581692424));
#136127=CARTESIAN_POINT('Ctrl Pts',(-5.719507368,4.229787119,4.864666971));
#136128=CARTESIAN_POINT('Ctrl Pts',(-5.475241792,4.285714286,5.125595314));
#136129=CARTESIAN_POINT('Ctrl Pts',(-5.43799968,4.294241258,5.165377926));
#136130=CARTESIAN_POINT('Ctrl Pts',(-5.40018341600001,4.302795611,5.20461517));
#136131=CARTESIAN_POINT('Ctrl Pts',(-5.88208638225256,4.17289956298542,
4.23834399206812));
#136132=CARTESIAN_POINT('Ctrl Pts',(-5.79504213826813,4.197415223681,4.35914630590836));
#136133=CARTESIAN_POINT('Ctrl Pts',(-5.70444709207052,4.22178368168539,
4.47702311374695));
#136134=CARTESIAN_POINT('Ctrl Pts',(-5.61060950626881,4.24593817251312,
4.59168389254803));
#136135=CARTESIAN_POINT('Ctrl Pts',(-5.55883415213957,4.25926553282117,
4.65494854685941));
#136136=CARTESIAN_POINT('Ctrl Pts',(-5.50607225823275,4.27252781056818,
4.71723484194515));
#136137=CARTESIAN_POINT('Ctrl Pts',(-5.45237953796616,4.28571428600831,
4.77849949003861));
#136138=CARTESIAN_POINT('Ctrl Pts',(-5.43029027710596,4.29113922040459,
4.80370385236194));
#136139=CARTESIAN_POINT('Ctrl Pts',(-5.40800898232443,4.2965769798951,4.82877473577457));
#136140=CARTESIAN_POINT('Ctrl Pts',(-5.38553804393672,4.30202682606781,
4.85370785848893));
#136141=CARTESIAN_POINT('Ctrl Pts',(-6.305336075,4.302796438,3.57844058));
#136142=CARTESIAN_POINT('Ctrl Pts',(-6.111576965,4.238074114,3.919850833));
#136143=CARTESIAN_POINT('Ctrl Pts',(-5.882086581,4.172899507,4.238343716));
#136144=CARTESIAN_POINT('Ctrl Pts',(-5.87421198671132,4.1706631449394,4.24927228822925));
#136145=CARTESIAN_POINT('Ctrl Pts',(-5.86633739242265,4.16842678287881,
4.26020086045845));
#136146=CARTESIAN_POINT('Ctrl Pts',(-6.6413377196824,4.302796438,3.48573903474629));
#136147=CARTESIAN_POINT('Ctrl Pts',(-6.45259804968316,4.238074114,3.84534251319503));
#136148=CARTESIAN_POINT('Ctrl Pts',(-6.22613332948798,4.172899507,4.18246423546578));
#136149=CARTESIAN_POINT('Ctrl Pts',(-6.21836255599781,4.1706631449394,4.19403202642291));
#136150=CARTESIAN_POINT('Ctrl Pts',(-6.21059178250765,4.16842678287881,
4.20559981738003));
#136151=CARTESIAN_POINT('',(-6.3030308728385,4.30202682607316,3.58249938071131));
#136152=CARTESIAN_POINT('Origin',(0.159834808439206,4.16072143984921,-0.117697143487096));
#136153=CARTESIAN_POINT('Ctrl Pts',(-6.52148930321773,4.26310680820184,
3.70407576429898));
#136154=CARTESIAN_POINT('Ctrl Pts',(-6.49641294089323,4.26736775487178,
3.69010441533625));
#136155=CARTESIAN_POINT('Ctrl Pts',(-6.47134001560251,4.27169422777064,
3.67614670344654));
#136156=CARTESIAN_POINT('Ctrl Pts',(-6.44627102503695,4.27608953507197,
3.66220377698965));
#136157=CARTESIAN_POINT('Ctrl Pts',(-6.42237710548024,4.28027881899269,
3.64891440411782));
#136158=CARTESIAN_POINT('Ctrl Pts',(-6.3984813683556,4.28452899143848,3.63564731287308));
#136159=CARTESIAN_POINT('Ctrl Pts',(-6.37460306918202,4.28884908356176,
3.62237175053091));
#136160=CARTESIAN_POINT('Ctrl Pts',(-6.35072417052129,4.29316928414502,
3.60909585489328));
#136161=CARTESIAN_POINT('Ctrl Pts',(-6.32686616717162,4.29756059498849,
3.59580527662949));
#136162=CARTESIAN_POINT('Ctrl Pts',(-6.30303086975177,4.30202682552141,
3.58249937757921));
#136163=CARTESIAN_POINT('Ctrl Pts',(-6.65885471669918,4.17158344184794,
2.86744097718168));
#136164=CARTESIAN_POINT('Ctrl Pts',(-6.65726999834959,4.17224147442397,
2.87110991559084));
#136165=CARTESIAN_POINT('Ctrl Pts',(-6.65568528,4.172899507,2.874778854));
#136166=CARTESIAN_POINT('Ctrl Pts',(-6.518684703,4.229787119,3.191962459));
#136167=CARTESIAN_POINT('Ctrl Pts',(-6.352142073,4.285714286,3.494680397));
#136168=CARTESIAN_POINT('Ctrl Pts',(-6.326750041,4.294241258,3.540834488));
#136169=CARTESIAN_POINT('Ctrl Pts',(-6.300690023,4.302795611,3.586614732));
#136170=CARTESIAN_POINT('Ctrl Pts',(-6.78748333890467,4.17158344184794,
3.19063289841924));
#136171=CARTESIAN_POINT('Ctrl Pts',(-6.78572038345234,4.17224147442397,
3.19437254670962));
#136172=CARTESIAN_POINT('Ctrl Pts',(-6.783957428,4.172899507,3.198112195));
#136173=CARTESIAN_POINT('Ctrl Pts',(-6.631548065,4.229787119,3.521408744));
#136174=CARTESIAN_POINT('Ctrl Pts',(-6.449085162,4.285714286,3.828746606));
#136175=CARTESIAN_POINT('Ctrl Pts',(-6.421265836,4.294241258,3.875605075));
#136176=CARTESIAN_POINT('Ctrl Pts',(-6.392768543,4.302795611,3.922054354));
#136177=CARTESIAN_POINT('Ctrl Pts',(-6.65568527858334,4.17289950772645,
2.87477885888926));
#136178=CARTESIAN_POINT('Ctrl Pts',(-6.65056502153285,4.17502562427833,
2.8866332729685));
#136179=CARTESIAN_POINT('Ctrl Pts',(-6.64896125271127,4.1756853480929,2.89030735746956));
#136180=CARTESIAN_POINT('Ctrl Pts',(-6.6424987876089,4.17834651454824,2.90512965729521));
#136181=CARTESIAN_POINT('Ctrl Pts',(-6.63917905077847,4.17970788564625,
2.91270836196509));
#136182=CARTESIAN_POINT('Ctrl Pts',(-6.6291833502722,4.18379006150965,2.93542190296867));
#136183=CARTESIAN_POINT('Ctrl Pts',(-6.62246849125797,4.18650992780003,
2.95053973621401));
#136184=CARTESIAN_POINT('Ctrl Pts',(-6.60217920028303,4.19466138425825,
2.99580084035583));
#136185=CARTESIAN_POINT('Ctrl Pts',(-6.58845000118158,4.20008900926453,
3.02587500834143));
#136186=CARTESIAN_POINT('Ctrl Pts',(-6.54669380299953,4.21633619562176,
3.11571132414243));
#136187=CARTESIAN_POINT('Ctrl Pts',(-6.51805456655974,4.22713823132758,
3.17518858420653));
#136188=CARTESIAN_POINT('Ctrl Pts',(-6.42988713789993,4.25939962926024,
3.3520704264618));
#136189=CARTESIAN_POINT('Ctrl Pts',(-6.3680251256942,4.28067055054578,3.46814882480474));
#136190=CARTESIAN_POINT('Ctrl Pts',(-6.30303087435391,4.30202682552899,
3.58249938167426));
#136191=CARTESIAN_POINT('Ctrl Pts',(-6.927179768,4.302796438,2.139317756));
#136192=CARTESIAN_POINT('Ctrl Pts',(-6.811343751,4.238074114,2.514398508));
#136193=CARTESIAN_POINT('Ctrl Pts',(-6.65568528000001,4.172899507,2.874778854));
#136194=CARTESIAN_POINT('Ctrl Pts',(-6.65034410928241,4.17066314491703,
2.88714472743355));
#136195=CARTESIAN_POINT('Ctrl Pts',(-6.64500293856484,4.16842678283405,
2.89951060086715));
#136196=CARTESIAN_POINT('Ctrl Pts',(-7.23539778916921,4.302796438,1.97655309987432));
#136197=CARTESIAN_POINT('Ctrl Pts',(-7.12837486615929,4.238074114,2.36832269907274));
#136198=CARTESIAN_POINT('Ctrl Pts',(-6.9796759695216,4.172899507,2.7462459230242));
#136199=CARTESIAN_POINT('Ctrl Pts',(-6.97457360543338,4.17066314491702,
2.75921375217153));
#136200=CARTESIAN_POINT('Ctrl Pts',(-6.96947124134512,4.16842678283406,
2.77218158131886));
#136201=CARTESIAN_POINT('',(-6.92580098261212,4.3020268259686,2.14377721513266));
#136202=CARTESIAN_POINT('Origin',(0.181399492165553,4.16072144628749,-0.0805857300572521));
#136203=CARTESIAN_POINT('Ctrl Pts',(-7.16528730494324,4.26310680820237,
2.21554910463716));
#136204=CARTESIAN_POINT('Ctrl Pts',(-7.13779378704632,4.26736775490308,
2.20729507488378));
#136205=CARTESIAN_POINT('Ctrl Pts',(-7.11030655738358,4.27169422779421,
2.19905362431567));
#136206=CARTESIAN_POINT('Ctrl Pts',(-7.08282634888507,4.27608953508727,
2.19082576765599));
#136207=CARTESIAN_POINT('Ctrl Pts',(-7.05663423357179,4.28027881900277,
2.18298357932531));
#136208=CARTESIAN_POINT('Ctrl Pts',(-7.03044513306719,4.28452899143874,
2.17516354243805));
#136209=CARTESIAN_POINT('Ctrl Pts',(-7.0042712418177,4.28884908356817,2.16733148377025));
#136210=CARTESIAN_POINT('Ctrl Pts',(-6.97809669344815,4.29316928415757,
2.15949922847128));
#136211=CARTESIAN_POINT('Ctrl Pts',(-6.95193939554079,4.29756059500922,
2.15164814193842));
#136212=CARTESIAN_POINT('Ctrl Pts',(-6.92580098108579,4.30202682519232,
2.14377721262106));
#136213=CARTESIAN_POINT('Ctrl Pts',(-7.11958944241024,4.17158344184794,
1.36894487045972));
#136214=CARTESIAN_POINT('Ctrl Pts',(-7.11883048720513,4.17224147442397,
1.37286869872986));
#136215=CARTESIAN_POINT('Ctrl Pts',(-7.118071532,4.172899507,1.376792527));
#136216=CARTESIAN_POINT('Ctrl Pts',(-7.052459052,4.229787119,1.71601163));
#136217=CARTESIAN_POINT('Ctrl Pts',(-6.954885505,4.285714286,2.047453934));
#136218=CARTESIAN_POINT('Ctrl Pts',(-6.94000889,4.294241258,2.097987503));
#136219=CARTESIAN_POINT('Ctrl Pts',(-6.924399539,4.302795611,2.148299564));
#136220=CARTESIAN_POINT('Ctrl Pts',(-7.31468750940415,4.17158344184794,
1.65692939362537));
#136221=CARTESIAN_POINT('Ctrl Pts',(-7.31376968470208,4.17224147442397,
1.66096059431268));
#136222=CARTESIAN_POINT('Ctrl Pts',(-7.31285186,4.172899507,1.664991795));
#136223=CARTESIAN_POINT('Ctrl Pts',(-7.233504944,4.229787119,2.013493357));
#136224=CARTESIAN_POINT('Ctrl Pts',(-7.121376478,4.285714286,2.352869961));
#136225=CARTESIAN_POINT('Ctrl Pts',(-7.104280738,4.294241258,2.404613239));
#136226=CARTESIAN_POINT('Ctrl Pts',(-7.08643491800001,4.302795611,2.456102635));
#136227=CARTESIAN_POINT('Ctrl Pts',(-7.11807146745239,4.17289956296434,
1.37679286071363));
#136228=CARTESIAN_POINT('Ctrl Pts',(-7.08979582541024,4.19741522461937,
1.52297900648501));
#136229=CARTESIAN_POINT('Ctrl Pts',(-7.05706917398433,4.22178368355328,
1.66800097785143));
#136230=CARTESIAN_POINT('Ctrl Pts',(-7.02004929737975,4.24593817527534,
1.81146566714692));
#136231=CARTESIAN_POINT('Ctrl Pts',(-6.99962339875592,4.25926553464218,
1.89062301364352));
#136232=CARTESIAN_POINT('Ctrl Pts',(-6.9778913386645,4.27252781145132,1.96930666269499));
#136233=CARTESIAN_POINT('Ctrl Pts',(-6.95488550517666,4.2857142859596,2.04745393395531));
#136234=CARTESIAN_POINT('Ctrl Pts',(-6.94542087204743,4.29113922043585,
2.07960383435806));
#136235=CARTESIAN_POINT('Ctrl Pts',(-6.93572590721988,4.29657697986723,
2.11171322429797));
#136236=CARTESIAN_POINT('Ctrl Pts',(-6.92580098234181,4.30202682588361,
2.14377721466289));
#136237=CARTESIAN_POINT('Ctrl Pts',(-7.225116234,4.302796438,0.600162811));
#136238=CARTESIAN_POINT('Ctrl Pts',(-7.19261967400001,4.238074114,0.991375703));
#136239=CARTESIAN_POINT('Ctrl Pts',(-7.118071532,4.172899507,1.376792527));
#136240=CARTESIAN_POINT('Ctrl Pts',(-7.11551353207835,4.17066314489725,
1.39001748712837));
#136241=CARTESIAN_POINT('Ctrl Pts',(-7.11295553215668,4.1684267827945,1.40324244725675));
#136242=CARTESIAN_POINT('Ctrl Pts',(-7.49113869911339,4.302796438,0.374945738428264));
#136243=CARTESIAN_POINT('Ctrl Pts',(-7.47083679599638,4.238074114,0.780562747110289));
#136244=CARTESIAN_POINT('Ctrl Pts',(-7.40685671966933,4.172899507,1.18161620345787));
#136245=CARTESIAN_POINT('Ctrl Pts',(-7.40466134597066,4.17066314489725,
1.19537770954496));
#136246=CARTESIAN_POINT('Ctrl Pts',(-7.40246597227197,4.1684267827945,1.20913921563204));
#136247=CARTESIAN_POINT('',(-7.2247283364511,4.30202682595718,0.604814408909641));
#136248=CARTESIAN_POINT('Origin',(0.194481632606994,4.1607214752105,-0.0397060957560117));
#136249=CARTESIAN_POINT('Ctrl Pts',(-7.47404443578633,4.26310680820214,
0.623425831514019));
#136250=CARTESIAN_POINT('Ctrl Pts',(-7.44541932874542,4.26736775483642,
0.621275069824007));
#136251=CARTESIAN_POINT('Ctrl Pts',(-7.41680306703337,4.27169422772008,
0.619135241647022));
#136252=CARTESIAN_POINT('Ctrl Pts',(-7.38819658462309,4.2760895350054,0.617007180217377));
#136253=CARTESIAN_POINT('Ctrl Pts',(-7.36093098775278,4.28027881891818,
0.614978868444409));
#136254=CARTESIAN_POINT('Ctrl Pts',(-7.33367309711141,4.28452899135015,
0.612971542138589));
#136255=CARTESIAN_POINT('Ctrl Pts',(-7.30642747581962,4.288849083484,0.610949205513844));
#136256=CARTESIAN_POINT('Ctrl Pts',(-7.27918117050091,4.29316928407784,
0.608926818116439));
#136257=CARTESIAN_POINT('Ctrl Pts',(-7.25194766417651,4.29756059492796,
0.606882331437864));
#136258=CARTESIAN_POINT('Ctrl Pts',(-7.22472833267039,4.3020268255214,0.604814407460073));
#136259=CARTESIAN_POINT('Ctrl Pts',(-7.24742007933239,4.17158344184794,
-0.193561576570007));
#136260=CARTESIAN_POINT('Ctrl Pts',(-7.24752237516619,4.17224147442397,
-0.189566332285004));
#136261=CARTESIAN_POINT('Ctrl Pts',(-7.247624671,4.172899507,-0.185571088));
#136262=CARTESIAN_POINT('Ctrl Pts',(-7.256468254,4.229787119,0.159822005));
#136263=CARTESIAN_POINT('Ctrl Pts',(-7.23242622,4.285714286,0.5044908));
#136264=CARTESIAN_POINT('Ctrl Pts',(-7.22876063600001,4.294241258,0.557040955));
#136265=CARTESIAN_POINT('Ctrl Pts',(-7.224331829,4.302795611,0.609532297));
#136266=CARTESIAN_POINT('Ctrl Pts',(-7.4998650209685,4.17158344184794,0.0457497107196035));
#136267=CARTESIAN_POINT('Ctrl Pts',(-7.49983524348425,4.17224147442397,
0.0498839693598018));
#136268=CARTESIAN_POINT('Ctrl Pts',(-7.499805466,4.172899507,0.054018228));
#136269=CARTESIAN_POINT('Ctrl Pts',(-7.497231171,4.229787119,0.411429259));
#136270=CARTESIAN_POINT('Ctrl Pts',(-7.460680145,4.285714286,0.766975733));
#136271=CARTESIAN_POINT('Ctrl Pts',(-7.455107369,4.294241258,0.82118436));
#136272=CARTESIAN_POINT('Ctrl Pts',(-7.448747472,4.302795611,0.875306286));
#136273=CARTESIAN_POINT('Ctrl Pts',(-7.24762467222106,4.17289950769165,
-0.185571082742715));
#136274=CARTESIAN_POINT('Ctrl Pts',(-7.24795519204109,4.17502562416708,
-0.172662368237618));
#136275=CARTESIAN_POINT('Ctrl Pts',(-7.24804235892694,4.17568534802917,
-0.168654454115379));
#136276=CARTESIAN_POINT('Ctrl Pts',(-7.24840090660423,4.17834651449988,
-0.152488580367354));
#136277=CARTESIAN_POINT('Ctrl Pts',(-7.24857021054988,4.17970788559751,
-0.144216412981057));
#136278=CARTESIAN_POINT('Ctrl Pts',(-7.24903552678746,4.18379006146066,
-0.119405075762955));
#136279=CARTESIAN_POINT('Ctrl Pts',(-7.24928909921507,4.1865099277502,-0.102865005793642));
#136280=CARTESIAN_POINT('Ctrl Pts',(-7.24987968178903,4.19466138420899,
-0.0532678880350508));
#136281=CARTESIAN_POINT('Ctrl Pts',(-7.25004721352457,4.200089009213,-0.0202085713368787));
#136282=CARTESIAN_POINT('Ctrl Pts',(-7.2498716043712,4.2163361945907,0.0788576272574867));
#136283=CARTESIAN_POINT('Ctrl Pts',(-7.24885319079528,4.22713823077996,
0.144863032802135));
#136284=CARTESIAN_POINT('Ctrl Pts',(-7.24310535697581,4.25939963221318,
0.342417208870289));
#136285=CARTESIAN_POINT('Ctrl Pts',(-7.23570096849353,4.28067055518881,
0.473742302818427));
#136286=CARTESIAN_POINT('Ctrl Pts',(-7.22472833839899,4.30202682550461,
0.604814409146449));
#136287=CARTESIAN_POINT('Ctrl Pts',(-7.185214296,4.302796438,-0.967055079));
#136288=CARTESIAN_POINT('Ctrl Pts',(-7.237576694,4.238074114,-0.578002727000001));
#136289=CARTESIAN_POINT('Ctrl Pts',(-7.247624671,4.172899507,-0.185571088));
#136290=CARTESIAN_POINT('Ctrl Pts',(-7.24796945123017,4.17066314479459,
-0.172105425128183));
#136291=CARTESIAN_POINT('Ctrl Pts',(-7.24831423146048,4.16842678258919,
-0.158639762256362));
#136292=CARTESIAN_POINT('Ctrl Pts',(-7.39660228961032,4.302796438,-1.24419366777359));
#136293=CARTESIAN_POINT('Ctrl Pts',(-7.46397070149007,4.238074114,-0.843695450120858));
#136294=CARTESIAN_POINT('Ctrl Pts',(-7.48770108087874,4.172899507,-0.438264575817995));
#136295=CARTESIAN_POINT('Ctrl Pts',(-7.48851535082266,4.17066314479459,
-0.424352865016336));
#136296=CARTESIAN_POINT('Ctrl Pts',(-7.48932962076643,4.16842678258918,
-0.410441154214679));
#136297=CARTESIAN_POINT('',(-7.18583542224986,4.30202682602123,-0.962428846804123));
#136298=CARTESIAN_POINT('Origin',(0.198470723781902,4.16072144092381,0.00303002836568644));
#136299=CARTESIAN_POINT('Ctrl Pts',(-7.43332355589999,4.26310680820188,
-0.997848140191728));
#136300=CARTESIAN_POINT('Ctrl Pts',(-7.40490533771934,4.26736775491181,
-0.993795066420131));
#136301=CARTESIAN_POINT('Ctrl Pts',(-7.3764981084869,4.27169422779882,-0.989733216274674));
#136302=CARTESIAN_POINT('Ctrl Pts',(-7.34810295942663,4.27608953509018,
-0.985661976730497));
#136303=CARTESIAN_POINT('Ctrl Pts',(-7.32103878997482,4.28027881900884,
-0.981781570374166));
#136304=CARTESIAN_POINT('Ctrl Pts',(-7.2939866578393,4.28452899145251,-0.977882325800221));
#136305=CARTESIAN_POINT('Ctrl Pts',(-7.26694328144623,4.28884908358092,
-0.974000378013041));
#136306=CARTESIAN_POINT('Ctrl Pts',(-7.23989922610386,4.2931692841693,-0.970118332765922));
#136307=CARTESIAN_POINT('Ctrl Pts',(-7.21286291982685,4.29756059502628,
-0.966260621572241));
#136308=CARTESIAN_POINT('Ctrl Pts',(-7.18583541843999,4.30202682552111,
-0.962428847399571));
#136309=CARTESIAN_POINT('Ctrl Pts',(-7.03636940770779,4.17158344184794,
-1.7470172992385));
#136310=CARTESIAN_POINT('Ctrl Pts',(-7.0373281713539,4.17224147442397,-1.74313745211925));
#136311=CARTESIAN_POINT('Ctrl Pts',(-7.038286935,4.172899507,-1.739257605));
#136312=CARTESIAN_POINT('Ctrl Pts',(-7.121173066,4.229787119,-1.403840719));
#136313=CARTESIAN_POINT('Ctrl Pts',(-7.171786724,4.285714286,-1.062061763));
#136314=CARTESIAN_POINT('Ctrl Pts',(-7.179503569,4.294241258,-1.009952209));
#136315=CARTESIAN_POINT('Ctrl Pts',(-7.186462392,4.302795611,-0.957736023));
#136316=CARTESIAN_POINT('Ctrl Pts',(-7.33435717978959,4.17158344184794,
-1.56756917649812));
#136317=CARTESIAN_POINT('Ctrl Pts',(-7.33521684189479,4.17224147442397,
-1.56352517324906));
#136318=CARTESIAN_POINT('Ctrl Pts',(-7.336076504,4.172899507,-1.55948117));
#136319=CARTESIAN_POINT('Ctrl Pts',(-7.410395202,4.229787119,-1.209872813));
#136320=CARTESIAN_POINT('Ctrl Pts',(-7.4511307,4.285714286,-0.854781429));
#136321=CARTESIAN_POINT('Ctrl Pts',(-7.457341465,4.294241258,-0.800642187));
#136322=CARTESIAN_POINT('Ctrl Pts',(-7.462764873,4.302795611,-0.746418412));
#136323=CARTESIAN_POINT('Ctrl Pts',(-7.03828701704771,4.17289956295234,
-1.73925727478107));
#136324=CARTESIAN_POINT('Ctrl Pts',(-7.07400671165685,4.19741522660035,
-1.59470967625666));
#136325=CARTESIAN_POINT('Ctrl Pts',(-7.10519795470142,4.22178368756786,
-1.44934972323286));
#136326=CARTESIAN_POINT('Ctrl Pts',(-7.13183888559359,4.2459381813504,-1.30360044244046));
#136327=CARTESIAN_POINT('Ctrl Pts',(-7.14653814647385,4.25926553867801,
-1.22318258053661));
#136328=CARTESIAN_POINT('Ctrl Pts',(-7.15985306735223,4.2725278134871,-1.14264619181022));
#136329=CARTESIAN_POINT('Ctrl Pts',(-7.17178672404415,4.28571428603967,
-1.06206176275147));
#136330=CARTESIAN_POINT('Ctrl Pts',(-7.17669624850512,4.29113922041278,
-1.02890920747046));
#136331=CARTESIAN_POINT('Ctrl Pts',(-7.18137971989326,4.29657697980703,
-0.995696704394958));
#136332=CARTESIAN_POINT('Ctrl Pts',(-7.18583542232086,4.30202682589502,
-0.962428846792947));
#136333=CARTESIAN_POINT('Ctrl Pts',(-6.809339722,4.302796438,-2.489054549));
#136334=CARTESIAN_POINT('Ctrl Pts',(-6.944112672,4.238074114,-2.120354393));
#136335=CARTESIAN_POINT('Ctrl Pts',(-7.03828693500001,4.172899507,-1.739257605));
#136336=CARTESIAN_POINT('Ctrl Pts',(-7.04151837395981,4.17066314477596,
-1.72618087926869));
#136337=CARTESIAN_POINT('Ctrl Pts',(-7.04474981291962,4.16842678255194,
-1.71310415353744));
#136338=CARTESIAN_POINT('Ctrl Pts',(-6.95620897777936,4.302796438,-2.80515596191518));
#136339=CARTESIAN_POINT('Ctrl Pts',(-7.10809763203523,4.238074114,-2.42850338715821));
#136340=CARTESIAN_POINT('Ctrl Pts',(-7.21842886209782,4.172899507,-2.03765259113535));
#136341=CARTESIAN_POINT('Ctrl Pts',(-7.22221470149757,4.17066314477596,
-2.02424117224549));
#136342=CARTESIAN_POINT('Ctrl Pts',(-7.2260005408973,4.16842678255194,-2.01082975335561));
#136343=CARTESIAN_POINT('',(-6.81094083021135,4.30202682600845,-2.48466999876099));
#136344=CARTESIAN_POINT('Origin',(0.193179002053649,4.16072148814982,0.045624470169838));
#136345=CARTESIAN_POINT('Ctrl Pts',(-7.04502872801916,4.26310680820185,
-2.57246384252604));
#136346=CARTESIAN_POINT('Ctrl Pts',(-7.01814620294762,4.26736775489512,
-2.56239645050777));
#136347=CARTESIAN_POINT('Ctrl Pts',(-6.99127629662423,4.27169422777541,
-2.55232284955793));
#136348=CARTESIAN_POINT('Ctrl Pts',(-6.96442020648899,4.2760895350602,-2.54224267560679));
#136349=CARTESIAN_POINT('Ctrl Pts',(-6.93882295490606,4.28027881897259,
-2.53263499454347));
#136350=CARTESIAN_POINT('Ctrl Pts',(-6.91324150887699,4.28452899140873,
-2.52301150334713));
#136351=CARTESIAN_POINT('Ctrl Pts',(-6.88766489559402,4.28884908352697,
-2.51340678675703));
#136352=CARTESIAN_POINT('Ctrl Pts',(-6.86208764018609,4.2931692841052,-2.50380182903149));
#136353=CARTESIAN_POINT('Ctrl Pts',(-6.83651272154255,4.29756059496695,
-2.49422230234871));
#136354=CARTESIAN_POINT('Ctrl Pts',(-6.81094082624314,4.30202682552111,
-2.48466999852055));
#136355=CARTESIAN_POINT('Ctrl Pts',(-6.49630592356605,4.17158344184794,
-3.21878443522406));
#136356=CARTESIAN_POINT('Ctrl Pts',(-6.49807632428302,4.17224147442397,
-3.21520140261203));
#136357=CARTESIAN_POINT('Ctrl Pts',(-6.499846725,4.172899507,-3.21161837));
#136358=CARTESIAN_POINT('Ctrl Pts',(-6.652899739,4.229787119,-2.901861412));
#136359=CARTESIAN_POINT('Ctrl Pts',(-6.775802451,4.285714286,-2.578953498));
#136360=CARTESIAN_POINT('Ctrl Pts',(-6.794540894,4.294241258,-2.52972113));
#136361=CARTESIAN_POINT('Ctrl Pts',(-6.81256196000001,4.302795611,-2.480221671));
#136362=CARTESIAN_POINT('Ctrl Pts',(-6.82590294932948,4.17158344184794,
-3.10759027252605));
#136363=CARTESIAN_POINT('Ctrl Pts',(-6.82761185416474,4.17224147442397,
-3.10382561776302));
#136364=CARTESIAN_POINT('Ctrl Pts',(-6.829320759,4.172899507,-3.100060963));
#136365=CARTESIAN_POINT('Ctrl Pts',(-6.977057389,4.229787119,-2.774602578));
#136366=CARTESIAN_POINT('Ctrl Pts',(-7.093174665,4.285714286,-2.436569961));
#136367=CARTESIAN_POINT('Ctrl Pts',(-7.11087856200001,4.294241258,-2.385031595));
#136368=CARTESIAN_POINT('Ctrl Pts',(-7.127831683,4.302795611,-2.333241414));
#136369=CARTESIAN_POINT('Ctrl Pts',(-6.49984687581053,4.17289956305412,
-3.21161806478148));
#136370=CARTESIAN_POINT('Ctrl Pts',(-6.56580492407541,4.19741522640325,
-3.07812858848471));
#136371=CARTESIAN_POINT('Ctrl Pts',(-6.62751502573194,4.22178368708935,
-2.94287226689012));
#136372=CARTESIAN_POINT('Ctrl Pts',(-6.68486489301122,4.2459381806137,-2.80625753724418));
#136373=CARTESIAN_POINT('Ctrl Pts',(-6.7165079571281,4.25926553817461,-2.73087970544478));
#136374=CARTESIAN_POINT('Ctrl Pts',(-6.74682452604478,4.27252781322038,
-2.65508852572861));
#136375=CARTESIAN_POINT('Ctrl Pts',(-6.77580245114839,4.28571428601294,
-2.57895349787146));
#136376=CARTESIAN_POINT('Ctrl Pts',(-6.78772401284233,4.291139220383,-2.54763143360634));
#136377=CARTESIAN_POINT('Ctrl Pts',(-6.79943769358361,4.29657697979264,
-2.51620222834178));
#136378=CARTESIAN_POINT('Ctrl Pts',(-6.81094083028747,4.30202682596771,
-2.48466999878171));
#136379=CARTESIAN_POINT('Ctrl Pts',(-6.115067991,4.302796438,-3.894668594));
#136380=CARTESIAN_POINT('Ctrl Pts',(-6.32594966,4.238074114,-3.563560643));
#136381=CARTESIAN_POINT('Ctrl Pts',(-6.499846725,4.172899507,-3.21161837));
#136382=CARTESIAN_POINT('Ctrl Pts',(-6.50581372401252,4.17066314484168,
-3.19954203509781));
#136383=CARTESIAN_POINT('Ctrl Pts',(-6.5117807230249,4.16842678268336,-3.18746570019562));
#136384=CARTESIAN_POINT('Ctrl Pts',(-6.19055106550287,4.302796438,-4.23495228059749));
#136385=CARTESIAN_POINT('Ctrl Pts',(-6.41985781636945,4.238074114,-3.89975720418037));
#136386=CARTESIAN_POINT('Ctrl Pts',(-6.61163093230066,4.172899507,-3.5417622357951));
#136387=CARTESIAN_POINT('Ctrl Pts',(-6.61821131934391,4.17066314484168,
-3.5294782123538));
#136388=CARTESIAN_POINT('Ctrl Pts',(-6.62479170638728,4.16842678268338,
-3.51719418891246));
#136389=CARTESIAN_POINT('',(-6.1175742154234,4.30202682597258,-3.89073074407606));
#136390=CARTESIAN_POINT('Origin',(0.178854686864315,4.1607214229367,0.0860855762359175));
#136391=CARTESIAN_POINT('Ctrl Pts',(-6.32731618655374,4.26310680820184,
-4.02679399416409));
#136392=CARTESIAN_POINT('Ctrl Pts',(-6.30322635167546,4.2673677548649,-4.01118302401819));
#136393=CARTESIAN_POINT('Ctrl Pts',(-6.27915017526903,4.27169422775724,
-3.9955687026238));
#136394=CARTESIAN_POINT('Ctrl Pts',(-6.25508890503238,4.27608953505144,
-3.97995093197959));
#136395=CARTESIAN_POINT('Ctrl Pts',(-6.23215547048255,4.28027881895734,
-3.96506522073654));
#136396=CARTESIAN_POINT('Ctrl Pts',(-6.20924087068471,4.2845289913791,-3.95016746669878));
#136397=CARTESIAN_POINT('Ctrl Pts',(-6.18632695457098,4.28884908350346,
-3.93528908736913));
#136398=CARTESIAN_POINT('Ctrl Pts',(-6.16341246318179,4.29316928408781,
-3.92041033450374));
#136399=CARTESIAN_POINT('Ctrl Pts',(-6.14049478700705,4.29756059494739,
-3.90555692044372));
#136400=CARTESIAN_POINT('Ctrl Pts',(-6.11757421157827,4.30202682552139,
-3.8907307430016));
#136401=CARTESIAN_POINT('Ctrl Pts',(-5.6524823943449,4.17158344184794,-4.54004478794309));
#136402=CARTESIAN_POINT('Ctrl Pts',(-5.65498165017245,4.17224147442397,
-4.53692610847154));
#136403=CARTESIAN_POINT('Ctrl Pts',(-5.657480906,4.172899507,-4.533807429));
#136404=CARTESIAN_POINT('Ctrl Pts',(-5.873544215,4.229787119,-4.264194291));
#136405=CARTESIAN_POINT('Ctrl Pts',(-6.062989186,4.285714286,-3.975256234));
#136406=CARTESIAN_POINT('Ctrl Pts',(-6.091873039,4.294241258,-3.931203103));
#136407=CARTESIAN_POINT('Ctrl Pts',(-6.120113703,4.302795611,-3.88673491));
#136408=CARTESIAN_POINT('Ctrl Pts',(-5.9982770828366,4.17158344184794,-4.50230390039397));
#136409=CARTESIAN_POINT('Ctrl Pts',(-6.0007553239183,4.17224147442397,-4.49899462519698));
#136410=CARTESIAN_POINT('Ctrl Pts',(-6.003233565,4.172899507,-4.49568535));
#136411=CARTESIAN_POINT('Ctrl Pts',(-6.217480127,4.229787119,-4.20959501));
#136412=CARTESIAN_POINT('Ctrl Pts',(-6.403549666,4.285714286,-3.904427189));
#136413=CARTESIAN_POINT('Ctrl Pts',(-6.431918881,4.294241258,-3.857899576));
#136414=CARTESIAN_POINT('Ctrl Pts',(-6.45960900600001,4.302795611,-3.810964641));
#136415=CARTESIAN_POINT('Ctrl Pts',(-5.65748091034017,4.17289950777047,
-4.53380742519254));
#136416=CARTESIAN_POINT('Ctrl Pts',(-5.66555605643019,4.17502562434964,
-4.52373090866465));
#136417=CARTESIAN_POINT('Ctrl Pts',(-5.6680509353656,4.17568534813323,-4.52059298754607));
#136418=CARTESIAN_POINT('Ctrl Pts',(-5.67811954256308,4.17834651458591,
-4.50794043144338));
#136419=CARTESIAN_POINT('Ctrl Pts',(-5.68326042665598,4.17970788568245,
-4.50145747473345));
#136420=CARTESIAN_POINT('Ctrl Pts',(-5.69864604318714,4.18379006154285,
-4.48198693861613));
#136421=CARTESIAN_POINT('Ctrl Pts',(-5.70885753428319,4.18650992783038,
-4.4689729591054));
#136422=CARTESIAN_POINT('Ctrl Pts',(-5.73934258974514,4.19466138428471,
-4.42984644292587));
#136423=CARTESIAN_POINT('Ctrl Pts',(-5.75948260660457,4.20008900928439,
-4.40362953603836));
#136424=CARTESIAN_POINT('Ctrl Pts',(-5.81929511903045,4.21633619593903,
-4.32465734190559));
#136425=CARTESIAN_POINT('Ctrl Pts',(-5.85842913392724,4.22713823148072,
-4.27149458167131));
#136426=CARTESIAN_POINT('Ctrl Pts',(-5.97340800784085,4.25939963040738,
-4.11074464354552));
#136427=CARTESIAN_POINT('Ctrl Pts',(-6.04698798485694,4.28067055282548,
-4.00171670482559));
#136428=CARTESIAN_POINT('Ctrl Pts',(-6.11757421701856,4.30202682553039,
-3.89073074500549));
#136429=CARTESIAN_POINT('Ctrl Pts',(-5.134862478,4.302796438,-5.11817226500001));
#136430=CARTESIAN_POINT('Ctrl Pts',(-5.41199227200001,4.238074114,-4.840138759));
#136431=CARTESIAN_POINT('Ctrl Pts',(-5.657480906,4.172899507,-4.533807429));
#136432=CARTESIAN_POINT('Ctrl Pts',(-5.66590445502806,4.17066314481695,
-4.52329616037206));
#136433=CARTESIAN_POINT('Ctrl Pts',(-5.67432800405597,4.1684267826339,-4.51278489174419));
#136434=CARTESIAN_POINT('Ctrl Pts',(-5.13542986618061,4.302796438,-5.46672693770758));
#136435=CARTESIAN_POINT('Ctrl Pts',(-5.4314325856829,4.238074114,-5.18866270937467));
#136436=CARTESIAN_POINT('Ctrl Pts',(-5.69568048758393,4.172899507,-4.88026301484536));
#136437=CARTESIAN_POINT('Ctrl Pts',(-5.70474773082427,4.17066314481695,
-4.86968077360362));
#136438=CARTESIAN_POINT('Ctrl Pts',(-5.71381497406465,4.1684267826339,-4.85909853236175));
#136439=CARTESIAN_POINT('',(-5.13815662914318,4.30202682605394,-5.11486524284701));
#136440=CARTESIAN_POINT('Origin',(0.156167497269551,4.16072142532751,0.122521574995526));
#136441=CARTESIAN_POINT('Ctrl Pts',(-5.31374537287912,4.26310680820188,
-5.29283573461444));
#136442=CARTESIAN_POINT('Ctrl Pts',(-5.29357464216325,4.2673677548786,-5.27241113771949));
#136443=CARTESIAN_POINT('Ctrl Pts',(-5.27341797098531,4.2716942277604,-5.25198620429076));
#136444=CARTESIAN_POINT('Ctrl Pts',(-5.25327659895758,4.27608953504662,
-5.23156110664844));
#136445=CARTESIAN_POINT('Ctrl Pts',(-5.23407932319175,4.28027881897093,
-5.21209340447583));
#136446=CARTESIAN_POINT('Ctrl Pts',(-5.21490303063397,4.28452899142244,
-5.19261799002205));
#136447=CARTESIAN_POINT('Ctrl Pts',(-5.19572324093142,4.28884908354616,
-5.17316164412882));
#136448=CARTESIAN_POINT('Ctrl Pts',(-5.1765429697024,4.29316928412982,-5.15370480976592));
#136449=CARTESIAN_POINT('Ctrl Pts',(-5.15735414107386,4.29756059498671,
-5.13427203714466));
#136450=CARTESIAN_POINT('Ctrl Pts',(-5.13815662496132,4.3020268255211,-5.11486524163069));
#136451=CARTESIAN_POINT('Ctrl Pts',(-4.5443550709688,4.17158344184794,-5.64901769170602));
#136452=CARTESIAN_POINT('Ctrl Pts',(-4.5474663194844,4.17224147442397,-5.64650919135301));
#136453=CARTESIAN_POINT('Ctrl Pts',(-4.550577568,4.172899507,-5.644000691));
#136454=CARTESIAN_POINT('Ctrl Pts',(-4.819548292,4.229787119,-5.42713818300001));
#136455=CARTESIAN_POINT('Ctrl Pts',(-5.066677286,4.285714286,-5.185680407));
#136456=CARTESIAN_POINT('Ctrl Pts',(-5.104355971,4.294241258,-5.148866388));
#136457=CARTESIAN_POINT('Ctrl Pts',(-5.14149573100001,4.302795611,-5.111508744));
#136458=CARTESIAN_POINT('Ctrl Pts',(-4.8901784459381,4.17158344184794,-5.6864948022092));
#136459=CARTESIAN_POINT('Ctrl Pts',(-4.89331014346905,4.17224147442397,
-5.6837956446046));
#136460=CARTESIAN_POINT('Ctrl Pts',(-4.896441841,4.172899507,-5.681096487));
#136461=CARTESIAN_POINT('Ctrl Pts',(-5.167180404,4.229787119,-5.447751458));
#136462=CARTESIAN_POINT('Ctrl Pts',(-5.414501802,4.285714286,-5.189717742));
#136463=CARTESIAN_POINT('Ctrl Pts',(-5.452209822,4.294241258,-5.150376461));
#136464=CARTESIAN_POINT('Ctrl Pts',(-5.48934219,4.302795611,-5.110491397));
#136465=CARTESIAN_POINT('Ctrl Pts',(-4.55057757175014,4.17289950779316,
-5.64400068797639));
#136466=CARTESIAN_POINT('Ctrl Pts',(-4.81954829372672,4.22978711939077,
-5.42713818131292));
#136467=CARTESIAN_POINT('Ctrl Pts',(-5.066677286,4.285714286,-5.185680407));
#136468=CARTESIAN_POINT('Ctrl Pts',(-5.10266266459496,4.29385804992617,
-5.15052083571143));
#136469=CARTESIAN_POINT('Ctrl Pts',(-5.13815662986677,4.3020268261311,-5.11486524162382));
#136470=CARTESIAN_POINT('Ctrl Pts',(-3.914556502,4.302796438,-6.102355889));
#136471=CARTESIAN_POINT('Ctrl Pts',(-4.24497614,4.238074114,-5.890397365));
#136472=CARTESIAN_POINT('Ctrl Pts',(-4.550577568,4.172899507,-5.64400069100001));
#136473=CARTESIAN_POINT('Ctrl Pts',(-4.56106379122528,4.17066314481382,
-5.63554598402288));
#136474=CARTESIAN_POINT('Ctrl Pts',(-4.57155001445054,4.16842678262765,
-5.62709127704577));
#136475=CARTESIAN_POINT('Ctrl Pts',(-3.84018167302776,4.302796438,-6.44288351854466));
#136476=CARTESIAN_POINT('Ctrl Pts',(-4.18903960369835,4.238074114,-6.23495211221143));
#136477=CARTESIAN_POINT('Ctrl Pts',(-4.51340635488503,4.172899507,-5.9905681197649));
#136478=CARTESIAN_POINT('Ctrl Pts',(-4.52453648010094,4.17066314481382,
-5.98218247472962));
#136479=CARTESIAN_POINT('Ctrl Pts',(-4.53566660531688,4.16842678262766,
-5.9737968296945));
#136480=CARTESIAN_POINT('',(-3.91848454918051,4.30202682597578,-6.0998343282999));
#136481=CARTESIAN_POINT('Origin',(0.126177966822555,4.1607214641731,0.153228623991858));
#136482=CARTESIAN_POINT('Ctrl Pts',(-4.0517097311445,4.26310680820184,-6.31139035819562));
#136483=CARTESIAN_POINT('Ctrl Pts',(-4.03640126539844,4.26736775488148,
-6.28710716620262));
#136484=CARTESIAN_POINT('Ctrl Pts',(-4.02110660284375,4.27169422777429,
-6.26282666784151));
#136485=CARTESIAN_POINT('Ctrl Pts',(-4.00582691709567,4.2760895350694,-6.23854929794492));
#136486=CARTESIAN_POINT('Ctrl Pts',(-3.99126344352812,4.28027881897674,
-6.21540989307706));
#136487=CARTESIAN_POINT('Ctrl Pts',(-3.9767221205835,4.28452899140062,-6.19226746695518));
#136488=CARTESIAN_POINT('Ctrl Pts',(-3.96217328298514,4.28884908352118,
-6.16914291186207));
#136489=CARTESIAN_POINT('Ctrl Pts',(-3.94762408012453,4.29316928410171,
-6.14601777620528));
#136490=CARTESIAN_POINT('Ctrl Pts',(-3.93306134734588,4.29756059496636,
-6.1229143001681));
#136491=CARTESIAN_POINT('Ctrl Pts',(-3.91848454655754,4.3020268255211,-6.09983432616156));
#136492=CARTESIAN_POINT('Ctrl Pts',(-3.22373875465859,4.17158344184793,
-6.49384880706528));
#136493=CARTESIAN_POINT('Ctrl Pts',(-3.22731651732929,4.17224147442396,
-6.49206778053264));
#136494=CARTESIAN_POINT('Ctrl Pts',(-3.23089428,4.172899507,-6.490286754));
#136495=CARTESIAN_POINT('Ctrl Pts',(-3.540195646,4.229787119,-6.336315127));
#136496=CARTESIAN_POINT('Ctrl Pts',(-3.833453187,4.285714286,-6.153627927));
#136497=CARTESIAN_POINT('Ctrl Pts',(-3.878164891,4.294241258,-6.125774403));
#136498=CARTESIAN_POINT('Ctrl Pts',(-3.922467133,4.302795611,-6.097274111));
#136499=CARTESIAN_POINT('Ctrl Pts',(-3.55342050042447,4.17158344184793,
-6.60479152680991));
#136500=CARTESIAN_POINT('Ctrl Pts',(-3.55705921971224,4.17224147442396,
-6.60282869640496));
#136501=CARTESIAN_POINT('Ctrl Pts',(-3.560697939,4.172899507,-6.600865866));
#136502=CARTESIAN_POINT('Ctrl Pts',(-3.875269069,4.229787119,-6.431177102));
#136503=CARTESIAN_POINT('Ctrl Pts',(-4.172277851,4.285714286,-6.232342861));
#136504=CARTESIAN_POINT('Ctrl Pts',(-4.217561491,4.294241258,-6.202027467));
#136505=CARTESIAN_POINT('Ctrl Pts',(-4.262399835,4.302795611,-6.171057255));
#136506=CARTESIAN_POINT('Ctrl Pts',(-3.23089458435371,4.17289956251625,
-6.49028660284023));
#136507=CARTESIAN_POINT('Ctrl Pts',(-3.54019579132273,4.22978714684626,
-6.33631503609226));
#136508=CARTESIAN_POINT('Ctrl Pts',(-3.833453187,4.285714286,-6.153627927));
#136509=CARTESIAN_POINT('Ctrl Pts',(-3.876155517,4.29385805,-6.127026159));
#136510=CARTESIAN_POINT('Ctrl Pts',(-3.91848454655754,4.3020268255211,-6.09983432616156));
#136511=CARTESIAN_POINT('Ctrl Pts',(-2.511210214,4.302796438,-6.801200134));
#136512=CARTESIAN_POINT('Ctrl Pts',(-2.879469642,4.238074114,-6.665227538));
#136513=CARTESIAN_POINT('Ctrl Pts',(-3.23089428,4.172899507,-6.49028675400001));
#136514=CARTESIAN_POINT('Ctrl Pts',(-3.24295285297228,4.17066314486295,
-6.48428394150031));
#136515=CARTESIAN_POINT('Ctrl Pts',(-3.25501142594456,4.16842678272591,
-6.47828112900057));
#136516=CARTESIAN_POINT('Ctrl Pts',(-2.36537085379952,4.302796438,-7.11777802662557));
#136517=CARTESIAN_POINT('Ctrl Pts',(-2.75077178539864,4.238074114,-6.98970208423936));
#136518=CARTESIAN_POINT('Ctrl Pts',(-3.12009035661109,4.172899507,-6.82076091693253));
#136519=CARTESIAN_POINT('Ctrl Pts',(-3.1327629312101,4.17066314486295,-6.81496397165978));
#136520=CARTESIAN_POINT('Ctrl Pts',(-3.14543550580904,4.16842678272591,
-6.80916702638693));
#136521=CARTESIAN_POINT('',(-2.5155884870915,4.30202682598825,-6.7995819405079));
#136522=CARTESIAN_POINT('Origin',(0.0902882200923827,4.16072150620521,0.176770419752994));
#136523=CARTESIAN_POINT('Ctrl Pts',(-2.60022064565508,4.26310680820217,
-7.03483138315783));
#136524=CARTESIAN_POINT('Ctrl Pts',(-2.59049025192455,4.26736775487167,
-7.00782505119042));
#136525=CARTESIAN_POINT('Ctrl Pts',(-2.58077275948663,4.27169422775182,
-6.98082431713158));
#136526=CARTESIAN_POINT('Ctrl Pts',(-2.57106922114836,4.27608953503605,
-6.95382985797731));
#136527=CARTESIAN_POINT('Ctrl Pts',(-2.56182052148295,4.28027881894382,
-6.92810072323856));
#136528=CARTESIAN_POINT('Ctrl Pts',(-2.55259410397172,4.28452899137914,
-6.90237339964067));
#136529=CARTESIAN_POINT('Ctrl Pts',(-2.5433565058699,4.2888490834871,-6.87666191378213));
#136530=CARTESIAN_POINT('Ctrl Pts',(-2.53411867584956,4.29316928405502,
-6.85094978241272));
#136531=CARTESIAN_POINT('Ctrl Pts',(-2.52486297614486,4.2975605948876,-6.82525589570485));
#136532=CARTESIAN_POINT('Ctrl Pts',(-2.51558848481664,4.30202682552139,
-6.79958193754012));
#136533=CARTESIAN_POINT('Ctrl Pts',(-1.75238399671172,4.17158344184794,
-7.03503476980878));
#136534=CARTESIAN_POINT('Ctrl Pts',(-1.75626098135586,4.17224147442397,
-7.03406449590439));
#136535=CARTESIAN_POINT('Ctrl Pts',(-1.760137966,4.172899507,-7.033094222));
#136536=CARTESIAN_POINT('Ctrl Pts',(-2.095307388,4.229787119,-6.949213017));
#136537=CARTESIAN_POINT('Ctrl Pts',(-2.420981077,4.285714286,-6.833838645));
#136538=CARTESIAN_POINT('Ctrl Pts',(-2.470635131,4.294241258,-6.816248015));
#136539=CARTESIAN_POINT('Ctrl Pts',(-2.520028332,4.302795611,-6.797937717));
#136540=CARTESIAN_POINT('Ctrl Pts',(-2.05050856186381,4.17158344184794,
-7.21425554087441));
#136541=CARTESIAN_POINT('Ctrl Pts',(-2.0544841604319,4.17224147442397,-7.2131208174372));
#136542=CARTESIAN_POINT('Ctrl Pts',(-2.058459759,4.172899507,-7.211986094));
#136543=CARTESIAN_POINT('Ctrl Pts',(-2.402154459,4.229787119,-7.11388805300001));
#136544=CARTESIAN_POINT('Ctrl Pts',(-2.734962825,4.285714286,-6.983550554));
#136545=CARTESIAN_POINT('Ctrl Pts',(-2.785704672,4.294241258,-6.963678562));
#136546=CARTESIAN_POINT('Ctrl Pts',(-2.836152401,4.302795611,-6.943071335));
#136547=CARTESIAN_POINT('Ctrl Pts',(-1.76013829606613,4.17289956297316,
-7.03309413963776));
#136548=CARTESIAN_POINT('Ctrl Pts',(-1.90457922844313,4.19741522351749,
-6.99694560958115));
#136549=CARTESIAN_POINT('Ctrl Pts',(-2.04761672121439,4.22178368138733,
-6.9564156254032));
#136550=CARTESIAN_POINT('Ctrl Pts',(-2.18886678551531,4.24593817209426,
-6.91168302222974));
#136551=CARTESIAN_POINT('Ctrl Pts',(-2.26680221137891,4.25926553253887,
-6.88700158583135));
#136552=CARTESIAN_POINT('Ctrl Pts',(-2.34419392029766,4.27252781042464,
-6.8610415487873));
#136553=CARTESIAN_POINT('Ctrl Pts',(-2.42098107728448,4.28571428600471,
-6.83383864511283));
#136554=CARTESIAN_POINT('Ctrl Pts',(-2.45257142201105,4.29113922038427,
-6.82264733202966));
#136555=CARTESIAN_POINT('Ctrl Pts',(-2.48410884525471,4.2965769796734,-6.81122821862746));
#136556=CARTESIAN_POINT('Ctrl Pts',(-2.51558848703189,4.30202682577276,
-6.79958194024593));
#136557=CARTESIAN_POINT('Ctrl Pts',(-0.990442528,4.302796438,-7.182027819));
#136558=CARTESIAN_POINT('Ctrl Pts',(-1.379322344,4.238074114,-7.12839907900001));
#136559=CARTESIAN_POINT('Ctrl Pts',(-1.760137966,4.172899507,-7.033094222));
#136560=CARTESIAN_POINT('Ctrl Pts',(-1.77320504385938,4.17066314479498,
-7.0298239885462));
#136561=CARTESIAN_POINT('Ctrl Pts',(-1.7862721217187,4.16842678258996,-7.02655375509242));
#136562=CARTESIAN_POINT('Ctrl Pts',(-0.779957921281984,4.302796438,-7.45985314610527));
#136563=CARTESIAN_POINT('Ctrl Pts',(-1.1838809356057,4.238074114,-7.41762135551125));
#136564=CARTESIAN_POINT('Ctrl Pts',(-1.58088240025405,4.172899507,-7.33202251416165));
#136565=CARTESIAN_POINT('Ctrl Pts',(-1.59450486936809,4.17066314479498,
-7.32908532708222));
#136566=CARTESIAN_POINT('Ctrl Pts',(-1.60812733848218,4.16842678258996,
-7.32614814000278));
#136567=CARTESIAN_POINT('',(-0.995066304014444,4.30202682608954,-7.18138865763276));
#136568=CARTESIAN_POINT('Origin',(0.0501768802110265,4.16072148901941,0.192046736180631));
#136569=CARTESIAN_POINT('Ctrl Pts',(-1.02714813235652,4.26310680820184,
-7.42933151192896));
#136570=CARTESIAN_POINT('Ctrl Pts',(-1.02345079285982,4.26736775487571,
-7.40086482582209));
#136571=CARTESIAN_POINT('Ctrl Pts',(-1.01976484971036,4.27169422776037,
-7.37240638024215));
#136572=CARTESIAN_POINT('Ctrl Pts',(-1.0160911854935,4.2760895350484,-7.34395706258297));
#136573=CARTESIAN_POINT('Ctrl Pts',(-1.01258971872643,4.28027881895993,
-7.31684126362888));
#136574=CARTESIAN_POINT('Ctrl Pts',(-1.00910962384362,4.28452899139447,
-7.28973202347391));
#136575=CARTESIAN_POINT('Ctrl Pts',(-1.00561520513928,4.28884908349595,
-7.26263584728086));
#136576=CARTESIAN_POINT('Ctrl Pts',(-1.00212069870427,4.29316928405743,
-7.2355389908128));
#136577=CARTESIAN_POINT('Ctrl Pts',(-0.998604818079791,4.2975605949177,
-7.20845611103672));
#136578=CARTESIAN_POINT('Ctrl Pts',(-0.995066302196107,4.3020268255211,
-7.18138865409593));
#136579=CARTESIAN_POINT('Ctrl Pts',(-0.199089711805015,4.17158344184793,
-7.24727032571477));
#136580=CARTESIAN_POINT('Ctrl Pts',(-0.203084634902507,4.17224147442396,
-7.24715617335739));
#136581=CARTESIAN_POINT('Ctrl Pts',(-0.207079558,4.172899507,-7.247042021));
#136582=CARTESIAN_POINT('Ctrl Pts',(-0.552444884,4.229787119,-7.237173429));
#136583=CARTESIAN_POINT('Ctrl Pts',(-0.895306583,4.285714286,-7.194506663));
#136584=CARTESIAN_POINT('Ctrl Pts',(-0.947581218,4.294241258,-7.188001446));
#136585=CARTESIAN_POINT('Ctrl Pts',(-0.999755805999999,4.302795611,-7.180737311));
#136586=CARTESIAN_POINT('Ctrl Pts',(-0.451717121439883,4.17158344184793,
-7.48638898311077));
#136587=CARTESIAN_POINT('Ctrl Pts',(-0.455843704719942,4.17224147442396,
-7.48613542505538));
#136588=CARTESIAN_POINT('Ctrl Pts',(-0.459970288,4.172899507,-7.48588186700001));
#136589=CARTESIAN_POINT('Ctrl Pts',(-0.816717776000001,4.229787119,-7.46396150500001));
#136590=CARTESIAN_POINT('Ctrl Pts',(-1.169763977,4.285714286,-7.408215186));
#136591=CARTESIAN_POINT('Ctrl Pts',(-1.223591399,4.294241258,-7.399715786));
#136592=CARTESIAN_POINT('Ctrl Pts',(-1.277289632,4.302795611,-7.390435115));
#136593=CARTESIAN_POINT('Ctrl Pts',(-0.20707956336158,4.17289950774601,
-7.24704202165685));
#136594=CARTESIAN_POINT('Ctrl Pts',(-0.21998723992398,4.17502562418936,
-7.24667319304932));
#136595=CARTESIAN_POINT('Ctrl Pts',(-0.223993995176412,4.17568534804455,
-7.24654324800825));
#136596=CARTESIAN_POINT('Ctrl Pts',(-0.240155571671878,4.17834651451532,
-7.24602606710527));
#136597=CARTESIAN_POINT('Ctrl Pts',(-0.248424773146666,4.17970788561247,
-7.2457472766494));
#136598=CARTESIAN_POINT('Ctrl Pts',(-0.273224914126765,4.18379006147442,
-7.24486865177658));
#136599=CARTESIAN_POINT('Ctrl Pts',(-0.289754454797499,4.18650992776272,
-7.24422639100457));
#136600=CARTESIAN_POINT('Ctrl Pts',(-0.339310807627244,4.1946613842195,
-7.24213097367978));
#136601=CARTESIAN_POINT('Ctrl Pts',(-0.372330709975183,4.20008900922057,
-7.2405084644347));
#136602=CARTESIAN_POINT('Ctrl Pts',(-0.471242108456474,4.21633619398169,
-7.23496977729559));
#136603=CARTESIAN_POINT('Ctrl Pts',(-0.537095577453983,4.22713823046721,
-7.23037939677633));
#136604=CARTESIAN_POINT('Ctrl Pts',(-0.73404881608325,4.25939962768096,
-7.2139446275718));
#136605=CARTESIAN_POINT('Ctrl Pts',(-0.864780427711907,4.28067054765987,
-7.19944130409139));
#136606=CARTESIAN_POINT('Ctrl Pts',(-0.995066304340255,4.3020268256754,
-7.18138865949419));
#136607=CARTESIAN_POINT('Ctrl Pts',(0.57663715,4.302796438,-7.227031866));
#136608=CARTESIAN_POINT('Ctrl Pts',(0.185320533,4.238074114,-7.25825460100001));
#136609=CARTESIAN_POINT('Ctrl Pts',(-0.207079558,4.172899507,-7.247042021));
#136610=CARTESIAN_POINT('Ctrl Pts',(-0.220544138690441,4.1706631447385,
-7.24665727927435));
#136611=CARTESIAN_POINT('Ctrl Pts',(-0.234008719380881,4.16842678247702,
-7.24627253754872));
#136612=CARTESIAN_POINT('Ctrl Pts',(0.841924975632872,4.302796438,-7.45311382237723));
#136613=CARTESIAN_POINT('Ctrl Pts',(0.438366870732096,4.238074114,-7.49870089635587));
#136614=CARTESIAN_POINT('Ctrl Pts',(0.0322458591927978,4.172899507,-7.50044688815672));
#136615=CARTESIAN_POINT('Ctrl Pts',(0.0183104670882274,4.1706631447385,
-7.50050679906916));
#136616=CARTESIAN_POINT('Ctrl Pts',(0.00437507498365682,4.16842678247702,
-7.50056670998151));
#136617=CARTESIAN_POINT('',(0.571984074783619,4.30202682599323,-7.22740162258272));
#136618=CARTESIAN_POINT('Origin',(0.00771940334921756,4.16072144823275,
0.198343469846251));
#136619=CARTESIAN_POINT('Ctrl Pts',(0.593952685418298,4.26310680820187,
-7.47644435599597));
#136620=CARTESIAN_POINT('Ctrl Pts',(0.59144408727556,4.26736775488579,-7.44784838639655));
#136621=CARTESIAN_POINT('Ctrl Pts',(0.588926130551418,4.27169422777635,
-7.41926291457612));
#136622=CARTESIAN_POINT('Ctrl Pts',(0.586398144197795,4.27608953506819,
-7.39068899687837));
#136623=CARTESIAN_POINT('Ctrl Pts',(0.583988653383373,4.28027881897436,
-7.3634544383824));
#136624=CARTESIAN_POINT('Ctrl Pts',(0.581559700274735,4.2845289913987,-7.33623087966888));
#136625=CARTESIAN_POINT('Ctrl Pts',(0.579147544540272,4.28884908349961,
-7.30901700028622));
#136626=CARTESIAN_POINT('Ctrl Pts',(0.576735328246355,4.29316928406052,
-7.28180243767334));
#136627=CARTESIAN_POINT('Ctrl Pts',(0.574346991003685,4.29756059491905,
-7.25459693016561));
#136628=CARTESIAN_POINT('Ctrl Pts',(0.571984075604951,4.30202682552139,
-7.22740161874865));
#136629=CARTESIAN_POINT('Ctrl Pts',(1.36351378779211,4.17158344184794,-7.120631576332));
#136630=CARTESIAN_POINT('Ctrl Pts',(1.35958772439605,4.17224147442397,-7.121378883166));
#136631=CARTESIAN_POINT('Ctrl Pts',(1.355661661,4.172899507,-7.12212619));
#136632=CARTESIAN_POINT('Ctrl Pts',(1.016249329,4.229787119,-7.186731656));
#136633=CARTESIAN_POINT('Ctrl Pts',(0.672231452,4.285714286,-7.218767545));
#136634=CARTESIAN_POINT('Ctrl Pts',(0.619780539,4.294241258,-7.223651918));
#136635=CARTESIAN_POINT('Ctrl Pts',(0.56726419,4.302795611,-7.227773609));
#136636=CARTESIAN_POINT('Ctrl Pts',(1.16819610908937,4.17158344184794,-7.40846719817912));
#136637=CARTESIAN_POINT('Ctrl Pts',(1.16411149554469,4.17224147442397,-7.40910666158956));
#136638=CARTESIAN_POINT('Ctrl Pts',(1.160026882,4.172899507,-7.409746125));
#136639=CARTESIAN_POINT('Ctrl Pts',(0.806907722,4.229787119,-7.465028413));
#136640=CARTESIAN_POINT('Ctrl Pts',(0.450131734,4.285714286,-7.486479909));
#136641=CARTESIAN_POINT('Ctrl Pts',(0.395735648,4.294241258,-7.489750525));
#136642=CARTESIAN_POINT('Ctrl Pts',(0.34129778,4.302795611,-7.492230364));
#136643=CARTESIAN_POINT('Ctrl Pts',(1.35566132646284,4.1728995630705,-7.1221262536775));
#136644=CARTESIAN_POINT('Ctrl Pts',(1.20939187737991,4.19741522958354,-7.14996791590427));
#136645=CARTESIAN_POINT('Ctrl Pts',(1.06255643070428,4.2217836932938,-7.17324378695403));
#136646=CARTESIAN_POINT('Ctrl Pts',(0.915578576336522,4.24593818969773,
-7.19195494056951));
#136647=CARTESIAN_POINT('Ctrl Pts',(0.834482868858626,4.25926554423746,
-7.20227890567774));
#136648=CARTESIAN_POINT('Ctrl Pts',(0.753343755120934,4.27252781626317,
-7.21121414472586));
#136649=CARTESIAN_POINT('Ctrl Pts',(0.672231451661361,4.28571428604748,
-7.21876754508335));
#136650=CARTESIAN_POINT('Ctrl Pts',(0.638861721101172,4.29113922036799,
-7.22187502600129));
#136651=CARTESIAN_POINT('Ctrl Pts',(0.605444369423189,4.29657697969623,
-7.22475354016177));
#136652=CARTESIAN_POINT('Ctrl Pts',(0.571984074806843,4.302026825889,-7.22740162309087));
#136653=CARTESIAN_POINT('Ctrl Pts',(2.116753915,4.302796438,-6.934107936));
#136654=CARTESIAN_POINT('Ctrl Pts',(1.741298029,4.238074114,-7.048722205));
#136655=CARTESIAN_POINT('Ctrl Pts',(1.355661661,4.172899507,-7.12212619));
#136656=CARTESIAN_POINT('Ctrl Pts',(1.34242916693796,4.17066314479019,-7.12464493012992));
#136657=CARTESIAN_POINT('Ctrl Pts',(1.32919667287593,4.16842678258039,-7.12716367025997));
#136658=CARTESIAN_POINT('Ctrl Pts',(2.42444039675729,4.302796438,-7.09787518030707));
#136659=CARTESIAN_POINT('Ctrl Pts',(2.04011712962238,4.238074114,-7.22914951711653));
#136660=CARTESIAN_POINT('Ctrl Pts',(1.64386633789201,4.172899507,-7.31815870169129));
#136661=CARTESIAN_POINT('Ctrl Pts',(1.63026962688718,4.17066314479019,-7.32121290924037));
#136662=CARTESIAN_POINT('Ctrl Pts',(1.61667291588234,4.16842678258039,-7.32426711678959));
#136663=CARTESIAN_POINT('',(2.11228911235521,4.30202682605736,-6.93546932111101));
#136664=CARTESIAN_POINT('Origin',(-0.035099148622541,4.16072145763487,0.195366131088097));
#136665=CARTESIAN_POINT('Ctrl Pts',(2.1872809357983,4.26310680658203,-7.17396697110051));
#136666=CARTESIAN_POINT('Ctrl Pts',(2.17868369939943,4.26736775489131,-7.14657883414244));
#136667=CARTESIAN_POINT('Ctrl Pts',(2.17007957965209,4.27169422777959,-7.11920296110774));
#136668=CARTESIAN_POINT('Ctrl Pts',(2.16146814827941,4.27608953521548,-7.09184052727085));
#136669=CARTESIAN_POINT('Ctrl Pts',(2.15525374053094,4.27926139264596,-7.07209452762295));
#136670=CARTESIAN_POINT('Ctrl Pts',(2.14903015416925,4.28246998646097,-7.05235727007208));
#136671=CARTESIAN_POINT('Ctrl Pts',(2.14281165749886,4.285714286,-7.03262430918845));
#136672=CARTESIAN_POINT('Ctrl Pts',(2.14081697072266,4.28675494926488,-7.02629463208906));
#136673=CARTESIAN_POINT('Ctrl Pts',(2.13882292648665,4.28779988860438,-7.01996545799532));
#136674=CARTESIAN_POINT('Ctrl Pts',(2.13683000013097,4.28884908283037,-7.01363664650976));
#136675=CARTESIAN_POINT('Ctrl Pts',(2.12862385216706,4.2931692841448,-6.98757689606371));
#136676=CARTESIAN_POINT('Ctrl Pts',(2.12044297297646,4.29756059502454,-6.96152086016398));
#136677=CARTESIAN_POINT('Ctrl Pts',(2.11228911061973,4.30202682639742,-6.93546932209822));
#136678=CARTESIAN_POINT('Ctrl Pts',(2.86236089767707,4.17158344184794,-6.66104000740502));
#136679=CARTESIAN_POINT('Ctrl Pts',(2.85868727233853,4.17224147442397,-6.66261383020251));
#136680=CARTESIAN_POINT('Ctrl Pts',(2.855013647,4.172899507,-6.664187653));
#136681=CARTESIAN_POINT('Ctrl Pts',(2.537424852,4.229787119,-6.800246298));
#136682=CARTESIAN_POINT('Ctrl Pts',(2.208336691,4.285714286,-6.905486881));
#136683=CARTESIAN_POINT('Ctrl Pts',(2.158162048,4.294241258,-6.92153245500001));
#136684=CARTESIAN_POINT('Ctrl Pts',(2.107759543,4.302795611,-6.936847246));
#136685=CARTESIAN_POINT('Ctrl Pts',(2.73348578762687,4.17158344184794,-6.98413372045932));
#136686=CARTESIAN_POINT('Ctrl Pts',(2.72963413581344,4.17224147442397,-6.98563630472967));
#136687=CARTESIAN_POINT('Ctrl Pts',(2.725782484,4.172899507,-6.987138889));
#136688=CARTESIAN_POINT('Ctrl Pts',(2.392803112,4.229787119,-7.117038888));
#136689=CARTESIAN_POINT('Ctrl Pts',(2.048979786,4.285714286,-7.214685152));
#136690=CARTESIAN_POINT('Ctrl Pts',(1.996558536,4.294241258,-7.229572853));
#136691=CARTESIAN_POINT('Ctrl Pts',(1.943926487,4.302795611,-7.243697248));
#136692=CARTESIAN_POINT('Ctrl Pts',(2.85501333397931,4.17289956286129,-6.66418778679595));
#136693=CARTESIAN_POINT('Ctrl Pts',(2.53742468986878,4.22978714683597,-6.80024635016384));
#136694=CARTESIAN_POINT('Ctrl Pts',(2.208336691,4.285714286,-6.905486881));
#136695=CARTESIAN_POINT('Ctrl Pts',(2.16041693,4.29385805,-6.920811357));
#136696=CARTESIAN_POINT('Ctrl Pts',(2.11228911319059,4.30202682552139,-6.93546931684795));
#136697=CARTESIAN_POINT('Ctrl Pts',(3.55789362,4.302796438,-6.316952824));
#136698=CARTESIAN_POINT('Ctrl Pts',(3.215854364,4.238074114,-6.509599393));
#136699=CARTESIAN_POINT('Ctrl Pts',(2.855013647,4.172899507,-6.664187653));
#136700=CARTESIAN_POINT('Ctrl Pts',(2.84263197655568,4.17066314489563,-6.66949210119473));
#136701=CARTESIAN_POINT('Ctrl Pts',(2.83025030611137,4.16842678279126,-6.67479654938961));
#136702=CARTESIAN_POINT('Ctrl Pts',(3.8935916797487,4.302796438,-6.41074778369885));
#136703=CARTESIAN_POINT('Ctrl Pts',(3.54647377862577,4.238074114,-6.62157114079839));
#136704=CARTESIAN_POINT('Ctrl Pts',(3.17862145369182,4.172899507,-6.79368154768867));
#136705=CARTESIAN_POINT('Ctrl Pts',(3.16599919116732,4.17066314489563,-6.79958724024984));
#136706=CARTESIAN_POINT('Ctrl Pts',(3.15337692864277,4.16842678279128,-6.80549293281101));
#136707=CARTESIAN_POINT('',(3.55382586057344,4.30202682596346,-6.31924218176628));
#136708=CARTESIAN_POINT('Origin',(-0.0762763638463032,4.16072146698572,
0.183253025037982));
#136709=CARTESIAN_POINT('Ctrl Pts',(3.67833436109219,4.26310680820193,-6.53604286415009));
#136710=CARTESIAN_POINT('Ctrl Pts',(3.66405048306734,4.26736775486722,-6.51114319839327));
#136711=CARTESIAN_POINT('Ctrl Pts',(3.64976251940713,4.2716942277443,-6.48625698950045));
#136712=CARTESIAN_POINT('Ctrl Pts',(3.63547030455461,4.27608953502506,-6.46138547817639));
#136713=CARTESIAN_POINT('Ctrl Pts',(3.62184801560651,4.28027881894025,-6.4376797812408));
#136714=CARTESIAN_POINT('Ctrl Pts',(3.60821268185684,4.28452899137762,-6.41399223943781));
#136715=CARTESIAN_POINT('Ctrl Pts',(3.59459665732802,4.28884908351028,-6.39030642927422));
#136716=CARTESIAN_POINT('Ctrl Pts',(3.5809802909561,4.2931692841029,-6.36662002445608));
#136717=CARTESIAN_POINT('Ctrl Pts',(3.56738939858886,4.29756059496313,-6.34293181137133));
#136718=CARTESIAN_POINT('Ctrl Pts',(3.55382585953241,4.30202682552139,-6.31924217758476));
#136719=CARTESIAN_POINT('Ctrl Pts',(4.22736719328809,4.17158344184794,-5.8899856118872));
#136720=CARTESIAN_POINT('Ctrl Pts',(4.22411778064405,4.17224147442397,-5.8923123604436));
#136721=CARTESIAN_POINT('Ctrl Pts',(4.220868368,4.172899507,-5.89463910900001));
#136722=CARTESIAN_POINT('Ctrl Pts',(3.939953209,4.229787119,-6.095788982));
#136723=CARTESIAN_POINT('Ctrl Pts',(3.641182561,4.285714286,-6.269313324));
#136724=CARTESIAN_POINT('Ctrl Pts',(3.595630297,4.294241258,-6.29576982800001));
#136725=CARTESIAN_POINT('Ctrl Pts',(3.549698402,4.302795611,-6.321561615));
#136726=CARTESIAN_POINT('Ctrl Pts',(4.17096070925658,4.17158344184794,-6.23322991204395));
#136727=CARTESIAN_POINT('Ctrl Pts',(4.16752211812829,4.17224147442397,-6.23552535802198));
#136728=CARTESIAN_POINT('Ctrl Pts',(4.164083527,4.172899507,-6.237820804));
#136729=CARTESIAN_POINT('Ctrl Pts',(3.866813688,4.229787119,-6.436264536));
#136730=CARTESIAN_POINT('Ctrl Pts',(3.55201982,4.285714286,-6.605539735));
#136731=CARTESIAN_POINT('Ctrl Pts',(3.504024566,4.294241258,-6.63134839));
#136732=CARTESIAN_POINT('Ctrl Pts',(3.455659352,4.302795611,-6.656456899));
#136733=CARTESIAN_POINT('Ctrl Pts',(4.22086836419622,4.17289950772743,-5.89463911285146));
#136734=CARTESIAN_POINT('Ctrl Pts',(4.21036944622223,4.17502562429124,-5.90215688440212));
#136735=CARTESIAN_POINT('Ctrl Pts',(4.20710105665032,4.175685348168,-5.90447822109222));
#136736=CARTESIAN_POINT('Ctrl Pts',(4.19392195323513,4.17834651461355,-5.91384706622864));
#136737=CARTESIAN_POINT('Ctrl Pts',(4.18717018248245,4.17970788571012,-5.91862943058245));
#136738=CARTESIAN_POINT('Ctrl Pts',(4.16689524109046,4.18379006157001,-5.9329383692362));
#136739=CARTESIAN_POINT('Ctrl Pts',(4.15334750871452,4.18650992785742,-5.94243032167265));
#136740=CARTESIAN_POINT('Ctrl Pts',(4.11262794730963,4.1946613843096,-5.97075240133703));
#136741=CARTESIAN_POINT('Ctrl Pts',(4.08535913123871,4.20008900930932,-5.98944352643003));
#136742=CARTESIAN_POINT('Ctrl Pts',(4.00326457661388,4.21633619514749,-6.04489284753308));
#136743=CARTESIAN_POINT('Ctrl Pts',(3.94806110930445,4.22713823109094,-6.08109129674243));
#136744=CARTESIAN_POINT('Ctrl Pts',(3.78132209108869,4.25939963061046,-6.18719871994207));
#136745=CARTESIAN_POINT('Ctrl Pts',(3.66847050410133,4.28067055425272,-6.25476813660489));
#136746=CARTESIAN_POINT('Ctrl Pts',(3.55382586154031,4.3020268255718,-6.31924218361524));
#136747=CARTESIAN_POINT('Ctrl Pts',(4.832670174,4.302796438,-5.40442402));
#136748=CARTESIAN_POINT('Ctrl Pts',(4.540040923,4.238074114,-5.666094949));
#136749=CARTESIAN_POINT('Ctrl Pts',(4.220868368,4.172899507,-5.894639109));
#136750=CARTESIAN_POINT('Ctrl Pts',(4.20991647333625,4.17066314482088,-5.90248123554604));
#136751=CARTESIAN_POINT('Ctrl Pts',(4.19896457867244,4.16842678264175,-5.91032336209221));
#136752=CARTESIAN_POINT('Ctrl Pts',(5.18068294323162,4.302796438,-5.42386094580911));
#136753=CARTESIAN_POINT('Ctrl Pts',(4.88700125593113,4.238074114,-5.7043754577779));
#136754=CARTESIAN_POINT('Ctrl Pts',(4.56474776398164,4.172899507,-5.95153939466388));
#136755=CARTESIAN_POINT('Ctrl Pts',(4.55369015190452,4.17066314482088,-5.96002042901051));
#136756=CARTESIAN_POINT('Ctrl Pts',(4.54263253982728,4.16842678264174,-5.96850146335713));
#136757=CARTESIAN_POINT('',(4.82918966053496,4.30202682607914,-5.4075343008958));
#136758=CARTESIAN_POINT('Origin',(-0.113887094330756,4.16072143125059,0.162571574944076));
#136759=CARTESIAN_POINT('Ctrl Pts',(4.99739295987823,4.26310680820187,-5.5925006574533));
#136760=CARTESIAN_POINT('Ctrl Pts',(4.97809033885805,4.26736775488714,-5.57125374342459));
#136761=CARTESIAN_POINT('Ctrl Pts',(4.9587866205154,4.27169422777249,-5.55002085012781));
#136762=CARTESIAN_POINT('Ctrl Pts',(4.93948190990831,4.27608953505775,-5.52880322466369));
#136763=CARTESIAN_POINT('Ctrl Pts',(4.92108207837028,4.28027881897154,-5.50858014325509));
#136764=CARTESIAN_POINT('Ctrl Pts',(4.90267340981735,4.28452899140277,-5.48837759677755));
#136765=CARTESIAN_POINT('Ctrl Pts',(4.88428397121445,4.2888490835086,-5.46817259061411));
#136766=CARTESIAN_POINT('Ctrl Pts',(4.8658940709274,4.29316928407441,-5.44796707718501));
#136767=CARTESIAN_POINT('Ctrl Pts',(4.84752866049303,4.29756059493458,-5.42775432148553));
#136768=CARTESIAN_POINT('Ctrl Pts',(4.82918965923875,4.3020268255211,-5.40753429774623));
#136769=CARTESIAN_POINT('Ctrl Pts',(5.39470649704281,4.17158344184794,-4.84352203473393));
#136770=CARTESIAN_POINT('Ctrl Pts',(5.39203323602141,4.17224147442397,-4.84649291286697));
#136771=CARTESIAN_POINT('Ctrl Pts',(5.389359975,4.172899507,-4.849463791));
#136772=CARTESIAN_POINT('Ctrl Pts',(5.158253733,4.229787119,-5.106299347));
#136773=CARTESIAN_POINT('Ctrl Pts',(4.903770781,4.285714286,-5.339993645));
#136774=CARTESIAN_POINT('Ctrl Pts',(4.86497087,4.294241258,-5.37562400000001));
#136775=CARTESIAN_POINT('Ctrl Pts',(4.825657309,4.302795611,-5.41068678999999));
#136776=CARTESIAN_POINT('Ctrl Pts',(5.41340614349393,4.17158344184794,-5.19086720064895));
#136777=CARTESIAN_POINT('Ctrl Pts',(5.41054139774697,4.17224147442397,-5.19384817582448));
#136778=CARTESIAN_POINT('Ctrl Pts',(5.40767665200001,4.172899507,-5.196829151));
#136779=CARTESIAN_POINT('Ctrl Pts',(5.160016353,4.229787119,-5.454537607));
#136780=CARTESIAN_POINT('Ctrl Pts',(4.888971356,4.285714286,-5.687526623));
#136781=CARTESIAN_POINT('Ctrl Pts',(4.847646301,4.294241258,-5.723049447));
#136782=CARTESIAN_POINT('Ctrl Pts',(4.805809426,4.302795611,-5.75796802300001));
#136783=CARTESIAN_POINT('Ctrl Pts',(5.389359747424,4.17289956286129,-4.84946404403705));
#136784=CARTESIAN_POINT('Ctrl Pts',(5.15825360814972,4.22978714684751,-5.10629946169107));
#136785=CARTESIAN_POINT('Ctrl Pts',(4.903770781,4.285714286,-5.339993645));
#136786=CARTESIAN_POINT('Ctrl Pts',(4.866714564,4.29385805,-5.374022748));
#136787=CARTESIAN_POINT('Ctrl Pts',(4.82918965923875,4.3020268255211,-5.40753429774623));
#136788=CARTESIAN_POINT('Ctrl Pts',(5.881476442,4.302796438,-4.239190355));
#136789=CARTESIAN_POINT('Ctrl Pts',(5.651940215,4.238074114,-4.557650202));
#136790=CARTESIAN_POINT('Ctrl Pts',(5.389359975,4.172899507,-4.84946379100001));
#136791=CARTESIAN_POINT('Ctrl Pts',(5.38034995519343,4.17066314488853,-4.85947690629275));
#136792=CARTESIAN_POINT('Ctrl Pts',(5.37133993538672,4.16842678277707,-4.86949002158551));
#136793=CARTESIAN_POINT('Ctrl Pts',(6.22553122981452,4.302796438,-4.18336039794204));
#136794=CARTESIAN_POINT('Ctrl Pts',(5.99901798618111,4.238074114,-4.52044951809392));
#136795=CARTESIAN_POINT('Ctrl Pts',(5.73743154150416,4.172899507,-4.83110987552454));
#136796=CARTESIAN_POINT('Ctrl Pts',(5.7284556221902,4.17066314488853,-4.84176968744937));
#136797=CARTESIAN_POINT('Ctrl Pts',(5.71947970287635,4.16842678277705,-4.85242949937412));
#136798=CARTESIAN_POINT('',(5.87874591915956,4.30202682596213,-4.242976127138));
#136799=CARTESIAN_POINT('Origin',(-0.146172589532412,4.16072141476489,0.134288418613644));
#136800=CARTESIAN_POINT('Ctrl Pts',(6.08277901778227,4.26310680820167,-4.38745933518201));
#136801=CARTESIAN_POINT('Ctrl Pts',(6.05936022279369,4.26736775488834,-4.37085865528994));
#136802=CARTESIAN_POINT('Ctrl Pts',(6.03594337023099,4.2716942277768,-4.35427190405316));
#136803=CARTESIAN_POINT('Ctrl Pts',(6.01252883073701,4.27608953506782,-4.33770027700124));
#136804=CARTESIAN_POINT('Ctrl Pts',(5.99021181229749,4.28027881899059,-4.32190541985338));
#136805=CARTESIAN_POINT('Ctrl Pts',(5.96789057786926,4.28452899143785,-4.30613251721398));
#136806=CARTESIAN_POINT('Ctrl Pts',(5.94558759502439,4.28884908355563,-4.2903530785531));
#136807=CARTESIAN_POINT('Ctrl Pts',(5.92328405224215,4.29316928413338,-4.27457324373456));
#136808=CARTESIAN_POINT('Ctrl Pts',(5.90100286981083,4.29756059498866,-4.25878107146336));
#136809=CARTESIAN_POINT('Ctrl Pts',(5.87874591645362,4.30202682552206,-4.24297612382547));
#136810=CARTESIAN_POINT('Ctrl Pts',(6.30979532136944,4.17158344184794,-3.57058075049655));
#136811=CARTESIAN_POINT('Ctrl Pts',(6.30782321068473,4.17224147442397,-3.57405684324828));
#136812=CARTESIAN_POINT('Ctrl Pts',(6.3058511,4.172899507,-3.577532936));
#136813=CARTESIAN_POINT('Ctrl Pts',(6.135360046,4.229787119,-3.87804483));
#136814=CARTESIAN_POINT('Ctrl Pts',(5.93706413,4.285714286,-4.160981797));
#136815=CARTESIAN_POINT('Ctrl Pts',(5.906830812,4.294241258,-4.204119968));
#136816=CARTESIAN_POINT('Ctrl Pts',(5.875973844,4.302795611,-4.246814263));
#136817=CARTESIAN_POINT('Ctrl Pts',(6.40272672408439,4.17158344184794,-3.90578530842664));
#136818=CARTESIAN_POINT('Ctrl Pts',(6.4005697760422,4.17224147442397,-3.90931242571332));
#136819=CARTESIAN_POINT('Ctrl Pts',(6.398412828,4.172899507,-3.912839543));
#136820=CARTESIAN_POINT('Ctrl Pts',(6.211942389,4.229787119,-4.217762562));
#136821=CARTESIAN_POINT('Ctrl Pts',(5.997320024,4.285714286,-4.503571086));
#136822=CARTESIAN_POINT('Ctrl Pts',(5.964597484,4.294241258,-4.547147072));
#136823=CARTESIAN_POINT('Ctrl Pts',(5.931245193,4.302795611,-4.590242963));
#136824=CARTESIAN_POINT('Ctrl Pts',(6.30585109805129,4.17289950775651,-3.57753294115029));
#136825=CARTESIAN_POINT('Ctrl Pts',(6.29947916846551,4.17502562433408,-3.58876426714043));
#136826=CARTESIAN_POINT('Ctrl Pts',(6.29748756240345,4.17568534821138,-3.59224341642849));
#136827=CARTESIAN_POINT('Ctrl Pts',(6.28946040807777,4.17834651465004,-3.60628011185563));
#136828=CARTESIAN_POINT('Ctrl Pts',(6.28534072957839,4.17970788574548,-3.6134554631478));
#136829=CARTESIAN_POINT('Ctrl Pts',(6.27294785853963,4.1837900616024,-3.63495513108321));
#136830=CARTESIAN_POINT('Ctrl Pts',(6.26463783703034,4.18650992788744,-3.64925833897672));
#136831=CARTESIAN_POINT('Ctrl Pts',(6.23957389659969,4.19466138433422,-3.69206046238253));
#136832=CARTESIAN_POINT('Ctrl Pts',(6.22267358914811,4.20008900932887,-3.72047394676422));
#136833=CARTESIAN_POINT('Ctrl Pts',(6.17144914928316,4.21633619694954,-3.80526900580106));
#136834=CARTESIAN_POINT('Ctrl Pts',(6.13654717623975,4.2271382319934,-3.86130115791271));
#136835=CARTESIAN_POINT('Ctrl Pts',(6.02977230827358,4.25939962672662,-4.02761351906478));
#136836=CARTESIAN_POINT('Ctrl Pts',(5.95572265761057,4.28067054646697,-4.13632299277107));
#136837=CARTESIAN_POINT('Ctrl Pts',(5.87874592074033,4.30202682557444,-4.24297612835655));
#136838=CARTESIAN_POINT('Ctrl Pts',(6.655271408,4.302796438,-2.87573686));
#136839=CARTESIAN_POINT('Ctrl Pts',(6.499561064,4.238074114,-3.236094797));
#136840=CARTESIAN_POINT('Ctrl Pts',(6.30585110000001,4.172899507,-3.577532936));
#136841=CARTESIAN_POINT('Ctrl Pts',(6.29920425302589,4.17066314480995,-3.58924883854929));
#136842=CARTESIAN_POINT('Ctrl Pts',(6.29255740605191,4.16842678261991,-3.60096474109857));
#136843=CARTESIAN_POINT('Ctrl Pts',(6.97928059608469,4.302796438,-2.74725056763748));
#136844=CARTESIAN_POINT('Ctrl Pts',(6.83052730232644,4.238074114,-3.12515238362164));
#136845=CARTESIAN_POINT('Ctrl Pts',(6.64183939664013,4.172899507,-3.48478302660876));
#136846=CARTESIAN_POINT('Ctrl Pts',(6.63536487354871,4.17066314480995,-3.49712317577696));
#136847=CARTESIAN_POINT('Ctrl Pts',(6.62889035045719,4.16842678261991,-3.50946332494515));
#136848=CARTESIAN_POINT('',(6.65341855241806,4.30202682601949,-2.88002110588503));
#136849=CARTESIAN_POINT('Origin',(-0.171623230891431,4.16072138151534,0.0997260640717268));
#136850=CARTESIAN_POINT('Ctrl Pts',(6.88374108930325,4.26310680659847,-2.97726529110235));
#136851=CARTESIAN_POINT('Ctrl Pts',(6.85730115750649,4.26736775493315,-2.96608707433597));
#136852=CARTESIAN_POINT('Ctrl Pts',(6.83086611675001,4.27169422781411,-2.95492204319667));
#136853=CARTESIAN_POINT('Ctrl Pts',(6.80443658539477,4.27608953524134,-2.94377128502033));
#136854=CARTESIAN_POINT('Ctrl Pts',(6.7853638114032,4.27926139266311,-2.93572438143837));
#136855=CARTESIAN_POINT('Ctrl Pts',(6.76629175820736,4.28246998646359,-2.92769013290502));
#136856=CARTESIAN_POINT('Ctrl Pts',(6.7472262747399,4.285714286,-2.91965478686889));
#136857=CARTESIAN_POINT('Ctrl Pts',(6.74111070209016,4.28675494927158,-2.9170773152643));
#136858=CARTESIAN_POINT('Ctrl Pts',(6.73499592878079,4.2877998886161,-2.91449967958568));
#136859=CARTESIAN_POINT('Ctrl Pts',(6.72888215553343,4.28884908284639,-2.91192142665916));
#136860=CARTESIAN_POINT('Ctrl Pts',(6.70370785482667,4.29316928413364,-2.90130511626555));
#136861=CARTESIAN_POINT('Ctrl Pts',(6.67855274380647,4.29756059496317,-2.89067195182173));
#136862=CARTESIAN_POINT('Ctrl Pts',(6.65341855208966,4.30202682584539,-2.88002110531445));
#136863=CARTESIAN_POINT('Ctrl Pts',(6.92984512827001,4.17158344184793,-2.13068307872255));
#136864=CARTESIAN_POINT('Ctrl Pts',(6.928666381635,4.17224147442396,-2.13450184786127));
#136865=CARTESIAN_POINT('Ctrl Pts',(6.92748763500001,4.172899507,-2.138320617));
#136866=CARTESIAN_POINT('Ctrl Pts',(6.825583742,4.229787119,-2.468457247));
#136867=CARTESIAN_POINT('Ctrl Pts',(6.692746959,4.285714286,-2.787407065));
#136868=CARTESIAN_POINT('Ctrl Pts',(6.672493911,4.294241258,-2.83603596));
#136869=CARTESIAN_POINT('Ctrl Pts',(6.651536372,4.302795611,-2.884365422));
#136870=CARTESIAN_POINT('Ctrl Pts',(7.09266291765338,4.17158344184793,-2.43807323536181));
#136871=CARTESIAN_POINT('Ctrl Pts',(7.09131462382669,4.17224147442396,-2.4419815706809));
#136872=CARTESIAN_POINT('Ctrl Pts',(7.08996633,4.172899507,-2.445889906));
#136873=CARTESIAN_POINT('Ctrl Pts',(6.973404903,4.229787119,-2.783769627));
#136874=CARTESIAN_POINT('Ctrl Pts',(6.825240674,4.285714286,-3.109033571));
#136875=CARTESIAN_POINT('Ctrl Pts',(6.80265071700001,4.294241258,-3.158625153));
#136876=CARTESIAN_POINT('Ctrl Pts',(6.779342527,4.302795611,-3.207883243));
#136877=CARTESIAN_POINT('Ctrl Pts',(6.92748753519233,4.17289956295265,-2.13832094250849));
#136878=CARTESIAN_POINT('Ctrl Pts',(6.88357214225513,4.19741522520789,-2.2805930073402));
#136879=CARTESIAN_POINT('Ctrl Pts',(6.83535770137452,4.22178368474058,-2.42122648355313));
#136880=CARTESIAN_POINT('Ctrl Pts',(6.78304357401901,4.24593817707607,-2.55984762726379));
#136881=CARTESIAN_POINT('Ctrl Pts',(6.75417899942936,4.25926553587831,-2.63633251852746));
#136882=CARTESIAN_POINT('Ctrl Pts',(6.72406713596566,4.27252781213611,-2.71220526836914));
#136883=CARTESIAN_POINT('Ctrl Pts',(6.69274695873652,4.28571428611093,-2.78740706563264));
#136884=CARTESIAN_POINT('Ctrl Pts',(6.67986179168243,4.29113922060291,-2.81834519581253));
#136885=CARTESIAN_POINT('Ctrl Pts',(6.66675202366146,4.29657697989847,-2.84921814883435));
#136886=CARTESIAN_POINT('Ctrl Pts',(6.65341855208966,4.30202682584539,-2.88002110531445));
#136887=CARTESIAN_POINT('Ctrl Pts',(7.117873279,4.302796438,-1.377817106));
#136888=CARTESIAN_POINT('Ctrl Pts',(7.043269661,4.238074114,-1.763223195));
#136889=CARTESIAN_POINT('Ctrl Pts',(6.927487635,4.172899507,-2.138320617));
#136890=CARTESIAN_POINT('Ctrl Pts',(6.92351476036112,4.17066314482709,-2.15119148380426));
#136891=CARTESIAN_POINT('Ctrl Pts',(6.91954188572229,4.16842678265418,-2.16406235060846));
#136892=CARTESIAN_POINT('Ctrl Pts',(7.40668655768233,4.302796438,-1.18268235378972));
#136893=CARTESIAN_POINT('Ctrl Pts',(7.34264875278569,4.238074114,-1.58372659622447));
#136894=CARTESIAN_POINT('Ctrl Pts',(7.23568222365171,4.172899507,-1.97551159685042));
#136895=CARTESIAN_POINT('Ctrl Pts',(7.23201183865772,4.17066314482709,-1.98895507116724));
#136896=CARTESIAN_POINT('Ctrl Pts',(7.22834145366371,4.16842678265418,-2.00239854548401));
#136897=CARTESIAN_POINT('',(7.11698472910248,4.30202682608696,-1.38239949858852));
#136898=CARTESIAN_POINT('Origin',(-0.189048592298741,4.16072148633095,0.0605005003374037));
#136899=CARTESIAN_POINT('Ctrl Pts',(7.36282707780144,4.26310680656247,-1.42785763095792));
#136900=CARTESIAN_POINT('Ctrl Pts',(7.33460231089812,4.26736775486543,-1.42262455834587));
#136901=CARTESIAN_POINT('Ctrl Pts',(7.30638515506275,4.27169422775027,-1.4174033117379));
#136902=CARTESIAN_POINT('Ctrl Pts',(7.27817644810359,4.27608953517981,-1.41219482004959));
#136903=CARTESIAN_POINT('Ctrl Pts',(7.25781973845827,4.27926139262348,-1.40843613117588));
#136904=CARTESIAN_POINT('Ctrl Pts',(7.23746645323342,4.28246998644609,-1.40468964655264));
#136905=CARTESIAN_POINT('Ctrl Pts',(7.21711934821421,4.285714286,-1.40094067775963));
#136906=CARTESIAN_POINT('Ctrl Pts',(7.21059267423742,4.28675494924643,-1.39973813337481));
#136907=CARTESIAN_POINT('Ctrl Pts',(7.20406674564231,4.28779988856547,-1.3985352569144));
#136908=CARTESIAN_POINT('Ctrl Pts',(7.19754166103911,4.28884908277022,-1.39733156264874));
#136909=CARTESIAN_POINT('Ctrl Pts',(7.17067372868453,4.2931692840602,-1.39237518613073));
#136910=CARTESIAN_POINT('Ctrl Pts',(7.14382091426537,4.29756059489632,-1.38739822434175));
#136911=CARTESIAN_POINT('Ctrl Pts',(7.11698472848189,4.30202682631765,-1.38239949983428));
#136912=CARTESIAN_POINT('Ctrl Pts',(7.22586307942343,4.17158344184794,-0.591157034752303));
#136913=CARTESIAN_POINT('Ctrl Pts',(7.22553281371172,4.17224147442397,-0.595139918876151));
#136914=CARTESIAN_POINT('Ctrl Pts',(7.225202548,4.172899507,-0.599122803));
#136915=CARTESIAN_POINT('Ctrl Pts',(7.196650728,4.229787119,-0.943447347));
#136916=CARTESIAN_POINT('Ctrl Pts',(7.135484378,4.285714286,-1.283496277));
#136917=CARTESIAN_POINT('Ctrl Pts',(7.12615861,4.294241258,-1.335342062));
#136918=CARTESIAN_POINT('Ctrl Pts',(7.11608045300001,4.302795611,-1.387046859));
#136919=CARTESIAN_POINT('Ctrl Pts',(7.45095407682186,4.17158344184794,-0.856359568123212));
#136920=CARTESIAN_POINT('Ctrl Pts',(7.45047748191092,4.17224147442397,-0.860466372061607));
#136921=CARTESIAN_POINT('Ctrl Pts',(7.450000887,4.172899507,-0.864573176));
#136922=CARTESIAN_POINT('Ctrl Pts',(7.408798753,4.229787119,-1.219610719));
#136923=CARTESIAN_POINT('Ctrl Pts',(7.334020655,4.285714286,-1.569121102));
#136924=CARTESIAN_POINT('Ctrl Pts',(7.322619563,4.294241258,-1.622409433));
#136925=CARTESIAN_POINT('Ctrl Pts',(7.310445339,4.302795611,-1.675526468));
#136926=CARTESIAN_POINT('Ctrl Pts',(7.22520252064608,4.17289956288448,-0.599123142072916));
#136927=CARTESIAN_POINT('Ctrl Pts',(7.21289813244332,4.19741522779708,-0.747509492860021));
#136928=CARTESIAN_POINT('Ctrl Pts',(7.1960429562716,4.22178369001281,-0.895219732403616));
#136929=CARTESIAN_POINT('Ctrl Pts',(7.17475134897079,4.24593818502351,-1.04184599794281));
#136930=CARTESIAN_POINT('Ctrl Pts',(7.16300360461675,4.25926554112103,-1.12274772878938));
#136931=CARTESIAN_POINT('Ctrl Pts',(7.14990614052798,4.27252781471258,-1.20331976014873));
#136932=CARTESIAN_POINT('Ctrl Pts',(7.1354843779457,4.28571428606412,-1.28349627741262));
#136933=CARTESIAN_POINT('Ctrl Pts',(7.12955124246503,4.29113922050012,-1.31648102090752));
#136934=CARTESIAN_POINT('Ctrl Pts',(7.123384745955,4.29657697988621,-1.34945039443806));
#136935=CARTESIAN_POINT('Ctrl Pts',(7.11698472873802,4.30202682609955,-1.38239949851566));
#136936=CARTESIAN_POINT('Ctrl Pts',(7.247651307,4.302796438,0.184527844));
#136937=CARTESIAN_POINT('Ctrl Pts',(7.257642797,4.238074114,-0.207905238));
#136938=CARTESIAN_POINT('Ctrl Pts',(7.225202548,4.172899507,-0.599122803));
#136939=CARTESIAN_POINT('Ctrl Pts',(7.22408941287079,4.1706631448628,-0.612546806458474));
#136940=CARTESIAN_POINT('Ctrl Pts',(7.22297627774156,4.16842678272561,-0.62597080991694));
#136941=CARTESIAN_POINT('Ctrl Pts',(7.48776408865884,4.302796438,0.437186772684723));
#136942=CARTESIAN_POINT('Ctrl Pts',(7.51143610924894,4.238074114,0.031752486387759));
#136943=CARTESIAN_POINT('Ctrl Pts',(7.49119259234274,4.172899507,-0.373867440734867));
#136944=CARTESIAN_POINT('Ctrl Pts',(7.4904979685189,4.1706631448628,-0.387785638156601));
#136945=CARTESIAN_POINT('Ctrl Pts',(7.48980334469506,4.16842678272561,-0.401703835578327));
#136946=CARTESIAN_POINT('',(7.24776860934395,4.30202682592312,0.179861575525647));
#136947=CARTESIAN_POINT('Origin',(-0.197634449238847,4.16072144827485,0.0184461769716144));
#136948=CARTESIAN_POINT('Ctrl Pts',(7.49763545645216,4.26310680820235,0.188315065585071));
#136949=CARTESIAN_POINT('Ctrl Pts',(7.4689456126465,4.26736775486193,0.18735830090538));
#136950=CARTESIAN_POINT('Ctrl Pts',(7.44026574456446,4.27169422773965,0.186391623159985));
#136951=CARTESIAN_POINT('Ctrl Pts',(7.41159687066663,4.27608953501748,0.185414304967327));
#136952=CARTESIAN_POINT('Ctrl Pts',(7.38427180671391,4.28027881893866,0.184482797081399));
#136953=CARTESIAN_POINT('Ctrl Pts',(7.35695667274408,4.28452899137757,0.183531259927492));
#136954=CARTESIAN_POINT('Ctrl Pts',(7.32965211329939,4.28884908351549,0.182595971637373));
#136955=CARTESIAN_POINT('Ctrl Pts',(7.30234686834818,4.29316928411336,0.181660659865965));
#136956=CARTESIAN_POINT('Ctrl Pts',(7.27505195801011,4.29756059497224,0.180748701676423));
#136957=CARTESIAN_POINT('Ctrl Pts',(7.24776860697028,4.30202682519232,0.179861576786871));
#136958=CARTESIAN_POINT('Ctrl Pts',(7.18400770487018,4.17158344184794,0.976010855747786));
#136959=CARTESIAN_POINT('Ctrl Pts',(7.1845413629351,4.17224147442397,0.972050091873893));
#136960=CARTESIAN_POINT('Ctrl Pts',(7.185075021,4.172899507,0.968089328));
#136961=CARTESIAN_POINT('Ctrl Pts',(7.23121032499999,4.229787119,0.625677103));
#136962=CARTESIAN_POINT('Ctrl Pts',(7.244574478,4.285714286,0.28042937));
#136963=CARTESIAN_POINT('Ctrl Pts',(7.246612053,4.294241258,0.227790947));
#136964=CARTESIAN_POINT('Ctrl Pts',(7.24788452,4.302795611,0.175128473));
#136965=CARTESIAN_POINT('Ctrl Pts',(7.46084690487036,4.17158344184793,0.765396519891662));
#136966=CARTESIAN_POINT('Ctrl Pts',(7.46126429393518,4.17224147442396,0.761283276945831));
#136967=CARTESIAN_POINT('Ctrl Pts',(7.46168168300001,4.172899507,0.757170034));
#136968=CARTESIAN_POINT('Ctrl Pts',(7.497765409,4.229787119,0.401575832));
#136969=CARTESIAN_POINT('Ctrl Pts',(7.499869982,4.285714286,0.044161726));
#136970=CARTESIAN_POINT('Ctrl Pts',(7.500190857,4.294241258,-0.010331651));
#136971=CARTESIAN_POINT('Ctrl Pts',(7.499719852,4.302795611,-0.064823938));
#136972=CARTESIAN_POINT('Ctrl Pts',(7.18507502325376,4.17289950769094,0.968089322549891));
#136973=CARTESIAN_POINT('Ctrl Pts',(7.18679928313913,4.17502562425059,0.955292014454728));
#136974=CARTESIAN_POINT('Ctrl Pts',(7.18731927076748,4.1756853480949,0.951317019401954));
#136975=CARTESIAN_POINT('Ctrl Pts',(7.18942355498595,4.17834651455219,0.935284676602476));
#136976=CARTESIAN_POINT('Ctrl Pts',(7.19048624506953,4.17970788565082,0.927079305986244));
#136977=CARTESIAN_POINT('Ctrl Pts',(7.19363141099024,4.18379006151612,0.902463723411376));
#136978=CARTESIAN_POINT('Ctrl Pts',(7.1956717930712,4.18650992780772,0.886048028029467));
#136979=CARTESIAN_POINT('Ctrl Pts',(7.20162130524362,4.19466138426959,0.836805503884857));
#136980=CARTESIAN_POINT('Ctrl Pts',(7.20536219573357,4.20008900927845,0.803958095649033));
#136981=CARTESIAN_POINT('Ctrl Pts',(7.2158985568298,4.21633619585876,0.705453633347998));
#136982=CARTESIAN_POINT('Ctrl Pts',(7.22202255225789,4.22713823146259,0.639725048026729));
#136983=CARTESIAN_POINT('Ctrl Pts',(7.23766777348088,4.25939962771955,0.442707524339282));
#136984=CARTESIAN_POINT('Ctrl Pts',(7.24450553306108,4.28067055357091,0.311351690624788));
#136985=CARTESIAN_POINT('Ctrl Pts',(7.2477686110021,4.30202682546369,0.17986157549218));
#136986=CARTESIAN_POINT('Ctrl Pts',(7.038537216,4.302796438,1.738244478));
#136987=CARTESIAN_POINT('Ctrl Pts',(7.132656622,4.238074114,1.357134138));
#136988=CARTESIAN_POINT('Ctrl Pts',(7.185075021,4.172899507,0.968089328));
#136989=CARTESIAN_POINT('Ctrl Pts',(7.18687367436045,4.17066314480402,0.954739878794608));
#136990=CARTESIAN_POINT('Ctrl Pts',(7.18867232772096,4.16842678260804,0.941390429589207));
#136991=CARTESIAN_POINT('Ctrl Pts',(7.21872209223334,4.302796438,2.03661353051088));
#136992=CARTESIAN_POINT('Ctrl Pts',(7.32899706144724,4.238074114,1.64574685777162));
#136993=CARTESIAN_POINT('Ctrl Pts',(7.39642312066713,4.172899507,1.24525834150018));
#136994=CARTESIAN_POINT('Ctrl Pts',(7.39873673783805,4.17066314480401,1.23151621985278));
#136995=CARTESIAN_POINT('Ctrl Pts',(7.40105035500898,4.16842678260803,1.21777409820541));
#136996=CARTESIAN_POINT('',(7.03965488517183,4.30202682592122,1.7337125204802));
#136997=CARTESIAN_POINT('Origin',(-0.196979586829847,4.16072142722509,-0.0244707087506646));
#136998=CARTESIAN_POINT('Ctrl Pts',(7.28186273350202,4.26310680820227,1.79568235830517));
#136999=CARTESIAN_POINT('Ctrl Pts',(7.25404931831883,4.26736775489622,1.78858049393525));
#137000=CARTESIAN_POINT('Ctrl Pts',(7.22624777665622,4.27169422779228,1.78147109270522));
#137001=CARTESIAN_POINT('Ctrl Pts',(7.19845925952399,4.27608953508906,1.77435366321102));
#137002=CARTESIAN_POINT('Ctrl Pts',(7.17197328713478,4.28027881899905,1.76756985246761));
#137003=CARTESIAN_POINT('Ctrl Pts',(7.14550131827908,4.28452899142257,1.76076861535023));
#137004=CARTESIAN_POINT('Ctrl Pts',(7.1190361837065,4.28884908354054,1.7539855203759));
#137005=CARTESIAN_POINT('Ctrl Pts',(7.09257038470169,4.29316928411851,1.74720225510555));
#137006=CARTESIAN_POINT('Ctrl Pts',(7.06610965831957,4.29756059499092,1.74044401924817));
#137007=CARTESIAN_POINT('Ctrl Pts',(7.0396548826298,4.30202682519237,1.73371252114864));
#137008=CARTESIAN_POINT('Ctrl Pts',(6.80623611384359,4.17158344184793,2.49754156239315));
#137009=CARTESIAN_POINT('Ctrl Pts',(6.8076087424218,4.17224147442396,2.49378811969657));
#137010=CARTESIAN_POINT('Ctrl Pts',(6.808981371,4.172899507,2.490034677));
#137011=CARTESIAN_POINT('Ctrl Pts',(6.927646563,4.229787119,2.165545587));
#137012=CARTESIAN_POINT('Ctrl Pts',(7.014916327,4.285714286,1.831242452));
#137013=CARTESIAN_POINT('Ctrl Pts',(7.02822197000001,4.294241258,1.780272704));
#137014=CARTESIAN_POINT('Ctrl Pts',(7.040785563,4.302795611,1.729114993));
#137015=CARTESIAN_POINT('Ctrl Pts',(7.12187882321818,4.17158344184793,2.35136351863107));
#137016=CARTESIAN_POINT('Ctrl Pts',(7.12317067960909,4.17224147442396,2.34743616731554));
#137017=CARTESIAN_POINT('Ctrl Pts',(7.124462536,4.172899507,2.343508816));
#137018=CARTESIAN_POINT('Ctrl Pts',(7.236144887,4.229787119,2.003985142));
#137019=CARTESIAN_POINT('Ctrl Pts',(7.315033724,4.285714286,1.655379601));
#137020=CARTESIAN_POINT('Ctrl Pts',(7.32706156200001,4.294241258,1.602229227));
#137021=CARTESIAN_POINT('Ctrl Pts',(7.3383158,4.302795611,1.548909688));
#137022=CARTESIAN_POINT('Ctrl Pts',(6.80898137388471,4.17289950770924,2.49003467230179));
#137023=CARTESIAN_POINT('Ctrl Pts',(6.81341636437782,4.17502562421675,2.47790722337832));
#137024=CARTESIAN_POINT('Ctrl Pts',(6.8147787014379,4.17568534806893,2.47413694343038));
#137025=CARTESIAN_POINT('Ctrl Pts',(6.82028026846994,4.1783465145361,2.45893178676429));
#137026=CARTESIAN_POINT('Ctrl Pts',(6.82308202557879,4.17970788563266,2.45114670013015));
#137027=CARTESIAN_POINT('Ctrl Pts',(6.83144528188024,4.18379006149366,2.42778273395339));
#137028=CARTESIAN_POINT('Ctrl Pts',(6.83696685021433,4.18650992778079,2.41218945028609));
#137029=CARTESIAN_POINT('Ctrl Pts',(6.8533629531749,4.19466138423686,2.36537715833159));
#137030=CARTESIAN_POINT('Ctrl Pts',(6.86407760550708,4.20008900923532,2.33410188521755));
#137031=CARTESIAN_POINT('Ctrl Pts',(6.89554317839344,4.21633619501415,2.24016541342386));
#137032=CARTESIAN_POINT('Ctrl Pts',(6.9156537019838,4.22713823099044,2.17729000179038));
#137033=CARTESIAN_POINT('Ctrl Pts',(6.97328609825812,4.25939963164881,1.98824187278948));
#137034=CARTESIAN_POINT('Ctrl Pts',(7.00820160458577,4.28067055172509,1.86142701520606));
#137035=CARTESIAN_POINT('Ctrl Pts',(7.03965488694047,4.30202682549038,1.73371252084374));
#137036=CARTESIAN_POINT('Ctrl Pts',(6.500308946,4.302796438,3.210682731));
#137037=CARTESIAN_POINT('Ctrl Pts',(6.67415535,4.238074114,2.85871543));
#137038=CARTESIAN_POINT('Ctrl Pts',(6.80898137100001,4.172899507,2.490034677));
#137039=CARTESIAN_POINT('Ctrl Pts',(6.81360770973313,4.17066314486052,2.4773839880965));
#137040=CARTESIAN_POINT('Ctrl Pts',(6.81823404846635,4.16842678272104,2.46473329919302));
#137041=CARTESIAN_POINT('Ctrl Pts',(6.61214067371357,4.302796438,3.54081050413914));
#137042=CARTESIAN_POINT('Ctrl Pts',(6.80386225587372,4.238074114,3.18278793553515));
#137043=CARTESIAN_POINT('Ctrl Pts',(6.95580512444798,4.172899507,2.80615722777803));
#137044=CARTESIAN_POINT('Ctrl Pts',(6.96101880036082,4.17066314486052,2.79323374892385));
#137045=CARTESIAN_POINT('Ctrl Pts',(6.96623247627363,4.16842678272103,2.78031027006967));
#137046=CARTESIAN_POINT('',(6.50237472155639,4.30202682607388,3.20649699365));
#137047=CARTESIAN_POINT('Origin',(-0.187113793004612,4.16072150002556,-0.0662433900295017));
#137048=CARTESIAN_POINT('Ctrl Pts',(6.72559820206182,4.26310680820237,3.31908553995907));
#137049=CARTESIAN_POINT('Ctrl Pts',(6.69996174009863,4.26736775483089,3.30617065118014));
#137050=CARTESIAN_POINT('Ctrl Pts',(6.67433849417783,4.27169422772263,3.29325095419085));
#137051=CARTESIAN_POINT('Ctrl Pts',(6.64872969411649,4.27608953501734,3.28032621653173));
#137052=CARTESIAN_POINT('Ctrl Pts',(6.6243212678066,4.28027881893362,3.26800730639257));
#137053=CARTESIAN_POINT('Ctrl Pts',(6.59993026376815,4.28452899137277,3.25567438769194));
#137054=CARTESIAN_POINT('Ctrl Pts',(6.57554203423745,4.28884908349646,3.24336065608557));
#137055=CARTESIAN_POINT('Ctrl Pts',(6.55115319241728,4.29316928408013,3.23104661533138));
#137056=CARTESIAN_POINT('Ctrl Pts',(6.52676392411202,4.29756059493291,3.21875810912994));
#137057=CARTESIAN_POINT('Ctrl Pts',(6.50237471819514,4.3020268255211,3.20649699335662));
#137058=CARTESIAN_POINT('Ctrl Pts',(6.110212485956,4.17158344184793,3.9022900024487));
#137059=CARTESIAN_POINT('Ctrl Pts',(6.112359902478,4.17224147442396,3.89891938772435));
#137060=CARTESIAN_POINT('Ctrl Pts',(6.114507319,4.172899507,3.895548773));
#137061=CARTESIAN_POINT('Ctrl Pts',(6.300153748,4.229787119,3.604155566));
#137062=CARTESIAN_POINT('Ctrl Pts',(6.457248486,4.285714286,3.296428672));
#137063=CARTESIAN_POINT('Ctrl Pts',(6.481200039,4.294241258,3.249510888));
#137064=CARTESIAN_POINT('Ctrl Pts',(6.504467298,4.302795611,3.202250017));
#137065=CARTESIAN_POINT('Ctrl Pts',(6.44989960413632,4.17158344184793,3.82738337217394));
#137066=CARTESIAN_POINT('Ctrl Pts',(6.45200552206816,4.17224147442396,3.82382555108697));
#137067=CARTESIAN_POINT('Ctrl Pts',(6.45411144,4.172899507,3.82026773));
#137068=CARTESIAN_POINT('Ctrl Pts',(6.636170272,4.229787119,3.512690335));
#137069=CARTESIAN_POINT('Ctrl Pts',(6.788154619,4.285714286,3.189193765));
#137070=CARTESIAN_POINT('Ctrl Pts',(6.811327012,4.294241258,3.139871648));
#137071=CARTESIAN_POINT('Ctrl Pts',(6.833780257,4.302795611,3.090218018));
#137072=CARTESIAN_POINT('Ctrl Pts',(6.11450750225399,4.17289956286128,3.89554848604006));
#137073=CARTESIAN_POINT('Ctrl Pts',(6.30015382568167,4.22978714685332,3.60415541375994));
#137074=CARTESIAN_POINT('Ctrl Pts',(6.457248486,4.285714286,3.296428672));
#137075=CARTESIAN_POINT('Ctrl Pts',(6.48012364,4.29385805,3.251619405));
#137076=CARTESIAN_POINT('Ctrl Pts',(6.50237471819514,4.3020268255211,3.20649699335661));
#137077=CARTESIAN_POINT('Ctrl Pts',(5.658133455,4.302796438,4.532993029));
#137078=CARTESIAN_POINT('Ctrl Pts',(5.903577993,4.238074114,4.226626366));
#137079=CARTESIAN_POINT('Ctrl Pts',(6.114507319,4.172899507,3.895548773));
#137080=CARTESIAN_POINT('Ctrl Pts',(6.12174502027726,4.17066314496693,3.88418837678026));
#137081=CARTESIAN_POINT('Ctrl Pts',(6.12898272155437,4.16842678293385,3.87282798056048));
#137082=CARTESIAN_POINT('Ctrl Pts',(5.69638290676083,4.302796438,4.87944311363592));
#137083=CARTESIAN_POINT('Ctrl Pts',(5.96058641405342,4.238074114,4.57100538662989));
#137084=CARTESIAN_POINT('Ctrl Pts',(6.18994141211535,4.172899507,4.2358433205947));
#137085=CARTESIAN_POINT('Ctrl Pts',(6.19781136075596,4.17066314496693,4.22434277223839));
#137086=CARTESIAN_POINT('Ctrl Pts',(6.20568130939647,4.16842678293385,4.21284222388206));
#137087=CARTESIAN_POINT('',(5.66105074341552,4.30202682603145,4.52934923318187));
#137088=CARTESIAN_POINT('Origin',(-0.168498607298304,4.16072146875512,-0.104918434826472));
#137089=CARTESIAN_POINT('Ctrl Pts',(5.85485217389105,4.26310680820223,4.68729197081692));
#137090=CARTESIAN_POINT('Ctrl Pts',(5.83259139768624,4.26736775487359,4.66916794326473));
#137091=CARTESIAN_POINT('Ctrl Pts',(5.81034456199046,4.271694227753,4.65104206117557));
#137092=CARTESIAN_POINT('Ctrl Pts',(5.78811291800977,4.27608953503455,4.63291436170113));
#137093=CARTESIAN_POINT('Ctrl Pts',(5.76692334865122,4.28027881894786,4.61563637066914));
#137094=CARTESIAN_POINT('Ctrl Pts',(5.74575380567805,4.2845289913801,4.5983484438477));
#137095=CARTESIAN_POINT('Ctrl Pts',(5.72458284762704,4.28884908350985,4.58107985205215));
#137096=CARTESIAN_POINT('Ctrl Pts',(5.70341135805906,4.29316928409961,4.56381082671223));
#137097=CARTESIAN_POINT('Ctrl Pts',(5.68223396277897,4.29756059496175,4.5465666472899));
#137098=CARTESIAN_POINT('Ctrl Pts',(5.66105074131829,4.30202682519241,4.52934923316963));
#137099=CARTESIAN_POINT('Ctrl Pts',(5.12848211471851,4.17158344184793,5.12457169809598));
#137100=CARTESIAN_POINT('Ctrl Pts',(5.13130390835926,4.17224147442396,5.121741517548));
#137101=CARTESIAN_POINT('Ctrl Pts',(5.134125702,4.172899507,5.118911337));
#137102=CARTESIAN_POINT('Ctrl Pts',(5.378072746,4.229787119,4.874239236));
#137103=CARTESIAN_POINT('Ctrl Pts',(5.597646882,4.285714286,4.607477551));
#137104=CARTESIAN_POINT('Ctrl Pts',(5.631124397,4.294241258,4.566805555));
#137105=CARTESIAN_POINT('Ctrl Pts',(5.664007371,4.302795611,4.52565139));
#137106=CARTESIAN_POINT('Ctrl Pts',(5.47633024678037,4.17158344184793,5.12443903217739));
#137107=CARTESIAN_POINT('Ctrl Pts',(5.47915175589019,4.17224147442396,5.12141710108869));
#137108=CARTESIAN_POINT('Ctrl Pts',(5.481973265,4.172899507,5.11839517));
#137109=CARTESIAN_POINT('Ctrl Pts',(5.725895711,4.229787119,4.857146032));
#137110=CARTESIAN_POINT('Ctrl Pts',(5.943868948,4.285714286,4.573884774));
#137111=CARTESIAN_POINT('Ctrl Pts',(5.977102382,4.294241258,4.53069716));
#137112=CARTESIAN_POINT('Ctrl Pts',(6.009704745,4.302795611,4.487031188));
#137113=CARTESIAN_POINT('Ctrl Pts',(5.13412594167712,4.17289956286129,5.11891109617975));
#137114=CARTESIAN_POINT('Ctrl Pts',(5.37807285460148,4.22978714684998,4.87423910519998));
#137115=CARTESIAN_POINT('Ctrl Pts',(5.597646882,4.285714286,4.607477551));
#137116=CARTESIAN_POINT('Ctrl Pts',(5.629619895,4.29385805,4.568633382));
#137117=CARTESIAN_POINT('Ctrl Pts',(5.66105074131829,4.30202682519241,4.52934923316963));
#137118=CARTESIAN_POINT('Ctrl Pts',(4.551389933,4.302796438,5.643345611));
#137119=CARTESIAN_POINT('Ctrl Pts',(4.85695589,4.238074114,5.39690495000001));
#137120=CARTESIAN_POINT('Ctrl Pts',(5.134125702,4.172899507,5.118911337));
#137121=CARTESIAN_POINT('Ctrl Pts',(5.14363633911191,4.17066314499645,5.10937243247936));
#137122=CARTESIAN_POINT('Ctrl Pts',(5.15314697622385,4.1684267829929,5.09983352795872));
#137123=CARTESIAN_POINT('Ctrl Pts',(4.51426860610591,4.302796438,5.9899183865558));
#137124=CARTESIAN_POINT('Ctrl Pts',(4.83860017587704,4.238074114,5.74548770562787));
#137125=CARTESIAN_POINT('Ctrl Pts',(5.13464291838638,4.172899507,5.46746608780856));
#137126=CARTESIAN_POINT('Ctrl Pts',(5.14480114980883,4.17066314499645,5.45792622234752));
#137127=CARTESIAN_POINT('Ctrl Pts',(5.15495938123141,4.16842678299289,5.44838635688648));
#137128=CARTESIAN_POINT('',(4.55502232502809,4.30202682596754,5.64041413559328));
#137129=CARTESIAN_POINT('Origin',(-0.142005119474485,4.16072144008022,-0.13868801311401));
#137130=CARTESIAN_POINT('Ctrl Pts',(4.71033976553897,4.26310680820237,5.83632583837018));
#137131=CARTESIAN_POINT('Ctrl Pts',(4.69249556405986,4.26736775487414,5.81384013165561));
#137132=CARTESIAN_POINT('Ctrl Pts',(4.67466537587514,4.27169422776848,5.79135561055881));
#137133=CARTESIAN_POINT('Ctrl Pts',(4.65685041491454,4.27608953506659,5.7688725803372));
#137134=CARTESIAN_POINT('Ctrl Pts',(4.63987050326624,4.28027881899228,5.74744340810419));
#137135=CARTESIAN_POINT('Ctrl Pts',(4.6229122856843,4.28452899144104,5.72600883746806));
#137136=CARTESIAN_POINT('Ctrl Pts',(4.6059485297059,4.28884908357724,5.70459284556887));
#137137=CARTESIAN_POINT('Ctrl Pts',(4.58898434783651,4.2931692841734,5.68317631600114));
#137138=CARTESIAN_POINT('Ctrl Pts',(4.57200905721618,4.29756059503823,5.66178278189233));
#137139=CARTESIAN_POINT('Ctrl Pts',(4.55502232147118,4.30202682552115,5.64041413303933));
#137140=CARTESIAN_POINT('Ctrl Pts',(3.90694961831175,4.17158344184794,6.10723411756125));
#137141=CARTESIAN_POINT('Ctrl Pts',(3.91031384515587,4.17224147442397,6.10507670728062));
#137142=CARTESIAN_POINT('Ctrl Pts',(3.913678072,4.172899507,6.10291929700001));
#137143=CARTESIAN_POINT('Ctrl Pts',(4.20451904,4.229787119,5.916408897));
#137144=CARTESIAN_POINT('Ctrl Pts',(4.476305531,4.285714286,5.703085901));
#137145=CARTESIAN_POINT('Ctrl Pts',(4.517743638,4.294241258,5.67056147000001));
#137146=CARTESIAN_POINT('Ctrl Pts',(4.55870475500001,4.302795611,5.637438333));
#137147=CARTESIAN_POINT('Ctrl Pts',(4.24669377469677,4.17158344184794,6.18188161995671));
#137148=CARTESIAN_POINT('Ctrl Pts',(4.25009894434839,4.17224147442397,6.17953688097836));
#137149=CARTESIAN_POINT('Ctrl Pts',(4.253504114,4.172899507,6.177192142));
#137150=CARTESIAN_POINT('Ctrl Pts',(4.547884631,4.229787119,5.974486978));
#137151=CARTESIAN_POINT('Ctrl Pts',(4.821654572,4.285714286,5.744706014));
#137152=CARTESIAN_POINT('Ctrl Pts',(4.863395087,4.294241258,5.709672308));
#137153=CARTESIAN_POINT('Ctrl Pts',(4.904622117,4.302795611,5.674035767));
#137154=CARTESIAN_POINT('Ctrl Pts',(3.91367807732903,4.17289950768826,6.10291929513916));
#137155=CARTESIAN_POINT('Ctrl Pts',(3.92454796154736,4.17502562412239,6.09594865927556));
#137156=CARTESIAN_POINT('Ctrl Pts',(3.92791418505326,4.17568534801395,6.09377161668534));
#137157=CARTESIAN_POINT('Ctrl Pts',(3.94149571326175,4.17834651449182,6.0849963033746));
#137158=CARTESIAN_POINT('Ctrl Pts',(3.94843750638517,4.17970788558933,6.08049420104513));
#137159=CARTESIAN_POINT('Ctrl Pts',(3.96923470669487,4.18379006145286,6.06695553664428));
#137160=CARTESIAN_POINT('Ctrl Pts',(3.98306704220716,4.18650992774202,6.05788334242269));
#137161=CARTESIAN_POINT('Ctrl Pts',(4.02444945824376,4.19466138420298,6.03053890013995));
#137162=CARTESIAN_POINT('Ctrl Pts',(4.05190630760384,4.20008900920532,6.01212510339892));
#137163=CARTESIAN_POINT('Ctrl Pts',(4.13380376324285,4.21633619508676,5.95638508265756));
#137164=CARTESIAN_POINT('Ctrl Pts',(4.18786418937046,4.22713823102538,5.91850077395462));
#137165=CARTESIAN_POINT('Ctrl Pts',(4.34815197388925,4.2593996277154,5.80287852399229));
#137166=CARTESIAN_POINT('Ctrl Pts',(4.45269304977008,4.28067054815198,5.72305206009217));
#137167=CARTESIAN_POINT('Ctrl Pts',(4.55502232628601,4.3020268255026,5.6404141370308));
#137168=CARTESIAN_POINT('Ctrl Pts',(3.231828475,4.302796438,6.489821624));
#137169=CARTESIAN_POINT('Ctrl Pts',(3.583227927,4.238074114,6.314830257));
#137170=CARTESIAN_POINT('Ctrl Pts',(3.913678072,4.172899507,6.102919297));
#137171=CARTESIAN_POINT('Ctrl Pts',(3.92501693864835,4.17066314490783,6.09564791233541));
#137172=CARTESIAN_POINT('Ctrl Pts',(3.93635580529665,4.16842678281565,6.08837652767085));
#137173=CARTESIAN_POINT('Ctrl Pts',(3.12107212213211,4.302796438,6.8203117322704));
#137174=CARTESIAN_POINT('Ctrl Pts',(3.49036637109628,4.238074114,6.65131740573638));
#137175=CARTESIAN_POINT('Ctrl Pts',(3.83925422858816,4.172899507,6.44343621778832));
#137176=CARTESIAN_POINT('Ctrl Pts',(3.8512257557646,4.17066314490783,6.43630310828754));
#137177=CARTESIAN_POINT('Ctrl Pts',(3.86319728294106,4.16842678281565,6.42916999878664));
#137178=CARTESIAN_POINT('',(3.23600612433553,4.30202682597445,6.48773954084562));
#137179=CARTESIAN_POINT('Origin',(-0.108871229324251,4.16072146210519,-0.165972360017885));
#137180=CARTESIAN_POINT('Ctrl Pts',(3.34557710467499,4.26310680820227,6.71245959653848));
#137181=CARTESIAN_POINT('Ctrl Pts',(3.33298385271176,4.26736775486933,6.6866636173957));
#137182=CARTESIAN_POINT('Ctrl Pts',(3.32040403182692,4.27169422775713,6.66087180846766));
#137183=CARTESIAN_POINT('Ctrl Pts',(3.30783876168844,4.27608953504649,6.63508472895175));
#137184=CARTESIAN_POINT('Ctrl Pts',(3.29586246955396,4.28027881896461,6.61050637972617));
#137185=CARTESIAN_POINT('Ctrl Pts',(3.28390852482556,4.28452899140031,6.5859274218728));
#137186=CARTESIAN_POINT('Ctrl Pts',(3.27194517730307,4.2888490835254,6.56136541780598));
#137187=CARTESIAN_POINT('Ctrl Pts',(3.25998152942953,4.29316928411046,6.53680279708701));
#137188=CARTESIAN_POINT('Ctrl Pts',(3.2480020891073,4.29756059497838,6.51226024618941));
#137189=CARTESIAN_POINT('Ctrl Pts',(3.23600612183535,4.30202682552111,6.48773953829106));
#137190=CARTESIAN_POINT('Ctrl Pts',(2.50273250095792,4.17158344184794,6.80432905678979));
#137191=CARTESIAN_POINT('Ctrl Pts',(2.50648185347896,4.17224147442397,6.80294529489489));
#137192=CARTESIAN_POINT('Ctrl Pts',(2.510231206,4.172899507,6.801561533));
#137193=CARTESIAN_POINT('Ctrl Pts',(2.834366696,4.229787119,6.681933854));
#137194=CARTESIAN_POINT('Ctrl Pts',(3.145657109,4.285714286,6.532024292));
#137195=CARTESIAN_POINT('Ctrl Pts',(3.193118207,4.294241258,6.509168232));
#137196=CARTESIAN_POINT('Ctrl Pts',(3.240242171,4.302795611,6.485624925));
#137197=CARTESIAN_POINT('Ctrl Pts',(2.81848662049146,4.17158344184794,6.95026629291661));
#137198=CARTESIAN_POINT('Ctrl Pts',(2.82231622874573,4.17224147442397,6.9487083834583));
#137199=CARTESIAN_POINT('Ctrl Pts',(2.826145837,4.172899507,6.947150474));
#137200=CARTESIAN_POINT('Ctrl Pts',(3.15721952,4.229787119,6.812467554));
#137201=CARTESIAN_POINT('Ctrl Pts',(3.473984987,4.285714286,6.646911186));
#137202=CARTESIAN_POINT('Ctrl Pts',(3.522280843,4.294241258,6.62166952500001));
#137203=CARTESIAN_POINT('Ctrl Pts',(3.570204811,4.302795611,6.59572874));
#137204=CARTESIAN_POINT('Ctrl Pts',(2.51023152525807,4.17289956251626,6.8015614158811));
#137205=CARTESIAN_POINT('Ctrl Pts',(2.83436684933752,4.22978714686279,6.68193378041409));
#137206=CARTESIAN_POINT('Ctrl Pts',(3.145657109,4.285714286,6.532024292));
#137207=CARTESIAN_POINT('Ctrl Pts',(3.190985273,4.29385805,6.510195399));
#137208=CARTESIAN_POINT('Ctrl Pts',(3.23600612183535,4.30202682552111,6.48773953829106));
#137209=CARTESIAN_POINT('Ctrl Pts',(1.76115031,4.302796438,7.032840791));
#137210=CARTESIAN_POINT('Ctrl Pts',(2.141952209,4.238074114,6.93748112));
#137211=CARTESIAN_POINT('Ctrl Pts',(2.510231206,4.172899507,6.801561533));
#137212=CARTESIAN_POINT('Ctrl Pts',(2.52286810920761,4.17066314487519,6.7968976703336));
#137213=CARTESIAN_POINT('Ctrl Pts',(2.53550501241526,4.16842678275038,6.79223380766704));
#137214=CARTESIAN_POINT('Ctrl Pts',(1.58193777457203,4.302796438,7.3317948824841));
#137215=CARTESIAN_POINT('Ctrl Pts',(1.9789269150573,4.238074114,7.24613889640495));
#137216=CARTESIAN_POINT('Ctrl Pts',(2.3643462773467,4.172899507,7.11811843102602));
#137217=CARTESIAN_POINT('Ctrl Pts',(2.37757132470284,4.17066314487519,7.11372561405092));
#137218=CARTESIAN_POINT('Ctrl Pts',(2.39079637205892,4.16842678275038,7.10933279707585));
#137219=CARTESIAN_POINT('',(1.76567787428357,4.30202682597753,7.03170545777996));
#137220=CARTESIAN_POINT('Origin',(-0.0706467007222489,4.16072148923606,
-0.185496026492233));
#137221=CARTESIAN_POINT('Ctrl Pts',(1.82437897687012,4.26310680820178,7.27472620427878));
#137222=CARTESIAN_POINT('Ctrl Pts',(1.81762552129248,4.26736775486331,7.24682614389789));
#137223=CARTESIAN_POINT('Ctrl Pts',(1.81088428609454,4.27169422775163,7.21893304355694));
#137224=CARTESIAN_POINT('Ctrl Pts',(1.80415624475797,4.27608953504463,7.19104769004101));
#137225=CARTESIAN_POINT('Ctrl Pts',(1.79774357016074,4.28027881897063,7.16446942020277));
#137226=CARTESIAN_POINT('Ctrl Pts',(1.79135285131702,4.28452899141856,7.13789536000321));
#137227=CARTESIAN_POINT('Ctrl Pts',(1.78494930497304,4.28884908355464,7.11133583589126));
#137228=CARTESIAN_POINT('Ctrl Pts',(1.77854559786201,4.29316928415071,7.08477564497745));
#137229=CARTESIAN_POINT('Ctrl Pts',(1.77212215308869,4.29756059503481,7.0582316597583));
#137230=CARTESIAN_POINT('Ctrl Pts',(1.76567787233577,4.30202682519262,7.03170545551019));
#137231=CARTESIAN_POINT('Ctrl Pts',(0.9814903926885,4.17158344184794,7.18326113271218));
#137232=CARTESIAN_POINT('Ctrl Pts',(0.98544955534425,4.17224147442397,7.18271572235609));
#137233=CARTESIAN_POINT('Ctrl Pts',(0.989408718,4.172899507,7.18217031200001));
#137234=CARTESIAN_POINT('Ctrl Pts',(1.331682516,4.229787119,7.13501901));
#137235=CARTESIAN_POINT('Ctrl Pts',(1.667921256,4.285714286,7.055532488));
#137236=CARTESIAN_POINT('Ctrl Pts',(1.719186117,4.294241258,7.043413523));
#137237=CARTESIAN_POINT('Ctrl Pts',(1.770269464,4.302795611,7.030550905));
#137238=CARTESIAN_POINT('Ctrl Pts',(1.25849016475012,4.17158344184794,7.39366423866198));
#137239=CARTESIAN_POINT('Ctrl Pts',(1.26256514337506,4.17224147442397,7.39296600483099));
#137240=CARTESIAN_POINT('Ctrl Pts',(1.266640122,4.172899507,7.392267771));
#137241=CARTESIAN_POINT('Ctrl Pts',(1.618926333,4.229787119,7.331904718));
#137242=CARTESIAN_POINT('Ctrl Pts',(1.963875725,4.285714286,7.238314178));
#137243=CARTESIAN_POINT('Ctrl Pts',(2.016468661,4.294241258,7.224044834));
#137244=CARTESIAN_POINT('Ctrl Pts',(2.068848696,4.302795611,7.209012767));
#137245=CARTESIAN_POINT('Ctrl Pts',(0.989409055158278,4.17289956303739,
7.18217026555341));
#137246=CARTESIAN_POINT('Ctrl Pts',(1.13691161755963,4.19741522444947,7.16185045047789));
#137247=CARTESIAN_POINT('Ctrl Pts',(1.28349268583219,4.22178368318658,7.1370231269043));
#137248=CARTESIAN_POINT('Ctrl Pts',(1.42875118656237,4.24593817475617,7.10782456514262));
#137249=CARTESIAN_POINT('Ctrl Pts',(1.50889827891373,4.25926553430343,7.09171411505345));
#137250=CARTESIAN_POINT('Ctrl Pts',(1.58864308271313,4.27252781130386,7.0742737736276));
#137251=CARTESIAN_POINT('Ctrl Pts',(1.66792125607932,4.28571428601319,7.05553248798125));
#137252=CARTESIAN_POINT('Ctrl Pts',(1.70053641057144,4.29113922043624,7.04782229608627));
#137253=CARTESIAN_POINT('Ctrl Pts',(1.73312358400982,4.29657697982257,7.0398799173664));
#137254=CARTESIAN_POINT('Ctrl Pts',(1.76567787434394,4.30202682585967,7.03170545794183));
#137255=CARTESIAN_POINT('Ctrl Pts',(0.208122714,4.302796438,7.247012139));
#137256=CARTESIAN_POINT('Ctrl Pts',(0.600521186,4.238074114,7.235743076));
#137257=CARTESIAN_POINT('Ctrl Pts',(0.989408718000001,4.172899507,7.18217031200001));
#137258=CARTESIAN_POINT('Ctrl Pts',(1.00275277015647,4.17066314485536,7.18033204849665));
#137259=CARTESIAN_POINT('Ctrl Pts',(1.01609682231295,4.16842678271074,7.17849378499338));
#137260=CARTESIAN_POINT('Ctrl Pts',(-0.0311662251568304,4.302796438,7.5004514520176));
#137261=CARTESIAN_POINT('Ctrl Pts',(0.374955034168565,4.238074114,7.50213898580997));
#137262=CARTESIAN_POINT('Ctrl Pts',(0.778884123161325,4.172899507,7.45996533761075));
#137263=CARTESIAN_POINT('Ctrl Pts',(0.792744302229845,4.17066314485536,
7.45851821648986));
#137264=CARTESIAN_POINT('Ctrl Pts',(0.806604481298361,4.16842678271073,
7.45707109536911));
#137265=CARTESIAN_POINT('',(0.212788490584648,4.30202682621549,7.24687664241124));
#137266=CARTESIAN_POINT('Origin',(-0.0291188721727571,4.16072147706576,
-0.196346383455754));
#137267=CARTESIAN_POINT('Ctrl Pts',(0.217874915450326,4.2631068065521,7.49683469975628));
#137268=CARTESIAN_POINT('Ctrl Pts',(0.217277039860373,4.26736775487693,
7.46813513417208));
#137269=CARTESIAN_POINT('Ctrl Pts',(0.216689603126521,4.27169422777341,
7.43944499266939));
#137270=CARTESIAN_POINT('Ctrl Pts',(0.216113386426567,4.2760895352188,7.41076525225242));
#137271=CARTESIAN_POINT('Ctrl Pts',(0.215697561767632,4.27926139264598,
7.39006862322674));
#137272=CARTESIAN_POINT('Ctrl Pts',(0.215293226590095,4.28246998645481,
7.36937734793203));
#137273=CARTESIAN_POINT('Ctrl Pts',(0.21488544015339,4.285714286,7.3486917695344));
#137274=CARTESIAN_POINT('Ctrl Pts',(0.214754635844401,4.2867549492685,7.34205652434719));
#137275=CARTESIAN_POINT('Ctrl Pts',(0.214623383247917,4.28779988861281,
7.33542196099898));
#137276=CARTESIAN_POINT('Ctrl Pts',(0.214491187080227,4.28884908284614,
7.32878809821868));
#137277=CARTESIAN_POINT('Ctrl Pts',(0.213946851210435,4.29316928414664,
7.30147225745247));
#137278=CARTESIAN_POINT('Ctrl Pts',(0.213379755318496,4.29756059501892,
7.27416800514923));
#137279=CARTESIAN_POINT('Ctrl Pts',(0.212788492433934,4.30202682634648,
7.24687664195078));
#137280=CARTESIAN_POINT('Ctrl Pts',(-0.585645114452639,4.17158344184794,
7.22631190105834));
#137281=CARTESIAN_POINT('Ctrl Pts',(-0.58166126772632,4.17224147442397,
7.22663034502917));
#137282=CARTESIAN_POINT('Ctrl Pts',(-0.577677420999999,4.172899507,7.226948789));
#137283=CARTESIAN_POINT('Ctrl Pts',(-0.233269659,4.229787119,7.25447860700001));
#137284=CARTESIAN_POINT('Ctrl Pts',(0.112195259,4.285714286,7.249131826));
#137285=CARTESIAN_POINT('Ctrl Pts',(0.164866796,4.294241258,7.24831662500001));
#137286=CARTESIAN_POINT('Ctrl Pts',(0.217520925,4.302795611,7.246736138));
#137287=CARTESIAN_POINT('Ctrl Pts',(-0.360351892041105,4.17158344184794,
7.49134266211465));
#137288=CARTESIAN_POINT('Ctrl Pts',(-0.356222084520552,4.17224147442397,
7.49153675255733));
#137289=CARTESIAN_POINT('Ctrl Pts',(-0.352092277,4.172899507,7.491730843));
#137290=CARTESIAN_POINT('Ctrl Pts',(0.00493395,4.229787119,7.508510167));
#137291=CARTESIAN_POINT('Ctrl Pts',(0.361937816,4.285714286,7.491261644));
#137292=CARTESIAN_POINT('Ctrl Pts',(0.416368646,4.294241258,7.488631836));
#137293=CARTESIAN_POINT('Ctrl Pts',(0.470755515,4.302795611,7.485211369));
#137294=CARTESIAN_POINT('Ctrl Pts',(-0.577677413703493,4.17289950809451,
7.22694879031625));
#137295=CARTESIAN_POINT('Ctrl Pts',(-0.56480552482683,4.17502562458467,
7.22797768913303));
#137296=CARTESIAN_POINT('Ctrl Pts',(-0.560808210063437,4.17568534806879,
7.228281712103));
#137297=CARTESIAN_POINT('Ctrl Pts',(-0.544685456375747,4.17834651453278,
7.22951493671606));
#137298=CARTESIAN_POINT('Ctrl Pts',(-0.536434586763961,4.17970788563026,
7.23013183848652));
#137299=CARTESIAN_POINT('Ctrl Pts',(-0.511684829216335,4.18379006149283,
7.23193973104456));
#137300=CARTESIAN_POINT('Ctrl Pts',(-0.495182744814378,4.18650992778213,
7.23308839294241));
#137301=CARTESIAN_POINT('Ctrl Pts',(-0.445690338987542,4.19466138423982,
7.23636324326149));
#137302=CARTESIAN_POINT('Ctrl Pts',(-0.412688576604694,4.20008900924327,
7.23832032466424));
#137303=CARTESIAN_POINT('Ctrl Pts',(-0.31375816172737,4.216336194307,7.24350830895865));
#137304=CARTESIAN_POINT('Ctrl Pts',(-0.247794422042017,4.22713823064889,
7.24606484978825));
#137305=CARTESIAN_POINT('Ctrl Pts',(-0.0502188363241316,4.25939962529463,
7.25102081240762));
#137306=CARTESIAN_POINT('Ctrl Pts',(0.0813145238869553,4.2806705478024,
7.25073708286748));
#137307=CARTESIAN_POINT('Ctrl Pts',(0.212788490677497,4.30202682582528,
7.24687664341437));
#137308=CARTESIAN_POINT('Ctrl Pts',(0.208833664,1.716084912,7.24699168599999));
#137309=CARTESIAN_POINT('Ctrl Pts',(0.602705566,1.651909459,7.235641637));
#137310=CARTESIAN_POINT('Ctrl Pts',(0.993027302,1.586734015,7.18167089));
#137311=CARTESIAN_POINT('Ctrl Pts',(1.00632215130568,1.58451405739453,7.17983257846853));
#137312=CARTESIAN_POINT('Ctrl Pts',(1.01961700061136,1.58229409978908,7.17799426693693));
#137313=CARTESIAN_POINT('Ctrl Pts',(-0.0304295583832685,1.716084912,7.50045357073996));
#137314=CARTESIAN_POINT('Ctrl Pts',(0.377217924081657,1.651909459,7.50210740824932));
#137315=CARTESIAN_POINT('Ctrl Pts',(0.782643448641818,1.586734015,7.45957096278917));
#137316=CARTESIAN_POINT('Ctrl Pts',(0.796452751984597,1.58451405739453,
7.45812211795109));
#137317=CARTESIAN_POINT('Ctrl Pts',(0.810262055327374,1.58229409978908,
7.45667327311299));
#137318=CARTESIAN_POINT('',(0.221461492134119,1.67637478032017,7.49672960736312));
#137319=CARTESIAN_POINT('',(0.783069556218465,1.5867340154113,7.45900811558597));
#137320=CARTESIAN_POINT('Origin',(-0.0362756096552462,1.48219936157375,
-0.185156248438731));
#137321=CARTESIAN_POINT('',(0.888048434082533,1.58673401622023,7.32033950208015));
#137322=CARTESIAN_POINT('Ctrl Pts',(0.221461497219396,1.67637477933497,
7.4967296070682));
#137323=CARTESIAN_POINT('Ctrl Pts',(0.220241943763555,1.68255913647788,
7.45504166138719));
#137324=CARTESIAN_POINT('Ctrl Pts',(0.218971997975702,1.68889233601893,
7.41335297032202));
#137325=CARTESIAN_POINT('Ctrl Pts',(0.216324551305769,1.70186464078375,
7.33007576431632));
#137326=CARTESIAN_POINT('Ctrl Pts',(0.214945489005334,1.70851143074018,
7.28843788680386));
#137327=CARTESIAN_POINT('Ctrl Pts',(0.213507121522031,1.71532338698339,
7.24685550635322));
#137328=CARTESIAN_POINT('Ctrl Pts',(0.993027301999999,1.586734015,7.18167089));
#137329=CARTESIAN_POINT('Ctrl Pts',(1.055355172,1.596957843,7.173052662));
#137330=CARTESIAN_POINT('Ctrl Pts',(1.117524075,1.607142857,7.163353959));
#137331=CARTESIAN_POINT('Ctrl Pts',(1.447313794,1.661171687,7.111904882));
#137332=CARTESIAN_POINT('Ctrl Pts',(1.770981213,1.716105035,7.03037165));
#137333=CARTESIAN_POINT('Ctrl Pts',(1.270364528,1.586734015,7.391628641));
#137334=CARTESIAN_POINT('Ctrl Pts',(1.334514567,1.596957843,7.380603475));
#137335=CARTESIAN_POINT('Ctrl Pts',(1.398463589,1.607142857,7.36846657));
#137336=CARTESIAN_POINT('Ctrl Pts',(1.737696375,1.661171687,7.304083473));
#137337=CARTESIAN_POINT('Ctrl Pts',(2.06957851,1.716105035,7.208803284));
#137338=CARTESIAN_POINT('',(1.27036453248219,1.5867340145549,7.39162863951456));
#137339=CARTESIAN_POINT('',(1.82785910999321,1.67637477921978,7.27385256010028));
#137340=CARTESIAN_POINT('Ctrl Pts',(1.27036453168524,1.58673401558733,7.39162864036663));
#137341=CARTESIAN_POINT('Ctrl Pts',(1.31316981756271,1.59355605166269,7.38427189684406));
#137342=CARTESIAN_POINT('Ctrl Pts',(1.35587255570895,1.60035948085478,7.37654993560476));
#137343=CARTESIAN_POINT('Ctrl Pts',(1.39846358896283,1.60714285699732,7.36846656998833));
#137344=CARTESIAN_POINT('Ctrl Pts',(1.5420458747753,1.63001087929659,7.34121604280571));
#137345=CARTESIAN_POINT('Ctrl Pts',(1.68530485402972,1.65310706305942,7.30967526843382));
#137346=CARTESIAN_POINT('Ctrl Pts',(1.82785910592338,1.67637477811409,7.27385256090117));
#137347=CARTESIAN_POINT('Ctrl Pts',(1.76637516206954,1.71532338708051,7.03153033114753));
#137348=CARTESIAN_POINT('Ctrl Pts',(1.77671888970243,1.70851142704495,7.07183135470349));
#137349=CARTESIAN_POINT('Ctrl Pts',(1.78701662973198,1.70186463305822,7.11219933048093));
#137350=CARTESIAN_POINT('Ctrl Pts',(1.80750430589202,1.68889233606769,7.19296039064618));
#137351=CARTESIAN_POINT('Ctrl Pts',(1.81770639724589,1.68255913656091,7.23340142230929));
#137352=CARTESIAN_POINT('Ctrl Pts',(1.82785911422308,1.67637477942243,7.27385255906961));
#137353=CARTESIAN_POINT('',(1.13169592297835,1.58673401368698,7.28664976426088));
#137354=CARTESIAN_POINT('Origin',(-1.58944038486375E-13,1.67745375800067,
-1.02565525517129E-12));
#137355=CARTESIAN_POINT('',(1.82088906321883,1.49654505841717,7.27560052616862));
#137356=CARTESIAN_POINT('Origin',(-0.0489661124338905,1.48214578504932,
-0.186087345027959));
#137357=CARTESIAN_POINT('',(2.36822808233295,1.58673401541125,7.11628384459579));
#137358=CARTESIAN_POINT('Origin',(-0.0202030731975594,1.33942798224484,
-0.183880141435366));
#137359=CARTESIAN_POINT('Origin',(-0.0752306731453836,1.48219934190074,
-0.173029379240938));
#137360=CARTESIAN_POINT('Ctrl Pts',(1.761840242,1.716084912,7.032667983));
#137361=CARTESIAN_POINT('Ctrl Pts',(2.144063713,1.651909459,6.93691247599999));
#137362=CARTESIAN_POINT('Ctrl Pts',(2.513657828,1.586734015,6.8002959));
#137363=CARTESIAN_POINT('Ctrl Pts',(2.52624666878501,1.5845140573375,6.79564256745476));
#137364=CARTESIAN_POINT('Ctrl Pts',(2.53883550957,1.58229409967501,6.79098923490962));
#137365=CARTESIAN_POINT('Ctrl Pts',(1.58265767436727,1.716084912,7.33163858915172));
#137366=CARTESIAN_POINT('Ctrl Pts',(1.98113011132105,1.651909459,7.24562160212943));
#137367=CARTESIAN_POINT('Ctrl Pts',(2.36793293409444,1.586734015,7.1169251321701));
#137368=CARTESIAN_POINT('Ctrl Pts',(2.38110792512774,1.5845140573375,7.11254156840608));
#137369=CARTESIAN_POINT('Ctrl Pts',(2.39428291616108,1.58229409967502,7.10815800464207));
#137370=CARTESIAN_POINT('',(2.44094296070756,1.58673401622024,6.95828986997161));
#137371=CARTESIAN_POINT('Ctrl Pts',(2.513657828,1.586734015,6.8002959));
#137372=CARTESIAN_POINT('Ctrl Pts',(2.572675843,1.596957843,6.778480511));
#137373=CARTESIAN_POINT('Ctrl Pts',(2.631306337,1.607142857,6.755644082));
#137374=CARTESIAN_POINT('Ctrl Pts',(2.942325725,1.661171687,6.634502815));
#137375=CARTESIAN_POINT('Ctrl Pts',(3.240898745,1.716105035,6.48529685700001));
#137376=CARTESIAN_POINT('Ctrl Pts',(2.829645774,1.586734015,6.94572564900001));
#137377=CARTESIAN_POINT('Ctrl Pts',(2.889925936,1.596957843,6.921167883));
#137378=CARTESIAN_POINT('Ctrl Pts',(2.94977079,1.607142857,6.895567583));
#137379=CARTESIAN_POINT('Ctrl Pts',(3.267232039,1.661171687,6.75976470500001));
#137380=CARTESIAN_POINT('Ctrl Pts',(3.57087253,1.716105035,6.59536726600001));
#137381=CARTESIAN_POINT('',(2.82964577863492,1.58673401412041,6.94572564643079));
#137382=CARTESIAN_POINT('',(3.34878806638739,1.67637478036033,6.71085825246303));
#137383=CARTESIAN_POINT('Ctrl Pts',(2.82964577786913,1.58673401434343,6.94572564760425));
#137384=CARTESIAN_POINT('Ctrl Pts',(2.86986881736956,1.59355605125276,6.92933902946382));
#137385=CARTESIAN_POINT('Ctrl Pts',(2.90991319578077,1.60035948085479,6.9126177769304));
#137386=CARTESIAN_POINT('Ctrl Pts',(2.94977078968452,1.60714285723677,6.89556758275372));
#137387=CARTESIAN_POINT('Ctrl Pts',(3.08413814382473,1.63001087929511,6.83808821045067));
#137388=CARTESIAN_POINT('Ctrl Pts',(3.21726747328943,1.65310706412526,6.77648839638024));
#137389=CARTESIAN_POINT('Ctrl Pts',(3.34878806267424,1.67637478135681,6.71085825444783));
#137390=CARTESIAN_POINT('Ctrl Pts',(3.23664946313647,1.71532338696461,6.48741861413624));
#137391=CARTESIAN_POINT('Ctrl Pts',(3.25541488900748,1.70851142691025,6.52455382658057));
#137392=CARTESIAN_POINT('Ctrl Pts',(3.2741497950716,1.70186463296974,6.56176431152001));
#137393=CARTESIAN_POINT('Ctrl Pts',(3.31151972142592,1.68889233604064,6.63623297774042));
#137394=CARTESIAN_POINT('Ctrl Pts',(3.33017692015088,1.68255913650151,6.67353537259707));
#137395=CARTESIAN_POINT('Ctrl Pts',(3.34878807097847,1.67637477938387,6.71085825001188));
#137396=CARTESIAN_POINT('',(2.6716518085261,1.58673401368687,6.87301077157449));
#137397=CARTESIAN_POINT('Origin',(3.76001313417973E-13,1.677453758,7.04297731246584E-13));
#137398=CARTESIAN_POINT('',(3.34235673590871,1.49654505837964,6.71406370599629));
#137399=CARTESIAN_POINT('Origin',(-0.0878244442498344,1.48214574245629,
-0.171210134418975));
#137400=CARTESIAN_POINT('',(3.84265089985349,1.58673401497662,6.44081004656482));
#137401=CARTESIAN_POINT('Origin',(-0.0592595317475542,1.33942796996735,
-0.17523807301288));
#137402=CARTESIAN_POINT('Origin',(-0.11066787247884,1.48219935974344,-0.152811403070521));
#137403=CARTESIAN_POINT('Ctrl Pts',(3.232465128,1.716084912,6.489504542));
#137404=CARTESIAN_POINT('Ctrl Pts',(3.585167823,1.651909459,6.313820997));
#137405=CARTESIAN_POINT('Ctrl Pts',(3.916752508,1.586734015,6.100946631));
#137406=CARTESIAN_POINT('Ctrl Pts',(3.92804669933292,1.5845140574204,6.09369586240833));
#137407=CARTESIAN_POINT('Ctrl Pts',(3.93934089066585,1.58229409984081,6.08644509381663));
#137408=CARTESIAN_POINT('Ctrl Pts',(3.12174159234192,1.716084912,6.82000433698394));
#137409=CARTESIAN_POINT('Ctrl Pts',(3.49240685595113,1.651909459,6.65033858415981));
#137410=CARTESIAN_POINT('Ctrl Pts',(3.84250050620848,1.586734015,6.44149979263774));
#137411=CARTESIAN_POINT('Ctrl Pts',(3.85442513617274,1.5845140574204,6.43438648078746));
#137412=CARTESIAN_POINT('Ctrl Pts',(3.86634976613706,1.58229409984081,6.42727316893712));
#137413=CARTESIAN_POINT('',(3.87970170699552,1.58673401622024,6.27087833698131));
#137414=CARTESIAN_POINT('Ctrl Pts',(3.916752508,1.586734015,6.100946631));
#137415=CARTESIAN_POINT('Ctrl Pts',(3.969701051,1.596957843,6.066954145));
#137416=CARTESIAN_POINT('Ctrl Pts',(4.022051639,1.607142857,6.032047796));
#137417=CARTESIAN_POINT('Ctrl Pts',(4.299757775,1.661171687,5.846878769));
#137418=CARTESIAN_POINT('Ctrl Pts',(4.559275454,1.716105035,5.636976791));
#137419=CARTESIAN_POINT('Ctrl Pts',(4.256615929,1.586734015,6.17504824600001));
#137420=CARTESIAN_POINT('Ctrl Pts',(4.310207581,1.596957843,6.138106173));
#137421=CARTESIAN_POINT('Ctrl Pts',(4.363149987,1.607142857,6.100239519));
#137422=CARTESIAN_POINT('Ctrl Pts',(4.643995564,1.661171687,5.899366853));
#137423=CARTESIAN_POINT('Ctrl Pts',(4.905196519,1.716105035,5.673539205));
#137424=CARTESIAN_POINT('',(4.25661593240845,1.58673401455502,6.17504824276234));
#137425=CARTESIAN_POINT('',(4.71313141536523,1.67637477921302,5.83407167023774));
#137426=CARTESIAN_POINT('Ctrl Pts',(4.2566159320791,1.58673401558741,6.1750482438775));
#137427=CARTESIAN_POINT('Ctrl Pts',(4.2923759412647,1.59355605166272,6.15039797052476));
#137428=CARTESIAN_POINT('Ctrl Pts',(4.32788952943669,1.6003594808548,6.12545929360655));
#137429=CARTESIAN_POINT('Ctrl Pts',(4.36314998703704,1.60714285700713,6.1002395189735));
#137430=CARTESIAN_POINT('Ctrl Pts',(4.48201954105858,1.63001087933828,6.01521897324191));
#137431=CARTESIAN_POINT('Ctrl Pts',(4.59879424145111,1.65310706305078,5.92644045793392));
#137432=CARTESIAN_POINT('Ctrl Pts',(4.71313141195594,1.67637477809031,5.83407167271127));
#137433=CARTESIAN_POINT('Ctrl Pts',(4.55558163244203,1.71532338704987,5.63996241217782));
#137434=CARTESIAN_POINT('Ctrl Pts',(4.58189130563171,1.70851142709471,5.67219541149811));
#137435=CARTESIAN_POINT('Ctrl Pts',(4.60818735396652,1.70186463322795,5.70450848448949));
#137436=CARTESIAN_POINT('Ctrl Pts',(4.66069215498257,1.6888923360782,5.76920268614747));
#137437=CARTESIAN_POINT('Ctrl Pts',(4.68693207092282,1.68255913655261,5.80162222542772));
#137438=CARTESIAN_POINT('Ctrl Pts',(4.71313141882367,1.67637477941883,5.83407166748466));
#137439=CARTESIAN_POINT('',(4.08668422522155,1.5867340136868,6.13799743402479));
#137440=CARTESIAN_POINT('Origin',(-3.35668992601512E-13,1.67745375799922,
-3.29163779566599E-13));
#137441=CARTESIAN_POINT('',(4.70753952324108,1.49654505823086,5.83858472873868));
#137442=CARTESIAN_POINT('Origin',(-0.122576383705985,1.48214561512888,-0.148327772102289));
#137443=CARTESIAN_POINT('',(5.13739562869252,1.58673401497662,5.46417113114493));
#137444=CARTESIAN_POINT('Origin',(-0.0955451243659877,1.33942795239901,
-0.158402113986218));
#137445=CARTESIAN_POINT('Origin',(-0.140930589051371,1.48219934068697,-0.125448596449305));
#137446=CARTESIAN_POINT('Ctrl Pts',(4.551943538,1.716084912,5.64289908));
#137447=CARTESIAN_POINT('Ctrl Pts',(4.858633471,1.651909459,5.395502265));
#137448=CARTESIAN_POINT('Ctrl Pts',(5.136704194,1.586734015,5.11632387800001));
#137449=CARTESIAN_POINT('Ctrl Pts',(5.14617563270623,1.58451405737073,5.10681471086421));
#137450=CARTESIAN_POINT('Ctrl Pts',(5.15564707141259,1.58229409974149,5.09730554372844));
#137451=CARTESIAN_POINT('Ctrl Pts',(4.51485634319875,1.716084912,5.98947426038962));
#137452=CARTESIAN_POINT('Ctrl Pts',(4.84038253734788,1.651909459,5.74409312385766));
#137453=CARTESIAN_POINT('Ctrl Pts',(5.13739702623245,1.586734015,5.46487708159231));
#137454=CARTESIAN_POINT('Ctrl Pts',(5.14751371344061,1.58451405737074,5.45536663187083));
#137455=CARTESIAN_POINT('Ctrl Pts',(5.15763040064876,1.58229409974148,5.44585618214922));
#137456=CARTESIAN_POINT('',(5.13704991397976,1.58673401622024,5.29024750217892));
#137457=CARTESIAN_POINT('Ctrl Pts',(5.136704194,1.586734015,5.116323878));
#137458=CARTESIAN_POINT('Ctrl Pts',(5.18110745,1.596957843,5.071743746));
#137459=CARTESIAN_POINT('Ctrl Pts',(5.224730277,1.607142857,5.026399659));
#137460=CARTESIAN_POINT('Ctrl Pts',(5.45613793,1.661171687,4.785861171));
#137461=CARTESIAN_POINT('Ctrl Pts',(5.664465509,1.716105035,4.525077954));
#137462=CARTESIAN_POINT('Ctrl Pts',(5.48455145300001,1.586734015,5.115632449));
#137463=CARTESIAN_POINT('Ctrl Pts',(5.528948709,1.596957843,5.068033441));
#137464=CARTESIAN_POINT('Ctrl Pts',(5.57251314,1.607142857,5.019671036));
#137465=CARTESIAN_POINT('Ctrl Pts',(5.80361101800001,1.661171687,4.763121164));
#137466=CARTESIAN_POINT('Ctrl Pts',(6.010158971,1.716105035,4.486422756));
#137467=CARTESIAN_POINT('',(5.48455145598238,1.58673401455096,5.1156324447679));
#137468=CARTESIAN_POINT('',(5.85709397744235,1.6763747791622,4.68449038193992));
#137469=CARTESIAN_POINT('Ctrl Pts',(5.48455145555049,1.58673401558733,5.11563244626559));
#137470=CARTESIAN_POINT('Ctrl Pts',(5.51417633597188,1.59355605166269,5.08387113827875));
#137471=CARTESIAN_POINT('Ctrl Pts',(5.54349855818175,1.6003594808548,5.05188114237765));
#137472=CARTESIAN_POINT('Ctrl Pts',(5.57251313993258,1.60714285700702,5.01967103596857));
#137473=CARTESIAN_POINT('Ctrl Pts',(5.67032668528231,1.63001087932259,4.91108478308228));
#137474=CARTESIAN_POINT('Ctrl Pts',(5.7652865019684,1.65310706301201,4.79927875139742));
#137475=CARTESIAN_POINT('Ctrl Pts',(5.85709397459755,1.67637477801778,4.68449038515019));
#137476=CARTESIAN_POINT('Ctrl Pts',(5.66149986807226,1.71532338702862,4.52878783547239));
#137477=CARTESIAN_POINT('Ctrl Pts',(5.69412357879441,1.70851142687279,4.55461144413884));
#137478=CARTESIAN_POINT('Ctrl Pts',(5.72675119652746,1.70186463284792,4.58051618321537));
#137479=CARTESIAN_POINT('Ctrl Pts',(5.79193580377598,1.68889233604302,4.63241088915536));
#137480=CARTESIAN_POINT('Ctrl Pts',(5.82453148777529,1.68255913650028,4.65843167155449));
#137481=CARTESIAN_POINT('Ctrl Pts',(5.85709398027991,1.67637477937176,4.68449037844389));
#137482=CARTESIAN_POINT('',(5.31062782910159,1.58673401368699,5.11597815768528));
#137483=CARTESIAN_POINT('Origin',(1.03302782994419E-12,1.6774537579995,
9.41521166586412E-13));
#137484=CARTESIAN_POINT('',(5.85260299487725,1.49654505844533,4.6901000181293));
#137485=CARTESIAN_POINT('Origin',(-0.151596599578943,1.48214574060145,-0.118509601591543));
#137486=CARTESIAN_POINT('',(6.19192144724154,1.58673401497662,4.2320336470176));
#137487=CARTESIAN_POINT('Origin',(-0.127363302340727,1.33942796605195,-0.134159530787841));
#137488=CARTESIAN_POINT('Origin',(-0.164603305646737,1.48219936907616,-0.0922196613299897));
#137489=CARTESIAN_POINT('Ctrl Pts',(5.658578127,1.716084912,4.532437929));
#137490=CARTESIAN_POINT('Ctrl Pts',(5.904914818,1.651909459,4.224895844));
#137491=CARTESIAN_POINT('Ctrl Pts',(6.116469301,1.586734015,3.892467507));
#137492=CARTESIAN_POINT('Ctrl Pts',(6.12367511279101,1.58451405739759,3.88114457970276));
#137493=CARTESIAN_POINT('Ctrl Pts',(6.13088092458192,1.58229409979519,3.86982165240546));
#137494=CARTESIAN_POINT('Ctrl Pts',(5.69686142934484,1.716084912,4.87888302591572));
#137495=CARTESIAN_POINT('Ctrl Pts',(5.96202731117359,1.651909459,4.56926025478402));
#137496=CARTESIAN_POINT('Ctrl Pts',(6.19207457064325,1.586734015,4.23272279233906));
#137497=CARTESIAN_POINT('Ctrl Pts',(6.1999102696616,1.58451405739759,4.22125990306055));
#137498=CARTESIAN_POINT('Ctrl Pts',(6.20774596868001,1.58229409979519,4.20979701378211));
#137499=CARTESIAN_POINT('',(6.15419537620777,1.58673401622024,4.06225057412534));
#137500=CARTESIAN_POINT('Ctrl Pts',(6.116469301,1.586734015,3.892467507));
#137501=CARTESIAN_POINT('Ctrl Pts',(6.15025102300001,1.596957843,3.839384247));
#137502=CARTESIAN_POINT('Ctrl Pts',(6.183106334,1.607142857,3.785722661));
#137503=CARTESIAN_POINT('Ctrl Pts',(6.35739514,1.661171687,3.501062024));
#137504=CARTESIAN_POINT('Ctrl Pts',(6.504791453,1.716105035,3.201591502));
#137505=CARTESIAN_POINT('Ctrl Pts',(6.456035448,1.586734015,3.817015365));
#137506=CARTESIAN_POINT('Ctrl Pts',(6.48916234,1.596957843,3.760985098));
#137507=CARTESIAN_POINT('Ctrl Pts',(6.521311771,1.607142857,3.704388314));
#137508=CARTESIAN_POINT('Ctrl Pts',(6.691856071,1.661171687,3.404157223));
#137509=CARTESIAN_POINT('Ctrl Pts',(6.834093069,1.716105035,3.089526165));
#137510=CARTESIAN_POINT('',(6.45603544999827,1.5867340141205,3.81701536011187));
#137511=CARTESIAN_POINT('',(6.72718533431618,1.67637478035739,3.31586752983505));
#137512=CARTESIAN_POINT('Ctrl Pts',(6.4560354499492,1.58673401434349,3.81701536137849));
#137513=CARTESIAN_POINT('Ctrl Pts',(6.47813997398216,1.59355605125278,3.77962814198058));
#137514=CARTESIAN_POINT('Ctrl Pts',(6.49989975501628,1.60035948085479,3.74208264361557));
#137515=CARTESIAN_POINT('Ctrl Pts',(6.52131177123809,1.60714285723678,3.70438831419057));
#137516=CARTESIAN_POINT('Ctrl Pts',(6.59349565604718,1.63001087929981,3.57731372649253));
#137517=CARTESIAN_POINT('Ctrl Pts',(6.66220037299145,1.6531070641298,3.44770810410909));
#137518=CARTESIAN_POINT('Ctrl Pts',(6.72718533265722,1.67637478135621,3.31586753355462));
#137519=CARTESIAN_POINT('Ctrl Pts',(6.50269266198306,1.71532338705695,3.20585217351008));
#137520=CARTESIAN_POINT('Ctrl Pts',(6.54010496095514,1.708511426897,3.22405890711588));
#137521=CARTESIAN_POINT('Ctrl Pts',(6.57753851629545,1.70186463285819,3.24234403449837));
#137522=CARTESIAN_POINT('Ctrl Pts',(6.65235497134765,1.68889233604686,3.27901270739335));
#137523=CARTESIAN_POINT('Ctrl Pts',(6.68978228522786,1.68255913652599,3.29741802977717));
#137524=CARTESIAN_POINT('Ctrl Pts',(6.72718533641487,1.67637477939228,3.31586752525681));
#137525=CARTESIAN_POINT('',(6.28625237872066,1.58673401368698,3.85474142911702));
#137526=CARTESIAN_POINT('Origin',(4.28910379435266E-13,1.67745375799939,
2.50233861409654E-13));
#137527=CARTESIAN_POINT('',(6.72400525501397,1.49654505839823,3.32231144352664));
#137528=CARTESIAN_POINT('Origin',(-0.173528731532434,1.48214576180425,-0.0831502913214777));
#137529=CARTESIAN_POINT('',(6.95691990064217,1.58673401497662,2.80201097326936));
#137530=CARTESIAN_POINT('Origin',(-0.153225813866532,1.33942799701563,-0.103643539900192));
#137531=CARTESIAN_POINT('Origin',(-0.180579826077908,1.48219935447444,-0.0546789315472151));
#137532=CARTESIAN_POINT('Ctrl Pts',(6.50062389200001,1.716084912,3.210045018));
#137533=CARTESIAN_POINT('Ctrl Pts',(6.67508891000001,1.651909459,2.85673799));
#137534=CARTESIAN_POINT('Ctrl Pts',(6.81023510100001,1.586734015,2.486603681));
#137535=CARTESIAN_POINT('Ctrl Pts',(6.81483835017594,1.58451405743652,2.47399644108972));
#137536=CARTESIAN_POINT('Ctrl Pts',(6.81944159935196,1.58229409987305,2.46138920117939));
#137537=CARTESIAN_POINT('Ctrl Pts',(6.6124876069262,1.716084912,3.5401606418956));
#137538=CARTESIAN_POINT('Ctrl Pts',(6.80489431324512,1.651909459,3.18077385321148));
#137539=CARTESIAN_POINT('Ctrl Pts',(6.95721758997104,1.586734015,2.80265108974158));
#137540=CARTESIAN_POINT('Ctrl Pts',(6.96240591228245,1.58451405743652,2.78977175302867));
#137541=CARTESIAN_POINT('Ctrl Pts',(6.96759423459393,1.58229409987304,2.77689241631583));
#137542=CARTESIAN_POINT('',(6.88357750223904,1.58673401622024,2.64430732386983));
#137543=CARTESIAN_POINT('Ctrl Pts',(6.810235101,1.586734015,2.486603681));
#137544=CARTESIAN_POINT('Ctrl Pts',(6.831815693,1.596957843,2.427499407));
#137545=CARTESIAN_POINT('Ctrl Pts',(6.852367211,1.607142857,2.368029478));
#137546=CARTESIAN_POINT('Ctrl Pts',(6.961387619,1.661171687,2.052557107));
#137547=CARTESIAN_POINT('Ctrl Pts',(7.040960579,1.716105035,1.72840219));
#137548=CARTESIAN_POINT('Ctrl Pts',(7.1256424,1.586734015,2.339918885));
#137549=CARTESIAN_POINT('Ctrl Pts',(7.145949953,1.596957843,2.278077271));
#137550=CARTESIAN_POINT('Ctrl Pts',(7.165181113,1.607142857,2.215892511));
#137551=CARTESIAN_POINT('Ctrl Pts',(7.267197371,1.661171687,1.886018673));
#137552=CARTESIAN_POINT('Ctrl Pts',(7.338472571,1.716105035,1.548166765));
#137553=CARTESIAN_POINT('',(7.1256424007853,1.58673401455508,2.33991888034589));
#137554=CARTESIAN_POINT('',(7.2827209820599,1.67637477916436,1.79219839630654));
#137555=CARTESIAN_POINT('Ctrl Pts',(7.1256424011666,1.58673401558733,2.33991888144739));
#137556=CARTESIAN_POINT('Ctrl Pts',(7.13919298701102,1.59355605166269,2.29865393432779));
#137557=CARTESIAN_POINT('Ctrl Pts',(7.15237286433238,1.60035948085477,2.25730851863362));
#137558=CARTESIAN_POINT('Ctrl Pts',(7.16518111287102,1.60714285699147,2.21589251110698));
#137559=CARTESIAN_POINT('Ctrl Pts',(7.20836009784246,1.63001087925354,2.0762714558123));
#137560=CARTESIAN_POINT('Ctrl Pts',(7.24759715930115,1.6531070630198,1.9349264571486));
#137561=CARTESIAN_POINT('Ctrl Pts',(7.28272098085021,1.67637477804653,1.79219840031975));
#137562=CARTESIAN_POINT('Ctrl Pts',(7.03982677420651,1.71532338701833,1.73301442804905));
#137563=CARTESIAN_POINT('Ctrl Pts',(7.08027830270189,1.70851142707053,1.74275295944677));
#137564=CARTESIAN_POINT('Ctrl Pts',(7.12076744301577,1.70186463321145,1.75256348237523));
#137565=CARTESIAN_POINT('Ctrl Pts',(7.20171741388181,1.68889233604349,1.77229153604284));
#137566=CARTESIAN_POINT('Ctrl Pts',(7.24222629826762,1.68255913651346,1.78222078597184));
#137567=CARTESIAN_POINT('Ctrl Pts',(7.28272098314211,1.67637477936909,1.79219839204119));
#137568=CARTESIAN_POINT('',(6.96793875314233,1.58673401368699,2.41326127537066));
#137569=CARTESIAN_POINT('Origin',(5.78096598369271E-13,1.67745375800033,
1.52221985016965E-13));
#137570=CARTESIAN_POINT('',(7.28100050215491,1.49654505820162,1.799175278978));
#137571=CARTESIAN_POINT('Origin',(-0.187346444560271,1.48214560241578,-0.0439026723522515));
#137572=CARTESIAN_POINT('',(7.39662051196621,1.5867340154113,1.24096938282043));
#137573=CARTESIAN_POINT('Origin',(-0.171923645285352,1.33942798281817,-0.0682813679420349));
#137574=CARTESIAN_POINT('Origin',(-0.188112242013981,1.48219937988002,-0.0145812322219743));
#137575=CARTESIAN_POINT('Ctrl Pts',(7.038707708,1.716084912,1.73755397));
#137576=CARTESIAN_POINT('Ctrl Pts',(7.133143264,1.651909459,1.355002242));
#137577=CARTESIAN_POINT('Ctrl Pts',(7.185561877,1.586734015,0.964469032));
#137578=CARTESIAN_POINT('Ctrl Pts',(7.18734732086528,1.58451405743156,0.951166979845766));
#137579=CARTESIAN_POINT('Ctrl Pts',(7.18913276473049,1.58229409986314,0.937864927691542));
#137580=CARTESIAN_POINT('Ctrl Pts',(7.21892121263256,1.716084912,2.0359042818088));
#137581=CARTESIAN_POINT('Ctrl Pts',(7.32957202130352,1.651909459,1.64355800234819));
#137582=CARTESIAN_POINT('Ctrl Pts',(7.39704884755691,1.586734015,1.24153053637962));
#137583=CARTESIAN_POINT('Ctrl Pts',(7.39934719309846,1.58451405743156,1.22783697541526));
#137584=CARTESIAN_POINT('Ctrl Pts',(7.40164553863998,1.58229409986314,1.21414341445083));
#137585=CARTESIAN_POINT('',(7.29109119514222,1.58673401622024,1.10271920244772));
#137586=CARTESIAN_POINT('Ctrl Pts',(7.18556187699999,1.586734015,0.964469031999999));
#137587=CARTESIAN_POINT('Ctrl Pts',(7.193932255,1.596957843,0.902107393));
#137588=CARTESIAN_POINT('Ctrl Pts',(7.201219013,1.607142857,0.839609869));
#137589=CARTESIAN_POINT('Ctrl Pts',(7.23987335,1.661171687,0.508076902));
#137590=CARTESIAN_POINT('Ctrl Pts',(7.247902213,1.716105035,0.174394712));
#137591=CARTESIAN_POINT('Ctrl Pts',(7.462062233,1.586734015,0.753410398));
#137592=CARTESIAN_POINT('Ctrl Pts',(7.468600888,1.596957843,0.688649083));
#137593=CARTESIAN_POINT('Ctrl Pts',(7.474014549,1.607142857,0.623784038));
#137594=CARTESIAN_POINT('Ctrl Pts',(7.502732599,1.661171687,0.279691987));
#137595=CARTESIAN_POINT('Ctrl Pts',(7.499713251,1.716105035,-0.065583193));
#137596=CARTESIAN_POINT('Ctrl Pts',(7.24778641104372,1.71532338698279,0.179142852969469));
#137597=CARTESIAN_POINT('Ctrl Pts',(7.28938567962167,1.70851143064064,0.17995781963721));
#137598=CARTESIAN_POINT('Ctrl Pts',(7.33103715327861,1.70186464057295,0.180835009060724));
#137599=CARTESIAN_POINT('Ctrl Pts',(7.41433555438445,1.68889233605274,0.182699982007276));
#137600=CARTESIAN_POINT('Ctrl Pts',(7.45603185895234,1.68255913649846,0.183688878893547));
#137601=CARTESIAN_POINT('Ctrl Pts',(7.49772469090217,1.67637477936472,0.184728053859447));
#137602=CARTESIAN_POINT('',(7.32381205594063,1.58673401368678,0.858939706979712));
#137603=CARTESIAN_POINT('Ctrl Pts',(7.247669375,1.716084912,0.183816829));
#137604=CARTESIAN_POINT('Ctrl Pts',(7.257659767,1.651909459,-0.210091905));
#137605=CARTESIAN_POINT('Ctrl Pts',(7.224899766,1.586734015,-0.602763118000001));
#137606=CARTESIAN_POINT('Ctrl Pts',(7.22439583072087,1.58573144465319,-0.608803437636323));
#137607=CARTESIAN_POINT('Ctrl Pts',(7.22389189544178,1.58472887430638,-0.614843757272649));
#137608=CARTESIAN_POINT('Ctrl Pts',(7.48753937345035,1.716084912,0.436170706964462));
#137609=CARTESIAN_POINT('Ctrl Pts',(7.51124512463293,1.651909459,0.0292251070795899));
#137610=CARTESIAN_POINT('Ctrl Pts',(7.49070676901871,1.586734015,-0.377892639641015));
#137611=CARTESIAN_POINT('Ctrl Pts',(7.49039083490232,1.58573144465319,-0.384155185094818));
#137612=CARTESIAN_POINT('Ctrl Pts',(7.49007490078591,1.58472887430638,-0.390417730548621));
#137613=CARTESIAN_POINT('',(7.357681566992,1.58673401622024,-0.490430843621259));
#137614=CARTESIAN_POINT('Ctrl Pts',(7.224899766,1.586734015,-0.602763118));
#137615=CARTESIAN_POINT('Ctrl Pts',(7.21966854,1.596957843,-0.665466161));
#137616=CARTESIAN_POINT('Ctrl Pts',(7.213349817,1.607142857,-0.728068964));
#137617=CARTESIAN_POINT('Ctrl Pts',(7.17983065,1.661171687,-1.060160415));
#137618=CARTESIAN_POINT('Ctrl Pts',(7.115939995,1.716105035,-1.387767269));
#137619=CARTESIAN_POINT('Ctrl Pts',(7.44956433,1.586734015,-0.868326722));
#137620=CARTESIAN_POINT('Ctrl Pts',(7.44202834600001,1.596957843,-0.93297957));
#137621=CARTESIAN_POINT('Ctrl Pts',(7.433371371,1.607142857,-0.997491884));
#137622=CARTESIAN_POINT('Ctrl Pts',(7.38744839,1.661171687,-1.339712786));
#137623=CARTESIAN_POINT('Ctrl Pts',(7.310275675,1.716105035,-1.676266553));
#137624=CARTESIAN_POINT('',(7.44956432875069,1.58673401455491,-0.868326726545714));
#137625=CARTESIAN_POINT('',(7.36214312592754,1.67637477918984,-1.43137995832493));
#137626=CARTESIAN_POINT('Ctrl Pts',(7.44956432956708,1.58673401558733,-0.868326725714101));
#137627=CARTESIAN_POINT('Ctrl Pts',(7.44453580649953,1.59355605166269,-0.911467520086966));
#137628=CARTESIAN_POINT('Ctrl Pts',(7.43913704964326,1.60035948085477,-0.954525689563659));
#137629=CARTESIAN_POINT('Ctrl Pts',(7.43337137100822,1.6071428569901,-0.997491883937084));
#137630=CARTESIAN_POINT('Ctrl Pts',(7.41393419733618,1.63001087925624,-1.14233890740316));
#137631=CARTESIAN_POINT('Ctrl Pts',(7.39019556503952,1.65310706303524,-1.28709536808967));
#137632=CARTESIAN_POINT('Ctrl Pts',(7.3621431265162,1.67637477806622,-1.43137995415095));
#137633=CARTESIAN_POINT('Ctrl Pts',(7.11684761016369,1.71532338701382,-1.38310524283572));
#137634=CARTESIAN_POINT('Ctrl Pts',(7.15764950362438,1.70851143085927,-1.39125194239245));
#137635=CARTESIAN_POINT('Ctrl Pts',(7.19851575811647,1.70186464089017,-1.39934909660988));
#137636=CARTESIAN_POINT('Ctrl Pts',(7.28026760508993,1.68889233603728,-1.41543442000141));
#137637=CARTESIAN_POINT('Ctrl Pts',(7.32120165656825,1.68255913652326,-1.42343211586704));
#137638=CARTESIAN_POINT('Ctrl Pts',(7.36214312511442,1.67637477939578,-1.43137996267382));
#137639=CARTESIAN_POINT('',(7.33723204719464,1.58673401368699,-0.735544928033687));
#137640=CARTESIAN_POINT('Origin',(1.43418263376383E-12,1.67745375799961,
-2.05998412772246E-13));
#137641=CARTESIAN_POINT('',(7.36351117796384,1.49654505843051,-1.42432549981701));
#137642=CARTESIAN_POINT('Origin',(-0.18846518142437,1.48214575541465,0.0388197040358929));
#137643=CARTESIAN_POINT('',(7.23406048264311,1.58673401497662,-1.97948703581295));
#137644=CARTESIAN_POINT('Origin',(-0.184704478899498,1.33942795330298,0.0102184252568263));
#137645=CARTESIAN_POINT('Origin',(-0.176848317883889,1.48219940476887,0.0657526625594348));
#137646=CARTESIAN_POINT('Ctrl Pts',(7.11773807800001,1.716084912,-1.378515382));
#137647=CARTESIAN_POINT('Ctrl Pts',(7.042816165,1.651909459,-1.765362388));
#137648=CARTESIAN_POINT('Ctrl Pts',(6.92640937100001,1.586734015,-2.141810735));
#137649=CARTESIAN_POINT('Ctrl Pts',(6.92244440913062,1.58451405737209,-2.1546330393549));
#137650=CARTESIAN_POINT('Ctrl Pts',(6.91847944726124,1.5822940997442,-2.16745534370988));
#137651=CARTESIAN_POINT('Ctrl Pts',(7.40656946861343,1.716084912,-1.18340965930295));
#137652=CARTESIAN_POINT('Ctrl Pts',(7.34225149637669,1.651909459,-1.5859545671548));
#137653=CARTESIAN_POINT('Ctrl Pts',(7.2346848528353,1.586734015,-1.97915759736593));
#137654=CARTESIAN_POINT('Ctrl Pts',(7.2310209976134,1.58451405737209,-1.99255058731215));
#137655=CARTESIAN_POINT('Ctrl Pts',(7.22735714239161,1.5822940997442,-2.00594357725841));
#137656=CARTESIAN_POINT('',(7.08023492586553,1.58673401622024,-2.06064888883387));
#137657=CARTESIAN_POINT('Ctrl Pts',(6.926409371,1.586734015,-2.141810735));
#137658=CARTESIAN_POINT('Ctrl Pts',(6.907821148,1.596957843,-2.201923256));
#137659=CARTESIAN_POINT('Ctrl Pts',(6.888192401,1.607142857,-2.261704102));
#137660=CARTESIAN_POINT('Ctrl Pts',(6.784067048,1.661171687,-2.578825809));
#137661=CARTESIAN_POINT('Ctrl Pts',(6.65124433100001,1.716105035,-2.885038794));
#137662=CARTESIAN_POINT('Ctrl Pts',(7.088733078,1.586734015,-2.449461849));
#137663=CARTESIAN_POINT('Ctrl Pts',(7.06747483,1.596957843,-2.510983136));
#137664=CARTESIAN_POINT('Ctrl Pts',(7.04515201,1.607142857,-2.572126194));
#137665=CARTESIAN_POINT('Ctrl Pts',(6.926735305,1.661171687,-2.896474078));
#137666=CARTESIAN_POINT('Ctrl Pts',(6.779017733,1.716105035,-3.208569553));
#137667=CARTESIAN_POINT('',(7.08873307580802,1.5867340145549,-2.44946185318096));
#137668=CARTESIAN_POINT('',(6.88231593134819,1.67637477914804,-2.98055823903319));
#137669=CARTESIAN_POINT('Ctrl Pts',(7.08873307677878,1.58673401558733,-2.44946185253421));
#137670=CARTESIAN_POINT('Ctrl Pts',(7.07454812228038,1.59355605166269,-2.49051305559517));
#137671=CARTESIAN_POINT('Ctrl Pts',(7.06001935183029,1.60035948085483,-2.53140397593767));
#137672=CARTESIAN_POINT('Ctrl Pts',(7.04515200990372,1.60714285702295,-2.57212619404686));
#137673=CARTESIAN_POINT('Ctrl Pts',(6.99503143785801,1.63001087938643,-2.70940835707287));
#137674=CARTESIAN_POINT('Ctrl Pts',(6.94072944202669,1.65310706300655,-2.84567738743838));
#137675=CARTESIAN_POINT('Ctrl Pts',(6.88231593282676,1.6763747780208,-2.98055823507385));
#137676=CARTESIAN_POINT('Ctrl Pts',(6.65313292476228,1.7153233870372,-2.88068087492377));
#137677=CARTESIAN_POINT('Ctrl Pts',(6.69122961548308,1.70851142685965,-2.8974083199357));
#137678=CARTESIAN_POINT('Ctrl Pts',(6.72939981587422,1.70186463283989,-2.91410121463492));
#137679=CARTESIAN_POINT('Ctrl Pts',(6.80578243382259,1.68889233601505,-2.94738468186202));
#137680=CARTESIAN_POINT('Ctrl Pts',(6.84404020187127,1.6825591364863,-2.9639950070758));
#137681=CARTESIAN_POINT('Ctrl Pts',(6.88231592961413,1.67637477935449,-2.98055824311748));
#137682=CARTESIAN_POINT('',(7.00757122198646,1.58673401368699,-2.29563629967273));
#137683=CARTESIAN_POINT('Origin',(-2.16406753628107E-13,1.67745375799956,
1.17961196366423E-13));
#137684=CARTESIAN_POINT('',(6.88516849880378,1.49654505841873,-2.9739628013933));
#137685=CARTESIAN_POINT('Origin',(-0.175713816965931,1.48214581178345,0.0784265254199706));
#137686=CARTESIAN_POINT('',(6.63940096982194,1.58673401497662,-3.48831689502028));
#137687=CARTESIAN_POINT('Origin',(-0.178189687439472,1.33942793954582,0.049685594845269));
#137688=CARTESIAN_POINT('Origin',(-0.158578871248328,1.48219936885196,0.102232585110383));
#137689=CARTESIAN_POINT('Ctrl Pts',(6.65498925800001,1.716084912,-2.876389747));
#137690=CARTESIAN_POINT('Ctrl Pts',(6.498658307,1.651909459,-3.238086488));
#137691=CARTESIAN_POINT('Ctrl Pts',(6.304047773,1.586734015,-3.580709661));
#137692=CARTESIAN_POINT('Ctrl Pts',(6.29741909342054,1.58451405739623,-3.59237983724195));
#137693=CARTESIAN_POINT('Ctrl Pts',(6.29079041384104,1.58229409979248,-3.60405001348384));
#137694=CARTESIAN_POINT('Ctrl Pts',(6.97900989538563,1.716084912,-2.74793569772402));
#137695=CARTESIAN_POINT('Ctrl Pts',(6.8296603852941,1.651909459,-3.12724286712408));
#137696=CARTESIAN_POINT('Ctrl Pts',(6.64008156230396,1.586734015,-3.48812937990261));
#137697=CARTESIAN_POINT('Ctrl Pts',(6.63362426913067,1.58451405739623,-3.50042162846999));
#137698=CARTESIAN_POINT('Ctrl Pts',(6.62716697595724,1.58229409979248,-3.51271387703745));
#137699=CARTESIAN_POINT('',(6.47172436983887,1.58673401622024,-3.53451328120357));
#137700=CARTESIAN_POINT('Ctrl Pts',(6.304047773,1.586734015,-3.580709661));
#137701=CARTESIAN_POINT('Ctrl Pts',(6.27297171700001,1.596957843,-3.635420867));
#137702=CARTESIAN_POINT('Ctrl Pts',(6.240950764,1.607142857,-3.68958447));
#137703=CARTESIAN_POINT('Ctrl Pts',(6.07108801100001,1.661171687,-3.976908175));
#137704=CARTESIAN_POINT('Ctrl Pts',(5.875543876,1.716105035,-4.247409112));
#137705=CARTESIAN_POINT('Ctrl Pts',(6.396440546,1.586734015,-3.916062862));
#137706=CARTESIAN_POINT('Ctrl Pts',(6.362454046,1.596957843,-3.971575921));
#137707=CARTESIAN_POINT('Ctrl Pts',(6.327509171,1.607142857,-4.026490742));
#137708=CARTESIAN_POINT('Ctrl Pts',(6.142135775,1.661171687,-4.317799462));
#137709=CARTESIAN_POINT('Ctrl Pts',(5.930780456,1.716105035,-4.590843406));
#137710=CARTESIAN_POINT('',(6.3964405427229,1.58673401455097,-3.91606286599164));
#137711=CARTESIAN_POINT('',(6.08067929234869,1.67637477917653,-4.39036892940065));
#137712=CARTESIAN_POINT('Ctrl Pts',(6.39644054404754,1.58673401558734,-3.91606286518912));
#137713=CARTESIAN_POINT('Ctrl Pts',(6.3737624307921,1.5935560516627,-3.9531049683109));
#137714=CARTESIAN_POINT('Ctrl Pts',(6.35078299580488,1.60035948085484,-3.98991662567754));
#137715=CARTESIAN_POINT('Ctrl Pts',(6.32750917087876,1.60714285702463,-4.02649074198977));
#137716=CARTESIAN_POINT('Ctrl Pts',(6.24904878270096,1.63001087940218,-4.14978888302909));
#137717=CARTESIAN_POINT('Ctrl Pts',(6.16672252380312,1.65310706302945,-4.2711986954548));
#137718=CARTESIAN_POINT('Ctrl Pts',(6.08067929460951,1.67637477806564,-4.39036892590092));
#137719=CARTESIAN_POINT('Ctrl Pts',(5.87832513927852,1.71532338701635,-4.2435590700475));
#137720=CARTESIAN_POINT('Ctrl Pts',(5.91193524335975,1.70851142698047,-4.26808509887298));
#137721=CARTESIAN_POINT('Ctrl Pts',(5.94562456606603,1.70186463304736,-4.2925931876029));
#137722=CARTESIAN_POINT('Ctrl Pts',(6.01306643993702,1.68889233602917,-4.34151851184358));
#137723=CARTESIAN_POINT('Ctrl Pts',(6.04685903352462,1.68255913651325,-4.36596478612269));
#137724=CARTESIAN_POINT('Ctrl Pts',(6.08067928981379,1.67637477938004,-4.39036893296519));
#137725=CARTESIAN_POINT('',(6.35024415539573,1.58673401368695,-3.74838626845317));
#137726=CARTESIAN_POINT('Origin',(-1.10154940724527E-13,1.67745375800039,
4.33680868994202E-15));
#137727=CARTESIAN_POINT('',(6.08488299311142,1.49654505834991,-4.38454090602216));
#137728=CARTESIAN_POINT('Origin',(-0.154746378784828,1.48214577664056,0.114366264112796));
#137729=CARTESIAN_POINT('',(5.73429044748078,1.58673401540867,-4.83403693234886));
#137730=CARTESIAN_POINT('Origin',(-0.163342471950216,1.33942798155973,0.0868292586961655));
#137731=CARTESIAN_POINT('Origin',(-0.132894531346506,1.4821993605615,0.133932321928627));
#137732=CARTESIAN_POINT('Ctrl Pts',(5.881060538,1.716084912,-4.239767323));
#137733=CARTESIAN_POINT('Ctrl Pts',(5.65063041,1.651909459,-4.559401263));
#137734=CARTESIAN_POINT('Ctrl Pts',(5.386915907,1.586734015,-4.852178584));
#137735=CARTESIAN_POINT('Ctrl Pts',(5.37793345927031,1.58451405738548,-4.86215094787234));
#137736=CARTESIAN_POINT('Ctrl Pts',(5.3689510115405,1.58229409977099,-4.87212331174469));
#137737=CARTESIAN_POINT('Ctrl Pts',(6.22511957529754,1.716084912,-4.18397131818438));
#137738=CARTESIAN_POINT('Ctrl Pts',(5.99772194418561,1.651909459,-4.5223047663597));
#137739=CARTESIAN_POINT('Ctrl Pts',(5.73499543622806,1.586734015,-4.83400011010498));
#137740=CARTESIAN_POINT('Ctrl Pts',(5.72604664085241,1.58451405738548,-4.84461684563125));
#137741=CARTESIAN_POINT('Ctrl Pts',(5.71709784547668,1.58229409977099,-4.8552335811575));
#137742=CARTESIAN_POINT('',(5.56060317398339,1.58673401622024,-4.84310776175981));
#137743=CARTESIAN_POINT('Ctrl Pts',(5.386915907,1.586734015,-4.852178584));
#137744=CARTESIAN_POINT('Ctrl Pts',(5.3448051,1.596957843,-4.898930239));
#137745=CARTESIAN_POINT('Ctrl Pts',(5.301889206,1.607142857,-4.944943968));
#137746=CARTESIAN_POINT('Ctrl Pts',(5.074231646,1.661171687,-5.189034734));
#137747=CARTESIAN_POINT('Ctrl Pts',(4.825109518,1.716105035,-5.411175301));
#137748=CARTESIAN_POINT('Ctrl Pts',(5.405057563,1.586734015,-5.199553129));
#137749=CARTESIAN_POINT('Ctrl Pts',(5.359931982,1.596957843,-5.24646223));
#137750=CARTESIAN_POINT('Ctrl Pts',(5.313999035,1.607142857,-5.292581058));
#137751=CARTESIAN_POINT('Ctrl Pts',(5.070336803,1.661171687,-5.537229341));
#137752=CARTESIAN_POINT('Ctrl Pts',(4.805226477,1.716105035,-5.758454524));
#137753=CARTESIAN_POINT('',(5.40505755925514,1.5867340145549,-5.19955313187524));
#137754=CARTESIAN_POINT('',(4.99471684849644,1.67637477913455,-5.59489084771419));
#137755=CARTESIAN_POINT('Ctrl Pts',(5.40505756040768,1.58673401558733,-5.19955313169478));
#137756=CARTESIAN_POINT('Ctrl Pts',(5.37494669178826,1.59355605166269,-5.23085408659786));
#137757=CARTESIAN_POINT('Ctrl Pts',(5.34459108494202,1.6003594808547,-5.26186520844752));
#137758=CARTESIAN_POINT('Ctrl Pts',(5.31399903520763,1.60714285695396,-5.29258105779153));
#137759=CARTESIAN_POINT('Ctrl Pts',(5.21086755313719,1.63001087907978,-5.39612989179284));
#137760=CARTESIAN_POINT('Ctrl Pts',(5.10436651448534,1.65310706299861,-5.49700349882506));
#137761=CARTESIAN_POINT('Ctrl Pts',(4.99471685148991,1.67637477801125,-5.59489084475157));
#137762=CARTESIAN_POINT('Ctrl Pts',(4.82865340178371,1.71532338709796,-5.40801315987009));
#137763=CARTESIAN_POINT('Ctrl Pts',(4.8562053335994,1.70851143095389,-5.43919094458338));
#137764=CARTESIAN_POINT('Ctrl Pts',(4.88383848635188,1.7018646410062,-5.47036823620498));
#137765=CARTESIAN_POINT('Ctrl Pts',(4.93918614250612,1.68889233601318,-5.53264776102485));
#137766=CARTESIAN_POINT('Ctrl Pts',(4.96693345785353,1.68255913648008,-5.56378690379754));
#137767=CARTESIAN_POINT('Ctrl Pts',(4.9947168452189,1.67637477934025,-5.59489085068274));
#137768=CARTESIAN_POINT('',(5.39598672949708,1.58673401368699,-5.02586586240818));
#137769=CARTESIAN_POINT('Origin',(1.14491749414469E-12,1.67745375800011,
-1.23555679576448E-12));
#137770=CARTESIAN_POINT('',(5.00007512100252,1.49654505843305,-5.59010275254307));
#137771=CARTESIAN_POINT('Origin',(-0.126543208156581,1.48214574783257,0.144958432986629));
#137772=CARTESIAN_POINT('',(4.56105087436642,1.58673401497662,-5.95372277775556));
#137773=CARTESIAN_POINT('Origin',(-0.140857935027798,1.33942800656016,0.119913108632639));
#137774=CARTESIAN_POINT('Origin',(-0.100995901576229,1.48219934910415,0.159369293085917));
#137775=CARTESIAN_POINT('Ctrl Pts',(4.832139962,1.716084912,-5.404898092));
#137776=CARTESIAN_POINT('Ctrl Pts',(4.53838531400001,1.651909459,-5.667523501));
#137777=CARTESIAN_POINT('Ctrl Pts',(4.21789784,1.586734015,-5.896765029));
#137778=CARTESIAN_POINT('Ctrl Pts',(4.20698163327222,1.58451405734799,-5.90457328396551));
#137779=CARTESIAN_POINT('Ctrl Pts',(4.19606542654451,1.58229409969599,-5.91238153893092));
#137780=CARTESIAN_POINT('Ctrl Pts',(5.18014958365216,1.716084912,-5.42436908871552));
#137781=CARTESIAN_POINT('Ctrl Pts',(4.88533669233185,1.651909459,-5.7059087207657));
#137782=CARTESIAN_POINT('Ctrl Pts',(4.56174729883813,1.586734015,-5.95383836687271));
#137783=CARTESIAN_POINT('Ctrl Pts',(4.55072543682834,1.58451405734799,-5.96228316266166));
#137784=CARTESIAN_POINT('Ctrl Pts',(4.53970357481859,1.58229409969599,-5.97072795845062));
#137785=CARTESIAN_POINT('',(4.38947435436249,1.58673401622024,-5.92524390554672));
#137786=CARTESIAN_POINT('Ctrl Pts',(4.21789784,1.586734015,-5.896765029));
#137787=CARTESIAN_POINT('Ctrl Pts',(4.166721337,1.596957843,-5.933371077));
#137788=CARTESIAN_POINT('Ctrl Pts',(4.114917201,1.607142857,-5.969083383));
#137789=CARTESIAN_POINT('Ctrl Pts',(3.840109849,1.661171687,-6.158527796));
#137790=CARTESIAN_POINT('Ctrl Pts',(3.549058402,1.716105035,-6.32192094700001));
#137791=CARTESIAN_POINT('Ctrl Pts',(4.160940096,1.586734015,-6.23991807));
#137792=CARTESIAN_POINT('Ctrl Pts',(4.106785456,1.596957843,-6.276029796));
#137793=CARTESIAN_POINT('Ctrl Pts',(4.052012211,1.607142857,-6.311196166));
#137794=CARTESIAN_POINT('Ctrl Pts',(3.761454517,1.661171687,-6.49774453));
#137795=CARTESIAN_POINT('Ctrl Pts',(3.454985449,1.716105035,-6.656806708));
#137796=CARTESIAN_POINT('',(4.16094009122312,1.58673401412031,-6.23991807225148));
#137797=CARTESIAN_POINT('',(3.6752069964955,1.67637478034391,-6.5378018882331));
#137798=CARTESIAN_POINT('Ctrl Pts',(4.1609400924762,1.58673401434335,-6.23991807212436));
#137799=CARTESIAN_POINT('Ctrl Pts',(4.12480441948581,1.59355605125273,-6.26401428120538));
#137800=CARTESIAN_POINT('Ctrl Pts',(4.08849203547424,1.60035948085479,-6.28777482204739));
#137801=CARTESIAN_POINT('Ctrl Pts',(4.05201221122053,1.60714285723681,-6.31119616555529));
#137802=CARTESIAN_POINT('Ctrl Pts',(3.9290319461485,1.63001087929038,-6.39015386592446));
#137803=CARTESIAN_POINT('Ctrl Pts',(3.80333600022774,1.65310706412051,-6.46577452826259));
#137804=CARTESIAN_POINT('Ctrl Pts',(3.67520700022725,1.67637478135681,-6.5378018863744));
#137805=CARTESIAN_POINT('Ctrl Pts',(3.55319919884997,1.71532338706032,-6.31959456502606));
#137806=CARTESIAN_POINT('Ctrl Pts',(3.57340469129327,1.70851142706105,-6.35596630201538));
#137807=CARTESIAN_POINT('Ctrl Pts',(3.5936896134933,1.70186463310274,-6.39235502044082));
#137808=CARTESIAN_POINT('Ctrl Pts',(3.63435499056764,1.68889233603733,-6.46507655017275));
#137809=CARTESIAN_POINT('Ctrl Pts',(3.65475959393252,1.68255913648579,-6.50145252979146));
#137810=CARTESIAN_POINT('Ctrl Pts',(3.67520699193589,1.67637477935762,-6.53780189063019));
#137811=CARTESIAN_POINT('',(4.18941896135415,1.58673401368669,-6.06834155408811));
#137812=CARTESIAN_POINT('Origin',(3.68411898210574E-13,1.67745375799978,
-6.76975836499949E-13));
#137813=CARTESIAN_POINT('',(3.68146929365968,1.4965450583892,-6.53427760673528));
#137814=CARTESIAN_POINT('Origin',(-0.0924228176382863,1.48214577209747,
0.168772261139138));
#137815=CARTESIAN_POINT('',(3.17454163251369,1.58673401497662,-6.79501916224933));
#137816=CARTESIAN_POINT('Origin',(-0.111786908323656,1.33942794745275,0.147389747057465));
#137817=CARTESIAN_POINT('Origin',(-0.0643749739487942,1.48219938687106,
0.17735442406437));
#137818=CARTESIAN_POINT('Ctrl Pts',(3.557273893,1.716084912,-6.317301833));
#137819=CARTESIAN_POINT('Ctrl Pts',(3.213930366,1.651909459,-6.51063864));
#137820=CARTESIAN_POINT('Ctrl Pts',(2.851655559,1.586734015,-6.665625295));
#137821=CARTESIAN_POINT('Ctrl Pts',(2.83931602349466,1.58451405741593,-6.67090433537289));
#137822=CARTESIAN_POINT('Ctrl Pts',(2.82697648798927,1.58229409983188,-6.67618337574564));
#137823=CARTESIAN_POINT('Ctrl Pts',(3.89296155426518,1.716084912,-6.41112939027493));
#137824=CARTESIAN_POINT('Ctrl Pts',(3.54451852595587,1.651909459,-6.62271072495192));
#137825=CARTESIAN_POINT('Ctrl Pts',(3.1751969266877,1.586734015,-6.79528175959364));
#137826=CARTESIAN_POINT('Ctrl Pts',(3.162617368576,1.58451405741593,-6.80115974605037));
#137827=CARTESIAN_POINT('Ctrl Pts',(3.15003781046428,1.58229409983188,-6.8070377325071));
#137828=CARTESIAN_POINT('',(3.01309859252858,1.58673401622024,-6.73032223012104));
#137829=CARTESIAN_POINT('Ctrl Pts',(2.851655559,1.586734015,-6.665625295));
#137830=CARTESIAN_POINT('Ctrl Pts',(2.793806315,1.596957843,-6.690374079));
#137831=CARTESIAN_POINT('Ctrl Pts',(2.735536241,1.607142857,-6.714115092));
#137832=CARTESIAN_POINT('Ctrl Pts',(2.426428783,1.661171687,-6.840054943));
#137833=CARTESIAN_POINT('Ctrl Pts',(2.10705726,1.716105035,-6.937060595));
#137834=CARTESIAN_POINT('Ctrl Pts',(2.722261695,1.586734015,-6.988511377));
#137835=CARTESIAN_POINT('Ctrl Pts',(2.661610206,1.596957843,-7.012137184));
#137836=CARTESIAN_POINT('Ctrl Pts',(2.600557799,1.607142857,-7.034706755));
#137837=CARTESIAN_POINT('Ctrl Pts',(2.276690798,1.661171687,-7.154432408));
#137838=CARTESIAN_POINT('Ctrl Pts',(1.94319314,1.716105035,-7.243894009));
#137839=CARTESIAN_POINT('',(2.72226169039777,1.5867340145549,-6.9885113780276));
#137840=CARTESIAN_POINT('',(2.1838485481367,1.67637477913636,-7.17501257923925));
#137841=CARTESIAN_POINT('Ctrl Pts',(2.72226169151576,1.58673401558733,-6.98851137835724));
#137842=CARTESIAN_POINT('Ctrl Pts',(2.68179087705114,1.59355605166269,-7.00427612982548));
#137843=CARTESIAN_POINT('Ctrl Pts',(2.64121964210082,1.60035948085471,-7.01967507320326));
#137844=CARTESIAN_POINT('Ctrl Pts',(2.60055779923287,1.60714285696172,-7.03470675490712));
#137845=CARTESIAN_POINT('Ctrl Pts',(2.4634791737446,1.63001087911566,-7.08538134630581));
#137846=CARTESIAN_POINT('Ctrl Pts',(2.32446572072597,1.65310706299496,-7.13221312719443));
#137847=CARTESIAN_POINT('Ctrl Pts',(2.18384855217046,1.67637477799263,-7.17501257778031));
#137848=CARTESIAN_POINT('Ctrl Pts',(2.11160135108966,1.71532338690958,-6.93567875205951));
#137849=CARTESIAN_POINT('Ctrl Pts',(2.12351559544664,1.70851143053091,-6.97554370062043));
#137850=CARTESIAN_POINT('Ctrl Pts',(2.13550376091455,1.70186464041742,-7.01544230514015));
#137851=CARTESIAN_POINT('Ctrl Pts',(2.15958543818596,1.68889233600329,-7.09520554538441));
#137852=CARTESIAN_POINT('Ctrl Pts',(2.17169323280053,1.6825591364667,-7.13511746140698));
#137853=CARTESIAN_POINT('Ctrl Pts',(2.18384854383863,1.67637477934591,-7.17501258058127));
#137854=CARTESIAN_POINT('',(2.7869586195249,1.58673401368699,-6.8270683390515));
#137855=CARTESIAN_POINT('Origin',(4.42679747025831E-13,1.67745375799939,
-1.495765317161E-12));
#137856=CARTESIAN_POINT('',(2.19072205418073,1.49654505837267,-7.17291690205873));
#137857=CARTESIAN_POINT('Origin',(-0.0539810490203899,1.48214576132564,
0.184694844397544));
#137858=CARTESIAN_POINT('',(1.63959435298178,1.58673401497662,-7.31858800252645));
#137859=CARTESIAN_POINT('Origin',(-0.0774889774619666,1.33942798701671,
0.167974844422635));
#137860=CARTESIAN_POINT('Origin',(-0.0247439678196198,1.48219933560951,
0.187046733158217));
#137861=CARTESIAN_POINT('Ctrl Pts',(2.116073651,1.716084912,-6.93431556100001));
#137862=CARTESIAN_POINT('Ctrl Pts',(1.739195605,1.651909459,-7.049323552));
#137863=CARTESIAN_POINT('Ctrl Pts',(1.352073032,1.586734015,-7.122808331));
#137864=CARTESIAN_POINT('Ctrl Pts',(1.33888715021876,1.58451405739596,-7.1253113150061));
#137865=CARTESIAN_POINT('Ctrl Pts',(1.32570126843754,1.58229409979194,-7.12781429901219));
#137866=CARTESIAN_POINT('Ctrl Pts',(2.42374296913084,1.716084912,-7.09811240704809));
#137867=CARTESIAN_POINT('Ctrl Pts',(2.03796261177443,1.651909459,-7.22984213653404));
#137868=CARTESIAN_POINT('Ctrl Pts',(1.64017787609125,1.586734015,-7.3189853294083));
#137869=CARTESIAN_POINT('Ctrl Pts',(1.62662882763753,1.58451405739596,-7.32202165868699));
#137870=CARTESIAN_POINT('Ctrl Pts',(1.61307977918388,1.58229409979194,-7.32505798796576));
#137871=CARTESIAN_POINT('',(1.49583368902063,1.58673401622024,-7.22069816754942));
#137872=CARTESIAN_POINT('Ctrl Pts',(1.352073032,1.586734015,-7.122808331));
#137873=CARTESIAN_POINT('Ctrl Pts',(1.290256015,1.596957843,-7.134542624));
#137874=CARTESIAN_POINT('Ctrl Pts',(1.228244647,1.607142857,-7.145202243));
#137875=CARTESIAN_POINT('Ctrl Pts',(0.899290605,1.661171687,-7.201748723));
#137876=CARTESIAN_POINT('Ctrl Pts',(0.566532463,1.716105035,-7.227831));
#137877=CARTESIAN_POINT('Ctrl Pts',(1.156293362,1.586734015,-7.410329659));
#137878=CARTESIAN_POINT('Ctrl Pts',(1.091981021,1.596957843,-7.42036483100001));
#137879=CARTESIAN_POINT('Ctrl Pts',(1.027504195,1.607142857,-7.429282275));
#137880=CARTESIAN_POINT('Ctrl Pts',(0.685471549000001,1.661171687,-7.476586977));
#137881=CARTESIAN_POINT('Ctrl Pts',(0.340539281,1.716105035,-7.492264878));
#137882=CARTESIAN_POINT('',(1.15629335682412,1.58673401455096,-7.41032965909313));
#137883=CARTESIAN_POINT('',(0.590375770590217,1.67637477916754,-7.47672765614166));
#137884=CARTESIAN_POINT('Ctrl Pts',(1.15629335830546,1.58673401558733,-7.41032965957648));
#137885=CARTESIAN_POINT('Ctrl Pts',(1.11337977344535,1.59355605166269,-7.41702581146744));
#137886=CARTESIAN_POINT('Ctrl Pts',(1.0704467538818,1.60035948085471,-7.42334311999044));
#137887=CARTESIAN_POINT('Ctrl Pts',(1.02750419524604,1.60714285696113,-7.42928227496597));
#137888=CARTESIAN_POINT('Ctrl Pts',(0.882736852912321,1.63001087912203,
-7.44930427014739));
#137889=CARTESIAN_POINT('Ctrl Pts',(0.736906008782792,1.65310706302017,
-7.46515736687437));
#137890=CARTESIAN_POINT('Ctrl Pts',(0.590375774770585,1.6763747780432,-7.47672765559436));
#137891=CARTESIAN_POINT('Ctrl Pts',(0.571267370680839,1.71532338695618,
-7.22745830928171));
#137892=CARTESIAN_POINT('Ctrl Pts',(0.574333282776174,1.70851142694226,
-7.26895247004213));
#137893=CARTESIAN_POINT('Ctrl Pts',(0.577464153095201,1.70186463307537,
-7.31049539372416));
#137894=CARTESIAN_POINT('Ctrl Pts',(0.583836071793672,1.68889233605644,
-7.39357061501269));
#137895=CARTESIAN_POINT('Ctrl Pts',(0.587080910820238,1.68255913651965,
-7.43515223045215));
#137896=CARTESIAN_POINT('Ctrl Pts',(0.590375766180676,1.67637477937349,
-7.47672765652176));
#137897=CARTESIAN_POINT('',(1.25418318904368,1.58673401368699,-7.26656899637323));
#137898=CARTESIAN_POINT('Origin',(1.03483709231952E-13,1.67745375799956,
-1.06902334207071E-12));
#137899=CARTESIAN_POINT('',(0.597539085963974,1.49654505840547,-7.47615857508329));
#137900=CARTESIAN_POINT('Origin',(-0.0130150326916503,1.48214575193959,
0.191980769349778));
#137901=CARTESIAN_POINT('',(0.0279814687171162,1.58673401541125,-7.49994780268285));
#137902=CARTESIAN_POINT('Origin',(-0.0395677149432771,1.33942796522644,
0.180705713823447));
#137903=CARTESIAN_POINT('Origin',(0.0160440422792048,1.48219934306306,0.187993145569987));
#137904=CARTESIAN_POINT('Ctrl Pts',(0.575928156,1.716084912,-7.227088401));
#137905=CARTESIAN_POINT('Ctrl Pts',(0.183137991,1.651909459,-7.25838993));
#137906=CARTESIAN_POINT('Ctrl Pts',(-0.210730926,1.586734015,-7.246936765));
#137907=CARTESIAN_POINT('Ctrl Pts',(-0.224146596640912,1.58451405741299,
-7.24654665579665));
#137908=CARTESIAN_POINT('Ctrl Pts',(-0.237562267281824,1.582294099826,-7.24615654659332));
#137909=CARTESIAN_POINT('Ctrl Pts',(0.841192856648398,1.716084912,-7.45319557669144));
#137910=CARTESIAN_POINT('Ctrl Pts',(0.436113832324383,1.651909459,-7.49891416437837));
#137911=CARTESIAN_POINT('Ctrl Pts',(0.0284659309655903,1.586734015,-7.50046127958347));
#137912=CARTESIAN_POINT('Ctrl Pts',(0.0145809307890254,1.58451405741299,
-7.50051397627298));
#137913=CARTESIAN_POINT('Ctrl Pts',(0.000695930612460646,1.582294099826,
-7.5005666729626));
#137914=CARTESIAN_POINT('',(-0.091374734637584,1.58673401622024,-7.37344228340535));
#137915=CARTESIAN_POINT('Ctrl Pts',(-0.210730926,1.586734015,-7.24693676500001));
#137916=CARTESIAN_POINT('Ctrl Pts',(-0.273625222,1.596957843,-7.245107886));
#137917=CARTESIAN_POINT('Ctrl Pts',(-0.336478302,1.607142857,-7.242187677));
#137918=CARTESIAN_POINT('Ctrl Pts',(-0.669897403,1.661171687,-7.226696737));
#137919=CARTESIAN_POINT('Ctrl Pts',(-1.000482763,1.716105035,-7.18063606100001));
#137920=CARTESIAN_POINT('Ctrl Pts',(-0.463741963,1.586734015,-7.48564916300001));
#137921=CARTESIAN_POINT('Ctrl Pts',(-0.528707983,1.596957843,-7.481624466));
#137922=CARTESIAN_POINT('Ctrl Pts',(-0.593594363,1.607142857,-7.476472814));
#137923=CARTESIAN_POINT('Ctrl Pts',(-0.937799589,1.661171687,-7.449144649));
#137924=CARTESIAN_POINT('Ctrl Pts',(-1.278037818,1.716105035,-7.390305767));
#137925=CARTESIAN_POINT('',(-0.463741967621627,1.58673401455466,-7.48564916200989));
#137926=CARTESIAN_POINT('',(-1.0307023228524,1.67637477913704,-7.42883925771828));
#137927=CARTESIAN_POINT('Ctrl Pts',(-0.463741966734078,1.58673401558764,
-7.48564916276868));
#137928=CARTESIAN_POINT('Ctrl Pts',(-0.507091730847073,1.59355605166279,
-7.48296361012152));
#137929=CARTESIAN_POINT('Ctrl Pts',(-0.550379034849969,1.60035948085491,
-7.47990389355397));
#137930=CARTESIAN_POINT('Ctrl Pts',(-0.593594363123317,1.60714285706055,
-7.47647281373026));
#137931=CARTESIAN_POINT('Ctrl Pts',(-0.739281263995284,1.63001087954842,
-7.4649060051311));
#137932=CARTESIAN_POINT('Ctrl Pts',(-0.885110609776605,1.6531070629954,
-7.44903914546373));
#137933=CARTESIAN_POINT('Ctrl Pts',(-1.03070231858164,1.67637477799372,
-7.42883925808922));
#137934=CARTESIAN_POINT('Ctrl Pts',(-0.995778437805123,1.71532338707607,
-7.18128994846951));
#137935=CARTESIAN_POINT('Ctrl Pts',(-1.00170422311022,1.70851142698573,
-7.22247307939769));
#137936=CARTESIAN_POINT('Ctrl Pts',(-1.00757705150579,1.70186463299444,
-7.26371779773764));
#137937=CARTESIAN_POINT('Ctrl Pts',(-1.01921282155258,1.68889233601896,
-7.34622054014056));
#137938=CARTESIAN_POINT('Ctrl Pts',(-1.0249826632171,1.68255913647026,-7.38752754502936));
#137939=CARTESIAN_POINT('Ctrl Pts',(-1.0307023273142,1.67637477934645,-7.42883925713188));
#137940=CARTESIAN_POINT('',(-0.337236452569776,1.58673401368629,-7.36629296363056));
#137941=CARTESIAN_POINT('Origin',(3.81991530420955E-13,1.67745375799972,
2.79160375371568E-12));
#137942=CARTESIAN_POINT('',(-1.02358414613805,1.49654505839789,-7.42982338246688));
#137943=CARTESIAN_POINT('Origin',(0.0285594814258901,1.4821457438531,0.190290540546657));
#137944=CARTESIAN_POINT('',(-1.58493980789077,1.58673401497662,-7.33061837789233));
#137945=CARTESIAN_POINT('Origin',(0.000203747006136679,1.33942799327937,
0.184986838896626));
#137946=CARTESIAN_POINT('Origin',(0.0560818439985851,1.48219938129434,0.180148667665314));
#137947=CARTESIAN_POINT('Ctrl Pts',(-0.9911471,1.716084912,-7.18193062000001));
#137948=CARTESIAN_POINT('Ctrl Pts',(-1.381482952,1.651909459,-7.128062062));
#137949=CARTESIAN_POINT('Ctrl Pts',(-1.763681341,1.586734015,-7.032206491));
#137950=CARTESIAN_POINT('Ctrl Pts',(-1.77669949876394,1.5845140574158,-7.02894152970832));
#137951=CARTESIAN_POINT('Ctrl Pts',(-1.78971765652795,1.58229409983161,
-7.02567656841653));
#137952=CARTESIAN_POINT('Ctrl Pts',(-0.780690499306596,1.716084912,-7.45977560420975));
#137953=CARTESIAN_POINT('Ctrl Pts',(-1.18612714580241,1.651909459,-7.41734530175765));
#137954=CARTESIAN_POINT('Ctrl Pts',(-1.58457704991799,1.586734015,-7.33122399711957));
#137955=CARTESIAN_POINT('Ctrl Pts',(-1.59814875472392,1.5845140574158,-7.32829059718152));
#137956=CARTESIAN_POINT('Ctrl Pts',(-1.61172045952986,1.58229409983162,
-7.32535719724342));
#137957=CARTESIAN_POINT('',(-1.67431057793867,1.58673401622024,-7.18141243376571));
#137958=CARTESIAN_POINT('Ctrl Pts',(-1.763681341,1.586734015,-7.03220649099999));
#137959=CARTESIAN_POINT('Ctrl Pts',(-1.824712048,1.596957843,-7.01689995500001));
#137960=CARTESIAN_POINT('Ctrl Pts',(-1.885467899,1.607142857,-7.000536465));
#137961=CARTESIAN_POINT('Ctrl Pts',(-2.207761753,1.661171687,-6.913732444));
#137962=CARTESIAN_POINT('Ctrl Pts',(-2.520716527,1.716105035,-6.79768256));
#137963=CARTESIAN_POINT('Ctrl Pts',(-2.06209323,1.586734015,-7.210948031));
#137964=CARTESIAN_POINT('Ctrl Pts',(-2.124675189,1.596957843,-7.193051656));
#137965=CARTESIAN_POINT('Ctrl Pts',(-2.186937109,1.607142857,-7.174071792));
#137966=CARTESIAN_POINT('Ctrl Pts',(-2.51722026,1.661171687,-7.073388596));
#137967=CARTESIAN_POINT('Ctrl Pts',(-2.836855288,1.716105035,-6.94278417300001));
#137968=CARTESIAN_POINT('',(-2.06209323492603,1.58673401411967,-7.21094802900619));
#137969=CARTESIAN_POINT('',(-2.60358592031819,1.6763747803427,-7.03358659236033));
#137970=CARTESIAN_POINT('Ctrl Pts',(-2.06209323404642,1.58673401434289,
-7.21094803018993));
#137971=CARTESIAN_POINT('Ctrl Pts',(-2.10385218957466,1.59355605125258,
-7.19900634661447));
#137972=CARTESIAN_POINT('Ctrl Pts',(-2.14546971161618,1.60035948085479,
-7.1867126736392));
#137973=CARTESIAN_POINT('Ctrl Pts',(-2.18693710880305,1.60714285723704,
-7.17407179237427));
#137974=CARTESIAN_POINT('Ctrl Pts',(-2.32673140886269,1.63001087929119,
-7.1314570331068));
#137975=CARTESIAN_POINT('Ctrl Pts',(-2.46574043981844,1.65310706412132,
-7.0846121322515));
#137976=CARTESIAN_POINT('Ctrl Pts',(-2.60358591652084,1.67637478135681,
-7.03358659399984));
#137977=CARTESIAN_POINT('Ctrl Pts',(-2.51626275262574,1.7153233870309,-6.79933245094728));
#137978=CARTESIAN_POINT('Ctrl Pts',(-2.53090315232834,1.70851142686521,
-6.83827887509107));
#137979=CARTESIAN_POINT('Ctrl Pts',(-2.54550507265091,1.7018646328347,-6.87729683070493));
#137980=CARTESIAN_POINT('Ctrl Pts',(-2.57460445544453,1.68889233602686,
-6.9553693573294));
#137981=CARTESIAN_POINT('Ctrl Pts',(-2.58911918650035,1.6825591364838,-6.99447028196159));
#137982=CARTESIAN_POINT('Ctrl Pts',(-2.60358592505921,1.6763747793587,-7.03358659045134));
#137983=CARTESIAN_POINT('',(-1.91288729330474,1.58673401368578,-7.12157725890361));
#137984=CARTESIAN_POINT('Origin',(2.82326245715225E-13,1.67745375799956,
7.75855074630627E-13));
#137985=CARTESIAN_POINT('',(-2.59684572075915,1.49654505838387,-7.03607790633467));
#137986=CARTESIAN_POINT('Origin',(0.0687986018264219,1.48214576764147,0.179702193597693));
#137987=CARTESIAN_POINT('',(-3.12375105413881,1.58673401540865,-6.81851738676565));
#137988=CARTESIAN_POINT('Origin',(0.0399656944841692,1.33942795304523,0.180618175323255));
#137989=CARTESIAN_POINT('Origin',(0.093497447181683,1.48219938683692,0.163881262855647));
#137990=CARTESIAN_POINT('Ctrl Pts',(-2.511877418,1.716084912,-6.800953745));
#137991=CARTESIAN_POINT('Ctrl Pts',(-2.881507287,1.651909459,-6.664433933));
#137992=CARTESIAN_POINT('Ctrl Pts',(-3.234163976,1.586734015,-6.488658057));
#137993=CARTESIAN_POINT('Ctrl Pts',(-3.24617590589201,1.58451405749336,
-6.48267090982519));
#137994=CARTESIAN_POINT('Ctrl Pts',(-3.25818783578402,1.58229409998675,
-6.47668376265049));
#137995=CARTESIAN_POINT('Ctrl Pts',(-2.36606963523562,1.716084912,-7.11754481583485));
#137996=CARTESIAN_POINT('Ctrl Pts',(-2.75290613680355,1.651909459,-6.98894961499887));
#137997=CARTESIAN_POINT('Ctrl Pts',(-3.12352696960189,1.586734015,-6.81918682764803));
#137998=CARTESIAN_POINT('Ctrl Pts',(-3.13615078080114,1.58451405749337,
-6.81340449382726));
#137999=CARTESIAN_POINT('Ctrl Pts',(-3.14877459200044,1.58229409998674,
-6.80762216000638));
#138000=CARTESIAN_POINT('',(-3.17895751939195,1.58673401622024,-6.65358771970716));
#138001=CARTESIAN_POINT('Ctrl Pts',(-3.234163976,1.586734015,-6.488658057));
#138002=CARTESIAN_POINT('Ctrl Pts',(-3.290477367,1.596957843,-6.460589581));
#138003=CARTESIAN_POINT('Ctrl Pts',(-3.346295113,1.607142857,-6.431547949));
#138004=CARTESIAN_POINT('Ctrl Pts',(-3.642393617,1.661171687,-6.277489706));
#138005=CARTESIAN_POINT('Ctrl Pts',(-3.923084388,1.716105035,-6.09687697800001));
#138006=CARTESIAN_POINT('Ctrl Pts',(-3.564023309,1.586734015,-6.599070984));
#138007=CARTESIAN_POINT('Ctrl Pts',(-3.621294945,1.596957843,-6.568139745));
#138008=CARTESIAN_POINT('Ctrl Pts',(-3.678021106,1.607142857,-6.536219148));
#138009=CARTESIAN_POINT('Ctrl Pts',(-3.978938509,1.661171687,-6.366888754));
#138010=CARTESIAN_POINT('Ctrl Pts',(-4.263024558,1.716105035,-6.170625707));
#138011=CARTESIAN_POINT('',(-3.56402331316047,1.58673401455072,-6.59907098094287));
#138012=CARTESIAN_POINT('',(-4.05472873457929,1.67637477916353,-6.3094512345042));
#138013=CARTESIAN_POINT('Ctrl Pts',(-3.56402331229197,1.58673401558767,
-6.59907098222207));
#138014=CARTESIAN_POINT('Ctrl Pts',(-3.60223885805523,1.5935560516628,-6.57843154770463));
#138015=CARTESIAN_POINT('Ctrl Pts',(-3.64024060934755,1.60035948085481,
-6.55747875709107));
#138016=CARTESIAN_POINT('Ctrl Pts',(-3.67802110594051,1.60714285701092,
-6.53621914792779));
#138017=CARTESIAN_POINT('Ctrl Pts',(-3.80538617878491,1.63001087933882,
-6.46454905554143));
#138018=CARTESIAN_POINT('Ctrl Pts',(-3.93107498717681,1.65310706301777,
-6.38891652970493));
#138019=CARTESIAN_POINT('Ctrl Pts',(-4.0547287309188,1.67637477803959,-6.30945123659626));
#138020=CARTESIAN_POINT('Ctrl Pts',(-3.9190894175443,1.71532338703037,-6.09944572512069));
#138021=CARTESIAN_POINT('Ctrl Pts',(-3.94175986227678,1.70851142704216,
-6.13433434944167));
#138022=CARTESIAN_POINT('Ctrl Pts',(-3.96440810447552,1.70186463314016,
-6.16930110495159));
#138023=CARTESIAN_POINT('Ctrl Pts',(-4.00961044632058,1.68889233604367,
-6.23929283370253));
#138024=CARTESIAN_POINT('Ctrl Pts',(-4.03219137397222,1.68255913650916,
-6.27435936226819));
#138025=CARTESIAN_POINT('Ctrl Pts',(-4.05472873831957,1.67637477936948,
-6.30945123213834));
#138026=CARTESIAN_POINT('',(-3.39909364966914,1.58673401368624,-6.54386451677612));
#138027=CARTESIAN_POINT('Origin',(-1.49619899803E-14,1.67745375800056,1.30104260698261E-14));
#138028=CARTESIAN_POINT('',(-4.04868167575622,1.49654505838002,-6.31333324677893));
#138029=CARTESIAN_POINT('Origin',(0.105820797630874,1.48214573279163,0.160711178895498));
#138030=CARTESIAN_POINT('',(-4.51649917455081,1.58673401540864,-5.98759010069407));
#138031=CARTESIAN_POINT('Origin',(0.077858890967587,1.33942797597349,0.167803995583545));
#138032=CARTESIAN_POINT('Origin',(0.126541175047707,1.48219933721307,0.139950647587942));
#138033=CARTESIAN_POINT('Ctrl Pts',(-3.91515514,1.716084912,-6.101971831));
#138034=CARTESIAN_POINT('Ctrl Pts',(-4.246795545,1.651909459,-5.889184282));
#138035=CARTESIAN_POINT('Ctrl Pts',(-4.553420698,1.586734015,-5.641707183));
#138036=CARTESIAN_POINT('Ctrl Pts',(-4.56386473620058,1.58451405743873,
-5.63327780187965));
#138037=CARTESIAN_POINT('Ctrl Pts',(-4.57430877440114,1.58229409987748,
-5.62484842075922));
#138038=CARTESIAN_POINT('Ctrl Pts',(-3.84081398363992,1.716084912,-6.44250554223807));
#138039=CARTESIAN_POINT('Ctrl Pts',(-4.19096229675586,1.651909459,-6.2337584125284));
#138040=CARTESIAN_POINT('Ctrl Pts',(-4.51642423897335,1.586734015,-5.98829206201134));
#138041=CARTESIAN_POINT('Ctrl Pts',(-4.52750988189632,1.58451405743873,
-5.9799311695122));
#138042=CARTESIAN_POINT('Ctrl Pts',(-4.53859552481923,1.58229409987747,
-5.97157027701318));
#138043=CARTESIAN_POINT('',(-4.53495994002295,1.58673401622024,-5.81464863880259));
#138044=CARTESIAN_POINT('Ctrl Pts',(-4.553420698,1.586734015,-5.641707183));
#138045=CARTESIAN_POINT('Ctrl Pts',(-4.602383621,1.596957843,-5.602189219));
#138046=CARTESIAN_POINT('Ctrl Pts',(-4.650653287,1.607142857,-5.561827398));
#138047=CARTESIAN_POINT('Ctrl Pts',(-4.906711204,1.661171687,-5.347718525));
#138048=CARTESIAN_POINT('Ctrl Pts',(-5.142013183,1.716105035,-5.110988204));
#138049=CARTESIAN_POINT('Ctrl Pts',(-4.899303619,1.586734015,-5.678628712));
#138050=CARTESIAN_POINT('Ctrl Pts',(-4.948586973,1.596957843,-5.636108919));
#138051=CARTESIAN_POINT('Ctrl Pts',(-4.997124924,1.607142857,-5.59274016));
#138052=CARTESIAN_POINT('Ctrl Pts',(-5.254606016,1.661171687,-5.36268027));
#138053=CARTESIAN_POINT('Ctrl Pts',(-5.489859537,1.716105035,-5.109935642));
#138054=CARTESIAN_POINT('',(-4.89930362251769,1.58673401411985,-5.67862870804427));
#138055=CARTESIAN_POINT('',(-5.31627693897885,1.67637478034043,-5.29029295069965));
#138056=CARTESIAN_POINT('Ctrl Pts',(-4.89930362211821,1.58673401434301,
-5.67862870931878));
#138057=CARTESIAN_POINT('Ctrl Pts',(-4.93218884071548,1.59355605125262,
-5.65025660069274));
#138058=CARTESIAN_POINT('Ctrl Pts',(-4.96479790140868,1.60035948085479,
-5.62162442138197));
#138059=CARTESIAN_POINT('Ctrl Pts',(-4.99712492354918,1.60714285723698,
-5.59274016010432));
#138060=CARTESIAN_POINT('Ctrl Pts',(-5.10610532116016,1.6300108792918,-5.49536594898596));
#138061=CARTESIAN_POINT('Ctrl Pts',(-5.21259683738857,1.65310706412193,
-5.39448229136159));
#138062=CARTESIAN_POINT('Ctrl Pts',(-5.31627693626695,1.67637478135681,
-5.29029295378962));
#138063=CARTESIAN_POINT('Ctrl Pts',(-5.13866381750373,1.71532338696521,
-5.11435569607225));
#138064=CARTESIAN_POINT('Ctrl Pts',(-5.16830424634674,1.70851143073915,
-5.14355515230682));
#138065=CARTESIAN_POINT('Ctrl Pts',(-5.19793978547661,1.70186464073664,
-5.17283568354511));
#138066=CARTESIAN_POINT('Ctrl Pts',(-5.2571315092576,1.6888923360179,-5.23147391192988));
#138067=CARTESIAN_POINT('Ctrl Pts',(-5.28672277448894,1.68255913648335,
-5.26086637267337));
#138068=CARTESIAN_POINT('Ctrl Pts',(-5.3162769424568,1.67637477935555,-5.29029294699963));
#138069=CARTESIAN_POINT('',(-4.726362164702,1.58673401368602,-5.6601679423212));
#138070=CARTESIAN_POINT('Origin',(5.96311194867027E-13,1.67745375799967,
5.55111512312578E-13));
#138071=CARTESIAN_POINT('',(-5.31120577464674,1.49654505840871,-5.29538414253195));
#138072=CARTESIAN_POINT('Origin',(0.137894918178038,1.48214572826549,0.134205497018995));
#138073=CARTESIAN_POINT('',(-5.69806081408171,1.58673401497662,-4.87668975361135));
#138074=CARTESIAN_POINT('Origin',(0.112111456014379,1.33942796695583,0.147143430278365));
#138075=CARTESIAN_POINT('Origin',(0.153667784907622,1.48219935481058,0.109475894747609));
#138076=CARTESIAN_POINT('Ctrl Pts',(-5.135364559,1.716084912,-5.11766849700001));
#138077=CARTESIAN_POINT('Ctrl Pts',(-5.413508362,1.651909459,-4.838562918));
#138078=CARTESIAN_POINT('Ctrl Pts',(-5.65976453,1.586734015,-4.530956353));
#138079=CARTESIAN_POINT('Ctrl Pts',(-5.66815232495067,1.58451405736592,
-4.52047888632921));
#138080=CARTESIAN_POINT('Ctrl Pts',(-5.67654011990131,1.58229409973185,
-4.51000141965846));
#138081=CARTESIAN_POINT('Ctrl Pts',(-5.13596613941497,1.716084912,-5.46622186993683));
#138082=CARTESIAN_POINT('Ctrl Pts',(-5.4330537173179,1.651909459,-5.18708359571734));
#138083=CARTESIAN_POINT('Ctrl Pts',(-5.69813853004114,1.586734015,-4.8773914146006));
#138084=CARTESIAN_POINT('Ctrl Pts',(-5.70716765232347,1.58451405736592,
-4.86684290922051));
#138085=CARTESIAN_POINT('Ctrl Pts',(-5.71619677460589,1.58229409973185,
-4.85629440384044));
#138086=CARTESIAN_POINT('',(-5.67891267437233,1.58673401622024,-4.70382305061765));
#138087=CARTESIAN_POINT('Ctrl Pts',(-5.65976453,1.586734015,-4.530956353));
#138088=CARTESIAN_POINT('Ctrl Pts',(-5.699087532,1.596957843,-4.481836715));
#138089=CARTESIAN_POINT('Ctrl Pts',(-5.737552082,1.607142857,-4.43204198));
#138090=CARTESIAN_POINT('Ctrl Pts',(-5.941596428,1.661171687,-4.167893971));
#138091=CARTESIAN_POINT('Ctrl Pts',(-6.120507157,1.716105035,-3.886115303));
#138092=CARTESIAN_POINT('Ctrl Pts',(-6.005497937,1.586734015,-4.492660073));
#138093=CARTESIAN_POINT('Ctrl Pts',(-6.044488575,1.596957843,-4.440539904));
#138094=CARTESIAN_POINT('Ctrl Pts',(-6.082568734,1.607142857,-4.387750858));
#138095=CARTESIAN_POINT('Ctrl Pts',(-6.284573986,1.661171687,-4.107718817));
#138096=CARTESIAN_POINT('Ctrl Pts',(-6.459994786,1.716105035,-3.810310665));
#138097=CARTESIAN_POINT('',(-6.00549793922469,1.5867340145539,-4.49266006883129));
#138098=CARTESIAN_POINT('',(-6.32924194324064,1.67637477916489,-4.023766446818));
#138099=CARTESIAN_POINT('Ctrl Pts',(-6.00549793924492,1.58673401558864,
-4.49266006999914));
#138100=CARTESIAN_POINT('Ctrl Pts',(-6.03151515499356,1.59355605166312,
-4.45788193471596));
#138101=CARTESIAN_POINT('Ctrl Pts',(-6.0572067617763,1.6003594808548,-4.4229091754408));
#138102=CARTESIAN_POINT('Ctrl Pts',(-6.08256873376882,1.60714285700729,
-4.38775085799541));
#138103=CARTESIAN_POINT('Ctrl Pts',(-6.16806865231114,1.63001087932493,
-4.26922563809061));
#138104=CARTESIAN_POINT('Ctrl Pts',(-6.25038345283621,1.65310706301181,
-4.14780805601408));
#138105=CARTESIAN_POINT('Ctrl Pts',(-6.329241940739,1.67637477801304,-4.0237664503399));
#138106=CARTESIAN_POINT('Ctrl Pts',(-6.11796000837387,1.7153233870224,-3.89012407945758));
#138107=CARTESIAN_POINT('Ctrl Pts',(-6.15318448065138,1.7085114307687,-3.91226905256771));
#138108=CARTESIAN_POINT('Ctrl Pts',(-6.18842160622695,1.70186464073718,
-3.93449425635916));
#138109=CARTESIAN_POINT('Ctrl Pts',(-6.25883494579709,1.68889233608524,
-3.97903708417286));
#138110=CARTESIAN_POINT('Ctrl Pts',(-6.29405289406707,1.68255913651809,
-4.00138111820375));
#138111=CARTESIAN_POINT('Ctrl Pts',(-6.32924194570051,1.67637477937598,
-4.02376644300949));
#138112=CARTESIAN_POINT('',(-5.83263123845116,1.58673401368404,-4.51180820659941));
#138113=CARTESIAN_POINT('Origin',(8.00574884163296E-13,1.6774537580005,
5.19549681055054E-13));
#138114=CARTESIAN_POINT('',(-6.32538379609198,1.49654505840891,-4.02982876001943));
#138115=CARTESIAN_POINT('Origin',(0.163521297462732,1.48214578095595,0.101424576443183));
#138116=CARTESIAN_POINT('',(-6.61318746238814,1.58673401497662,-3.53776081556057));
#138117=CARTESIAN_POINT('Origin',(0.141121857032126,1.33942798108242,0.119602660461818));
#138118=CARTESIAN_POINT('Origin',(0.173609169352683,1.48219938729381,0.0738823743943423));
#138119=CARTESIAN_POINT('Ctrl Pts',(-6.115450039,1.716084912,-3.894068671));
#138120=CARTESIAN_POINT('Ctrl Pts',(-6.327091546,1.651909459,-3.56169573));
#138121=CARTESIAN_POINT('Ctrl Pts',(-6.501464062,1.586734015,-3.208343039));
#138122=CARTESIAN_POINT('Ctrl Pts',(-6.50740340903144,1.58451405747043,
-3.1963074022811));
#138123=CARTESIAN_POINT('Ctrl Pts',(-6.51334275606286,1.58229409994087,
-3.18427176556214));
#138124=CARTESIAN_POINT('Ctrl Pts',(-6.19096622721656,1.716084912,-4.23434373838217));
#138125=CARTESIAN_POINT('Ctrl Pts',(-6.42110158486059,1.651909459,-3.8978665147459));
#138126=CARTESIAN_POINT('Ctrl Pts',(-6.61341419795615,1.586734015,-3.53842936554782));
#138127=CARTESIAN_POINT('Ctrl Pts',(-6.61996460724023,1.58451405747043,
-3.52618648453627));
#138128=CARTESIAN_POINT('Ctrl Pts',(-6.62651501652436,1.58229409994087,
-3.51394360352467));
#138129=CARTESIAN_POINT('',(-6.55732576399389,1.58673401622024,-3.37305192420777));
#138130=CARTESIAN_POINT('Ctrl Pts',(-6.501464062,1.586734015,-3.208343039));
#138131=CARTESIAN_POINT('Ctrl Pts',(-6.529308444,1.596957843,-3.151918508));
#138132=CARTESIAN_POINT('Ctrl Pts',(-6.556169318,1.607142857,-3.095019205));
#138133=CARTESIAN_POINT('Ctrl Pts',(-6.698659207,1.661171687,-2.793183326));
#138134=CARTESIAN_POINT('Ctrl Pts',(-6.812813018,1.716105035,-2.479531969));
#138135=CARTESIAN_POINT('Ctrl Pts',(-6.830881846,1.586734015,-3.096619642));
#138136=CARTESIAN_POINT('Ctrl Pts',(-6.85775661,1.596957843,-3.037336179));
#138137=CARTESIAN_POINT('Ctrl Pts',(-6.883598391,1.607142857,-2.977595203));
#138138=CARTESIAN_POINT('Ctrl Pts',(-7.020682261,1.661171687,-2.660684997));
#138139=CARTESIAN_POINT('Ctrl Pts',(-7.128067859,1.716105035,-2.332519796));
#138140=CARTESIAN_POINT('',(-6.83088184728289,1.58673401455455,-3.09661963745425));
#138141=CARTESIAN_POINT('',(-7.04625862555874,1.67637477889898,-2.56909310230143));
#138142=CARTESIAN_POINT('Ctrl Pts',(-6.83088184754511,1.5867340155878,-3.09661963859161));
#138143=CARTESIAN_POINT('Ctrl Pts',(-6.84881452494674,1.59355605166285,
-3.05706166447727));
#138144=CARTESIAN_POINT('Ctrl Pts',(-6.86638736696152,1.60035948085478,
-3.01738361286274));
#138145=CARTESIAN_POINT('Ctrl Pts',(-6.88359839099221,1.60714285699693,
-2.97759520301802));
#138146=CARTESIAN_POINT('Ctrl Pts',(-6.94161994920343,1.63001087863148,
-2.84346108523285));
#138147=CARTESIAN_POINT('Ctrl Pts',(-6.99590908163633,1.65310706174197,
-2.70718693367039));
#138148=CARTESIAN_POINT('Ctrl Pts',(-7.04625862155055,1.67637477616413,
-2.56909311176525));
#138149=CARTESIAN_POINT('Ctrl Pts',(-6.81118718894288,1.71532338700859,
-2.48399458411567));
#138150=CARTESIAN_POINT('Ctrl Pts',(-6.85034866843755,1.70851142705774,
-2.49804960736224));
#138151=CARTESIAN_POINT('Ctrl Pts',(-6.88953975570717,1.70186463317932,
-2.51218026669214));
#138152=CARTESIAN_POINT('Ctrl Pts',(-6.96788221635299,1.6888923360513,-2.54054490485863));
#138153=CARTESIAN_POINT('Ctrl Pts',(-7.00708009495013,1.68255913655582,
-2.55479572977348));
#138154=CARTESIAN_POINT('Ctrl Pts',(-7.0462586293168,1.67637477940267,-2.56909309222123));
#138155=CARTESIAN_POINT('',(-6.6661729574545,1.58673401368593,-3.15248133319519));
#138156=CARTESIAN_POINT('Ctrl Pts',(-6.809583872,1.716084912,-2.488386523));
#138157=CARTESIAN_POINT('Ctrl Pts',(-6.94482696000001,1.651909459,-2.118287608));
#138158=CARTESIAN_POINT('Ctrl Pts',(-7.03916236,1.586734015,-1.73571117));
#138159=CARTESIAN_POINT('Ctrl Pts',(-7.04237554241109,1.58451405737756,
-1.72268013518725));
#138160=CARTESIAN_POINT('Ctrl Pts',(-7.04558872482218,1.58229409975514,
-1.70964910037451));
#138161=CARTESIAN_POINT('Ctrl Pts',(-6.95648361439213,1.716084912,-2.80447239967962));
#138162=CARTESIAN_POINT('Ctrl Pts',(-7.10890587835298,1.651909459,-2.42638952731729));
#138163=CARTESIAN_POINT('Ctrl Pts',(-7.21945396683182,1.586734015,-2.03401429125501));
#138164=CARTESIAN_POINT('Ctrl Pts',(-7.22321937381032,1.58451405737757,
-2.020649497052));
#138165=CARTESIAN_POINT('Ctrl Pts',(-7.22698478078881,1.58229409975514,
-2.00728470284901));
#138166=CARTESIAN_POINT('',(-7.21908881409604,1.58673401498684,-2.03341011390865));
#138167=CARTESIAN_POINT('Origin',(0.185432819398685,1.48219938584591,0.0348342073597357));
#138168=CARTESIAN_POINT('',(-7.12912558795207,1.58673401622024,-1.88456063811549));
#138169=CARTESIAN_POINT('Origin',(9.4542429440736E-13,1.67745375799972,
2.49366499671666E-13));
#138170=CARTESIAN_POINT('',(-7.04379390009598,1.49654505840544,-2.57584306385715));
#138171=CARTESIAN_POINT('Origin',(0.181501620529565,1.48214573542086,0.0639010986816974));
#138172=CARTESIAN_POINT('Origin',(0.163533519886799,1.33942795423984,0.086469386724336));
#138173=CARTESIAN_POINT('Ctrl Pts',(-7.03916236,1.586734015,-1.73571117));
#138174=CARTESIAN_POINT('Ctrl Pts',(-7.05422615,1.596957843,-1.674620094));
#138175=CARTESIAN_POINT('Ctrl Pts',(-7.068227363,1.607142857,-1.613276771));
#138176=CARTESIAN_POINT('Ctrl Pts',(-7.142500127,1.661171687,-1.287866533));
#138177=CARTESIAN_POINT('Ctrl Pts',(-7.186559314,1.716105035,-0.957008476));
#138178=CARTESIAN_POINT('Ctrl Pts',(-7.336861312,1.586734015,-1.555784718));
#138179=CARTESIAN_POINT('Ctrl Pts',(-7.350363566,1.596957843,-1.49210999));
#138180=CARTESIAN_POINT('Ctrl Pts',(-7.362758637,1.607142857,-1.428210506));
#138181=CARTESIAN_POINT('Ctrl Pts',(-7.428511236,1.661171687,-1.089240504));
#138182=CARTESIAN_POINT('Ctrl Pts',(-7.462840401,1.716105035,-0.745662894));
#138183=CARTESIAN_POINT('',(-7.33686131228108,1.58673401455507,-1.55578471328603));
#138184=CARTESIAN_POINT('',(-7.188011837802,1.58673401368697,-1.64574793612957));
#138185=CARTESIAN_POINT('',(-7.43380009082176,1.67637477914435,-0.994291808505194));
#138186=CARTESIAN_POINT('Ctrl Pts',(-7.33686131277568,1.58673401558734,
-1.55578471434202));
#138187=CARTESIAN_POINT('Ctrl Pts',(-7.34587093849314,1.59355605166269,
-1.51329658840759));
#138188=CARTESIAN_POINT('Ctrl Pts',(-7.354503328865,1.60035948085488,-1.47076854621938));
#138189=CARTESIAN_POINT('Ctrl Pts',(-7.36275863686387,1.60714285704628,
-1.42821050583054));
#138190=CARTESIAN_POINT('Ctrl Pts',(-7.39058881335076,1.63001087948788,
-1.28473944435232));
#138191=CARTESIAN_POINT('Ctrl Pts',(-7.41431378314698,1.65310706300321,
-1.13998074464423));
#138192=CARTESIAN_POINT('Ctrl Pts',(-7.43380009004028,1.6763747780124,-0.994291812679242));
#138193=CARTESIAN_POINT('Ctrl Pts',(-7.18593082707723,1.71532338700727,
-0.961716262227243));
#138194=CARTESIAN_POINT('Ctrl Pts',(-7.22719814866542,1.70851142685462,
-0.967024126647668));
#138195=CARTESIAN_POINT('Ctrl Pts',(-7.26851064495947,1.70186463284726,
-0.97239949394857));
#138196=CARTESIAN_POINT('Ctrl Pts',(-7.35111905906606,1.68889233602461,
-0.983259669302536));
#138197=CARTESIAN_POINT('Ctrl Pts',(-7.39246401931295,1.68255913649073,
-0.988750932741153));
#138198=CARTESIAN_POINT('Ctrl Pts',(-7.43380009144446,1.67637477935179,
-0.994291804091257));
#138199=CARTESIAN_POINT('Origin',(3.40439482160448E-13,1.67745375799922,
5.13640779215008E-14));
#138200=CARTESIAN_POINT('',(-7.4874335964436,1.58673401541129,-0.43397941779166));
#138201=CARTESIAN_POINT('Origin',(0.188585854968112,1.48219938148668,-0.00584277830929555));
#138202=CARTESIAN_POINT('',(-7.4328440300674,1.49654505822092,-1.00141380955591));
#138203=CARTESIAN_POINT('Origin',(0.190994941521154,1.48214558438775,0.0233895971421555));
#138204=CARTESIAN_POINT('Origin',(0.178298506284001,1.33942798528867,0.049292893791802));
#138205=CARTESIAN_POINT('Ctrl Pts',(-7.185309132,1.716084912,-0.966350186));
#138206=CARTESIAN_POINT('Ctrl Pts',(-7.23782998500001,1.651909459,-0.575830712));
#138207=CARTESIAN_POINT('Ctrl Pts',(-7.24771725000001,1.586734015,-0.181919376));
#138208=CARTESIAN_POINT('Ctrl Pts',(-7.24805402267975,1.58451405741505,
-0.168502260527041));
#138209=CARTESIAN_POINT('Ctrl Pts',(-7.24839079535963,1.58229409983011,
-0.155085145054078));
#138210=CARTESIAN_POINT('Ctrl Pts',(-7.3967235596348,1.716084912,-1.24346704850373));
#138211=CARTESIAN_POINT('Ctrl Pts',(-7.46430563398088,1.651909459,-0.841457262522982));
#138212=CARTESIAN_POINT('Ctrl Pts',(-7.48792009244461,1.586734015,-0.434490970580043));
#138213=CARTESIAN_POINT('Ctrl Pts',(-7.48872443059658,1.58451405741505,
-0.420629186890223));
#138214=CARTESIAN_POINT('Ctrl Pts',(-7.48952876874859,1.58229409983011,
-0.4067674032004));
#138215=CARTESIAN_POINT('',(-7.36757542331898,1.58673401622022,-0.307949391868585));
#138216=CARTESIAN_POINT('Ctrl Pts',(-7.24771725,1.586734015,-0.181919376));
#138217=CARTESIAN_POINT('Ctrl Pts',(-7.24929608200001,1.596957843,-0.119018306));
#138218=CARTESIAN_POINT('Ctrl Pts',(-7.249782953,1.607142857,-0.056099309));
#138219=CARTESIAN_POINT('Ctrl Pts',(-7.25236567800001,1.661171687,0.277669467));
#138220=CARTESIAN_POINT('Ctrl Pts',(-7.224270084,1.716105035,0.610263670000001));
#138221=CARTESIAN_POINT('Ctrl Pts',(-7.49977729699999,1.586734015,0.05779697));
#138222=CARTESIAN_POINT('Ctrl Pts',(-7.49927569200001,1.596957843,0.122885604));
#138223=CARTESIAN_POINT('Ctrl Pts',(-7.497644473,1.607142857,0.187955727));
#138224=CARTESIAN_POINT('Ctrl Pts',(-7.488991283,1.661171687,0.533135664000001));
#138225=CARTESIAN_POINT('Ctrl Pts',(-7.44865882,1.716105035,0.876060377));
#138226=CARTESIAN_POINT('',(-7.49977729625411,1.58673401455095,0.057796975121696));
#138227=CARTESIAN_POINT('',(-7.47374532379189,1.67637477914009,0.62700145943416));
#138228=CARTESIAN_POINT('Ctrl Pts',(-7.49977729697118,1.58673401558734,
0.0577969737392455));
#138229=CARTESIAN_POINT('Ctrl Pts',(-7.49944259184632,1.59355605166269,
0.101228554286963));
#138230=CARTESIAN_POINT('Ctrl Pts',(-7.49873088997243,1.60035948085494,
0.144618023182082));
#138231=CARTESIAN_POINT('Ctrl Pts',(-7.49764447287025,1.60714285707618,
0.18795572737095));
#138232=CARTESIAN_POINT('Ctrl Pts',(-7.49398195850961,1.63001087961635,
0.334055181280936));
#138233=CARTESIAN_POINT('Ctrl Pts',(-7.48603341016074,1.65310706300346,
0.480529669341363));
#138234=CARTESIAN_POINT('Ctrl Pts',(-7.47374532392755,1.67637477802169,
0.627001455243438));
#138235=CARTESIAN_POINT('Ctrl Pts',(-7.2246683252045,1.71532338708746,0.605530843116696));
#138236=CARTESIAN_POINT('Ctrl Pts',(-7.26611187320349,1.70851142700761,
0.60921832783714));
#138237=CARTESIAN_POINT('Ctrl Pts',(-7.30761405160807,1.70186463296282,
0.612849599107477));
#138238=CARTESIAN_POINT('Ctrl Pts',(-7.39062574460637,1.6888923360062,0.620001695686318));
#138239=CARTESIAN_POINT('Ctrl Pts',(-7.43218454204251,1.68255913648216,
0.623526759146004));
#138240=CARTESIAN_POINT('Ctrl Pts',(-7.47374532345536,1.67637477934486,
0.627001463823824));
#138241=CARTESIAN_POINT('',(-7.37374727356795,1.58673401368695,-0.0620611949261003));
#138242=CARTESIAN_POINT('Origin',(-9.14632952708772E-13,1.67745375800011,
2.80537312130624E-15));
#138243=CARTESIAN_POINT('',(-7.47434263494036,1.49654505840813,0.619840442693668));
#138244=CARTESIAN_POINT('Origin',(0.191557338754434,1.48214579038053,-0.0182154483195574));
#138245=CARTESIAN_POINT('',(-7.40567430550057,1.58673401497661,1.18574367902254));
#138246=CARTESIAN_POINT('Origin',(0.18472656006578,1.33942794290295,0.00981153906990759));
#138247=CARTESIAN_POINT('Origin',(0.182920782974308,1.48219935504351,-0.0462465674927783));
#138248=CARTESIAN_POINT('Ctrl Pts',(-7.225057322,1.716084912,0.600871612));
#138249=CARTESIAN_POINT('Ctrl Pts',(-7.192400124,1.651909459,0.993551388));
#138250=CARTESIAN_POINT('Ctrl Pts',(-7.117376937,1.586734015,1.380378766));
#138251=CARTESIAN_POINT('Ctrl Pts',(-7.1148215528193,1.5845140573412,1.39355459339328));
#138252=CARTESIAN_POINT('Ctrl Pts',(-7.1122661686386,1.58229409968241,1.40673042078652));
#138253=CARTESIAN_POINT('Ctrl Pts',(-7.49110093223557,1.716084912,0.375681439552532));
#138254=CARTESIAN_POINT('Ctrl Pts',(-7.47068275461875,1.651909459,0.782820608983368));
#138255=CARTESIAN_POINT('Ctrl Pts',(-7.4062593970554,1.586734015,1.18534866545931));
#138256=CARTESIAN_POINT('Ctrl Pts',(-7.40406505640728,1.5845140573412,1.19905927772388));
#138257=CARTESIAN_POINT('Ctrl Pts',(-7.40187071575919,1.58229409968241,
1.21276988998847));
#138258=CARTESIAN_POINT('',(-7.261525620671,1.58673401622021,1.28306122602152));
#138259=CARTESIAN_POINT('Ctrl Pts',(-7.117376937,1.586734015,1.380378766));
#138260=CARTESIAN_POINT('Ctrl Pts',(-7.105396986,1.596957843,1.442148645));
#138261=CARTESIAN_POINT('Ctrl Pts',(-7.09234675,1.607142857,1.503701295));
#138262=CARTESIAN_POINT('Ctrl Pts',(-7.023118672,1.661171687,1.830221952));
#138263=CARTESIAN_POINT('Ctrl Pts',(-6.924182015,1.716105035,2.149000565));
#138264=CARTESIAN_POINT('Ctrl Pts',(-7.312012032,1.586734015,1.668676136));
#138265=CARTESIAN_POINT('Ctrl Pts',(-7.297530022,1.596957843,1.732135204));
#138266=CARTESIAN_POINT('Ctrl Pts',(-7.281948786,1.607142857,1.79533336));
#138267=CARTESIAN_POINT('Ctrl Pts',(-7.19929442,1.661171687,2.130583001));
#138268=CARTESIAN_POINT('Ctrl Pts',(-7.086186231,1.716105035,2.456820037));
#138269=CARTESIAN_POINT('',(-7.31201203007812,1.58673401412069,1.66867614091693));
#138270=CARTESIAN_POINT('',(-7.16422653185322,1.67637478035133,2.21897683545438));
#138271=CARTESIAN_POINT('Ctrl Pts',(-7.31201203089279,1.58673401434349,
1.66867613996222));
#138272=CARTESIAN_POINT('Ctrl Pts',(-7.30234864499606,1.59355605125278,
1.71102036257308));
#138273=CARTESIAN_POINT('Ctrl Pts',(-7.29232612896216,1.60035948085479,
1.75324241500101));
#138274=CARTESIAN_POINT('Ctrl Pts',(-7.28194878628072,1.60714285723673,
1.79533336012697));
#138275=CARTESIAN_POINT('Ctrl Pts',(-7.24696483610422,1.6300108792978,1.93722975618628));
#138276=CARTESIAN_POINT('Ctrl Pts',(-7.20771443454255,1.65310706412798,
2.07857105028278));
#138277=CARTESIAN_POINT('Ctrl Pts',(-7.16422653331938,1.67637478135684,
2.21897683162364));
#138278=CARTESIAN_POINT('Ctrl Pts',(-6.92558836329049,1.71532338701588,
2.14446399814966));
#138279=CARTESIAN_POINT('Ctrl Pts',(-6.96527028317949,1.70851142707599,
2.15697440921553));
#138280=CARTESIAN_POINT('Ctrl Pts',(-7.00502154671859,1.70186463319256,
2.1694425247741));
#138281=CARTESIAN_POINT('Ctrl Pts',(-7.08455498415042,1.68889233605714,
2.1942724700893));
#138282=CARTESIAN_POINT('Ctrl Pts',(-7.12438437564887,1.68255913650904,
2.20664903265677));
#138283=CARTESIAN_POINT('Ctrl Pts',(-7.16422653021818,1.67637477937239,
2.21897684024757));
#138284=CARTESIAN_POINT('',(-7.21469448283075,1.58673401368698,1.52452745889956));
#138285=CARTESIAN_POINT('Origin',(4.69676381120721E-13,1.67745375799961,
-1.7499023063916E-13));
#138286=CARTESIAN_POINT('',(-7.16634928489004,1.49654505824553,2.21211164336113));
#138287=CARTESIAN_POINT('Origin',(0.183163363348232,1.48214558960764,-0.058968873837181));
#138288=CARTESIAN_POINT('',(-6.97763391702804,1.58673401540863,2.75002271427369));
#138289=CARTESIAN_POINT('Origin',(0.182516852866949,1.3394279789947,-0.0301285564507109));
#138290=CARTESIAN_POINT('Origin',(0.168702839582741,1.4821993589666,-0.0844879943072543));
#138291=CARTESIAN_POINT('Ctrl Pts',(-6.926969862,1.716084912,2.13999732));
#138292=CARTESIAN_POINT('Ctrl Pts',(-6.810661627,1.651909459,2.516476129));
#138293=CARTESIAN_POINT('Ctrl Pts',(-6.654235988,1.586734015,2.878131931));
#138294=CARTESIAN_POINT('Ctrl Pts',(-6.64890793416401,1.58451405747489,
2.89045038208945));
#138295=CARTESIAN_POINT('Ctrl Pts',(-6.6435798803279,1.5822940999498,2.90276883317886));
#138296=CARTESIAN_POINT('Ctrl Pts',(-7.23520275053982,1.716084912,1.977263481934));
#138297=CARTESIAN_POINT('Ctrl Pts',(-7.12773905188058,1.651909459,2.37049465845346));
#138298=CARTESIAN_POINT('Ctrl Pts',(-6.97829024445302,1.586734015,2.74976271555198));
#138299=CARTESIAN_POINT('Ctrl Pts',(-6.9731998302678,1.58451405747489,2.76268106218245));
#138300=CARTESIAN_POINT('Ctrl Pts',(-6.96810941608252,1.5822940999498,2.77559940881284));
#138301=CARTESIAN_POINT('',(-6.81593495058514,1.58673401622023,2.81407732706006));
#138302=CARTESIAN_POINT('Ctrl Pts',(-6.654235988,1.586734015,2.878131931));
#138303=CARTESIAN_POINT('Ctrl Pts',(-6.629257423,1.596957843,2.935882329));
#138304=CARTESIAN_POINT('Ctrl Pts',(-6.603280295,1.607142857,2.993190497));
#138305=CARTESIAN_POINT('Ctrl Pts',(-6.465478441,1.661171687,3.297195292));
#138306=CARTESIAN_POINT('Ctrl Pts',(-6.30032689000001,1.716105035,3.587252582));
#138307=CARTESIAN_POINT('Ctrl Pts',(-6.78234521,1.586734015,3.201529861));
#138308=CARTESIAN_POINT('Ctrl Pts',(-6.754559958,1.596957843,3.260392086));
#138309=CARTESIAN_POINT('Ctrl Pts',(-6.725757268,1.607142857,3.3187632));
#138310=CARTESIAN_POINT('Ctrl Pts',(-6.572966551,1.661171687,3.628406645));
#138311=CARTESIAN_POINT('Ctrl Pts',(-6.39237145,1.716105035,3.922701524));
#138312=CARTESIAN_POINT('',(-6.78234520716232,1.58673401412049,3.20152986547042));
#138313=CARTESIAN_POINT('',(-6.51971646961656,1.67637478034357,3.70719532168303));
#138314=CARTESIAN_POINT('Ctrl Pts',(-6.78234520833718,1.58673401434349,
3.20152986475931));
#138315=CARTESIAN_POINT('Ctrl Pts',(-6.76380499121345,1.59355605125278,
3.24080675989459));
#138316=CARTESIAN_POINT('Ctrl Pts',(-6.74494030295206,1.60035948085479,
3.27988713929682));
#138317=CARTESIAN_POINT('Ctrl Pts',(-6.72575726772998,1.60714285723673,
3.31876319968409));
#138318=CARTESIAN_POINT('Ctrl Pts',(-6.66108769201959,1.63001087928986,
3.44982162195314));
#138319=CARTESIAN_POINT('Ctrl Pts',(-6.59237074276419,1.65310706411997,
3.57942075914026));
#138320=CARTESIAN_POINT('Ctrl Pts',(-6.51971647182816,1.67637478135681,
3.707195318158));
#138321=CARTESIAN_POINT('Ctrl Pts',(-6.30267558623198,1.7153233870683,3.58312440106051));
#138322=CARTESIAN_POINT('Ctrl Pts',(-6.33874037621333,1.70851143090008,
3.60387275388008));
#138323=CARTESIAN_POINT('Ctrl Pts',(-6.37488197802835,1.70186464092893,
3.62459470539109));
#138324=CARTESIAN_POINT('Ctrl Pts',(-6.44721830671353,1.6888923360433,3.66594150307704));
#138325=CARTESIAN_POINT('Ctrl Pts',(-6.48345591407357,1.68255913648982,
3.68659085031422));
#138326=CARTESIAN_POINT('Ctrl Pts',(-6.51971646694944,1.67637477935982,
3.70719532608147));
#138327=CARTESIAN_POINT('',(-6.71829059567161,1.58673401368698,3.03983090335604));
#138328=CARTESIAN_POINT('Origin',(-2.04697370165263E-13,1.67745375799961,
1.346579098227E-13));
#138329=CARTESIAN_POINT('',(-6.52326540700298,1.49654505841246,3.70094696342879));
#138330=CARTESIAN_POINT('Origin',(0.166204606236854,1.48214575970179,-0.0969649219425217));
#138331=CARTESIAN_POINT('',(-6.22332711995983,1.58673401540865,4.1857137457124));
#138332=CARTESIAN_POINT('Origin',(0.17177301985814,1.33942795617175,-0.068659935349929));
#138333=CARTESIAN_POINT('Origin',(0.146596010498544,1.48219934874745,-0.118778704936435));
#138334=CARTESIAN_POINT('Ctrl Pts',(-6.30498499000001,1.716084912,3.579059133));
#138335=CARTESIAN_POINT('Ctrl Pts',(-6.110464161,1.651909459,3.921733244));
#138336=CARTESIAN_POINT('Ctrl Pts',(-5.87995036100001,1.586734015,4.241306845));
#138337=CARTESIAN_POINT('Ctrl Pts',(-5.87209877115736,1.5845140574352,4.25219192363558));
#138338=CARTESIAN_POINT('Ctrl Pts',(-5.86424718131484,1.58229409987042,
4.26307700227107));
#138339=CARTESIAN_POINT('Ctrl Pts',(-6.64099453017892,1.716084912,3.48639088073289));
#138340=CARTESIAN_POINT('Ctrl Pts',(-6.45151019387323,1.651909459,3.84732701283999));
#138341=CARTESIAN_POINT('Ctrl Pts',(-6.22402399484519,1.586734015,4.18560091662383));
#138342=CARTESIAN_POINT('Ctrl Pts',(-6.21627552889814,1.5845140574352,4.19712295108326));
#138343=CARTESIAN_POINT('Ctrl Pts',(-6.20852706295096,1.58229409987042,
4.20864498554271));
#138344=CARTESIAN_POINT('',(-6.05163873763563,1.58673401622021,4.21351029926832));
#138345=CARTESIAN_POINT('Ctrl Pts',(-5.879950361,1.586734015,4.241306845));
#138346=CARTESIAN_POINT('Ctrl Pts',(-5.843141152,1.596957843,4.292337419));
#138347=CARTESIAN_POINT('Ctrl Pts',(-5.805451792,1.607142857,4.342721438));
#138348=CARTESIAN_POINT('Ctrl Pts',(-5.605519625,1.661171687,4.609995445));
#138349=CARTESIAN_POINT('Ctrl Pts',(-5.381875481,1.716105035,4.857768655));
#138350=CARTESIAN_POINT('Ctrl Pts',(-5.935543465,1.586734015,4.584683607));
#138351=CARTESIAN_POINT('Ctrl Pts',(-5.895754178,1.596957843,4.636196659));
#138352=CARTESIAN_POINT('Ctrl Pts',(-5.855076814,1.607142857,4.687011361));
#138353=CARTESIAN_POINT('Ctrl Pts',(-5.639294072,1.661171687,4.956570027));
#138354=CARTESIAN_POINT('Ctrl Pts',(-5.399656485,1.716105035,5.205161847));
#138355=CARTESIAN_POINT('',(-5.93554346122076,1.58673401412049,4.58468361069456));
#138356=CARTESIAN_POINT('',(-5.57035171146692,1.67637478034078,5.02206947459704));
#138357=CARTESIAN_POINT('Ctrl Pts',(-5.93554346242469,1.58673401434348,
4.58468361020337));
#138358=CARTESIAN_POINT('Ctrl Pts',(-5.908993333447,1.59355605125278,4.61905663523161));
#138359=CARTESIAN_POINT('Ctrl Pts',(-5.88216856458618,1.60035948085479,
4.65316798694213));
#138360=CARTESIAN_POINT('Ctrl Pts',(-5.85507681426963,1.60714285723673,
4.68701136109163));
#138361=CARTESIAN_POINT('Ctrl Pts',(-5.76374549062467,1.63001087929165,
4.80110366304963));
#138362=CARTESIAN_POINT('Ctrl Pts',(-5.6687751219266,1.65310706412178,4.9129007315449));
#138363=CARTESIAN_POINT('Ctrl Pts',(-5.57035171433747,1.67637478135681,
5.02206947169965));
#138364=CARTESIAN_POINT('Ctrl Pts',(-5.38505670288533,1.7153233870728,4.85424188880678));
#138365=CARTESIAN_POINT('Ctrl Pts',(-5.41581803545826,1.70851143101226,
4.88225801990094));
#138366=CARTESIAN_POINT('Ctrl Pts',(-5.44666005950121,1.70186464111915,
4.91026487937284));
#138367=CARTESIAN_POINT('Ctrl Pts',(-5.50841686694514,1.68889233603578,
4.96619518521198));
#138368=CARTESIAN_POINT('Ctrl Pts',(-5.53936825983376,1.68255913650977,
4.99415177652447));
#138369=CARTESIAN_POINT('Ctrl Pts',(-5.57035170798474,1.67637477936395,
5.02206947824522));
#138370=CARTESIAN_POINT('',(-5.90774690816807,1.58673401368697,4.41299523246859));
#138371=CARTESIAN_POINT('Origin',(-2.94902990916057E-13,1.67745375800039,
3.69062419514066E-13));
#138372=CARTESIAN_POINT('',(-5.57516088947637,1.4965450584209,5.01673011568442));
#138373=CARTESIAN_POINT('Origin',(0.141473953944199,1.48214574136492,-0.130426776897208));
#138374=CARTESIAN_POINT('',(-5.17802446096194,1.58673401497661,5.4256854564893));
#138375=CARTESIAN_POINT('Origin',(0.152997134318694,1.33942795405182,-0.103980765192834));
#138376=CARTESIAN_POINT('Origin',(0.11763457126844,1.48219938277928,-0.147515345083278));
#138377=CARTESIAN_POINT('Ctrl Pts',(-5.388186027,1.716084912,4.850768118));
#138378=CARTESIAN_POINT('Ctrl Pts',(-5.124548183,1.651909459,5.14361447));
#138379=CARTESIAN_POINT('Ctrl Pts',(-4.830724789,1.586734015,5.406162966));
#138380=CARTESIAN_POINT('Ctrl Pts',(-4.8207167940839,1.5845140572787,5.41510569849458));
#138381=CARTESIAN_POINT('Ctrl Pts',(-4.81070879916784,1.58229409955743,
5.42404843098929));
#138382=CARTESIAN_POINT('Ctrl Pts',(-5.73626078559967,1.716084912,4.83249851653737));
#138383=CARTESIAN_POINT('Ctrl Pts',(-5.47361588967387,1.651909459,5.14426263175886));
#138384=CARTESIAN_POINT('Ctrl Pts',(-5.17872930032388,1.586734015,5.42572507124403));
#138385=CARTESIAN_POINT('Ctrl Pts',(-5.1686850916349,1.5845140572787,5.43531203647878));
#138386=CARTESIAN_POINT('Ctrl Pts',(-5.15864088294596,1.58229409955742,
5.44489900171361));
#138387=CARTESIAN_POINT('',(-5.00437462239016,1.58673401622021,5.41592421368356));
#138388=CARTESIAN_POINT('Ctrl Pts',(-4.830724789,1.586734015,5.406162966));
#138389=CARTESIAN_POINT('Ctrl Pts',(-4.783806095,1.596957843,5.448087581));
#138390=CARTESIAN_POINT('Ctrl Pts',(-4.736166816,1.607142857,5.489191552));
#138391=CARTESIAN_POINT('Ctrl Pts',(-4.483452941,1.661171687,5.707237335));
#138392=CARTESIAN_POINT('Ctrl Pts',(-4.211773557,1.716105035,5.901140864));
#138393=CARTESIAN_POINT('Ctrl Pts',(-4.811202304,1.586734015,5.753462644));
#138394=CARTESIAN_POINT('Ctrl Pts',(-4.761269485,1.596957843,5.795217828));
#138395=CARTESIAN_POINT('Ctrl Pts',(-4.710619476,1.607142857,5.83610008));
#138396=CARTESIAN_POINT('Ctrl Pts',(-4.44193447,1.661171687,6.052969703));
#138397=CARTESIAN_POINT('Ctrl Pts',(-4.154459583,1.716105035,6.244234587));
#138398=CARTESIAN_POINT('',(-4.81120229945899,1.58673401412069,5.75346264667531));
#138399=CARTESIAN_POINT('',(-4.36052349819178,1.67637478035157,6.10211724071305));
#138400=CARTESIAN_POINT('Ctrl Pts',(-4.81120230059445,1.58673401434349,
5.75346264633348));
#138401=CARTESIAN_POINT('Ctrl Pts',(-4.77788371487983,1.59355605125278,
5.78132455595149));
#138402=CARTESIAN_POINT('Ctrl Pts',(-4.74435316195746,1.60035948085479,
5.80887187081411));
#138403=CARTESIAN_POINT('Ctrl Pts',(-4.71061947665077,1.60714285723673,
5.83610008020754));
#138404=CARTESIAN_POINT('Ctrl Pts',(-4.59689695616064,1.63001087929168,
5.92789143275329));
#138405=CARTESIAN_POINT('Ctrl Pts',(-4.48011387691959,1.65310706412176,
6.01665892591959));
#138406=CARTESIAN_POINT('Ctrl Pts',(-4.36052350170302,1.67637478135664,
6.10211723839322));
#138407=CARTESIAN_POINT('Ctrl Pts',(-4.21563855474019,1.7153233868915,5.89838042160329));
#138408=CARTESIAN_POINT('Ctrl Pts',(-4.2396580786889,1.70851142675315,5.93235434885314));
#138409=CARTESIAN_POINT('Ctrl Pts',(-4.2637584022233,1.70186463282375,5.96633656926233));
#138410=CARTESIAN_POINT('Ctrl Pts',(-4.3120479764043,1.68889233603723,6.03423510042615));
#138411=CARTESIAN_POINT('Ctrl Pts',(-4.33626590225745,1.68255913648983,
6.06819171687066));
#138412=CARTESIAN_POINT('Ctrl Pts',(-4.36052349387761,1.67637477936853,
6.10211724361858));
#138413=CARTESIAN_POINT('',(-4.82096354039051,1.58673401368698,5.5798128102786));
#138414=CARTESIAN_POINT('Origin',(-4.59918561568351E-13,1.67745375799967,
6.99960922556642E-13));
#138415=CARTESIAN_POINT('',(-4.36636804460131,1.49654505819906,6.0979365443449));
#138416=CARTESIAN_POINT('Origin',(0.110128493780438,1.48214560147655,-0.157790257786166));
#138417=CARTESIAN_POINT('',(-3.89060313579184,1.58673401497661,6.41195814384654));
#138418=CARTESIAN_POINT('Origin',(0.127067328912721,1.33942798463397,-0.134439566054244));
#138419=CARTESIAN_POINT('Origin',(0.0831730144276299,1.48219940270008,-0.169354622117295));
#138420=CARTESIAN_POINT('Ctrl Pts',(-4.219441475,1.716084912,5.895660577));
#138421=CARTESIAN_POINT('Ctrl Pts',(-3.899014027,1.651909459,6.124986001));
#138422=CARTESIAN_POINT('Ctrl Pts',(-3.555619896,1.586734015,6.318232914));
#138423=CARTESIAN_POINT('Ctrl Pts',(-3.54392346041923,1.58451405748362,
6.32481514667389));
#138424=CARTESIAN_POINT('Ctrl Pts',(-3.53222702483845,1.58229409996724,
6.33139737934781));
#138425=CARTESIAN_POINT('Ctrl Pts',(-4.56330586303262,1.716084912,5.95264389354036));
#138426=CARTESIAN_POINT('Ctrl Pts',(-4.2397813894512,1.651909459,6.20065824728892));
#138427=CARTESIAN_POINT('Ctrl Pts',(-3.89128298046772,1.586734015,6.4121483522595));
#138428=CARTESIAN_POINT('Ctrl Pts',(-3.87941268676526,1.58451405748362,
6.41935197097467));
#138429=CARTESIAN_POINT('Ctrl Pts',(-3.86754239306272,1.58229409996724,
6.42655558968996));
#138430=CARTESIAN_POINT('',(-3.72311151290708,1.58673401622019,6.36509553085638));
#138431=CARTESIAN_POINT('Ctrl Pts',(-3.555619896,1.586734015,6.318232914));
#138432=CARTESIAN_POINT('Ctrl Pts',(-3.500785581,1.596957843,6.34909122300001));
#138433=CARTESIAN_POINT('Ctrl Pts',(-3.445423944,1.607142857,6.378993169));
#138434=CARTESIAN_POINT('Ctrl Pts',(-3.15174498,1.661171687,6.53761515));
#138435=CARTESIAN_POINT('Ctrl Pts',(-2.844733783,1.716105035,6.668582286));
#138436=CARTESIAN_POINT('Ctrl Pts',(-3.46189467,1.586734015,6.653216162));
#138437=CARTESIAN_POINT('Ctrl Pts',(-3.404153122,1.596957843,6.683261053));
#138438=CARTESIAN_POINT('Ctrl Pts',(-3.345898807,1.607142857,6.712299246));
#138439=CARTESIAN_POINT('Ctrl Pts',(-3.036874949,1.661171687,6.86633924400001));
#138440=CARTESIAN_POINT('Ctrl Pts',(-2.715004769,1.716105035,6.991333857));
#138441=CARTESIAN_POINT('',(-3.46189466553869,1.5867340145549,6.653216163509));
#138442=CARTESIAN_POINT('',(-2.94680205198768,1.67637477917517,6.89683678639208));
#138443=CARTESIAN_POINT('Ctrl Pts',(-3.46189466668291,1.58673401558733,
6.653216163726));
#138444=CARTESIAN_POINT('Ctrl Pts',(-3.42336556352834,1.59355605166269,
6.67326416630461));
#138445=CARTESIAN_POINT('Ctrl Pts',(-3.38469707774585,1.60035948085472,
6.69295936235249));
#138446=CARTESIAN_POINT('Ctrl Pts',(-3.34589880719225,1.60714285696639,
6.71229924590417));
#138447=CARTESIAN_POINT('Ctrl Pts',(-3.21510262968249,1.63001087914796,
6.77749758707386));
#138448=CARTESIAN_POINT('Ctrl Pts',(-3.08196748589179,1.65310706302618,
6.83908483597189));
#138449=CARTESIAN_POINT('Ctrl Pts',(-2.94680205576956,1.67637477805243,
6.89683678453843));
#138450=CARTESIAN_POINT('Ctrl Pts',(-2.8491018325826,1.71532338701036,6.66671724050236));
#138451=CARTESIAN_POINT('Ctrl Pts',(-2.86525640264206,1.70851142706009,
6.70506036268628));
#138452=CARTESIAN_POINT('Ctrl Pts',(-2.881488100747,1.70186463322583,6.74342895411978));
#138453=CARTESIAN_POINT('Ctrl Pts',(-2.91405251523444,1.68889233606425,
6.82012088845218));
#138454=CARTESIAN_POINT('Ctrl Pts',(-2.93040457065015,1.6825591365248,6.85848975614808));
#138455=CARTESIAN_POINT('Ctrl Pts',(-2.94680204793491,1.67637477938092,
6.89683678815825));
#138456=CARTESIAN_POINT('',(-3.50875727589861,1.58673401368698,6.48572454184184));
#138457=CARTESIAN_POINT('Origin',(7.02563007770607E-14,1.67745375799983,
-7.28583859910259E-14));
#138458=CARTESIAN_POINT('',(-2.95340868202948,1.49654505841521,6.89401023776211));
#138459=CARTESIAN_POINT('Origin',(0.0736336045579739,1.4821457425204,-0.177775726754538));
#138460=CARTESIAN_POINT('',(-2.4212615321408,1.58673401497661,7.0984147942295));
#138461=CARTESIAN_POINT('Origin',(0.0951960600761595,1.33942795485371,-0.158612234490675));
#138462=CARTESIAN_POINT('Origin',(0.0448223004672105,1.48219937047135,-0.183275116942858));
#138463=CARTESIAN_POINT('Ctrl Pts',(-2.853400528,1.716084912,6.6648785));
#138464=CARTESIAN_POINT('Ctrl Pts',(-2.491166309,1.651909459,6.819959994));
#138465=CARTESIAN_POINT('Ctrl Pts',(-2.114258167,1.586734015,6.934869314));
#138466=CARTESIAN_POINT('Ctrl Pts',(-2.10142020173575,1.5845140574217,6.93878326993332));
#138467=CARTESIAN_POINT('Ctrl Pts',(-2.08858223647144,1.58229409984341,
6.94269722586663));
#138468=CARTESIAN_POINT('Ctrl Pts',(-3.17697582941391,1.716084912,6.79445025702993));
#138469=CARTESIAN_POINT('Ctrl Pts',(-2.80769942347321,1.651909459,6.96711797440578));
#138470=CARTESIAN_POINT('Ctrl Pts',(-2.42188459325229,1.586734015,7.09874670217079));
#138471=CARTESIAN_POINT('Ctrl Pts',(-2.4087432549874,1.5845140574217,7.10323014215661));
#138472=CARTESIAN_POINT('Ctrl Pts',(-2.39560191672256,1.58229409984341,
7.10771358214244));
#138473=CARTESIAN_POINT('',(-2.26775984623204,1.58673401622023,7.01664205534898));
#138474=CARTESIAN_POINT('Ctrl Pts',(-2.114258167,1.586734015,6.934869314));
#138475=CARTESIAN_POINT('Ctrl Pts',(-2.054072224,1.596957843,6.95321841600001));
#138476=CARTESIAN_POINT('Ctrl Pts',(-1.993576877,1.607142857,6.970520155));
#138477=CARTESIAN_POINT('Ctrl Pts',(-1.672664928,1.661171687,7.06230134600001));
#138478=CARTESIAN_POINT('Ctrl Pts',(-1.344677418,1.716105035,7.124208212));
#138479=CARTESIAN_POINT('Ctrl Pts',(-1.95071269,1.586734015,7.241872686));
#138480=CARTESIAN_POINT('Ctrl Pts',(-1.887862343,1.596957843,7.258802419));
#138481=CARTESIAN_POINT('Ctrl Pts',(-1.824727629,1.607142857,7.274638759));
#138482=CARTESIAN_POINT('Ctrl Pts',(-1.48981453,1.661171687,7.358646393));
#138483=CARTESIAN_POINT('Ctrl Pts',(-1.148599349,1.716105035,7.411526127));
#138484=CARTESIAN_POINT('',(-1.95071268475582,1.58673401412067,7.24187268671358));
#138485=CARTESIAN_POINT('',(-1.39529141789594,1.67637478035405,7.36906790958503));
#138486=CARTESIAN_POINT('Ctrl Pts',(-1.95071268604658,1.58673401434349,
7.24187268712292));
#138487=CARTESIAN_POINT('Ctrl Pts',(-1.90877464357686,1.59355605125278,
7.25316936065035));
#138488=CARTESIAN_POINT('Ctrl Pts',(-1.86677632062753,1.60035948085479,
7.26409151275274));
#138489=CARTESIAN_POINT('Ctrl Pts',(-1.82472762875065,1.60714285723673,
7.27463875947624));
#138490=CARTESIAN_POINT('Ctrl Pts',(-1.68297367624678,1.63001087929739,
7.31019548774422));
#138491=CARTESIAN_POINT('Ctrl Pts',(-1.53971172097606,1.65310706412721,
7.34172274042649));
#138492=CARTESIAN_POINT('Ctrl Pts',(-1.39529142198336,1.67637478135573,
7.3690679090194));
#138493=CARTESIAN_POINT('Ctrl Pts',(-1.349344274309,1.71532338715986,7.12332577116148));
#138494=CARTESIAN_POINT('Ctrl Pts',(-1.35687852187631,1.70851142713905,
7.16424520772288));
#138495=CARTESIAN_POINT('Ctrl Pts',(-1.36448261923405,1.70186463308513,
7.20520609934646));
#138496=CARTESIAN_POINT('Ctrl Pts',(-1.37979919683592,1.68889233604116,
7.28710540449341));
#138497=CARTESIAN_POINT('Ctrl Pts',(-1.38752077788562,1.68255913650202,
7.32809243790103));
#138498=CARTESIAN_POINT('Ctrl Pts',(-1.39529141286165,1.6763747793784,7.36906791039249));
#138499=CARTESIAN_POINT('',(-2.03248542073876,1.58673401368698,7.08837100222542));
#138500=CARTESIAN_POINT('Origin',(2.86988315056913E-13,1.67745375800067,
-1.91426735574041E-12));
#138501=CARTESIAN_POINT('',(-1.40235121259847,1.49654505820771,7.36772767361412));
#138502=CARTESIAN_POINT('Origin',(0.0336955570525715,1.48214561198427,-0.189448532417833));
#138503=CARTESIAN_POINT('',(-0.838704434774169,1.58673401541122,7.45295745902514));
#138504=CARTESIAN_POINT('Origin',(0.058873471499683,1.3394279908441,-0.175368207935244));
#138505=CARTESIAN_POINT('Origin',(0.00437563783938805,1.48219935231658,
-0.18862567772804));
#138506=CARTESIAN_POINT('Ctrl Pts',(-1.353937744,1.716084912,7.122454113));
#138507=CARTESIAN_POINT('Ctrl Pts',(-0.966834423,1.651909459,7.196040237));
#138508=CARTESIAN_POINT('Ctrl Pts',(-0.574036077,1.586734015,7.227238932));
#138509=CARTESIAN_POINT('Ctrl Pts',(-0.560656871444095,1.58451405742799,
7.22830159877987));
#138510=CARTESIAN_POINT('Ctrl Pts',(-0.547277665888199,1.582294099856,7.22936426555975));
#138511=CARTESIAN_POINT('Ctrl Pts',(-1.64209393708288,1.716084912,7.3185556786243));
#138512=CARTESIAN_POINT('Ctrl Pts',(-1.24433255270257,1.651909459,7.40780300915423));
#138513=CARTESIAN_POINT('Ctrl Pts',(-0.839241573735745,1.586734015,7.45341554632637));
#138514=CARTESIAN_POINT('Ctrl Pts',(-0.825443665644656,1.58451405742799,
7.4549691666941));
#138515=CARTESIAN_POINT('Ctrl Pts',(-0.811645757553577,1.582294099856,7.45652278706179));
#138516=CARTESIAN_POINT('',(-0.706370249897001,1.58673401622023,7.34009819573167));
#138517=CARTESIAN_POINT('Origin',(3.25802752831894E-14,1.67745375800039,
5.0263612716428E-13));
#138518=CARTESIAN_POINT('',(0.214278640529097,1.49654505838871,7.49693835249985));
#138519=CARTESIAN_POINT('',(-0.34831754416533,1.58673401414387,7.49190729318426));
#138520=CARTESIAN_POINT('Origin',(-0.00781804144820934,1.48214575524756,
-0.192262944512581));
#138521=CARTESIAN_POINT('Origin',(0.0197980510459872,1.33942797864341,-0.183924310824504));
#138522=CARTESIAN_POINT('Ctrl Pts',(-0.348317544006022,1.5867340149536,
7.49190729310884));
#138523=CARTESIAN_POINT('Ctrl Pts',(-0.304931542030917,1.59355605145578,
7.49392441706153));
#138524=CARTESIAN_POINT('Ctrl Pts',(-0.261567178121288,1.60035948085479,
7.49556281730996));
#138525=CARTESIAN_POINT('Ctrl Pts',(-0.218234214930498,1.60714285723674,
7.49682424946948));
#138526=CARTESIAN_POINT('Ctrl Pts',(-0.0721507453448591,1.63001087927846,
7.501076771636));
#138527=CARTESIAN_POINT('Ctrl Pts',(0.0745392523939352,1.65310706410833,
7.50106984908632));
#138528=CARTESIAN_POINT('Ctrl Pts',(0.221461488025658,1.67637478135631,
7.49672960759033));
#138529=CARTESIAN_POINT('Ctrl Pts',(-0.574036077,1.586734015,7.227238932));
#138530=CARTESIAN_POINT('Ctrl Pts',(-0.511312734,1.596957843,7.23222084300001));
#138531=CARTESIAN_POINT('Ctrl Pts',(-0.448512371,1.607142857,7.236113367));
#138532=CARTESIAN_POINT('Ctrl Pts',(-0.115372922,1.661171687,7.256762181));
#138533=CARTESIAN_POINT('Ctrl Pts',(0.218254568,1.716105035,7.246714079));
#138534=CARTESIAN_POINT('Ctrl Pts',(-0.348317552,1.586734015,7.491907293));
#138535=CARTESIAN_POINT('Ctrl Pts',(-0.28329722,1.596957843,7.494930251));
#138536=CARTESIAN_POINT('Ctrl Pts',(-0.218234215,1.607142857,7.496824249));
#138537=CARTESIAN_POINT('Ctrl Pts',(0.12690796,1.661171687,7.506871415));
#138538=CARTESIAN_POINT('Ctrl Pts',(0.4715133,1.716105035,7.485163673));
#138539=CARTESIAN_POINT('',(-0.461176806441667,1.58673401368695,7.35957311300496));
#138540=CARTESIAN_POINT('Ctrl Pts',(-1.16218918388351,4.30331728230629,
7.40941170763586));
#138541=CARTESIAN_POINT('Ctrl Pts',(-1.15818926544175,4.30267205415314,
7.41003468381793));
#138542=CARTESIAN_POINT('Ctrl Pts',(-1.154189347,4.302026826,7.41065766));
#138543=CARTESIAN_POINT('Ctrl Pts',(-0.752921796,4.237298226,7.473153966));
#138544=CARTESIAN_POINT('Ctrl Pts',(-0.347252113,4.172121859,7.49195675200001));
#138545=CARTESIAN_POINT('Ctrl Pts',(-1.35774016039859,4.30331728230629,
7.12173454350632));
#138546=CARTESIAN_POINT('Ctrl Pts',(-1.35389540219929,4.30267205415314,
7.12246323625316));
#138547=CARTESIAN_POINT('Ctrl Pts',(-1.350050644,4.302026826,7.123191929));
#138548=CARTESIAN_POINT('Ctrl Pts',(-0.964348603,4.237298226,7.196293608));
#138549=CARTESIAN_POINT('Ctrl Pts',(-0.573008275,4.172121859,7.227320494));
#138550=CARTESIAN_POINT('',(-0.596334988833243,4.21216499469303,7.47625471614313));
#138551=CARTESIAN_POINT('Ctrl Pts',(-0.596334996445509,4.21216499507849,
7.47625471552231));
#138552=CARTESIAN_POINT('Ctrl Pts',(-0.593257936526993,4.20594050668202,
7.43465989744348));
#138553=CARTESIAN_POINT('Ctrl Pts',(-0.590163983306183,4.19956141145742,
7.39306522936547));
#138554=CARTESIAN_POINT('Ctrl Pts',(-0.583946887358536,4.18648410045661,
7.30997722747781));
#138555=CARTESIAN_POINT('Ctrl Pts',(-0.58082009119411,4.17977820241928,
7.2684350382799));
#138556=CARTESIAN_POINT('Ctrl Pts',(-0.577677422272544,4.17289950750523,
7.22694879429211));
#138557=CARTESIAN_POINT('',(-1.15418934995013,4.30202682545374,7.41065766134707));
#138558=CARTESIAN_POINT('Origin',(0.00695330665491684,4.16072878976292,
-0.19114668498882));
#138559=CARTESIAN_POINT('',(-1.252120005472,4.30202682438465,7.26692479278178));
#138560=CARTESIAN_POINT('Ctrl Pts',(-2.429504099,4.172114527,7.095597919));
#138561=CARTESIAN_POINT('Ctrl Pts',(-2.089017748,4.22940039,7.212179072));
#138562=CARTESIAN_POINT('Ctrl Pts',(-1.738933089,4.285714286,7.295622778));
#138563=CARTESIAN_POINT('Ctrl Pts',(-1.688306028,4.29385805,7.307689886));
#138564=CARTESIAN_POINT('Ctrl Pts',(-1.637516375,4.302026826,7.319053226));
#138565=CARTESIAN_POINT('Ctrl Pts',(-2.12231099,4.172114527,6.932409109));
#138566=CARTESIAN_POINT('Ctrl Pts',(-1.789655348,4.22940039,7.034249424));
#138567=CARTESIAN_POINT('Ctrl Pts',(-1.448776863,4.285714286,7.103769816));
#138568=CARTESIAN_POINT('Ctrl Pts',(-1.399481142,4.29385805,7.11382342199999));
#138569=CARTESIAN_POINT('Ctrl Pts',(-1.350050644,4.302026826,7.12319192899999));
#138570=CARTESIAN_POINT('',(-1.63751638118266,4.30202682641445,7.31905322493326));
#138571=CARTESIAN_POINT('',(-1.49378351347216,4.30202682665757,7.2211225766783));
#138572=CARTESIAN_POINT('',(-2.18956677646246,4.21216499392671,7.17326964037794));
#138573=CARTESIAN_POINT('Ctrl Pts',(-1.63751638169652,4.30202682552111,
7.31905322426853));
#138574=CARTESIAN_POINT('Ctrl Pts',(-1.67140098825403,4.29657697961046,
7.31147210733645));
#138575=CARTESIAN_POINT('Ctrl Pts',(-1.70520808357999,4.29113922035365,
7.3036612314913));
#138576=CARTESIAN_POINT('Ctrl Pts',(-1.73893308847754,4.28571428571329,
7.29562277765223));
#138577=CARTESIAN_POINT('Ctrl Pts',(-1.88988482580287,4.26143250098634,
7.25964298829109));
#138578=CARTESIAN_POINT('Ctrl Pts',(-2.04024794992858,4.23689343089983,
7.21884767604786));
#138579=CARTESIAN_POINT('Ctrl Pts',(-2.18956676991572,4.21216499285672,
7.17326964222597));
#138580=CARTESIAN_POINT('Ctrl Pts',(-2.11775200805595,4.17289950701588,
6.9338031746523));
#138581=CARTESIAN_POINT('Ctrl Pts',(-2.1297395193464,4.17977820193676,6.97364391235997));
#138582=CARTESIAN_POINT('Ctrl Pts',(-2.14172355644561,4.18648410048624,
7.01354270257986));
#138583=CARTESIAN_POINT('Ctrl Pts',(-2.16565676462317,4.19956141148085,
7.09335166142063));
#138584=CARTESIAN_POINT('Ctrl Pts',(-2.17762000701025,4.20594050665356,
7.13330876057114));
#138585=CARTESIAN_POINT('Ctrl Pts',(-2.18956678338983,4.21216499505426,
7.17326963813129));
#138586=CARTESIAN_POINT('Ctrl Pts',(-2.7278223432099,4.30331728230629,6.98634745883686));
#138587=CARTESIAN_POINT('Ctrl Pts',(-2.72404986210495,4.30267205415314,
6.98781573441843));
#138588=CARTESIAN_POINT('Ctrl Pts',(-2.720277381,4.302026826,6.98928401000001));
#138589=CARTESIAN_POINT('Ctrl Pts',(-2.341826101,4.237298226,7.13657985));
#138590=CARTESIAN_POINT('Ctrl Pts',(-1.949682793,4.172121859,7.242150027));
#138591=CARTESIAN_POINT('Ctrl Pts',(-2.85695935998706,4.30331728230629,
6.66335834764232));
#138592=CARTESIAN_POINT('Ctrl Pts',(-2.85336113749353,4.30267205415314,
6.66489651332116));
#138593=CARTESIAN_POINT('Ctrl Pts',(-2.849762915,4.302026826,6.666434679));
#138594=CARTESIAN_POINT('Ctrl Pts',(-2.488793073,4.237298226,6.820741819));
#138595=CARTESIAN_POINT('Ctrl Pts',(-2.113271928,4.172121859,6.935169916));
#138596=CARTESIAN_POINT('',(-2.72027738416813,4.30202682545393,6.98928401068239));
#138597=CARTESIAN_POINT('Origin',(0.0478815511175334,4.16072878634873,-0.185182782745746));
#138598=CARTESIAN_POINT('',(-2.78502015736614,4.30202682438522,6.82785934067964));
#138599=CARTESIAN_POINT('Origin',(-2.65629532258949E-14,4.39277644300044,
3.06178693509906E-13));
#138600=CARTESIAN_POINT('',(-2.18434923164388,4.39169923735961,7.17486016787817));
#138601=CARTESIAN_POINT('Origin',(0.0183603401161009,4.16082469438197,-0.185324740864866));
#138602=CARTESIAN_POINT('Origin',(0.0286009939169851,4.55341984216358,-0.182407753897521));
#138603=CARTESIAN_POINT('Ctrl Pts',(-3.898047452,4.172114527,6.407435217));
#138604=CARTESIAN_POINT('Ctrl Pts',(-3.590582984,4.22940039,6.594485268));
#138605=CARTESIAN_POINT('Ctrl Pts',(-3.26662104,4.285714286,6.75123596));
#138606=CARTESIAN_POINT('Ctrl Pts',(-3.219771683,4.29385805,6.77390426700001));
#138607=CARTESIAN_POINT('Ctrl Pts',(-3.172612246,4.302026826,6.795920213));
#138608=CARTESIAN_POINT('Ctrl Pts',(-3.562955577,4.172114527,6.31409910900001));
#138609=CARTESIAN_POINT('Ctrl Pts',(-3.259969896,4.22940039,6.485069584));
#138610=CARTESIAN_POINT('Ctrl Pts',(-2.94200579,4.285714286,6.626243425));
#138611=CARTESIAN_POINT('Ctrl Pts',(-2.896023804,4.29385805,6.646659106));
#138612=CARTESIAN_POINT('Ctrl Pts',(-2.849762915,4.302026826,6.666434679));
#138613=CARTESIAN_POINT('',(-3.17261225178721,4.30202682641445,6.79592021059555));
#138614=CARTESIAN_POINT('',(-3.01118758420266,4.30202682665757,6.73117744434362));
#138615=CARTESIAN_POINT('',(-3.68041685431122,4.21216499393234,6.53487044845151));
#138616=CARTESIAN_POINT('Ctrl Pts',(-3.17261225212519,4.30202682552111,
6.79592020977771));
#138617=CARTESIAN_POINT('Ctrl Pts',(-3.20407493953318,4.29657697961046,
6.78123214628165));
#138618=CARTESIAN_POINT('Ctrl Pts',(-3.23541253640356,4.29113922035365,
6.76633635817626));
#138619=CARTESIAN_POINT('Ctrl Pts',(-3.26662103946589,4.28571428571329,
6.75123595977202));
#138620=CARTESIAN_POINT('Ctrl Pts',(-3.40630901782547,4.26143250099806,
6.68364719650128));
#138621=CARTESIAN_POINT('Ctrl Pts',(-3.54438694943116,4.23689343091171,
6.61148202900684));
#138622=CARTESIAN_POINT('Ctrl Pts',(-3.68041684841466,4.21216499285689,
6.5348704518074));
#138623=CARTESIAN_POINT('Ctrl Pts',(-3.55880286439848,4.17289950713874,
6.31644062907105));
#138624=CARTESIAN_POINT('Ctrl Pts',(-3.57907469528383,4.17977820208842,
6.35277295199961));
#138625=CARTESIAN_POINT('Ctrl Pts',(-3.59935561209294,4.18648410044242,
6.38916271579995));
#138626=CARTESIAN_POINT('Ctrl Pts',(-3.63988584216034,4.19956141147502,
6.4619608532525));
#138627=CARTESIAN_POINT('Ctrl Pts',(-3.66015898579949,4.20594050667283,
6.498412034188));
#138628=CARTESIAN_POINT('Ctrl Pts',(-3.6804168605763,4.21216499507368,6.53487044477551));
#138629=CARTESIAN_POINT('Ctrl Pts',(-4.16590556149365,4.30331728230629,
6.23660936793102));
#138630=CARTESIAN_POINT('Ctrl Pts',(-4.16253691474683,4.30267205415314,
6.23885428796551));
#138631=CARTESIAN_POINT('Ctrl Pts',(-4.159168268,4.302026826,6.241099208));
#138632=CARTESIAN_POINT('Ctrl Pts',(-3.82122922,4.237298226,6.466307191));
#138633=CARTESIAN_POINT('Ctrl Pts',(-3.460948472,4.172121859,6.653708415));
#138634=CARTESIAN_POINT('Ctrl Pts',(-4.22259031477876,4.30331728230629,
5.8934109206062));
#138635=CARTESIAN_POINT('Ctrl Pts',(-4.21940687688938,4.30267205415314,
5.8956866363031));
#138636=CARTESIAN_POINT('Ctrl Pts',(-4.216223439,4.302026826,5.897962352));
#138637=CARTESIAN_POINT('Ctrl Pts',(-3.896864346,4.237298226,6.126259723));
#138638=CARTESIAN_POINT('Ctrl Pts',(-3.554721335,4.172121859,6.3187385));
#138639=CARTESIAN_POINT('',(-4.1591682712504,4.30202682545375,6.24109920797393));
#138640=CARTESIAN_POINT('Origin',(0.0865709208982096,4.16072878307092,-0.170560193251753));
#138641=CARTESIAN_POINT('',(-4.18769586182889,4.30202682438465,6.06953077425346));
#138642=CARTESIAN_POINT('Origin',(-2.08166817117217E-14,4.39277644300022,
1.63931368479808E-13));
#138643=CARTESIAN_POINT('',(-3.6756632088494,4.39169923737625,6.53754540854676));
#138644=CARTESIAN_POINT('Origin',(0.0577704175562865,4.16082470835826,-0.177044994129791));
#138645=CARTESIAN_POINT('Origin',(0.0671445342074956,4.55341983699392,-0.171994702565974));
#138646=CARTESIAN_POINT('Ctrl Pts',(-5.18432243800001,4.172114527,5.419667966));
#138647=CARTESIAN_POINT('Ctrl Pts',(-4.92425655,4.22940039,5.668440663));
#138648=CARTESIAN_POINT('Ctrl Pts',(-4.641565421,4.285714286,5.891168852));
#138649=CARTESIAN_POINT('Ctrl Pts',(-4.600684393,4.29385805,5.923378414));
#138650=CARTESIAN_POINT('Ctrl Pts',(-4.55936029400001,4.302026826,5.955017524));
#138651=CARTESIAN_POINT('Ctrl Pts',(-4.83700032,4.172114527,5.400548852));
#138652=CARTESIAN_POINT('Ctrl Pts',(-4.577851874,4.22940039,5.632655097));
#138653=CARTESIAN_POINT('Ctrl Pts',(-4.297669796,4.285714286,5.838881257));
#138654=CARTESIAN_POINT('Ctrl Pts',(-4.25715161,4.29385805,5.868704398));
#138655=CARTESIAN_POINT('Ctrl Pts',(-4.216223439,4.302026826,5.897962352));
#138656=CARTESIAN_POINT('',(-4.55936029919639,4.30202682641445,5.9550175204685));
#138657=CARTESIAN_POINT('',(-4.38779186976002,4.30202682665757,5.92648993558638));
#138658=CARTESIAN_POINT('',(-4.99917473014842,4.21216499393112,5.59090797795424));
#138659=CARTESIAN_POINT('Ctrl Pts',(-4.55936029942192,4.30202682552111,
5.95501751971019));
#138660=CARTESIAN_POINT('Ctrl Pts',(-4.58692990753124,4.29657697961046,
5.93390930696889));
#138661=CARTESIAN_POINT('Ctrl Pts',(-4.61433269467468,4.29113922035365,
5.91262511711567));
#138662=CARTESIAN_POINT('Ctrl Pts',(-4.6415654209329,4.28571428571329,5.89116885203607));
#138663=CARTESIAN_POINT('Ctrl Pts',(-4.76345798551428,4.26143250100584,
5.79513149051414));
#138664=CARTESIAN_POINT('Ctrl Pts',(-4.88279435397564,4.23689343091949,
5.69497083082674));
#138665=CARTESIAN_POINT('Ctrl Pts',(-4.99917472505921,4.21216499285672,
5.59090798245948));
#138666=CARTESIAN_POINT('Ctrl Pts',(-4.83344805250004,4.17289950697198,
5.40372833833061));
#138667=CARTESIAN_POINT('Ctrl Pts',(-4.86105631482581,4.17977820193647,
5.43485338735993));
#138668=CARTESIAN_POINT('Ctrl Pts',(-4.88868579927659,4.18648410044146,
5.46603258182227));
#138669=CARTESIAN_POINT('Ctrl Pts',(-4.94391790281236,4.19956141147817,
5.52841593800416));
#138670=CARTESIAN_POINT('Ctrl Pts',(-4.97155299800196,4.20594050666816,
5.55965678400575));
#138671=CARTESIAN_POINT('Ctrl Pts',(-4.99917473548726,4.2121649950684,5.59090797300892));
#138672=CARTESIAN_POINT('Ctrl Pts',(-5.40919566542744,4.30331728230629,
5.19525435393708));
#138673=CARTESIAN_POINT('Ctrl Pts',(-5.40638836721372,4.30267205415314,
5.19817094846854));
#138674=CARTESIAN_POINT('Ctrl Pts',(-5.403581069,4.302026826,5.201087543));
#138675=CARTESIAN_POINT('Ctrl Pts',(-5.121955907,4.237298226,5.493677195));
#138676=CARTESIAN_POINT('Ctrl Pts',(-4.810384047,4.172121859,5.754146794));
#138677=CARTESIAN_POINT('Ctrl Pts',(-5.39077763956017,4.30331728230629,
4.84789414945679));
#138678=CARTESIAN_POINT('Ctrl Pts',(-5.38815784028008,4.30267205415314,
4.8508010052284));
#138679=CARTESIAN_POINT('Ctrl Pts',(-5.385538041,4.302026826,4.853707861));
#138680=CARTESIAN_POINT('Ctrl Pts',(-5.122722572,4.237298226,5.145320531));
#138681=CARTESIAN_POINT('Ctrl Pts',(-4.829955922,4.172121859,5.406849895));
#138682=CARTESIAN_POINT('',(-5.40358107215755,4.30202682545392,5.2010875422987));
#138683=CARTESIAN_POINT('Origin',(0.121212436242013,4.1607287553436,-0.147962496286492));
#138684=CARTESIAN_POINT('',(-5.39455956189629,4.30202682438524,5.02739769460006));
#138685=CARTESIAN_POINT('Origin',(4.87457296749483E-13,4.39277644300022,
-4.17634676841416E-13));
#138686=CARTESIAN_POINT('',(-4.9951072604849,4.3916992374024,5.59454229148361));
#138687=CARTESIAN_POINT('Origin',(0.0944792292999891,4.16082469009487,-0.160486871840761));
#138688=CARTESIAN_POINT('Origin',(0.102548316312207,4.55341980934995,-0.153539253888896));
#138689=CARTESIAN_POINT('Ctrl Pts',(-6.228184269,4.172114527,4.178483064));
#138690=CARTESIAN_POINT('Ctrl Pts',(-6.027677353,4.22940039,4.477346072));
#138691=CARTESIAN_POINT('Ctrl Pts',(-5.799475362,4.285714286,4.755637236));
#138692=CARTESIAN_POINT('Ctrl Pts',(-5.766474213,4.29385805,4.795881969));
#138693=CARTESIAN_POINT('Ctrl Pts',(-5.73291772300001,4.302026826,4.835664834));
#138694=CARTESIAN_POINT('Ctrl Pts',(-5.884872305,4.172114527,4.234474933));
#138695=CARTESIAN_POINT('Ctrl Pts',(-5.681678587,4.22940039,4.516863918));
#138696=CARTESIAN_POINT('Ctrl Pts',(-5.452379538,4.285714286,4.77849949));
#138697=CARTESIAN_POINT('Ctrl Pts',(-5.419219739,4.29385805,4.81633559500001));
#138698=CARTESIAN_POINT('Ctrl Pts',(-5.385538041,4.302026826,4.853707861));
#138699=CARTESIAN_POINT('',(-5.73291772724476,4.30202682620655,4.83566482943548));
#138700=CARTESIAN_POINT('',(-5.55922788466495,4.30202682665757,4.844686344442));
#138701=CARTESIAN_POINT('',(-6.08417675202275,4.21216499536652,4.38552086333923));
#138702=CARTESIAN_POINT('Ctrl Pts',(-5.73291772722235,4.3020268248974,4.83566482864614));
#138703=CARTESIAN_POINT('Ctrl Pts',(-5.75530513081357,4.29657697940857,
4.80912346338663));
#138704=CARTESIAN_POINT('Ctrl Pts',(-5.77749178408189,4.29113922035363,
4.78244609672125));
#138705=CARTESIAN_POINT('Ctrl Pts',(-5.79947536162674,4.28571428598682,
4.75563723596294));
#138706=CARTESIAN_POINT('Ctrl Pts',(-5.89787295242218,4.26143250093749,
4.63564187593636));
#138707=CARTESIAN_POINT('Ctrl Pts',(-5.9928877215738,4.23689343233045,4.51216912531119));
#138708=CARTESIAN_POINT('Ctrl Pts',(-6.08417674795619,4.21216499709052,
4.38552086837866));
#138709=CARTESIAN_POINT('Ctrl Pts',(-5.88208658344157,4.17289950707543,
4.23834371760513));
#138710=CARTESIAN_POINT('Ctrl Pts',(-5.91574034525287,4.17977820202404,
4.26280611985181));
#138711=CARTESIAN_POINT('Ctrl Pts',(-5.9494264724858,4.18648410047085,4.28731683939213));
#138712=CARTESIAN_POINT('Ctrl Pts',(-6.01677785733755,4.19956141147629,
4.33636843760983));
#138713=CARTESIAN_POINT('Ctrl Pts',(-6.05048271772771,4.20594050667205,
4.36093816143897));
#138714=CARTESIAN_POINT('Ctrl Pts',(-6.08417675605191,4.21216499505843,
4.3855208578947));
#138715=CARTESIAN_POINT('Ctrl Pts',(-6.3995577920639,4.30331728230629,3.91097502038183));
#138716=CARTESIAN_POINT('Ctrl Pts',(-6.39744310853195,4.30267205415314,
3.91442691269092));
#138717=CARTESIAN_POINT('Ctrl Pts',(-6.395328425,4.302026826,3.917878805));
#138718=CARTESIAN_POINT('Ctrl Pts',(-6.18318562899999,4.237298226,4.264168959));
#138719=CARTESIAN_POINT('Ctrl Pts',(-5.93489141,4.172121859,4.585527663));
#138720=CARTESIAN_POINT('Ctrl Pts',(-6.30689819352099,4.30331728230629,
3.57569523599079));
#138721=CARTESIAN_POINT('Ctrl Pts',(-6.30496453176049,4.30267205415314,
3.5790973104954));
#138722=CARTESIAN_POINT('Ctrl Pts',(-6.30303087000001,4.302026826,3.582499385));
#138723=CARTESIAN_POINT('Ctrl Pts',(-6.109047985,4.237298226,3.92379187));
#138724=CARTESIAN_POINT('Ctrl Pts',(-5.879347139,4.172121859,4.242142999));
#138725=CARTESIAN_POINT('',(-6.39532842773336,4.30202682545334,3.91787880426053));
#138726=CARTESIAN_POINT('Origin',(0.150186028649116,4.16072874257247,-0.118446067871733));
#138727=CARTESIAN_POINT('',(-6.34917965264429,4.30202682438524,3.75018908629057));
#138728=CARTESIAN_POINT('Origin',(-3.88578058618805E-13,4.392776443,2.26381413614973E-13));
#138729=CARTESIAN_POINT('',(-6.08098564727151,4.3916992373645,4.38994459505378));
#138730=CARTESIAN_POINT('Origin',(0.12677023788604,4.1608246923527,-0.136424485744108));
#138731=CARTESIAN_POINT('Origin',(0.133157392753959,4.55341981119211,-0.12790486823742));
#138732=CARTESIAN_POINT('Ctrl Pts',(-6.980823125,4.172114527,2.741916938));
#138733=CARTESIAN_POINT('Ctrl Pts',(-6.849250662,4.22940039,3.076895755));
#138734=CARTESIAN_POINT('Ctrl Pts',(-6.686208281,4.285714286,3.397737309));
#138735=CARTESIAN_POINT('Ctrl Pts',(-6.662630109,4.29385805,3.444135414));
#138736=CARTESIAN_POINT('Ctrl Pts',(-6.63841029,4.302026826,3.490201831));
#138737=CARTESIAN_POINT('Ctrl Pts',(-6.657574201,4.172114527,2.870401672));
#138738=CARTESIAN_POINT('Ctrl Pts',(-6.51983632400001,4.22940039,3.189869203));
#138739=CARTESIAN_POINT('Ctrl Pts',(-6.352142073,4.285714286,3.494680397));
#138740=CARTESIAN_POINT('Ctrl Pts',(-6.327891176,4.29385805,3.538760292));
#138741=CARTESIAN_POINT('Ctrl Pts',(-6.30303087,4.302026826,3.582499385));
#138742=CARTESIAN_POINT('',(-6.63841029328694,4.30202682641445,3.49020182563221));
#138743=CARTESIAN_POINT('',(-6.46904368484552,4.30202682665757,3.53681209221154));
#138744=CARTESIAN_POINT('',(-6.88468943140282,4.2121649939256,2.97507166832603));
#138745=CARTESIAN_POINT('Ctrl Pts',(-6.63841029324683,4.30202682552111,
3.49020182489699));
#138746=CARTESIAN_POINT('Ctrl Pts',(-6.65456868331828,4.29657697961046,
3.45946835206243));
#138747=CARTESIAN_POINT('Ctrl Pts',(-6.67050177997155,4.29113922035365,
3.42864521292141));
#138748=CARTESIAN_POINT('Ctrl Pts',(-6.68620828108225,4.28571428571329,
3.39773730914955));
#138749=CARTESIAN_POINT('Ctrl Pts',(-6.75650993520172,4.26143250099124,
3.25939480083334));
#138750=CARTESIAN_POINT('Ctrl Pts',(-6.82276032055342,4.23689343090483,
3.11838340739359));
#138751=CARTESIAN_POINT('Ctrl Pts',(-6.88468942882511,4.21216499285689,
2.97507167453552));
#138752=CARTESIAN_POINT('Ctrl Pts',(-6.65568528196482,4.17289950695789,
2.87477885399687));
#138753=CARTESIAN_POINT('Ctrl Pts',(-6.69381093092921,4.17977820193302,
2.89143477508571));
#138754=CARTESIAN_POINT('Ctrl Pts',(-6.73197857598899,4.18648410048819,
2.90813092634623));
#138755=CARTESIAN_POINT('Ctrl Pts',(-6.80829996668031,4.19956141150126,
2.941557168664));
#138756=CARTESIAN_POINT('Ctrl Pts',(-6.84649859056851,4.20594050668918,
2.95830691729174));
#138757=CARTESIAN_POINT('Ctrl Pts',(-6.88468943413949,4.21216499506285,
2.97507166166953));
#138758=CARTESIAN_POINT('Ctrl Pts',(-7.09068370918432,4.30331728230629,
2.44382284214771));
#138759=CARTESIAN_POINT('Ctrl Pts',(-7.08936052059216,4.30267205415314,
2.44764862557385));
#138760=CARTESIAN_POINT('Ctrl Pts',(-7.088037332,4.302026826,2.451474409));
#138761=CARTESIAN_POINT('Ctrl Pts',(-6.955296464,4.237298226,2.835272921));
#138762=CARTESIAN_POINT('Ctrl Pts',(-6.781889847,4.172121859,3.202494356));
#138763=CARTESIAN_POINT('Ctrl Pts',(-6.92811519775424,4.30331728230629,
2.13630078798455));
#138764=CARTESIAN_POINT('Ctrl Pts',(-6.92695808937712,4.30267205415314,
2.14003900399228));
#138765=CARTESIAN_POINT('Ctrl Pts',(-6.925800981,4.302026826,2.14377722));
#138766=CARTESIAN_POINT('Ctrl Pts',(-6.809721103,4.237298226,2.518791062));
#138767=CARTESIAN_POINT('Ctrl Pts',(-6.653826618,4.172121859,2.87907821));
#138768=CARTESIAN_POINT('',(-7.08803733451121,4.30202682545315,2.45147440767622));
#138769=CARTESIAN_POINT('Origin',(0.172137087639891,4.1607288156607,-0.0833912659878833));
#138770=CARTESIAN_POINT('',(-7.00691915965291,4.30202682438465,2.29762580488479));
#138771=CARTESIAN_POINT('Origin',(1.08333481074752E-12,4.39277644300067,
-5.55545193181572E-13));
#138772=CARTESIAN_POINT('',(-6.88252390416385,4.39169923737767,2.98007796857426));
#138773=CARTESIAN_POINT('Origin',(0.153133619751964,4.16082474247324,-0.105983085249925));
#138774=CARTESIAN_POINT('Origin',(0.1575399643161,4.55341983999308,-0.0962896094476801));
#138775=CARTESIAN_POINT('Ctrl Pts',(-7.407046451,4.172114527,1.177141824));
#138776=CARTESIAN_POINT('Ctrl Pts',(-7.35056062300001,4.22940039,1.532573212));
#138777=CARTESIAN_POINT('Ctrl Pts',(-7.260301532,4.285714286,1.880962961));
#138778=CARTESIAN_POINT('Ctrl Pts',(-7.247248825,4.29385805,1.931344914));
#138779=CARTESIAN_POINT('Ctrl Pts',(-7.233498171,4.302026826,1.981540869));
#138780=CARTESIAN_POINT('Ctrl Pts',(-7.118975327,4.172114527,1.372111619));
#138781=CARTESIAN_POINT('Ctrl Pts',(-7.053133761,4.22940039,1.713719749));
#138782=CARTESIAN_POINT('Ctrl Pts',(-6.954885505,4.285714286,2.047453934));
#138783=CARTESIAN_POINT('Ctrl Pts',(-6.940677455,4.29385805,2.095716491));
#138784=CARTESIAN_POINT('Ctrl Pts',(-6.925800981,4.302026826,2.14377722));
#138785=CARTESIAN_POINT('',(-7.23349817293618,4.30202682620654,1.98154086307485));
#138786=CARTESIAN_POINT('',(-7.07964957713462,4.30202682665757,2.06265904060565));
#138787=CARTESIAN_POINT('',(-7.36328168429495,4.21216499534027,1.4255114278799));
#138788=CARTESIAN_POINT('Ctrl Pts',(-7.23349817258395,4.3020268248974,1.98154086236812));
#138789=CARTESIAN_POINT('Ctrl Pts',(-7.24267199974551,4.29657697940857,
1.94805234476445));
#138790=CARTESIAN_POINT('Ctrl Pts',(-7.25160652540155,4.29113922035358,
1.91452468863712));
#138791=CARTESIAN_POINT('Ctrl Pts',(-7.26030153158397,4.28571428595545,
1.88096296099009));
#138792=CARTESIAN_POINT('Ctrl Pts',(-7.29922002221488,4.2614325007481,1.73074204502813));
#138793=CARTESIAN_POINT('Ctrl Pts',(-7.33360822920324,4.23689343229803,
1.57878554621227));
#138794=CARTESIAN_POINT('Ctrl Pts',(-7.36328168273712,4.21216499704637,
1.42551143409564));
#138795=CARTESIAN_POINT('Ctrl Pts',(-7.11807153505751,4.1728995071105,1.37679252714695));
#138796=CARTESIAN_POINT('Ctrl Pts',(-7.15888635834678,4.17977820204914,
1.38486315444477));
#138797=CARTESIAN_POINT('Ctrl Pts',(-7.19975084304136,4.18648410041248,
1.39296404330249));
#138798=CARTESIAN_POINT('Ctrl Pts',(-7.28147353617586,4.19956141143594,
1.40920195580249));
#138799=CARTESIAN_POINT('Ctrl Pts',(-7.32237979828495,4.2059405066357,1.4173485297049));
#138800=CARTESIAN_POINT('Ctrl Pts',(-7.36328168565133,4.2121649950354,1.42551142131593));
#138801=CARTESIAN_POINT('Ctrl Pts',(-7.45025713667788,4.30331728230629,
0.862400223638416));
#138802=CARTESIAN_POINT('Ctrl Pts',(-7.44978731383894,4.30267205415314,
0.866421008819208));
#138803=CARTESIAN_POINT('Ctrl Pts',(-7.449317491,4.302026826,0.870441794));
#138804=CARTESIAN_POINT('Ctrl Pts',(-7.40218536500001,4.237298226,1.273802674));
#138805=CARTESIAN_POINT('Ctrl Pts',(-7.311774653,4.172121859,1.669715971));
#138806=CARTESIAN_POINT('Ctrl Pts',(-7.22538123576582,4.30331728230629,
0.597015288620854));
#138807=CARTESIAN_POINT('Ctrl Pts',(-7.22505478588291,4.30267205415314,
0.600914851310427));
#138808=CARTESIAN_POINT('Ctrl Pts',(-7.224728336,4.302026826,0.604814414));
#138809=CARTESIAN_POINT('Ctrl Pts',(-7.191979232,4.237298226,0.996014383));
#138810=CARTESIAN_POINT('Ctrl Pts',(-7.117180559,4.172121859,1.381390924));
#138811=CARTESIAN_POINT('',(-7.4493174931666,4.30202682545335,0.870441792165976));
#138812=CARTESIAN_POINT('Origin',(0.186039531007829,4.16072872556647,-0.0444372955112665));
#138813=CARTESIAN_POINT('',(-7.33702291451184,4.30202682438524,0.737628093935509));
#138814=CARTESIAN_POINT('Origin',(-1.12583553590895E-12,4.39277644300022,
2.0046898169257E-13));
#138815=CARTESIAN_POINT('',(-7.36224299305595,4.39169923741706,1.43086620813188));
#138816=CARTESIAN_POINT('Origin',(0.17233670797613,4.16082467495845,-0.0705860755585144));
#138817=CARTESIAN_POINT('Origin',(0.174556151942689,4.55341981959481,-0.0601719639733485));
#138818=CARTESIAN_POINT('Ctrl Pts',(-7.486924517,4.172114527,-0.442675134));
#138819=CARTESIAN_POINT('Ctrl Pts',(-7.50816653800001,4.22940039,-0.0834107510000001));
#138820=CARTESIAN_POINT('Ctrl Pts',(-7.494911153,4.285714286,0.276236876));
#138821=CARTESIAN_POINT('Ctrl Pts',(-7.492994242,4.29385805,0.328246873));
#138822=CARTESIAN_POINT('Ctrl Pts',(-7.490355716,4.302026826,0.380225258));
#138823=CARTESIAN_POINT('Ctrl Pts',(-7.247501079,4.172114527,-0.190336848));
#138824=CARTESIAN_POINT('Ctrl Pts',(-7.256634502,4.22940039,0.157438664));
#138825=CARTESIAN_POINT('Ctrl Pts',(-7.23242622,4.285714286,0.5044908));
#138826=CARTESIAN_POINT('Ctrl Pts',(-7.22892537,4.29385805,0.554679316));
#138827=CARTESIAN_POINT('Ctrl Pts',(-7.224728336,4.302026826,0.604814414));
#138828=CARTESIAN_POINT('',(-7.49035571664362,4.30202682620655,0.380225251774799));
#138829=CARTESIAN_POINT('',(-7.35754202627092,4.30202682665757,0.492519831952797));
#138830=CARTESIAN_POINT('',(-7.49757506976613,4.21216499536516,-0.190704142493896));
#138831=CARTESIAN_POINT('Ctrl Pts',(-7.49035571612153,4.3020268248974,0.380225251182439));
#138832=CARTESIAN_POINT('Ctrl Pts',(-7.4921160237264,4.29657697940857,0.345547575253956));
#138833=CARTESIAN_POINT('Ctrl Pts',(-7.49363421042152,4.29113922035358,
0.310883118420912));
#138834=CARTESIAN_POINT('Ctrl Pts',(-7.49491115271027,4.28571428596,0.276236876004686));
#138835=CARTESIAN_POINT('Ctrl Pts',(-7.50062669436462,4.26143250076421,
0.121161716035054));
#138836=CARTESIAN_POINT('Ctrl Pts',(-7.50154476801792,4.23689343230145,
-0.0346345719932585));
#138837=CARTESIAN_POINT('Ctrl Pts',(-7.49757506958192,4.21216499708899,
-0.190704136023857));
#138838=CARTESIAN_POINT('Ctrl Pts',(-7.24762467296213,4.17289950691553,
-0.185571088361909));
#138839=CARTESIAN_POINT('Ctrl Pts',(-7.28922021464216,4.17977820189018,
-0.186463128323594));
#138840=CARTESIAN_POINT('Ctrl Pts',(-7.33087076318371,4.18648410045675,
-0.187336290073957));
#138841=CARTESIAN_POINT('Ctrl Pts',(-7.41417349632566,4.19956141148362,
-0.189045974414105));
#138842=CARTESIAN_POINT('Ctrl Pts',(-7.45587466532089,4.20594050667357,
-0.189883500166995));
#138843=CARTESIAN_POINT('Ctrl Pts',(-7.49757506967887,4.21216499505722,
-0.190704149263988));
#138844=CARTESIAN_POINT('Ctrl Pts',(-7.46146482034059,4.30331728230629,
-0.759347270947339));
#138845=CARTESIAN_POINT('Ctrl Pts',(-7.46187033167029,4.30267205415314,
-0.75531949147367));
#138846=CARTESIAN_POINT('Ctrl Pts',(-7.462275843,4.302026826,-0.751291712));
#138847=CARTESIAN_POINT('Ctrl Pts',(-7.502956307,4.237298226,-0.347229172));
#138848=CARTESIAN_POINT('Ctrl Pts',(-7.499769002,4.172121859,0.058863524));
#138849=CARTESIAN_POINT('Ctrl Pts',(-7.18479647692406,4.30331728230629,
-0.970185982323433));
#138850=CARTESIAN_POINT('Ctrl Pts',(-7.18531594996203,4.30267205415314,
-0.966307412161716));
#138851=CARTESIAN_POINT('Ctrl Pts',(-7.185835423,4.302026826,-0.962428841999999));
#138852=CARTESIAN_POINT('Ctrl Pts',(-7.23794840400001,4.237298226,-0.573334821));
#138853=CARTESIAN_POINT('Ctrl Pts',(-7.247743048,4.172121859,-0.180888666));
#138854=CARTESIAN_POINT('',(-7.46227584451965,4.30202682545371,-0.751291714841994));
#138855=CARTESIAN_POINT('Origin',(0.19124235071154,4.16072878392355,-0.00340538346760563));
#138856=CARTESIAN_POINT('',(-7.32405563182418,4.30202682438465,-0.856860287050402));
#138857=CARTESIAN_POINT('Origin',(-9.41954847455406E-13,4.39277644300022,
-5.42372136785874E-14));
#138858=CARTESIAN_POINT('',(-7.49771178195657,4.39169923736653,-0.185251266036152));
#138859=CARTESIAN_POINT('Origin',(0.183481501523408,4.16082467772807,-0.0318885222126206));
#138860=CARTESIAN_POINT('Origin',(0.183410145336235,4.5534198137753,-0.0212407675007344));
#138861=CARTESIAN_POINT('Ctrl Pts',(-7.216722314,4.172114527,-2.041793095));
#138862=CARTESIAN_POINT('Ctrl Pts',(-7.314698931,4.22940039,-1.69549452));
#138863=CARTESIAN_POINT('Ctrl Pts',(-7.379067058,4.285714286,-1.341405739));
#138864=CARTESIAN_POINT('Ctrl Pts',(-7.388375575,4.29385805,-1.290199627));
#138865=CARTESIAN_POINT('Ctrl Pts',(-7.39697255300001,4.302026826,-1.238869262));
#138866=CARTESIAN_POINT('Ctrl Pts',(-7.037141735,4.172114527,-1.743885375));
#138867=CARTESIAN_POINT('Ctrl Pts',(-7.120823079,4.22940039,-1.406204078));
#138868=CARTESIAN_POINT('Ctrl Pts',(-7.171786724,4.285714286,-1.062061763));
#138869=CARTESIAN_POINT('Ctrl Pts',(-7.179156768,4.29385805,-1.012294047));
#138870=CARTESIAN_POINT('Ctrl Pts',(-7.185835423,4.302026826,-0.962428842));
#138871=CARTESIAN_POINT('',(-7.39697255240167,4.30202682641445,-1.2388692682728));
#138872=CARTESIAN_POINT('',(-7.29140398739456,4.30202682665757,-1.10064905601082));
#138873=CARTESIAN_POINT('',(-7.2812901778864,4.21216499391656,-1.79800259874241));
#138874=CARTESIAN_POINT('Ctrl Pts',(-7.39697255197888,4.30202682552111,
-1.23886926883788));
#138875=CARTESIAN_POINT('Ctrl Pts',(-7.39123702897011,4.29657697961046,
-1.27311461443996));
#138876=CARTESIAN_POINT('Ctrl Pts',(-7.38526788766412,4.29113922035365,
-1.30729500118857));
#138877=CARTESIAN_POINT('Ctrl Pts',(-7.37906705786746,4.28571428571329,
-1.3414057385799));
#138878=CARTESIAN_POINT('Ctrl Pts',(-7.35131239827258,4.26143250098364,
-1.49408399872788));
#138879=CARTESIAN_POINT('Ctrl Pts',(-7.31871741129183,4.23689343089718,
-1.64643521610912));
#138880=CARTESIAN_POINT('Ctrl Pts',(-7.28129017951097,4.21216499285689,
-1.79800259225534));
#138881=CARTESIAN_POINT('Ctrl Pts',(-7.03828693800445,4.17289950705686,
-1.73925760595926));
#138882=CARTESIAN_POINT('Ctrl Pts',(-7.07871823679367,4.1797782020216,-1.74907060253793));
#138883=CARTESIAN_POINT('Ctrl Pts',(-7.11920731380291,4.18648410043831,
-1.75887698685823));
#138884=CARTESIAN_POINT('Ctrl Pts',(-7.20019494374002,4.19956141146568,
-1.77845432503505));
#138885=CARTESIAN_POINT('Ctrl Pts',(-7.24074111926083,4.20594050665211,
-1.78823678857437));
#138886=CARTESIAN_POINT('Ctrl Pts',(-7.2812901760473,4.21216499504079,-1.79800260566205));
#138887=CARTESIAN_POINT('Ctrl Pts',(-7.12378270255569,4.30331728230629,
-2.34558853055555));
#138888=CARTESIAN_POINT('Ctrl Pts',(-7.12504458677785,4.30267205415314,
-2.34174209127778));
#138889=CARTESIAN_POINT('Ctrl Pts',(-7.126306471,4.302026826,-2.337895652));
#138890=CARTESIAN_POINT('Ctrl Pts',(-7.25289735,4.237298226,-1.952024967));
#138891=CARTESIAN_POINT('Ctrl Pts',(-7.337082488,4.172121859,-1.554741317));
#138892=CARTESIAN_POINT('Ctrl Pts',(-6.80825862002472,4.30331728230629,
-2.4920224339872));
#138893=CARTESIAN_POINT('Ctrl Pts',(-6.80959972601237,4.30267205415314,
-2.4883462139936));
#138894=CARTESIAN_POINT('Ctrl Pts',(-6.81094083199999,4.302026826,-2.484669994));
#138895=CARTESIAN_POINT('Ctrl Pts',(-6.945479154,4.237298226,-2.115875526));
#138896=CARTESIAN_POINT('Ctrl Pts',(-7.039409127,4.172121859,-1.734710103));
#138897=CARTESIAN_POINT('',(-7.12630647186188,4.30202682545374,-2.33789565511669));
#138898=CARTESIAN_POINT('Origin',(0.187503352522165,4.16072876702414,0.0377857023399969));
#138899=CARTESIAN_POINT('',(-6.96862364819113,4.30202682438465,-2.41128283256266));
#138900=CARTESIAN_POINT('Origin',(-7.1730815731641E-13,4.39277644300044,
-1.89843800402212E-13));
#138901=CARTESIAN_POINT('',(-7.28259590084164,4.39169923740603,-1.79270659643726));
#138902=CARTESIAN_POINT('Origin',(0.186046560586159,4.16082471231166,0.00830004912923704));
#138903=CARTESIAN_POINT('Origin',(0.18368817995575,4.55341980852378,0.0186835631696336));
#138904=CARTESIAN_POINT('Ctrl Pts',(-6.609074196,4.172114527,-3.54543908));
#138905=CARTESIAN_POINT('Ctrl Pts',(-6.779204132,4.22940039,-3.22829885));
#138906=CARTESIAN_POINT('Ctrl Pts',(-6.918185988,4.285714286,-2.896325712));
#138907=CARTESIAN_POINT('Ctrl Pts',(-6.938284678,4.29385805,-2.848317827));
#138908=CARTESIAN_POINT('Ctrl Pts',(-6.957715175,4.302026826,-2.800035633));
#138909=CARTESIAN_POINT('Ctrl Pts',(-6.497733465,4.172114527,-3.215891761));
#138910=CARTESIAN_POINT('Ctrl Pts',(-6.652049883,4.22940039,-2.90409428));
#138911=CARTESIAN_POINT('Ctrl Pts',(-6.775802451,4.285714286,-2.578953498));
#138912=CARTESIAN_POINT('Ctrl Pts',(-6.793698776,4.29385805,-2.531933665));
#138913=CARTESIAN_POINT('Ctrl Pts',(-6.81094083200001,4.302026826,-2.484669994));
#138914=CARTESIAN_POINT('',(-6.95771517296804,4.30202682641445,-2.80003563894042));
#138915=CARTESIAN_POINT('',(-6.88432800204651,4.30202682665757,-2.6423528172869));
#138916=CARTESIAN_POINT('',(-6.72454024984592,4.21216499393534,-3.32122845186731));
#138917=CARTESIAN_POINT('Ctrl Pts',(-6.95771517226492,4.30202682552111,
-2.80003563935076));
#138918=CARTESIAN_POINT('Ctrl Pts',(-6.94475200541274,4.29657697961046,
-2.83224738030877));
#138919=CARTESIAN_POINT('Ctrl Pts',(-6.93157464648108,4.29113922035365,
-2.86434545977854));
#138920=CARTESIAN_POINT('Ctrl Pts',(-6.91818598841666,4.28571428571329,
-2.89632571194525));
#138921=CARTESIAN_POINT('Ctrl Pts',(-6.85825890466453,4.26143250101328,
-3.0394680075202));
#138922=CARTESIAN_POINT('Ctrl Pts',(-6.79367496218216,4.23689343092699,
-3.18125037923024));
#138923=CARTESIAN_POINT('Ctrl Pts',(-6.72454025279714,4.21216499285671,
-3.32122844569756));
#138924=CARTESIAN_POINT('Ctrl Pts',(-6.49984672779771,4.1728995071943,-3.21161837090972));
#138925=CARTESIAN_POINT('Ctrl Pts',(-6.53722326117339,4.17977820215861,
-3.22989347930327));
#138926=CARTESIAN_POINT('Ctrl Pts',(-6.57465764293399,4.18648410049424,
-3.24817455038812));
#138927=CARTESIAN_POINT('Ctrl Pts',(-6.64954327818949,4.19956141151884,
-3.28470412787107));
#138928=CARTESIAN_POINT('Ctrl Pts',(-6.68703856609739,4.20594050668611,
-3.30297411204387));
#138929=CARTESIAN_POINT('Ctrl Pts',(-6.72454024648908,4.21216499507469,
-3.3212284583751));
#138930=CARTESIAN_POINT('Ctrl Pts',(-6.45300042338213,4.30331728230629,
-3.82215267771983));
#138931=CARTESIAN_POINT('Ctrl Pts',(-6.45505967619106,4.30267205415314,
-3.81866743385991));
#138932=CARTESIAN_POINT('Ctrl Pts',(-6.457118929,4.302026826,-3.81518219));
#138933=CARTESIAN_POINT('Ctrl Pts',(-6.663700974,4.237298226,-3.465546244));
#138934=CARTESIAN_POINT('Ctrl Pts',(-6.83132215200001,4.172121859,-3.095648181));
#138935=CARTESIAN_POINT('Ctrl Pts',(-6.11337415738809,4.30331728230629,
-3.89733468775749));
#138936=CARTESIAN_POINT('Ctrl Pts',(-6.11547418769404,4.30267205415314,
-3.89403271387874));
#138937=CARTESIAN_POINT('Ctrl Pts',(-6.117574218,4.302026826,-3.89073074));
#138938=CARTESIAN_POINT('Ctrl Pts',(-6.328247018,4.237298226,-3.559480243));
#138939=CARTESIAN_POINT('Ctrl Pts',(-6.501920259,4.172121859,-3.207418423));
#138940=CARTESIAN_POINT('',(-6.45711892914839,4.30202682545394,-3.81518219324713));
#138941=CARTESIAN_POINT('Origin',(0.174996990872773,4.16072877815487,0.0772100619350202));
#138942=CARTESIAN_POINT('',(-6.28734656821467,4.30202682438522,-3.85295647362473));
#138943=CARTESIAN_POINT('Origin',(-5.98479599211998E-14,4.39277644300111,
9.97465998686664E-15));
#138944=CARTESIAN_POINT('',(-6.72695392951752,4.3916992373877,-3.31633695910688));
#138945=CARTESIAN_POINT('Origin',(0.179912927710379,4.16082471999665,0.0481006479497342));
#138946=CARTESIAN_POINT('Origin',(0.175377460269127,4.55341978905206,0.0577343964042454));
#138947=CARTESIAN_POINT('Ctrl Pts',(-5.692393115,4.172114527,-4.883304274));
#138948=CARTESIAN_POINT('Ctrl Pts',(-5.926721282,4.22940039,-4.610151513));
#138949=CARTESIAN_POINT('Ctrl Pts',(-6.133818231,4.285714286,-4.315816714));
#138950=CARTESIAN_POINT('Ctrl Pts',(-6.163767301,4.29385805,-4.27325185));
#138951=CARTESIAN_POINT('Ctrl Pts',(-6.193122768,4.302026826,-4.23027545));
#138952=CARTESIAN_POINT('Ctrl Pts',(-5.6544984,4.172114527,-4.537526622));
#138953=CARTESIAN_POINT('Ctrl Pts',(-5.87223422700001,4.22940039,-4.266192261));
#138954=CARTESIAN_POINT('Ctrl Pts',(-6.062989186,4.285714286,-3.975256234));
#138955=CARTESIAN_POINT('Ctrl Pts',(-6.090574979,4.29385805,-3.93318288));
#138956=CARTESIAN_POINT('Ctrl Pts',(-6.117574218,4.302026826,-3.89073074));
#138957=CARTESIAN_POINT('',(-6.19312276474054,4.30202682641444,-4.2302754553667));
#138958=CARTESIAN_POINT('',(-6.15534849076645,4.30202682665756,-4.06050309838586));
#138959=CARTESIAN_POINT('',(-5.85335829350893,4.21216499391699,-4.6891573537254));
#138960=CARTESIAN_POINT('Ctrl Pts',(-6.1931227639692,4.30202682552109,-4.23027545561829));
#138961=CARTESIAN_POINT('Ctrl Pts',(-6.17353809687833,4.29657697961046,
-4.25894740591034));
#138962=CARTESIAN_POINT('Ctrl Pts',(-6.15376867898852,4.29113922035365,
-4.28746230749566));
#138963=CARTESIAN_POINT('Ctrl Pts',(-6.13381823140102,4.28571428571329,
-4.3158167134544));
#138964=CARTESIAN_POINT('Ctrl Pts',(-6.04452084714403,4.26143250100524,
-4.44272987032328));
#138965=CARTESIAN_POINT('Ctrl Pts',(-5.95096782255411,4.23689343091894,
-4.56731381033318));
#138966=CARTESIAN_POINT('Ctrl Pts',(-5.85335829768833,4.21216499285688,
-4.68915734848842));
#138967=CARTESIAN_POINT('Ctrl Pts',(-5.65748090767041,4.17289950703237,
-4.53380742990244));
#138968=CARTESIAN_POINT('Ctrl Pts',(-5.69005499041686,4.17977820200376,
-4.55969012622329));
#138969=CARTESIAN_POINT('Ctrl Pts',(-5.72268428790545,4.18648410046869,
-4.58559108199846));
#138970=CARTESIAN_POINT('Ctrl Pts',(-5.78796635935612,4.19956141148752,
-4.63736481611499));
#138971=CARTESIAN_POINT('Ctrl Pts',(-5.82065752182051,4.20594050665946,
-4.66326803672648));
#138972=CARTESIAN_POINT('Ctrl Pts',(-5.85335828892578,4.2121649950401,-4.68915735924435));
#138973=CARTESIAN_POINT('Ctrl Pts',(-5.4804830149175,4.30331728230629,-5.1199972136303));
#138974=CARTESIAN_POINT('Ctrl Pts',(-5.48324334795874,4.30267205415314,
-5.11703613131514));
#138975=CARTESIAN_POINT('Ctrl Pts',(-5.486003681,4.302026826,-5.114075049));
#138976=CARTESIAN_POINT('Ctrl Pts',(-5.762917347,4.237298226,-4.81702243));
#138977=CARTESIAN_POINT('Ctrl Pts',(-6.006136784,4.172121859,-4.491805977));
#138978=CARTESIAN_POINT('Ctrl Pts',(-5.13263511291799,4.30331728230629,
-5.12041190225208));
#138979=CARTESIAN_POINT('Ctrl Pts',(-5.135395872459,4.30267205415314,-5.11763857112605));
#138980=CARTESIAN_POINT('Ctrl Pts',(-5.138156632,4.302026826,-5.11486524));
#138981=CARTESIAN_POINT('Ctrl Pts',(-5.415113084,4.237298226,-4.83664762));
#138982=CARTESIAN_POINT('Ctrl Pts',(-5.660408826,4.172121859,-4.530151423));
#138983=CARTESIAN_POINT('',(-5.48600368048579,4.30202682545371,-5.11407505218425));
#138984=CARTESIAN_POINT('Origin',(0.154307684794188,4.16072873661738,0.113024035958856));
#138985=CARTESIAN_POINT('',(-5.31208014948166,4.30202682438463,-5.11447015178951));
#138986=CARTESIAN_POINT('Origin',(-3.62557206479153E-13,4.39277644300067,
-2.0643209364124E-13));
#138987=CARTESIAN_POINT('',(-5.85676706859328,4.39169923740595,-4.68489909144703));
#138988=CARTESIAN_POINT('Origin',(0.165366468826336,4.16082471323804,0.0856520620843465));
#138989=CARTESIAN_POINT('Origin',(0.158866106015709,4.55341982996691,0.0940856226204201));
#138990=CARTESIAN_POINT('Ctrl Pts',(-4.509542057,4.172114527,-5.992831587));
#138991=CARTESIAN_POINT('Ctrl Pts',(-4.79711153099999,4.22940039,-5.776438615));
#138992=CARTESIAN_POINT('Ctrl Pts',(-5.062639951,4.285714286,-5.533504923));
#138993=CARTESIAN_POINT('Ctrl Pts',(-5.101039015,4.29385805,-5.498373367));
#138994=CARTESIAN_POINT('Ctrl Pts',(-5.138946823,4.302026826,-5.462712289));
#138995=CARTESIAN_POINT('Ctrl Pts',(-4.546865274,4.172114527,-5.646991781));
#138996=CARTESIAN_POINT('Ctrl Pts',(-4.817839426,4.22940039,-5.428807833));
#138997=CARTESIAN_POINT('Ctrl Pts',(-5.066677286,4.285714286,-5.185680407));
#138998=CARTESIAN_POINT('Ctrl Pts',(-5.102662666,4.29385805,-5.150520834));
#138999=CARTESIAN_POINT('Ctrl Pts',(-5.138156632,4.302026826,-5.11486524));
#139000=CARTESIAN_POINT('',(-5.13894681866893,4.30202682641444,-5.4627122935483));
#139001=CARTESIAN_POINT('',(-5.1385517245908,4.30202682665756,-5.28878876732656));
#139002=CARTESIAN_POINT('',(-4.70847980829036,4.21216499392856,-5.83782647009015));
#139003=CARTESIAN_POINT('Ctrl Pts',(-5.13894681787326,4.30202682552109,
-5.46271229363858));
#139004=CARTESIAN_POINT('Ctrl Pts',(-5.11365640767574,4.29657697961046,
-5.48650378512141));
#139005=CARTESIAN_POINT('Ctrl Pts',(-5.08821932709154,4.29113922035365,
-5.51010218345383));
#139006=CARTESIAN_POINT('Ctrl Pts',(-5.06263995080817,4.28571428571329,
-5.53350492260383));
#139007=CARTESIAN_POINT('Ctrl Pts',(-4.94814771273062,4.26143250098491,
-5.63825462223473));
#139008=CARTESIAN_POINT('Ctrl Pts',(-4.83000004119946,4.23689343089845,
-5.73981472429379));
#139009=CARTESIAN_POINT('Ctrl Pts',(-4.70847981356072,4.21216499285688,
-5.83782646584249));
#139010=CARTESIAN_POINT('Ctrl Pts',(-4.55057756815832,4.17289950692595,
-5.64400069300954));
#139011=CARTESIAN_POINT('Ctrl Pts',(-4.57682607217492,4.1797782018608,-5.67628073086688));
#139012=CARTESIAN_POINT('Ctrl Pts',(-4.60312457549802,4.1864841004784,-5.70859047178126));
#139013=CARTESIAN_POINT('Ctrl Pts',(-4.65575056577685,4.1995614114796,-5.77318748021941));
#139014=CARTESIAN_POINT('Ctrl Pts',(-4.68210900029073,4.20594050666992,
-5.80551273159959));
#139015=CARTESIAN_POINT('Ctrl Pts',(-4.7084798025698,4.21216499506463,-5.83782647453979));
#139016=CARTESIAN_POINT('Ctrl Pts',(-4.2517043126979,4.30331728230629,-6.178436370691));
#139017=CARTESIAN_POINT('Ctrl Pts',(-4.25503665584895,4.30267205415314,
-6.1761379068455));
#139018=CARTESIAN_POINT('Ctrl Pts',(-4.258368999,4.302026826,-6.173839443));
#139019=CARTESIAN_POINT('Ctrl Pts',(-4.592666109,4.237298226,-5.943260002));
#139020=CARTESIAN_POINT('Ctrl Pts',(-4.900111135,4.172121859,-5.677931918));
#139021=CARTESIAN_POINT('Ctrl Pts',(-3.91189975656577,4.30331728230629,
-6.10406434697834));
#139022=CARTESIAN_POINT('Ctrl Pts',(-3.91519215528289,4.30267205415314,
-6.10194933648917));
#139023=CARTESIAN_POINT('Ctrl Pts',(-3.918484554,4.302026826,-6.099834326));
#139024=CARTESIAN_POINT('Ctrl Pts',(-4.248774481,4.237298226,-5.88765873000001));
#139025=CARTESIAN_POINT('Ctrl Pts',(-4.554222968,4.172121859,-5.64105957800001));
#139026=CARTESIAN_POINT('',(-4.25836899838928,4.30202682545315,-6.17383944577572));
#139027=CARTESIAN_POINT('Origin',(0.126403232601331,4.16072876476957,0.143553190585521));
#139028=CARTESIAN_POINT('',(-4.08842676807871,4.30202682438463,-6.13683689011035));
#139029=CARTESIAN_POINT('Origin',(-1.50053580671994E-13,4.39277644300067,
-3.65592972562112E-13));
#139030=CARTESIAN_POINT('',(-4.71272428942334,4.39169923736879,-5.83440054895474));
#139031=CARTESIAN_POINT('Origin',(0.143087622696539,4.16082468452531,0.11919844841964));
#139032=CARTESIAN_POINT('Origin',(0.134926334767914,4.55341983712944,0.126037539353255));
#139033=CARTESIAN_POINT('Ctrl Pts',(-3.115829826,4.172114527,-6.822140756));
#139034=CARTESIAN_POINT('Ctrl Pts',(-3.443194178,4.22940039,-6.672625868));
#139035=CARTESIAN_POINT('Ctrl Pts',(-3.754738253,4.285714286,-6.492452591));
#139036=CARTESIAN_POINT('Ctrl Pts',(-3.799791815,4.29385805,-6.466397055));
#139037=CARTESIAN_POINT('Ctrl Pts',(-3.844479437,4.302026826,-6.439718772));
#139038=CARTESIAN_POINT('Ctrl Pts',(-3.226625782,4.172114527,-6.492409881));
#139039=CARTESIAN_POINT('Ctrl Pts',(-3.538167808,4.22940039,-6.337578385));
#139040=CARTESIAN_POINT('Ctrl Pts',(-3.833453187,4.285714286,-6.153627927));
#139041=CARTESIAN_POINT('Ctrl Pts',(-3.876155517,4.29385805,-6.127026159));
#139042=CARTESIAN_POINT('Ctrl Pts',(-3.918484554,4.302026826,-6.099834326));
#139043=CARTESIAN_POINT('',(-3.84447943177234,4.30202682641444,-6.4397187754636));
#139044=CARTESIAN_POINT('',(-3.88148199205119,4.30202682665756,-6.26977655113509));
#139045=CARTESIAN_POINT('',(-3.34343804111563,4.21216499391003,-6.71352530840784));
#139046=CARTESIAN_POINT('Ctrl Pts',(-3.84447943092908,4.30202682552109,
-6.43971877531644));
#139047=CARTESIAN_POINT('Ctrl Pts',(-3.81466582933418,4.29657697961046,
-6.45751734418141));
#139048=CARTESIAN_POINT('Ctrl Pts',(-3.78475049544117,4.29113922035365,
-6.47509580469299));
#139049=CARTESIAN_POINT('Ctrl Pts',(-3.7547382535708,4.28571428571329,-6.49245259106079));
#139050=CARTESIAN_POINT('Ctrl Pts',(-3.62040469104493,4.26143250097169,
-6.57014085429876));
#139051=CARTESIAN_POINT('Ctrl Pts',(-3.48318682656126,4.23689343088507,
-6.64392828065515));
#139052=CARTESIAN_POINT('Ctrl Pts',(-3.34343804705431,4.2121649928567,-6.71352530534514));
#139053=CARTESIAN_POINT('Ctrl Pts',(-3.23089428070165,4.17289950706335,
-6.49028675709695));
#139054=CARTESIAN_POINT('Ctrl Pts',(-3.24958985533249,4.17977820200827,
-6.52745475823694));
#139055=CARTESIAN_POINT('Ctrl Pts',(-3.26832787454873,4.18648410044612,
-6.56466251525528));
#139056=CARTESIAN_POINT('Ctrl Pts',(-3.3058370511616,4.19956141145617,-6.63906231389585));
#139057=CARTESIAN_POINT('Ctrl Pts',(-3.32463026659627,4.20594050662904,
-6.67629810299704));
#139058=CARTESIAN_POINT('Ctrl Pts',(-3.34343803465716,4.21216499502219,
-6.71352531148481));
#139059=CARTESIAN_POINT('Ctrl Pts',(-2.82412064279616,4.30331728230629,
-6.94797870952977));
#139060=CARTESIAN_POINT('Ctrl Pts',(-2.82786917939808,4.30267205415314,
-6.94645033776488));
#139061=CARTESIAN_POINT('Ctrl Pts',(-2.831617716,4.302026826,-6.94492196600001));
#139062=CARTESIAN_POINT('Ctrl Pts',(-3.207666909,4.237298226,-6.791597341));
#139063=CARTESIAN_POINT('Ctrl Pts',(-3.564961736,4.172121859,-6.598564073));
#139064=CARTESIAN_POINT('Ctrl Pts',(-2.5082483139853,4.30331728230629,-6.80229752762605));
#139065=CARTESIAN_POINT('Ctrl Pts',(-2.51191840299265,4.30267205415314,
-6.80093973331303));
#139066=CARTESIAN_POINT('Ctrl Pts',(-2.515588492,4.302026826,-6.799581939));
#139067=CARTESIAN_POINT('Ctrl Pts',(-2.883767906,4.237298226,-6.663369462));
#139068=CARTESIAN_POINT('Ctrl Pts',(-3.235086705,4.172121859,-6.488198056));
#139069=CARTESIAN_POINT('',(-2.83161771479313,4.30202682545336,-6.9449219685791));
#139070=CARTESIAN_POINT('Origin',(0.0925883270804578,4.1607287623299,0.167370006069153));
#139071=CARTESIAN_POINT('',(-2.67360309457301,4.30202682438522,-6.87225195616751));
#139072=CARTESIAN_POINT('Origin',(2.81892564846231E-13,4.39277644300022,
5.06539254985228E-13));
#139073=CARTESIAN_POINT('',(-3.3483197599588,4.39169923740935,-6.71109192160016));
#139074=CARTESIAN_POINT('Origin',(0.114118211480692,4.16082470782816,0.147171347731774));
#139075=CARTESIAN_POINT('Origin',(0.104677531084114,4.5534198439215,0.152096115214863));
#139076=CARTESIAN_POINT('Ctrl Pts',(-1.576424854,4.172114527,-7.332454206));
#139077=CARTESIAN_POINT('Ctrl Pts',(-1.928276891,4.22940039,-7.256808551));
#139078=CARTESIAN_POINT('Ctrl Pts',(-2.271269168,4.285714286,-7.147820393));
#139079=CARTESIAN_POINT('Ctrl Pts',(-2.320870572,4.29385805,-7.132059205));
#139080=CARTESIAN_POINT('Ctrl Pts',(-2.370248465,4.302026826,-7.115611162));
#139081=CARTESIAN_POINT('Ctrl Pts',(-1.755512854,4.172114527,-7.034250111));
#139082=CARTESIAN_POINT('Ctrl Pts',(-2.093055395,4.22940039,-6.950010816));
#139083=CARTESIAN_POINT('Ctrl Pts',(-2.420981077,4.285714286,-6.833838645));
#139084=CARTESIAN_POINT('Ctrl Pts',(-2.468403645,4.29385805,-6.81703855));
#139085=CARTESIAN_POINT('Ctrl Pts',(-2.515588492,4.302026826,-6.799581939));
#139086=CARTESIAN_POINT('',(-2.37024845919458,4.30202682641444,-7.11561116450187));
#139087=CARTESIAN_POINT('',(-2.44291847467284,4.30202682665756,-6.95759655184378));
#139088=CARTESIAN_POINT('',(-1.82206082675909,4.21216499392044,-7.27530716467459));
#139089=CARTESIAN_POINT('Ctrl Pts',(-2.37024845855516,4.30202682552109,
-7.11561116452528));
#139090=CARTESIAN_POINT('Ctrl Pts',(-2.33730571565344,4.29657697961046,
-7.12658456986995));
#139091=CARTESIAN_POINT('Ctrl Pts',(-2.30431093621402,4.29113922035365,
-7.1373211432536));
#139092=CARTESIAN_POINT('Ctrl Pts',(-2.27126916793844,4.28571428571329,
-7.14782039273317));
#139093=CARTESIAN_POINT('Ctrl Pts',(-2.12337556972221,4.26143250099285,
-7.19481460233943));
#139094=CARTESIAN_POINT('Ctrl Pts',(-1.97350366708589,4.23689343090646,
-7.2373791349662));
#139095=CARTESIAN_POINT('Ctrl Pts',(-1.82206083326747,4.21216499285688,
-7.27530716326621));
#139096=CARTESIAN_POINT('Ctrl Pts',(-1.76013796653428,4.172899507013,-7.03309422503798));
#139097=CARTESIAN_POINT('Ctrl Pts',(-1.77040642745592,4.1797782019747,-7.07341225479918));
#139098=CARTESIAN_POINT('Ctrl Pts',(-1.78070779428442,4.18648410042518,
-7.11377823530059));
#139099=CARTESIAN_POINT('Ctrl Pts',(-1.80134626972003,4.1995614114513,-7.19450197207154));
#139100=CARTESIAN_POINT('Ctrl Pts',(-1.81169551631347,4.20594050666897,
-7.23490719511896));
#139101=CARTESIAN_POINT('Ctrl Pts',(-1.82206081981772,4.21216499505768,
-7.2753071662803));
#139102=CARTESIAN_POINT('Ctrl Pts',(-1.26448422969873,4.30331728230629,
-7.39264128645948));
#139103=CARTESIAN_POINT('Ctrl Pts',(-1.26847368234936,4.30267205415314,
-7.39195447172974));
#139104=CARTESIAN_POINT('Ctrl Pts',(-1.272463135,4.302026826,-7.391267657));
#139105=CARTESIAN_POINT('Ctrl Pts',(-1.672680769,4.237298226,-7.322367136));
#139106=CARTESIAN_POINT('Ctrl Pts',(-2.063118688,4.172121859,-7.210654705));
#139107=CARTESIAN_POINT('Ctrl Pts',(-0.987313967966847,4.30331728230629,
-7.18246283536846));
#139108=CARTESIAN_POINT('Ctrl Pts',(-0.991190137983424,4.30267205415314,
-7.18192574618423));
#139109=CARTESIAN_POINT('Ctrl Pts',(-0.995066308,4.302026826,-7.181388657));
#139110=CARTESIAN_POINT('Ctrl Pts',(-1.383919549,4.237298226,-7.127508443));
#139111=CARTESIAN_POINT('Ctrl Pts',(-1.764681383,4.172121859,-7.031955604));
#139112=CARTESIAN_POINT('',(-1.27246313325074,4.30202682545318,-7.39126765925747));
#139113=CARTESIAN_POINT('Origin',(0.0544441196529202,4.16072874802149,0.18336095777007));
#139114=CARTESIAN_POINT('',(-1.13376471150132,4.30202682438463,-7.28632815855581));
#139115=CARTESIAN_POINT('Origin',(-1.57209315010398E-13,4.39277644300022,
-4.39318720291126E-13));
#139116=CARTESIAN_POINT('',(-1.82735151989587,4.39169923740219,-7.27398009464001));
#139117=CARTESIAN_POINT('Origin',(0.079812667389377,4.16082472253925,0.168262469875141));
#139118=CARTESIAN_POINT('Origin',(0.0695339680088305,4.55341979676417,0.171042352095149));
#139119=CARTESIAN_POINT('Ctrl Pts',(0.036691991,4.172114527,-7.499910246));
#139120=CARTESIAN_POINT('Ctrl Pts',(-0.32319552,4.22940039,-7.501670932));
#139121=CARTESIAN_POINT('Ctrl Pts',(-0.68159806,4.285714286,-7.468964057));
#139122=CARTESIAN_POINT('Ctrl Pts',(-0.733428001,4.29385805,-7.464234193));
#139123=CARTESIAN_POINT('Ctrl Pts',(-0.785187309,4.302026826,-7.458785484));
#139124=CARTESIAN_POINT('Ctrl Pts',(-0.202314096,4.172114527,-7.247176623));
#139125=CARTESIAN_POINT('Ctrl Pts',(-0.550074039,4.22940039,-7.237468465));
#139126=CARTESIAN_POINT('Ctrl Pts',(-0.895306583,4.285714286,-7.194506663));
#139127=CARTESIAN_POINT('Ctrl Pts',(-0.945231961,4.29385805,-7.188293795));
#139128=CARTESIAN_POINT('Ctrl Pts',(-0.995066308,4.302026826,-7.181388657));
#139129=CARTESIAN_POINT('',(-0.891176199469209,4.30202682665757,-7.31870008685521));
#139130=CARTESIAN_POINT('Ctrl Pts',(-0.207079557734034,4.17289950701476,
-7.24704202304173));
#139131=CARTESIAN_POINT('Ctrl Pts',(-0.208440763114175,4.17977820195709,
-7.28862485543279));
#139132=CARTESIAN_POINT('Ctrl Pts',(-0.209823797074378,4.18648410047151,
-7.33026159173366));
#139133=CARTESIAN_POINT('Ctrl Pts',(-0.212626539052888,4.19956141147973,
-7.41353471477598));
#139134=CARTESIAN_POINT('Ctrl Pts',(-0.214047897339691,4.20594050669437,
-7.45522006833701));
#139135=CARTESIAN_POINT('Ctrl Pts',(-0.215486066129178,4.21216499508158,
-7.49690374451352));
#139136=CARTESIAN_POINT('Ctrl Pts',(0.354278060649863,4.30331728230629,
-7.49163217195819));
#139137=CARTESIAN_POINT('Ctrl Pts',(0.350234234324932,4.30267205415314,
-7.49181902897909));
#139138=CARTESIAN_POINT('Ctrl Pts',(0.346190408,4.302026826,-7.492005886));
#139139=CARTESIAN_POINT('Ctrl Pts',(-0.059481935,4.237298226,-7.510751183));
#139140=CARTESIAN_POINT('Ctrl Pts',(-0.464806504,4.172121859,-7.48558313800001));
#139141=CARTESIAN_POINT('Ctrl Pts',(0.579786081215257,4.30331728230629,
-7.22678416372269));
#139142=CARTESIAN_POINT('Ctrl Pts',(0.575885075607629,4.30267205415314,
-7.22709289336134));
#139143=CARTESIAN_POINT('Ctrl Pts',(0.57198407,4.302026826,-7.227401623));
#139144=CARTESIAN_POINT('Ctrl Pts',(0.180639349,4.237298226,-7.258373051));
#139145=CARTESIAN_POINT('Ctrl Pts',(-0.211761522,4.172121859,-7.246906723));
#139146=CARTESIAN_POINT('',(0.459087249095649,4.30202682438522,-7.35970375387025));
#139147=CARTESIAN_POINT('Ctrl Pts',(1.64809316,4.172114527,-7.316678819));
#139148=CARTESIAN_POINT('Ctrl Pts',(1.296998114,4.22940039,-7.395763518));
#139149=CARTESIAN_POINT('Ctrl Pts',(0.939943815,4.285714286,-7.440867263));
#139150=CARTESIAN_POINT('Ctrl Pts',(0.888308847999999,4.29385805,-7.447389885));
#139151=CARTESIAN_POINT('Ctrl Pts',(0.836588333,4.302026826,-7.453195285));
#139152=CARTESIAN_POINT('Ctrl Pts',(1.360344644,4.172114527,-7.121233211));
#139153=CARTESIAN_POINT('Ctrl Pts',(1.018628168,4.22940039,-7.186510132));
#139154=CARTESIAN_POINT('Ctrl Pts',(0.672231452,4.285714286,-7.218767545));
#139155=CARTESIAN_POINT('Ctrl Pts',(0.622137718,4.29385805,-7.223432411));
#139156=CARTESIAN_POINT('Ctrl Pts',(0.57198407,4.302026826,-7.227401623));
#139157=CARTESIAN_POINT('',(0.83658833931498,4.30202682641444,-7.45319528481644));
#139158=CARTESIAN_POINT('',(0.704286205537671,4.30202682665756,-7.3402984536126));
#139159=CARTESIAN_POINT('',(1.40116456911329,4.21216499392617,-7.36795343699078));
#139160=CARTESIAN_POINT('Ctrl Pts',(0.836588339904591,4.30202682552109,
-7.45319528454309));
#139161=CARTESIAN_POINT('Ctrl Pts',(0.871093976326916,4.29657697961046,
-7.44932217884951));
#139162=CARTESIAN_POINT('Ctrl Pts',(0.90554739726429,4.29113922035365,-7.44521228065406));
#139163=CARTESIAN_POINT('Ctrl Pts',(0.939943814463379,4.28571428571329,
-7.44086726300447));
#139164=CARTESIAN_POINT('Ctrl Pts',(1.09390076555659,4.26143250100661,-7.42141914240793));
#139165=CARTESIAN_POINT('Ctrl Pts',(1.24779320355042,4.23689343092027,-7.39712008746252));
#139166=CARTESIAN_POINT('Ctrl Pts',(1.40116456249542,4.21216499285671,-7.3679534382898));
#139167=CARTESIAN_POINT('Ctrl Pts',(1.35566166214689,4.17289950714709,-7.12212619271643));
#139168=CARTESIAN_POINT('Ctrl Pts',(1.36327136050992,4.17977820208819,-7.16302946035241));
#139169=CARTESIAN_POINT('Ctrl Pts',(1.37087132825782,4.18648410045764,-7.20399006333472));
#139170=CARTESIAN_POINT('Ctrl Pts',(1.38603537237231,4.19956141147093,-7.28591881362589));
#139171=CARTESIAN_POINT('Ctrl Pts',(1.39360836328108,4.20594050666662,-7.32693513667193));
#139172=CARTESIAN_POINT('Ctrl Pts',(1.40116457618158,4.2121649950616,-7.36795343551639));
#139173=CARTESIAN_POINT('Ctrl Pts',(1.95647470236699,4.30331728230629,-7.24032266494494));
#139174=CARTESIAN_POINT('Ctrl Pts',(1.9525655871835,4.30267205415314,-7.24137445647247));
#139175=CARTESIAN_POINT('Ctrl Pts',(1.948656472,4.302026826,-7.242426248));
#139176=CARTESIAN_POINT('Ctrl Pts',(1.556498207,4.237298226,-7.347940852));
#139177=CARTESIAN_POINT('Ctrl Pts',(1.155239516,4.172121859,-7.410494023));
#139178=CARTESIAN_POINT('Ctrl Pts',(2.11977597804828,4.30331728230629,-6.93318909679542));
#139179=CARTESIAN_POINT('Ctrl Pts',(2.11603254352414,4.30267205415314,-6.93432920939771));
#139180=CARTESIAN_POINT('Ctrl Pts',(2.112289109,4.302026826,-6.935469322));
#139181=CARTESIAN_POINT('Ctrl Pts',(1.736751751,4.237298226,-7.049844202));
#139182=CARTESIAN_POINT('Ctrl Pts',(1.351060074,4.172121859,-7.123000539));
#139183=CARTESIAN_POINT('',(1.94865647508094,4.30202682545393,-7.24242624901735));
#139184=CARTESIAN_POINT('Origin',(-0.0275791282628238,4.16072876086824,
0.189274367559337));
#139185=CARTESIAN_POINT('',(2.03047280022433,4.30202682438522,-7.08894778221468));
#139186=CARTESIAN_POINT('Origin',(1.07661275727811E-13,4.39277644300133,
-1.57426155444895E-13));
#139187=CARTESIAN_POINT('',(1.39580564426364,4.39169923738589,-7.36897052498046));
#139188=CARTESIAN_POINT('Origin',(0.00178446840968821,4.16082465943076,
0.186223212668429));
#139189=CARTESIAN_POINT('Origin',(-0.00871151387813629,4.55341982448314,
0.184430458010395));
#139190=CARTESIAN_POINT('Ctrl Pts',(3.182431324,4.172114527,-6.791327622));
#139191=CARTESIAN_POINT('Ctrl Pts',(2.856545558,4.22940039,-6.944038421));
#139192=CARTESIAN_POINT('Ctrl Pts',(2.517534962,4.285714286,-7.064843786));
#139193=CARTESIAN_POINT('Ctrl Pts',(2.468509363,4.29385805,-7.082313904));
#139194=CARTESIAN_POINT('Ctrl Pts',(2.419246034,4.302026826,-7.099101959));
#139195=CARTESIAN_POINT('Ctrl Pts',(2.85939518,4.172114527,-6.66230884900001));
#139196=CARTESIAN_POINT('Ctrl Pts',(2.539700455,4.22940039,-6.799518573));
#139197=CARTESIAN_POINT('Ctrl Pts',(2.208336691,4.285714286,-6.905486881));
#139198=CARTESIAN_POINT('Ctrl Pts',(2.16041693,4.29385805,-6.920811357));
#139199=CARTESIAN_POINT('Ctrl Pts',(2.112289109,4.302026826,-6.93546932199999));
#139200=CARTESIAN_POINT('',(2.41924604010374,4.30202682641444,-7.09910195741508));
#139201=CARTESIAN_POINT('',(2.26576757536,4.30202682665756,-7.01728563925367));
#139202=CARTESIAN_POINT('',(2.95229831432839,4.21216499391278,-6.89448581575544));
#139203=CARTESIAN_POINT('Ctrl Pts',(2.41924604060121,4.30202682552109,-7.09910195694042));
#139204=CARTESIAN_POINT('Ctrl Pts',(2.45211235138791,4.29657697961046,-7.08790171038499));
#139205=CARTESIAN_POINT('Ctrl Pts',(2.4848767638631,4.29113922035365,-7.07648143225898));
#139206=CARTESIAN_POINT('Ctrl Pts',(2.51753496156321,4.28571428571329,-7.06484378576816));
#139207=CARTESIAN_POINT('Ctrl Pts',(2.66371171372217,4.26143250097783,-7.01275415784613));
#139208=CARTESIAN_POINT('Ctrl Pts',(2.80878265369269,4.23689343089126,-6.95594087607972));
#139209=CARTESIAN_POINT('Ctrl Pts',(2.95229830817655,4.21216499285671,-6.89448581835788));
#139210=CARTESIAN_POINT('Ctrl Pts',(2.85501364803054,4.17289950713964,-6.66418765580658));
#139211=CARTESIAN_POINT('Ctrl Pts',(2.87123842958936,4.17977820207062,-6.70249876752659));
#139212=CARTESIAN_POINT('Ctrl Pts',(2.88746603344633,4.18648410046127,-6.74086796610841));
#139213=CARTESIAN_POINT('Ctrl Pts',(2.91988781046986,4.19956141145946,-6.81762144647725));
#139214=CARTESIAN_POINT('Ctrl Pts',(2.93610104616866,4.20594050663945,-6.85605086142833));
#139215=CARTESIAN_POINT('Ctrl Pts',(2.95229832085231,4.21216499503082,-6.89448581282505));
#139216=CARTESIAN_POINT('Ctrl Pts',(3.46718876129397,4.30331728230629,-6.65046371610525));
#139217=CARTESIAN_POINT('Ctrl Pts',(3.46359714314698,4.30267205415314,-6.65233126155262));
#139218=CARTESIAN_POINT('Ctrl Pts',(3.460005525,4.302026826,-6.654198807));
#139219=CARTESIAN_POINT('Ctrl Pts',(3.099698224,4.237298226,-6.841548974));
#139220=CARTESIAN_POINT('Ctrl Pts',(2.721267821,4.172121859,-6.988898443));
#139221=CARTESIAN_POINT('Ctrl Pts',(3.56064750517537,4.30331728230629,-6.31540581365904));
#139222=CARTESIAN_POINT('Ctrl Pts',(3.55723668058768,4.30267205415314,-6.31732399882952));
#139223=CARTESIAN_POINT('Ctrl Pts',(3.553825856,4.302026826,-6.319242184));
#139224=CARTESIAN_POINT('Ctrl Pts',(3.211655572,4.237298226,-6.511672474));
#139225=CARTESIAN_POINT('Ctrl Pts',(2.850707601,4.172121859,-6.666030766));
#139226=CARTESIAN_POINT('',(3.46000552820812,4.30202682545392,-6.65419880735245));
#139227=CARTESIAN_POINT('Origin',(-0.0676225796773755,4.16072876375072,
0.1789201855255));
#139228=CARTESIAN_POINT('',(3.50691569939822,4.30202682438522,-6.48672049068936));
#139229=CARTESIAN_POINT('Origin',(1.59160878920872E-13,4.39277644299978,
-3.81639164714898E-13));
#139230=CARTESIAN_POINT('',(2.94728332132454,4.39169923738473,-6.89663113553976));
#139231=CARTESIAN_POINT('Origin',(-0.038289672908362,4.16082472551501,0.182252826938747));
#139232=CARTESIAN_POINT('Origin',(-0.048155027945111,4.55341983599227,0.178246030496119));
#139233=CARTESIAN_POINT('Ctrl Pts',(4.567962537,4.172114527,-5.948421493));
#139234=CARTESIAN_POINT('Ctrl Pts',(4.282524107,4.22940039,-6.167617806));
#139235=CARTESIAN_POINT('Ctrl Pts',(3.977408972,4.285714286,-6.358476065));
#139236=CARTESIAN_POINT('Ctrl Pts',(3.933285124,4.29385805,-6.38607679600001));
#139237=CARTESIAN_POINT('Ctrl Pts',(3.88878248,4.302026826,-6.413062515));
#139238=CARTESIAN_POINT('Ctrl Pts',(4.224743576,4.172114527,-5.89186233000001));
#139239=CARTESIAN_POINT('Ctrl Pts',(3.94201917,4.22940039,-6.094589083));
#139240=CARTESIAN_POINT('Ctrl Pts',(3.641182561,4.285714286,-6.269313324));
#139241=CARTESIAN_POINT('Ctrl Pts',(3.597677446,4.29385805,-6.294580855));
#139242=CARTESIAN_POINT('Ctrl Pts',(3.553825856,4.302026826,-6.319242184));
#139243=CARTESIAN_POINT('',(3.88878248551807,4.30202682620654,-6.41306251204045));
#139244=CARTESIAN_POINT('',(3.72130417150183,4.30202682665756,-6.36615234745303));
#139245=CARTESIAN_POINT('',(4.36538587107081,4.21216499538059,-6.09863970011031));
#139246=CARTESIAN_POINT('Ctrl Pts',(3.88878248571021,4.3020268248974,-6.41306251127443));
#139247=CARTESIAN_POINT('Ctrl Pts',(3.91847267837001,4.29657697940857,-6.39505883492328));
#139248=CARTESIAN_POINT('Ctrl Pts',(3.94801605464148,4.29113922035353,-6.37686217649245));
#139249=CARTESIAN_POINT('Ctrl Pts',(3.97740897183812,4.2857142859281,-6.35847606461008));
#139250=CARTESIAN_POINT('Ctrl Pts',(4.10897046367738,4.26143250061917,-6.27618058148517));
#139251=CARTESIAN_POINT('Ctrl Pts',(4.23843654813059,4.23689343234178,-6.18950960024396));
#139252=CARTESIAN_POINT('Ctrl Pts',(4.36538586557831,4.21216499711468,-6.09863970360881));
#139253=CARTESIAN_POINT('Ctrl Pts',(4.22086836923851,4.17289950698576,-5.8946391104573));
#139254=CARTESIAN_POINT('Ctrl Pts',(4.24494958093159,4.17977820193852,-5.92856668125073));
#139255=CARTESIAN_POINT('Ctrl Pts',(4.26904603628066,4.18648410046027,-5.96255037473311));
#139256=CARTESIAN_POINT('Ctrl Pts',(4.31720953947562,4.19956141148043,-6.03053967769934));
#139257=CARTESIAN_POINT('Ctrl Pts',(4.34130490693522,4.20594050667908,-6.06458526792232));
#139258=CARTESIAN_POINT('Ctrl Pts',(4.36538587665905,4.21216499507077,-6.09863969621531));
#139259=CARTESIAN_POINT('Ctrl Pts',(4.81578092811415,4.30331728230629,-5.74963647599278));
#139260=CARTESIAN_POINT('Ctrl Pts',(4.81267474705707,4.30267205415314,-5.75223245099639));
#139261=CARTESIAN_POINT('Ctrl Pts',(4.809568566,4.302026826,-5.75482842600001));
#139262=CARTESIAN_POINT('Ctrl Pts',(4.497959796,4.237298226,-6.015253869));
#139263=CARTESIAN_POINT('Ctrl Pts',(4.160052666,4.172121859,-6.24050974));
#139264=CARTESIAN_POINT('Ctrl Pts',(4.83502711359236,4.30331728230629,-5.40232117394616));
#139265=CARTESIAN_POINT('Ctrl Pts',(4.83210838529618,4.30267205415314,-5.40492773947309));
#139266=CARTESIAN_POINT('Ctrl Pts',(4.829189657,4.302026826,-5.407534305));
#139267=CARTESIAN_POINT('Ctrl Pts',(4.536385948,4.237298226,-5.669022178));
#139268=CARTESIAN_POINT('Ctrl Pts',(4.21705921,4.172121859,-5.897364803));
#139269=CARTESIAN_POINT('',(4.80956856922516,4.30202682545373,-5.75482842562856));
#139270=CARTESIAN_POINT('Origin',(-0.104504317360521,4.16072873536559,0.16020051259355));
#139271=CARTESIAN_POINT('',(4.81937911915879,4.30202682438463,-5.5811813588866));
#139272=CARTESIAN_POINT('Origin',(-9.54097911787244E-14,4.39277644299978,
-5.76795555762288E-14));
#139273=CARTESIAN_POINT('',(4.36094930658773,4.39169923740455,-6.10181293897598));
#139274=CARTESIAN_POINT('Origin',(-0.0765736298748837,4.16082464507458,
0.169761002488217));
#139275=CARTESIAN_POINT('Origin',(-0.0853466643918449,4.55341982008006,
0.163726636932791));
#139276=CARTESIAN_POINT('Ctrl Pts',(5.739900898,4.172114527,-4.827373787));
#139277=CARTESIAN_POINT('Ctrl Pts',(5.50825658799999,4.22940039,-5.102806236));
#139278=CARTESIAN_POINT('Ctrl Pts',(5.251303759,4.285714286,-5.35479307));
#139279=CARTESIAN_POINT('Ctrl Pts',(5.214144843,4.29385805,-5.391233835));
#139280=CARTESIAN_POINT('Ctrl Pts',(5.176483778,4.302026826,-5.427155396));
#139281=CARTESIAN_POINT('Ctrl Pts',(5.392547658,4.172114527,-4.845918877));
#139282=CARTESIAN_POINT('Ctrl Pts',(5.160013451,4.22940039,-5.10468338));
#139283=CARTESIAN_POINT('Ctrl Pts',(4.903770781,4.285714286,-5.339993645));
#139284=CARTESIAN_POINT('Ctrl Pts',(4.866714564,4.29385805,-5.374022748));
#139285=CARTESIAN_POINT('Ctrl Pts',(4.829189657,4.302026826,-5.40753430500001));
#139286=CARTESIAN_POINT('',(5.17648378289629,4.30202682641444,-5.42715539201625));
#139287=CARTESIAN_POINT('',(5.00110024987486,4.30202682665756,-5.41724674229405));
#139288=CARTESIAN_POINT('',(5.57435283649055,4.21216499393313,-5.01762797091983));
#139289=CARTESIAN_POINT('Ctrl Pts',(5.17648378317564,4.30202682552109,-5.42715539141083));
#139290=CARTESIAN_POINT('Ctrl Pts',(5.20160957745646,4.29657697961046,-5.40319011729322));
#139291=CARTESIAN_POINT('Ctrl Pts',(5.22655050253311,4.29113922035365,-5.37906793386813));
#139292=CARTESIAN_POINT('Ctrl Pts',(5.2513037591335,4.28571428571329,-5.35479307063405));
#139293=CARTESIAN_POINT('Ctrl Pts',(5.36209831934726,4.26143250100229,-5.24613977948583));
#139294=CARTESIAN_POINT('Ctrl Pts',(5.46990586068578,4.23689343091578,-5.1336637348362));
#139295=CARTESIAN_POINT('Ctrl Pts',(5.57435283192434,4.21216499285632,-5.01762797596803));
#139296=CARTESIAN_POINT('Ctrl Pts',(5.38935997722701,4.17289950705447,-4.84946379305138));
#139297=CARTESIAN_POINT('Ctrl Pts',(5.42017160857531,4.17977820204229,-4.87742140740549));
#139298=CARTESIAN_POINT('Ctrl Pts',(5.45101019120633,4.18648410043973,-4.90543055477744));
#139299=CARTESIAN_POINT('Ctrl Pts',(5.51266334906687,4.19956141148847,-4.9614765760749));
#139300=CARTESIAN_POINT('Ctrl Pts',(5.54351417574768,4.20594050667875,-4.98954640745752));
#139301=CARTESIAN_POINT('Ctrl Pts',(5.5743528412703,4.21216499507376,-5.01762796541796));
#139302=CARTESIAN_POINT('Ctrl Pts',(5.93919252974169,4.30331728230629,-4.57996262468676));
#139303=CARTESIAN_POINT('Ctrl Pts',(5.93671702737085,4.30267205415314,-4.58316564434338));
#139304=CARTESIAN_POINT('Ctrl Pts',(5.934241525,4.302026826,-4.586368664));
#139305=CARTESIAN_POINT('Ctrl Pts',(5.685901768,4.237298226,-4.907692179));
#139306=CARTESIAN_POINT('Ctrl Pts',(5.404318073,4.172121859,-5.20032173700001));
#139307=CARTESIAN_POINT('Ctrl Pts',(5.88332622702706,4.30331728230629,-4.23662999944104));
#139308=CARTESIAN_POINT('Ctrl Pts',(5.88103607151352,4.30267205415314,-4.23980306522052));
#139309=CARTESIAN_POINT('Ctrl Pts',(5.878745916,4.302026826,-4.242976131));
#139310=CARTESIAN_POINT('Ctrl Pts',(5.648999958,4.237298226,-4.561294705));
#139311=CARTESIAN_POINT('Ctrl Pts',(5.386225817,4.172121859,-4.852944616));
#139312=CARTESIAN_POINT('',(5.93424152780051,4.3020268254538,-4.58636866354332));
#139313=CARTESIAN_POINT('Origin',(-0.13649934832537,4.16072874717212,0.1339896869126));
#139314=CARTESIAN_POINT('',(5.90649372655079,4.30202682438657,-4.4146723894045));
#139315=CARTESIAN_POINT('Origin',(1.14925430283463E-13,4.39277644300022,
-2.97071395261028E-13));
#139316=CARTESIAN_POINT('',(5.57070214838826,4.39169923734753,-5.02168075129061));
#139317=CARTESIAN_POINT('Origin',(-0.111276857686425,4.16082467415457,0.149330892505302));
#139318=CARTESIAN_POINT('Origin',(-0.118547837337244,4.55341981857088,0.141551906684535));
#139319=CARTESIAN_POINT('Ctrl Pts',(6.643447873,4.172114527,-3.480603448));
#139320=CARTESIAN_POINT('Ctrl Pts',(6.476429113,4.22940039,-3.799393119));
#139321=CARTESIAN_POINT('Ctrl Pts',(6.279653419,4.285714286,-4.100725903));
#139322=CARTESIAN_POINT('Ctrl Pts',(6.25119694500001,4.29385805,-4.144302772));
#139323=CARTESIAN_POINT('Ctrl Pts',(6.222138449,4.302026826,-4.187480522));
#139324=CARTESIAN_POINT('Ctrl Pts',(6.308202204,4.172114527,-3.573385642));
#139325=CARTESIAN_POINT('Ctrl Pts',(6.136731237,4.22940039,-3.876088357));
#139326=CARTESIAN_POINT('Ctrl Pts',(5.93706413,4.285714286,-4.160981797));
#139327=CARTESIAN_POINT('Ctrl Pts',(5.908189518,4.29385805,-4.20218131));
#139328=CARTESIAN_POINT('Ctrl Pts',(5.878745916,4.302026826,-4.242976131));
#139329=CARTESIAN_POINT('',(6.22213845282046,4.30202682641444,-4.18748051700569));
#139330=CARTESIAN_POINT('',(6.05044218481867,4.30202682665756,-4.21522832317184));
#139331=CARTESIAN_POINT('',(6.52266925847057,4.21216499391789,-3.70199753443422));
#139332=CARTESIAN_POINT('Ctrl Pts',(6.22213845282351,4.30202682552109,-4.18748051624066));
#139333=CARTESIAN_POINT('Ctrl Pts',(6.24152499419235,4.29657697961046,-4.15867423426502));
#139334=CARTESIAN_POINT('Ctrl Pts',(6.26069725783376,4.29113922035365,-4.12975445256131));
#139335=CARTESIAN_POINT('Ctrl Pts',(6.27965341901304,4.28571428571329,-4.10072590367582));
#139336=CARTESIAN_POINT('Ctrl Pts',(6.36450041815192,4.26143250099931,-3.97079531071474));
#139337=CARTESIAN_POINT('Ctrl Pts',(6.44560845419607,4.23689343091297,-3.83777345896538));
#139338=CARTESIAN_POINT('Ctrl Pts',(6.5226692551384,4.21216499285688,-3.70199754025746));
#139339=CARTESIAN_POINT('Ctrl Pts',(6.30585110167865,4.17289950699659,-3.57753293676332));
#139340=CARTESIAN_POINT('Ctrl Pts',(6.34195243458989,4.17977820193396,-3.59821332791846));
#139341=CARTESIAN_POINT('Ctrl Pts',(6.37809116773949,4.18648410045907,-3.61893825397248));
#139342=CARTESIAN_POINT('Ctrl Pts',(6.45035114673858,4.19956141146249,-3.66042034419561));
#139343=CARTESIAN_POINT('Ctrl Pts',(6.48651488228287,4.20594050664729,-3.68120190282239));
#139344=CARTESIAN_POINT('Ctrl Pts',(6.52266926190589,4.21216499504144,-3.70199752812543));
#139345=CARTESIAN_POINT('Ctrl Pts',(6.78489409091065,4.30331728230629,-3.19613481065053));
#139346=CARTESIAN_POINT('Ctrl Pts',(6.78316501895532,4.30267205415314,-3.19979510532527));
#139347=CARTESIAN_POINT('Ctrl Pts',(6.781435947,4.302026826,-3.2034554));
#139348=CARTESIAN_POINT('Ctrl Pts',(6.60797729300001,4.237298226,-3.570652257));
#139349=CARTESIAN_POINT('Ctrl Pts',(6.395883572,4.172121859,-3.91697247));
#139350=CARTESIAN_POINT('Ctrl Pts',(6.65652754520183,4.30331728230629,-2.87283871599968));
#139351=CARTESIAN_POINT('Ctrl Pts',(6.65497304760091,4.30267205415314,-2.87642991299984));
#139352=CARTESIAN_POINT('Ctrl Pts',(6.65341854999999,4.302026826,-2.88002111));
#139353=CARTESIAN_POINT('Ctrl Pts',(6.497473009,4.237298226,-3.240286162));
#139354=CARTESIAN_POINT('Ctrl Pts',(6.303538491,4.172121859,-3.581606133));
#139355=CARTESIAN_POINT('',(6.78143594964156,4.30202682545316,-3.20345539893517));
#139356=CARTESIAN_POINT('Origin',(-0.162111758480733,4.16072877310877,0.101513687625245));
#139357=CARTESIAN_POINT('',(6.71742725267403,4.30202682438463,-3.041738245782));
#139358=CARTESIAN_POINT('Origin',(-1.1666015375944E-13,4.392776443,2.42861286636753E-14));
#139359=CARTESIAN_POINT('',(6.51997514986713,4.39169923735663,-3.70674035236029));
#139360=CARTESIAN_POINT('Origin',(-0.140777006050024,4.16082471773229,0.121918379360347));
#139361=CARTESIAN_POINT('Origin',(-0.146205751230233,4.55341981097136,0.112758233578279));
#139362=CARTESIAN_POINT('Ctrl Pts',(7.236354609,4.172114527,-1.971083959));
#139363=CARTESIAN_POINT('Ctrl Pts',(7.14177101,4.22940039,-2.318324601));
#139364=CARTESIAN_POINT('Ctrl Pts',(7.014373465,4.285714286,-2.65491335));
#139365=CARTESIAN_POINT('Ctrl Pts',(6.995950026,4.29385805,-2.703588717));
#139366=CARTESIAN_POINT('Ctrl Pts',(6.97685284100001,4.302026826,-2.752003713));
#139367=CARTESIAN_POINT('Ctrl Pts',(6.928892227,4.172114527,-2.133764867));
#139368=CARTESIAN_POINT('Ctrl Pts',(6.826502291,4.22940039,-2.466251749));
#139369=CARTESIAN_POINT('Ctrl Pts',(6.692746959,4.285714286,-2.787407065));
#139370=CARTESIAN_POINT('Ctrl Pts',(6.673404096,4.29385805,-2.833850545));
#139371=CARTESIAN_POINT('Ctrl Pts',(6.65341855,4.302026826,-2.88002111));
#139372=CARTESIAN_POINT('',(6.97685284363954,4.30202682641444,-2.75200370729722));
#139373=CARTESIAN_POINT('',(6.81513569704902,4.30202682665757,-2.81601240775116));
#139374=CARTESIAN_POINT('',(7.16599291560661,4.21216499395295,-2.21326580715179));
#139375=CARTESIAN_POINT('Ctrl Pts',(6.97685284345356,4.30202682552109,-2.75200370653707));
#139376=CARTESIAN_POINT('Ctrl Pts',(6.98959363920653,4.29657697961046,-2.71970336592859));
#139377=CARTESIAN_POINT('Ctrl Pts',(7.00210076784173,4.29113922035365,-2.68733824251606));
#139378=CARTESIAN_POINT('Ctrl Pts',(7.01437346458369,4.28571428571329,-2.65491335062824));
#139379=CARTESIAN_POINT('Ctrl Pts',(7.06930555124679,4.26143250102719,-2.50978086600207));
#139380=CARTESIAN_POINT('Ctrl Pts',(7.1199215604026,4.23689343094102,-2.36243316113239));
#139381=CARTESIAN_POINT('Ctrl Pts',(7.16599291358868,4.21216499285673,-2.21326581376853));
#139382=CARTESIAN_POINT('Ctrl Pts',(6.92748763804898,4.17289950710276,-2.13832061824829));
#139383=CARTESIAN_POINT('Ctrl Pts',(6.96719061483953,4.17977820206479,-2.1507567935532));
#139384=CARTESIAN_POINT('Ctrl Pts',(7.00693969037473,4.18648410049305,-2.16322842251709));
#139385=CARTESIAN_POINT('Ctrl Pts',(7.08642769447389,4.1995614115264,-2.18820692471099));
#139386=CARTESIAN_POINT('Ctrl Pts',(7.12621336273325,4.20594050671967,-2.20072848782133));
#139387=CARTESIAN_POINT('Ctrl Pts',(7.16599291766674,4.21216499511605,-2.21326580003777));
#139388=CARTESIAN_POINT('Ctrl Pts',(7.31334154411131,4.30331728230629,-1.66285928523758));
#139389=CARTESIAN_POINT('Ctrl Pts',(7.31243975205566,4.30267205415314,-1.66680570361879));
#139390=CARTESIAN_POINT('Ctrl Pts',(7.31153796000001,4.302026826,-1.670752122));
#139391=CARTESIAN_POINT('Ctrl Pts',(7.221071143,4.237298226,-2.066652604));
#139392=CARTESIAN_POINT('Ctrl Pts',(7.088384665,4.172121859,-2.450469923));
#139393=CARTESIAN_POINT('Ctrl Pts',(7.11847703421988,4.30331728230629,-1.37471668631063));
#139394=CARTESIAN_POINT('Ctrl Pts',(7.11773088110994,4.30267205415314,-1.37855809415531));
#139395=CARTESIAN_POINT('Ctrl Pts',(7.116984728,4.302026826,-1.382399502));
#139396=CARTESIAN_POINT('Ctrl Pts',(7.042131444,4.237298226,-1.767765439));
#139397=CARTESIAN_POINT('Ctrl Pts',(6.926104711,4.172121859,-2.142795728));
#139398=CARTESIAN_POINT('',(7.31153796235453,4.30202682545332,-1.67075212042859));
#139399=CARTESIAN_POINT('Origin',(-0.180144240362469,4.16072874364623,0.0642911481372335));
#139400=CARTESIAN_POINT('',(7.21426134609414,4.30202682438518,-1.52657580210354));
#139401=CARTESIAN_POINT('Origin',(1.90819582357449E-14,4.39277644300067,
-5.85469173142172E-15));
#139402=CARTESIAN_POINT('',(7.16438135929105,4.39169923736879,-2.21847689478551));
#139403=CARTESIAN_POINT('Origin',(-0.163694659822479,4.16082469767973,0.0888051356908687));
#139404=CARTESIAN_POINT('Origin',(-0.167027008642707,4.5534198132657,0.0786920270273214));
#139405=CARTESIAN_POINT('Ctrl Pts',(7.490897446,4.172114527,-0.369398776));
#139406=CARTESIAN_POINT('Ctrl Pts',(7.473171633,4.22940039,-0.728853803));
#139407=CARTESIAN_POINT('Ctrl Pts',(7.421109203,4.285714286,-1.08496));
#139408=CARTESIAN_POINT('Ctrl Pts',(7.413580259,4.29385805,-1.136457858));
#139409=CARTESIAN_POINT('Ctrl Pts',(7.405337348,4.302026826,-1.187846269));
#139410=CARTESIAN_POINT('Ctrl Pts',(7.22559495,4.172114527,-0.594371618));
#139411=CARTESIAN_POINT('Ctrl Pts',(7.197073686,4.22940039,-0.941095951));
#139412=CARTESIAN_POINT('Ctrl Pts',(7.135484378,4.285714286,-1.283496277));
#139413=CARTESIAN_POINT('Ctrl Pts',(7.126577716,4.29385805,-1.333012078));
#139414=CARTESIAN_POINT('Ctrl Pts',(7.116984728,4.302026826,-1.382399502));
#139415=CARTESIAN_POINT('',(7.40533734948122,4.30202682641445,-1.18784626286505));
#139416=CARTESIAN_POINT('',(7.26116103870691,4.30202682665756,-1.28512288150586));
#139417=CARTESIAN_POINT('',(7.47424270827965,4.21216499391622,-0.621044231009006));
#139418=CARTESIAN_POINT('Ctrl Pts',(7.40533734932785,4.30202682552109,-1.18784626221161));
#139419=CARTESIAN_POINT('Ctrl Pts',(7.41083665397239,4.29657697961046,-1.15356219080014));
#139420=CARTESIAN_POINT('Ctrl Pts',(7.41609382804621,4.29113922035365,-1.1192650831263));
#139421=CARTESIAN_POINT('Ctrl Pts',(7.42110920265718,4.28571428571329,-1.08496000029361));
#139422=CARTESIAN_POINT('Ctrl Pts',(7.44355781350102,4.26143250099309,-0.931411857988833));
#139423=CARTESIAN_POINT('Ctrl Pts',(7.46131504754232,4.2368934309067,-0.776628114674704));
#139424=CARTESIAN_POINT('Ctrl Pts',(7.474242707784,4.21216499285688,-0.621044237665823));
#139425=CARTESIAN_POINT('Ctrl Pts',(7.22520255128188,4.17289950705358,-0.599122803260408));
#139426=CARTESIAN_POINT('Ctrl Pts',(7.26665070451171,4.17977820198768,-0.602733261370328));
#139427=CARTESIAN_POINT('Ctrl Pts',(7.30815150059235,4.18648410045454,-0.60636843442612));
#139428=CARTESIAN_POINT('Ctrl Pts',(7.39115075880867,4.1995614114589,-0.613675382042574));
#139429=CARTESIAN_POINT('Ctrl Pts',(7.43269802619587,4.20594050665111,-0.617351455425911));
#139430=CARTESIAN_POINT('Ctrl Pts',(7.47424270874489,4.21216499504173,-0.621044223877748));
#139431=CARTESIAN_POINT('Ctrl Pts',(7.49982527573975,4.30331728230629,-0.0518303081088053));
#139432=CARTESIAN_POINT('Ctrl Pts',(7.49979293036987,4.30267205415314,-0.0558783200544026));
#139433=CARTESIAN_POINT('Ctrl Pts',(7.499760585,4.302026826,-0.059926332));
#139434=CARTESIAN_POINT('Ctrl Pts',(7.496515732,4.237298226,-0.466018572));
#139435=CARTESIAN_POINT('Ctrl Pts',(7.449440769,4.172121859,-0.869386126));
#139436=CARTESIAN_POINT('Ctrl Pts',(7.24757444764504,4.30331728230629,0.187685567453841));
#139437=CARTESIAN_POINT('Ctrl Pts',(7.24767152832252,4.30267205415314,0.18377356872692));
#139438=CARTESIAN_POINT('Ctrl Pts',(7.247768609,4.302026826,0.17986157));
#139439=CARTESIAN_POINT('Ctrl Pts',(7.25750763900001,4.237298226,-0.212585969));
#139440=CARTESIAN_POINT('Ctrl Pts',(7.224813973,4.172121859,-0.603790576));
#139441=CARTESIAN_POINT('',(7.49976058695747,4.30202682545315,-0.0599263299449481));
#139442=CARTESIAN_POINT('Origin',(-0.189753551632893,4.16072874191932,0.0240623880134643));
#139443=CARTESIAN_POINT('',(7.37376459691771,4.30202682438463,0.0599676291186608));
#139444=CARTESIAN_POINT('Origin',(2.31932528738099E-12,4.39277644299933,
-2.63183301107278E-13));
#139445=CARTESIAN_POINT('',(7.47378905921352,4.39169923737642,-0.626479923766734));
#139446=CARTESIAN_POINT('Origin',(-0.178957929415752,4.16082468300723,0.0515394024429872));
#139447=CARTESIAN_POINT('Origin',(-0.180038598006461,4.55341981446118,0.0409463889791393));
#139448=CARTESIAN_POINT('Ctrl Pts',(7.395174244,4.172114527,1.249559084));
#139449=CARTESIAN_POINT('Ctrl Pts',(7.455135056,4.22940039,0.894697389999999));
#139450=CARTESIAN_POINT('Ctrl Pts',(7.480842122,4.285714286,0.535724874));
#139451=CARTESIAN_POINT('Ctrl Pts',(7.484559718,4.29385805,0.483812507));
#139452=CARTESIAN_POINT('Ctrl Pts',(7.487556512,4.302026826,0.431853546));
#139453=CARTESIAN_POINT('Ctrl Pts',(7.18443688400001,4.172114527,0.972813787));
#139454=CARTESIAN_POINT('Ctrl Pts',(7.231117913,4.22940039,0.628064447));
#139455=CARTESIAN_POINT('Ctrl Pts',(7.244574478,4.285714286,0.28042937));
#139456=CARTESIAN_POINT('Ctrl Pts',(7.246520483,4.29385805,0.230156553));
#139457=CARTESIAN_POINT('Ctrl Pts',(7.247768609,4.302026826,0.17986157));
#139458=CARTESIAN_POINT('',(7.48755651189106,4.30202682641444,0.431853552262134));
#139459=CARTESIAN_POINT('',(7.36766256033176,4.30202682665756,0.305857562052724));
#139460=CARTESIAN_POINT('',(7.43300521886331,4.21216499391146,1.00021668358226));
#139461=CARTESIAN_POINT('Ctrl Pts',(7.48755651123017,4.30202682552109,0.431853552879705));
#139462=CARTESIAN_POINT('Ctrl Pts',(7.48555718325308,4.29657697961046,0.466518269918783));
#139463=CARTESIAN_POINT('Ctrl Pts',(7.48331858317738,4.29113922035365,0.501143667389628));
#139464=CARTESIAN_POINT('Ctrl Pts',(7.48084212235687,4.28571428571329,0.535724873765609));
#139465=CARTESIAN_POINT('Ctrl Pts',(7.46975758539743,4.26143250098825,0.69050893374431));
#139466=CARTESIAN_POINT('Ctrl Pts',(7.45382573571466,4.23689343090182,0.845491199722909));
#139467=CARTESIAN_POINT('Ctrl Pts',(7.43300521989358,4.21216499285686,1.00021667704294));
#139468=CARTESIAN_POINT('Ctrl Pts',(7.18507502302376,4.17289950688029,0.968089327989833));
#139469=CARTESIAN_POINT('Ctrl Pts',(7.22633028323422,4.17977820185,0.973473408110541));
#139470=CARTESIAN_POINT('Ctrl Pts',(7.26764226897952,4.18648410041496,0.978844667865212));
#139471=CARTESIAN_POINT('Ctrl Pts',(7.35027182833364,4.19956141144009,0.989550939784512));
#139472=CARTESIAN_POINT('Ctrl Pts',(7.39163799084773,4.20594050664826,0.994892245391633));
#139473=CARTESIAN_POINT('Ctrl Pts',(7.4330052177926,4.21216499503617,1.00021669058607));
#139474=CARTESIAN_POINT('Ctrl Pts',(7.33562551247557,4.30331728230629,1.56162219693697));
#139475=CARTESIAN_POINT('Ctrl Pts',(7.33646412623779,4.30267205415314,1.55766187196849));
#139476=CARTESIAN_POINT('Ctrl Pts',(7.33730274,4.302026826,1.553701547));
#139477=CARTESIAN_POINT('Ctrl Pts',(7.42143157800001,4.237298226,1.156405971));
#139478=CARTESIAN_POINT('Ctrl Pts',(7.462169301,4.172121859,0.7523492));
#139479=CARTESIAN_POINT('Ctrl Pts',(7.03778333585493,4.30331728230629,1.74131185278812));
#139480=CARTESIAN_POINT('Ctrl Pts',(7.03871911092747,4.30267205415314,1.73751218389406));
#139481=CARTESIAN_POINT('Ctrl Pts',(7.039654886,4.302026826,1.733712515));
#139482=CARTESIAN_POINT('Ctrl Pts',(7.133530843,4.237298226,1.352533785));
#139483=CARTESIAN_POINT('Ctrl Pts',(7.185698963,4.172121859,0.963447153));
#139484=CARTESIAN_POINT('',(7.33730274119938,4.30202682545375,1.55370154999587));
#139485=CARTESIAN_POINT('Origin',(-0.190489594696511,4.16072877780515,-0.0172915305091799));
#139486=CARTESIAN_POINT('',(7.18847881074456,4.30202682438474,1.64370704086378));
#139487=CARTESIAN_POINT('Origin',(-8.23559970219989E-13,4.39277644299978,
-1.08094956596805E-13));
#139488=CARTESIAN_POINT('',(7.43373068909092,4.39169923741036,0.994810553290058));
#139489=CARTESIAN_POINT('Origin',(-0.185853746422783,4.16082470961366,0.0118637316186057));
#139490=CARTESIAN_POINT('Origin',(-0.184631640022924,4.55341981006142,0.00128611064958345));
#139491=CARTESIAN_POINT('Ctrl Pts',(6.953660913,4.172114527,2.810088949));
#139492=CARTESIAN_POINT('Ctrl Pts',(7.088504649,4.22940039,2.476413527));
#139493=CARTESIAN_POINT('Ctrl Pts',(7.190779179,4.285714286,2.131359848));
#139494=CARTESIAN_POINT('Ctrl Pts',(7.20556948400001,4.29385805,2.081460337));
#139495=CARTESIAN_POINT('Ctrl Pts',(7.219665854,4.302026826,2.031360369));
#139496=CARTESIAN_POINT('Ctrl Pts',(6.80734253400001,4.172114527,2.494511501));
#139497=CARTESIAN_POINT('Ctrl Pts',(6.927043104,4.22940039,2.167857251));
#139498=CARTESIAN_POINT('Ctrl Pts',(7.014916327,4.285714286,1.831242452));
#139499=CARTESIAN_POINT('Ctrl Pts',(7.02762400500001,4.29385805,1.782563319));
#139500=CARTESIAN_POINT('Ctrl Pts',(7.039654886,4.302026826,1.733712515));
#139501=CARTESIAN_POINT('',(7.21966585287234,4.30202682641444,2.03136037523548));
#139502=CARTESIAN_POINT('',(7.12966036896448,4.30202682665756,1.88253644592181));
#139503=CARTESIAN_POINT('',(7.04420866668809,4.21216499392905,2.57470857710942));
#139504=CARTESIAN_POINT('Ctrl Pts',(7.21966585263097,4.30202682552109,2.03136037579604));
#139505=CARTESIAN_POINT('Ctrl Pts',(7.21026137828318,4.29657697961046,2.06478485483961));
#139506=CARTESIAN_POINT('Ctrl Pts',(7.20063167850688,4.29113922035365,2.09811949687687));
#139507=CARTESIAN_POINT('Ctrl Pts',(7.1907791788114,4.28571428571329,2.13135984797792));
#139508=CARTESIAN_POINT('Ctrl Pts',(7.14667979468729,4.26143250099391,2.28014229476132));
#139509=CARTESIAN_POINT('Ctrl Pts',(7.09780381684114,4.23689343090752,2.42807628479987));
#139510=CARTESIAN_POINT('Ctrl Pts',(7.04420866918739,4.21216499285688,2.57470857087657));
#139511=CARTESIAN_POINT('Ctrl Pts',(6.80898137272616,4.17289950689835,2.49003467807449));
#139512=CARTESIAN_POINT('Ctrl Pts',(6.84811468974111,4.17977820186027,2.50416154280778));
#139513=CARTESIAN_POINT('Ctrl Pts',(6.88730616221774,4.18648410044305,2.51828808128039));
#139514=CARTESIAN_POINT('Ctrl Pts',(6.96570235636468,4.19956141146743,2.54650695922136));
#139515=CARTESIAN_POINT('Ctrl Pts',(7.00495317822537,4.20594050668545,2.56061589023492));
#139516=CARTESIAN_POINT('Ctrl Pts',(7.04420866410003,4.21216499507508,2.57470858381234));
#139517=CARTESIAN_POINT('Ctrl Pts',(6.82842005352701,4.30331728230629,3.10205498320627));
#139518=CARTESIAN_POINT('Ctrl Pts',(6.83009041376351,4.30267205415314,3.09836752560313));
#139519=CARTESIAN_POINT('Ctrl Pts',(6.831760774,4.302026826,3.094680068));
#139520=CARTESIAN_POINT('Ctrl Pts',(6.999329531,4.237298226,2.724758255));
#139521=CARTESIAN_POINT('Ctrl Pts',(7.125975091,4.172121859,2.338905513));
#139522=CARTESIAN_POINT('Ctrl Pts',(6.49891329666129,4.30331728230629,3.21351633154874));
#139523=CARTESIAN_POINT('Ctrl Pts',(6.50064401033065,4.30267205415314,3.21000666077437));
#139524=CARTESIAN_POINT('Ctrl Pts',(6.502374724,4.302026826,3.20649699));
#139525=CARTESIAN_POINT('Ctrl Pts',(6.675998073,4.237298226,2.854410562));
#139526=CARTESIAN_POINT('Ctrl Pts',(6.810588656,4.172121859,2.485635163));
#139527=CARTESIAN_POINT('',(6.83176077452481,4.30202682545371,3.09468007118652));
#139528=CARTESIAN_POINT('Origin',(-0.182319011662516,4.16072878009169,-0.0578369453895083));
#139529=CARTESIAN_POINT('',(6.66706774467661,4.30202682438463,3.1505885381489));
#139530=CARTESIAN_POINT('Origin',(1.34484437475102E-12,4.39277644299978,
4.93962509784396E-13));
#139531=CARTESIAN_POINT('',(7.04607933373822,4.39169923741341,2.56958479416804));
#139532=CARTESIAN_POINT('Origin',(-0.184058831711233,4.16082468518637,-0.0283666495870066));
#139533=CARTESIAN_POINT('Origin',(-0.180591247415827,4.55341982673589,-0.0384341815324341));
#139534=CARTESIAN_POINT('Ctrl Pts',(6.187002127,4.172114527,4.239222179));
#139535=CARTESIAN_POINT('Ctrl Pts',(6.390423644,4.22940039,3.94233532));
#139536=CARTESIAN_POINT('Ctrl Pts',(6.564483393,4.285714286,3.627334805));
#139537=CARTESIAN_POINT('Ctrl Pts',(6.589654828,4.29385805,3.581781394));
#139538=CARTESIAN_POINT('Ctrl Pts',(6.61419164600001,4.302026826,3.53588304));
#139539=CARTESIAN_POINT('Ctrl Pts',(6.11194441300001,4.172114527,3.89956863));
#139540=CARTESIAN_POINT('Ctrl Pts',(6.299067458,4.22940039,3.606283458));
#139541=CARTESIAN_POINT('Ctrl Pts',(6.457248486,4.285714286,3.296428672));
#139542=CARTESIAN_POINT('Ctrl Pts',(6.48012364,4.29385805,3.251619405));
#139543=CARTESIAN_POINT('Ctrl Pts',(6.50237472400001,4.302026826,3.20649699));
#139544=CARTESIAN_POINT('',(6.61419164333589,4.30202682641444,3.53588304568432));
#139545=CARTESIAN_POINT('',(6.55772409853652,4.30202682665757,3.36954308835721));
#139546=CARTESIAN_POINT('',(6.32603274655909,4.21216499392067,4.02880995941814));
#139547=CARTESIAN_POINT('Ctrl Pts',(6.6141916425897,4.30202682552109,3.53588304601502));
#139548=CARTESIAN_POINT('Ctrl Pts',(6.59782176496394,4.29657697961046,3.56650439473428));
#139549=CARTESIAN_POINT('Ctrl Pts',(6.58125123958368,4.29113922035365,3.59698959050121));
#139550=CARTESIAN_POINT('Ctrl Pts',(6.56448339291723,4.28571428571329,3.62733480452437));
#139551=CARTESIAN_POINT('Ctrl Pts',(6.48943119969881,4.26143250100208,3.76315873656664));
#139552=CARTESIAN_POINT('Ctrl Pts',(6.40989648014607,4.23689343091575,3.897127221554));
#139553=CARTESIAN_POINT('Ctrl Pts',(6.32603275018521,4.21216499285683,4.02880995376847));
#139554=CARTESIAN_POINT('Ctrl Pts',(6.11450732205272,4.17289950712114,3.89554877408609));
#139555=CARTESIAN_POINT('Ctrl Pts',(6.14968886578877,4.1797782021083,3.91775786726618));
#139556=CARTESIAN_POINT('Ctrl Pts',(6.18492727408787,4.18648410045048,3.93997914259056));
#139557=CARTESIAN_POINT('Ctrl Pts',(6.25542438446169,4.19956141148895,3.98439114355122));
#139558=CARTESIAN_POINT('Ctrl Pts',(6.29072454069049,4.20594050666881,4.00660798203398));
#139559=CARTESIAN_POINT('Ctrl Pts',(6.32603274259154,4.21216499504938,4.02880996541136));
#139560=CARTESIAN_POINT('Ctrl Pts',(6.00192526193812,4.30331728230629,4.4974391266339));
#139561=CARTESIAN_POINT('Ctrl Pts',(6.00434926446906,4.30267205415315,4.49419695781695));
#139562=CARTESIAN_POINT('Ctrl Pts',(6.006773267,4.302026826,4.490954789));
#139563=CARTESIAN_POINT('Ctrl Pts',(6.249946615,4.237298226,4.165703872));
#139564=CARTESIAN_POINT('Ctrl Pts',(6.456578206,4.172121859,3.816097204));
#139565=CARTESIAN_POINT('Ctrl Pts',(5.65616129496628,4.30331728230629,4.53546035768119));
#139566=CARTESIAN_POINT('Ctrl Pts',(5.65860602098314,4.30267205415315,4.5324047933406));
#139567=CARTESIAN_POINT('Ctrl Pts',(5.661050747,4.302026826,4.529349229));
#139568=CARTESIAN_POINT('Ctrl Pts',(5.906303053,4.237298226,4.222818274));
#139569=CARTESIAN_POINT('Ctrl Pts',(6.117022792,4.172121859,3.891597635));
#139570=CARTESIAN_POINT('',(6.00677326682245,4.30202682545379,4.49095479222783));
#139571=CARTESIAN_POINT('Origin',(-0.165623166175317,4.16072878917566,-0.0956778885946874));
#139572=CARTESIAN_POINT('',(5.83391200081167,4.30202682438483,4.51015201700465));
#139573=CARTESIAN_POINT('Origin',(-5.31692745386891E-13,4.39277644300067,
-3.68411898210574E-13));
#139574=CARTESIAN_POINT('',(6.32896114034785,4.39169923739958,4.02420810597715));
#139575=CARTESIAN_POINT('Origin',(-0.173657580569582,4.1608246493853,-0.0672706206153839));
#139576=CARTESIAN_POINT('Origin',(-0.168107033907274,4.55341982151689,-0.076357479274628));
#139577=CARTESIAN_POINT('Ctrl Pts',(5.131045997,4.172114527,5.470134091));
#139578=CARTESIAN_POINT('Ctrl Pts',(5.393533531,4.22940039,5.223917895));
#139579=CARTESIAN_POINT('Ctrl Pts',(5.631239659,4.285714286,4.953699618));
#139580=CARTESIAN_POINT('Ctrl Pts',(5.66561523700001,4.29385805,4.914622335));
#139581=CARTESIAN_POINT('Ctrl Pts',(5.69944518700001,4.302026826,4.875071749));
#139582=CARTESIAN_POINT('Ctrl Pts',(5.130758564,4.172114527,5.122286263));
#139583=CARTESIAN_POINT('Ctrl Pts',(5.376554419,4.22940039,4.87608386));
#139584=CARTESIAN_POINT('Ctrl Pts',(5.597646882,4.285714286,4.607477551));
#139585=CARTESIAN_POINT('Ctrl Pts',(5.629619895,4.29385805,4.568633382));
#139586=CARTESIAN_POINT('Ctrl Pts',(5.661050747,4.302026826,4.529349229));
#139587=CARTESIAN_POINT('',(5.69944518326463,4.30202682641445,4.8750717540797));
#139588=CARTESIAN_POINT('',(5.68005599221441,4.30202682665756,4.70048187952442));
#139589=CARTESIAN_POINT('',(5.3120585659177,4.21216499394814,5.29452866556222));
#139590=CARTESIAN_POINT('Ctrl Pts',(5.69944518263236,4.30202682552109,4.87507175436104));
#139591=CARTESIAN_POINT('Ctrl Pts',(5.67687533869791,4.29657697961046,4.90145815332426));
#139592=CARTESIAN_POINT('Ctrl Pts',(5.65413880693874,4.29113922035365,4.92766844913144));
#139593=CARTESIAN_POINT('Ctrl Pts',(5.63123965919007,4.28571428571329,4.95369961753485));
#139594=CARTESIAN_POINT('Ctrl Pts',(5.52874401419247,4.26143250103135,5.07021405837047));
#139595=CARTESIAN_POINT('Ctrl Pts',(5.42226950816182,4.23689343094526,5.18395282076903));
#139596=CARTESIAN_POINT('Ctrl Pts',(5.3120585708442,4.21216499285688,5.29452866078942));
#139597=CARTESIAN_POINT('Ctrl Pts',(5.13412570350878,4.17289950703851,5.11891133959974));
#139598=CARTESIAN_POINT('Ctrl Pts',(5.16371042366419,4.17977820201081,5.14816418808481));
#139599=CARTESIAN_POINT('Ctrl Pts',(5.19334806060398,4.1864841004508,5.17744115868062));
#139600=CARTESIAN_POINT('Ctrl Pts',(5.25264972022252,4.19956141149291,5.23596962626228));
#139601=CARTESIAN_POINT('Ctrl Pts',(5.28234861498335,4.20594050671005,5.26525553759414));
#139602=CARTESIAN_POINT('Ctrl Pts',(5.31205856064242,4.21216499511036,5.29452867066908));
#139603=CARTESIAN_POINT('Ctrl Pts',(4.89478711568802,4.30331728230629,5.68252801464834));
#139604=CARTESIAN_POINT('Ctrl Pts',(4.89785141684401,4.30267205415314,5.67988273482417));
#139605=CARTESIAN_POINT('Ctrl Pts',(4.90091571800001,4.302026826,5.67723745499999));
#139606=CARTESIAN_POINT('Ctrl Pts',(5.208323141,4.237298226,5.41186580500001));
#139607=CARTESIAN_POINT('Ctrl Pts',(5.4852789,4.172121859,5.114852431));
#139608=CARTESIAN_POINT('Ctrl Pts',(4.54893347762908,4.30331728230629,5.64533129824391));
#139609=CARTESIAN_POINT('Ctrl Pts',(4.55197790331453,4.30267205415314,5.64287271512195));
#139610=CARTESIAN_POINT('Ctrl Pts',(4.555022329,4.302026826,5.640414132));
#139611=CARTESIAN_POINT('Ctrl Pts',(4.860435866,4.237298226,5.39377169600001));
#139612=CARTESIAN_POINT('Ctrl Pts',(5.137431742,4.172121859,5.115593328));
#139613=CARTESIAN_POINT('',(4.90091571714228,4.30202682545372,5.67723745811082));
#139614=CARTESIAN_POINT('Origin',(-0.141183175810484,4.16072878338812,-0.129045188906731));
#139615=CARTESIAN_POINT('',(4.72796901573467,4.30202682438463,5.65882579998796));
#139616=CARTESIAN_POINT('Origin',(7.01695646032618E-13,4.39277644300044,
6.59628601740181E-13));
#139617=CARTESIAN_POINT('',(5.31590775787188,4.39169923738042,5.29066391891839));
#139618=CARTESIAN_POINT('Origin',(-0.15513626692275,4.16082473539166,-0.103029040356922));
#139619=CARTESIAN_POINT('Origin',(-0.14776242244722,4.55341983644703,-0.110710578795594));
#139620=CARTESIAN_POINT('Ctrl Pts',(3.83516786,4.172114527,6.445268612));
#139621=CARTESIAN_POINT('Ctrl Pts',(4.144447785,4.22940039,6.261235875));
#139622=CARTESIAN_POINT('Ctrl Pts',(4.434685418,4.285714286,6.048434942));
#139623=CARTESIAN_POINT('Ctrl Pts',(4.476657775,4.29385805,6.01766099800001));
#139624=CARTESIAN_POINT('Ctrl Pts',(4.518199006,4.302026826,5.986307521));
#139625=CARTESIAN_POINT('Ctrl Pts',(3.909664147,4.172114527,6.105491484));
#139626=CARTESIAN_POINT('Ctrl Pts',(4.202639671,4.22940039,5.917883999));
#139627=CARTESIAN_POINT('Ctrl Pts',(4.476305531,4.285714286,5.703085901));
#139628=CARTESIAN_POINT('Ctrl Pts',(4.51588138100001,4.29385805,5.67202313900001));
#139629=CARTESIAN_POINT('Ctrl Pts',(4.555022329,4.302026826,5.640414132));
#139630=CARTESIAN_POINT('',(4.51819900130735,4.30202682641451,5.98630752524338));
#139631=CARTESIAN_POINT('',(4.53661066430174,4.30202682665767,5.81336082899585));
#139632=CARTESIAN_POINT('',(4.04969843050623,4.21216499391419,6.31268109603982));
#139633=CARTESIAN_POINT('Ctrl Pts',(4.51819900073126,4.30202682552109,5.98630752549441));
#139634=CARTESIAN_POINT('Ctrl Pts',(4.49048453128782,4.29657697961046,6.00722517591779));
#139635=CARTESIAN_POINT('Ctrl Pts',(4.46264512820145,4.29113922035365,6.02793500731677));
#139636=CARTESIAN_POINT('Ctrl Pts',(4.43468541808248,4.28571428571326,6.04843494158998));
#139637=CARTESIAN_POINT('Ctrl Pts',(4.30953890349148,4.2614325009866,6.14019180576064));
#139638=CARTESIAN_POINT('Ctrl Pts',(4.18110324017952,4.23689343090015,6.22838254783057));
#139639=CARTESIAN_POINT('Ctrl Pts',(4.04969843616027,4.21216499285689,6.31268109254388));
#139640=CARTESIAN_POINT('Ctrl Pts',(3.91367807290479,4.17289950687043,6.10291929893263));
#139641=CARTESIAN_POINT('Ctrl Pts',(3.93628262107007,4.17977820182286,6.13784807241261));
#139642=CARTESIAN_POINT('Ctrl Pts',(3.9589336638548,4.18648410041305,6.17281178040934));
#139643=CARTESIAN_POINT('Ctrl Pts',(4.00426699324573,4.1995614114377,6.24271998879621));
#139644=CARTESIAN_POINT('Ctrl Pts',(4.02697593910242,4.20594050664488,6.27770559622218));
#139645=CARTESIAN_POINT('Ctrl Pts',(4.04969842444934,4.21216499503999,6.31268109977444));
#139646=CARTESIAN_POINT('Ctrl Pts',(3.5587741640618,4.30331728230629,6.60190820898191));
#139647=CARTESIAN_POINT('Ctrl Pts',(3.5623354805309,4.30267205415314,6.59998350849095));
#139648=CARTESIAN_POINT('Ctrl Pts',(3.565896797,4.302026826,6.598058808));
#139649=CARTESIAN_POINT('Ctrl Pts',(3.923164266,4.237298226,6.404974908));
#139650=CARTESIAN_POINT('Ctrl Pts',(4.257494048,4.172121859,6.174442844));
#139651=CARTESIAN_POINT('Ctrl Pts',(3.22900258618386,4.30331728230629,6.49123282156182));
#139652=CARTESIAN_POINT('Ctrl Pts',(3.23250435759193,4.30267205415314,6.48948618028091));
#139653=CARTESIAN_POINT('Ctrl Pts',(3.236006129,4.302026826,6.487739539));
#139654=CARTESIAN_POINT('Ctrl Pts',(3.587300101,4.237298226,6.312518349));
#139655=CARTESIAN_POINT('Ctrl Pts',(3.917620093,4.172121859,6.100389562));
#139656=CARTESIAN_POINT('',(3.56589679608909,4.30202682545316,6.59805881069389));
#139657=CARTESIAN_POINT('Origin',(-0.110141570649285,4.16072872614212,-0.156378502227356));
#139658=CARTESIAN_POINT('',(3.40095145402154,4.30202682438465,6.54289917816694));
#139659=CARTESIAN_POINT('Origin',(-8.72565908416334E-13,4.392776443,-1.20823490101785E-12));
#139660=CARTESIAN_POINT('',(4.05428843735919,4.3916992373681,6.30973416716977));
#139661=CARTESIAN_POINT('Origin',(-0.129361106999302,4.16082469154354,-0.13397002573184));
#139662=CARTESIAN_POINT('Origin',(-0.120508300879558,4.55341982873688,-0.139886746186956));
#139663=CARTESIAN_POINT('Ctrl Pts',(2.359961536,4.172114527,7.119029537));
#139664=CARTESIAN_POINT('Ctrl Pts',(2.701572267,4.22940039,7.005785424));
#139665=CARTESIAN_POINT('Ctrl Pts',(3.030770215,4.285714286,6.86035217));
#139666=CARTESIAN_POINT('Ctrl Pts',(3.07837677,4.29385805,6.83932052));
#139667=CARTESIAN_POINT('Ctrl Pts',(3.125686861,4.302026826,6.817630208));
#139668=CARTESIAN_POINT('Ctrl Pts',(2.50575818,4.172114527,6.803210709));
#139669=CARTESIAN_POINT('Ctrl Pts',(2.832214162,4.22940039,6.68297046));
#139670=CARTESIAN_POINT('Ctrl Pts',(3.145657109,4.285714286,6.532024292));
#139671=CARTESIAN_POINT('Ctrl Pts',(3.190985273,4.29385805,6.510195399));
#139672=CARTESIAN_POINT('Ctrl Pts',(3.236006129,4.302026826,6.487739539));
#139673=CARTESIAN_POINT('',(3.1256868554126,4.30202682641445,6.81763021082508));
#139674=CARTESIAN_POINT('',(3.18084649134053,4.30202682665757,6.65268487524971));
#139675=CARTESIAN_POINT('',(2.59797889752575,4.21216499390815,7.03565957449181));
#139676=CARTESIAN_POINT('Ctrl Pts',(3.12568685454772,4.30202682552111,6.81763021051357));
#139677=CARTESIAN_POINT('Ctrl Pts',(3.0941236577602,4.29657697961046,6.83210102606678));
#139678=CARTESIAN_POINT('Ctrl Pts',(3.06248312301008,4.29113922035365,6.84634202432006));
#139679=CARTESIAN_POINT('Ctrl Pts',(3.03077021551498,4.28571428571329,6.8603521703151));
#139680=CARTESIAN_POINT('Ctrl Pts',(2.88882454346608,4.26143250097105,6.92306100863517));
#139681=CARTESIAN_POINT('Ctrl Pts',(2.74443323190568,4.23689343088443,6.98158002910692));
#139682=CARTESIAN_POINT('Ctrl Pts',(2.59797890375575,4.21216499285672,7.03565957218225));
#139683=CARTESIAN_POINT('Ctrl Pts',(2.51023120678092,4.17289950702997,6.80156153618877));
#139684=CARTESIAN_POINT('Ctrl Pts',(2.52479861929105,4.17977820199321,6.84053300412659));
#139685=CARTESIAN_POINT('Ctrl Pts',(2.53940392922748,4.18648410044078,6.8795485839286));
#139686=CARTESIAN_POINT('Ctrl Pts',(2.56864919216302,4.19956141145792,6.95756770310241));
#139687=CARTESIAN_POINT('Ctrl Pts',(2.58330634398361,4.20594050663845,6.99661711845852));
#139688=CARTESIAN_POINT('Ctrl Pts',(2.59797889080986,4.21216499502226,7.03565957683809));
#139689=CARTESIAN_POINT('Ctrl Pts',(2.05635688783999,4.30331728230629,7.21259051257531));
#139690=CARTESIAN_POINT('Ctrl Pts',(2.06024869641999,4.30267205415314,7.21147638828766));
#139691=CARTESIAN_POINT('Ctrl Pts',(2.064140505,4.302026826,7.210362264));
#139692=CARTESIAN_POINT('Ctrl Pts',(2.45456259,4.237298226,7.098594504));
#139693=CARTESIAN_POINT('Ctrl Pts',(2.830633507,4.172121859,6.945323171));
#139694=CARTESIAN_POINT('Ctrl Pts',(1.75808712366278,4.30331728230629,7.03361151287165));
#139695=CARTESIAN_POINT('Ctrl Pts',(1.76188250183139,4.30267205415314,7.03265848443582));
#139696=CARTESIAN_POINT('Ctrl Pts',(1.76567788,4.302026826,7.031705456));
#139697=CARTESIAN_POINT('Ctrl Pts',(2.146426169,4.237298226,6.93609866000001));
#139698=CARTESIAN_POINT('Ctrl Pts',(2.514624883,4.172121859,6.79993836));
#139699=CARTESIAN_POINT('',(2.06414050352516,4.30202682545337,7.2103622664337));
#139700=CARTESIAN_POINT('Origin',(-0.073949683909128,4.16072875403252,-0.176399408683935));
#139701=CARTESIAN_POINT('',(1.91490918273179,4.30202682438524,7.12103386262676));
#139702=CARTESIAN_POINT('Origin',(5.20417042793042E-15,4.39277644300089,
1.95156391047391E-14));
#139703=CARTESIAN_POINT('',(2.60309509487783,4.39169923735874,7.03376825908966));
#139704=CARTESIAN_POINT('Origin',(-0.0975371601152519,4.16082466558289,
-0.158646804130117));
#139705=CARTESIAN_POINT('Origin',(-0.0876193823186891,4.55341984404931,
-0.162522029489007));
#139706=CARTESIAN_POINT('Ctrl Pts',(0.774406033,4.172114527,7.45991255300001));
#139707=CARTESIAN_POINT('Ctrl Pts',(1.132374232,4.22940039,7.422752234));
#139708=CARTESIAN_POINT('Ctrl Pts',(1.485139566,4.285714286,7.351486956));
#139709=CARTESIAN_POINT('Ctrl Pts',(1.536154289,4.29385805,7.341181016));
#139710=CARTESIAN_POINT('Ctrl Pts',(1.587021072,4.302026826,7.330168082));
#139711=CARTESIAN_POINT('Ctrl Pts',(0.984685745,4.172114527,7.182819362));
#139712=CARTESIAN_POINT('Ctrl Pts',(1.329357467,4.22940039,7.135568649));
#139713=CARTESIAN_POINT('Ctrl Pts',(1.667921256,4.285714286,7.055532488));
#139714=CARTESIAN_POINT('Ctrl Pts',(1.71688224,4.29385805,7.043958157));
#139715=CARTESIAN_POINT('Ctrl Pts',(1.76567788,4.302026826,7.031705456));
#139716=CARTESIAN_POINT('',(1.58702106594486,4.30202682620655,7.33016808366913));
#139717=CARTESIAN_POINT('',(1.67634947204994,4.30202682665757,7.18093676992212));
#139718=CARTESIAN_POINT('',(1.02478075832104,4.21216499529598,7.42965843030395));
#139719=CARTESIAN_POINT('Ctrl Pts',(1.58702106529163,4.3020268248974,7.33016808322337));
#139720=CARTESIAN_POINT('Ctrl Pts',(1.55308500096568,4.29657697940857,7.33751542487662));
#139721=CARTESIAN_POINT('Ctrl Pts',(1.51912281074809,4.29113922035362,7.34462169677195));
#139722=CARTESIAN_POINT('Ctrl Pts',(1.48513956610293,4.28571428598436,7.35148695569453));
#139723=CARTESIAN_POINT('Ctrl Pts',(1.33303195779561,4.26143250089043,7.38221557329729));
#139724=CARTESIAN_POINT('Ctrl Pts',(1.1794365756078,4.23689343225755,7.40832658749199));
#139725=CARTESIAN_POINT('Ctrl Pts',(1.02478076449991,4.21216499697171,7.42965842910681));
#139726=CARTESIAN_POINT('Ctrl Pts',(0.989408718343246,4.17289950709276,
7.18217031486416));
#139727=CARTESIAN_POINT('Ctrl Pts',(0.995257839240748,4.17977820203178,
7.22336221448962));
#139728=CARTESIAN_POINT('Ctrl Pts',(1.00113448880787,4.18648410043884,7.26460534140605));
#139729=CARTESIAN_POINT('Ctrl Pts',(1.01292420948285,4.19956141142547,7.34708728384108));
#139730=CARTESIAN_POINT('Ctrl Pts',(1.01884421533533,4.20594050661628,7.38837460004229));
#139731=CARTESIAN_POINT('Ctrl Pts',(1.02478075181138,4.21216499499655,7.42965843128517));
#139732=CARTESIAN_POINT('Ctrl Pts',(0.457786649930205,4.30331728230629,
7.4860200997665));
#139733=CARTESIAN_POINT('Ctrl Pts',(0.461826973965103,4.30267205415314,
7.48576864688325));
#139734=CARTESIAN_POINT('Ctrl Pts',(0.465867298,4.302026826,7.485517194));
#139735=CARTESIAN_POINT('Ctrl Pts',(0.871188295,4.237298226,7.460291709));
#139736=CARTESIAN_POINT('Ctrl Pts',(1.271415689,4.172121859,7.391447906));
#139737=CARTESIAN_POINT('Ctrl Pts',(0.20496545941525,4.30331728230629,7.24710634709099));
#139738=CARTESIAN_POINT('Ctrl Pts',(0.208876976707625,4.30267205415314,
7.24699149404549));
#139739=CARTESIAN_POINT('Ctrl Pts',(0.212788494,4.302026826,7.246876641));
#139740=CARTESIAN_POINT('Ctrl Pts',(0.605187736,4.237298226,7.235354706));
#139741=CARTESIAN_POINT('Ctrl Pts',(0.994048608,4.172121859,7.181529598));
#139742=CARTESIAN_POINT('',(0.465867296042565,4.30202682545335,7.48551719606147));
#139743=CARTESIAN_POINT('Origin',(-0.0343001461811986,4.16072877971437,
-0.188172529920452));
#139744=CARTESIAN_POINT('',(0.33932788589549,4.30202682438524,7.36619691796547));
#139745=CARTESIAN_POINT('Origin',(-7.7005459300783E-14,4.392776443,-7.73686670285656E-13));
#139746=CARTESIAN_POINT('',(1.03018391903457,4.39169923738309,7.42891116439695));
#139747=CARTESIAN_POINT('Origin',(-0.0611523990539982,4.16082467447941,
-0.175905147910012));
#139748=CARTESIAN_POINT('Origin',(-0.0506334197676744,4.55341979579773,
-0.177557643365398));
#139749=CARTESIAN_POINT('Origin',(-8.63194335887912E-14,4.39277644299978,
1.0547118733939E-12));
#139750=CARTESIAN_POINT('',(-0.0258520642580682,4.30202682641445,7.49995544522258));
#139751=CARTESIAN_POINT('Ctrl Pts',(-0.0258520649115978,4.30202682552111,
7.49995544458365));
#139752=CARTESIAN_POINT('Ctrl Pts',(-0.0605741846835186,4.29657697961046,
7.49983575874007));
#139753=CARTESIAN_POINT('Ctrl Pts',(-0.0952699962294244,4.29113922035365,
7.49947502299388));
#139754=CARTESIAN_POINT('Ctrl Pts',(-0.129934559142506,4.28571428571329,
7.49887438288844));
#139755=CARTESIAN_POINT('Ctrl Pts',(-0.28509171907091,4.26143250106465,
7.49618594244476));
#139756=CARTESIAN_POINT('Ctrl Pts',(-0.440709222886184,4.23689343175884,
7.48866802895951));
#139757=CARTESIAN_POINT('Ctrl Pts',(-0.596334981605774,4.21216499520884,
7.47625471674912));
#139758=CARTESIAN_POINT('',(-0.590897510512571,4.39169923729323,7.47668644066963));
#139759=CARTESIAN_POINT('Origin',(-0.0219082601953907,4.1608246528612,-0.18493894311418));
#139760=CARTESIAN_POINT('Origin',(-0.0112799649723951,4.55341977946789,
-0.184291312800935));
#139761=CARTESIAN_POINT('Ctrl Pts',(-0.847359835,4.172114527,7.451978349));
#139762=CARTESIAN_POINT('Ctrl Pts',(-0.489772364,4.22940039,7.492639398));
#139763=CARTESIAN_POINT('Ctrl Pts',(-0.129934559,4.285714286,7.498874383));
#139764=CARTESIAN_POINT('Ctrl Pts',(-0.07789706,4.29385805,7.499776047));
#139765=CARTESIAN_POINT('Ctrl Pts',(-0.025852058,4.302026826,7.499955445));
#139766=CARTESIAN_POINT('Ctrl Pts',(-0.582429501,4.172114527,7.226567365));
#139767=CARTESIAN_POINT('Ctrl Pts',(-0.235658505,4.22940039,7.25451558));
#139768=CARTESIAN_POINT('Ctrl Pts',(0.112195259,4.285714286,7.249131826));
#139769=CARTESIAN_POINT('Ctrl Pts',(0.162499702,4.29385805,7.248353261));
#139770=CARTESIAN_POINT('Ctrl Pts',(0.212788494,4.302026826,7.246876641));
#139771=CARTESIAN_POINT('',(0.0946614167047613,4.30202682665757,7.37215064903207));
#139772=CARTESIAN_POINT('Ctrl Pts',(-0.0379316651699341,1.456406735,7.50043718252163));
#139773=CARTESIAN_POINT('Ctrl Pts',(0.373468759383251,1.522118786,7.50251774175917));
#139774=CARTESIAN_POINT('Ctrl Pts',(0.782628730039567,1.586734015,7.45959040487358));
#139775=CARTESIAN_POINT('Ctrl Pts',(0.796789298954691,1.58897027579979,
7.4581047377607));
#139776=CARTESIAN_POINT('Ctrl Pts',(0.810949867869816,1.59120653659958,
7.45661907064781));
#139777=CARTESIAN_POINT('Ctrl Pts',(0.201601146,1.456406735,7.247196491));
#139778=CARTESIAN_POINT('Ctrl Pts',(0.59911127,1.522118786,7.236138629));
#139779=CARTESIAN_POINT('Ctrl Pts',(0.993027301999999,1.586734015,7.18167089));
#139780=CARTESIAN_POINT('Ctrl Pts',(1.00666029524947,1.58897027579979,7.17978582247854));
#139781=CARTESIAN_POINT('Ctrl Pts',(1.02029328849892,1.59120653659958,7.17790075495718));
#139782=CARTESIAN_POINT('',(0.206355417658743,1.45719264060538,7.24706267593716));
#139783=CARTESIAN_POINT('Origin',(0.0140775383922631,1.3393957313777,-0.192312383039513));
#139784=CARTESIAN_POINT('Ctrl Pts',(0.206355413361966,1.45719264074914,
7.24706267701225));
#139785=CARTESIAN_POINT('Ctrl Pts',(0.207635378906658,1.46408307495124,
7.28864821236279));
#139786=CARTESIAN_POINT('Ctrl Pts',(0.208937534794803,1.47080219913258,
7.33028717574197));
#139787=CARTESIAN_POINT('Ctrl Pts',(0.211579281208753,1.48390865064158,
7.41356511687401));
#139788=CARTESIAN_POINT('Ctrl Pts',(0.212920408593059,1.49030358392773,
7.45525246629562));
#139789=CARTESIAN_POINT('Ctrl Pts',(0.21427864176539,1.49654505838725,7.49693835245978));
#139790=CARTESIAN_POINT('Ctrl Pts',(1.270364528,1.586734015,7.391628641));
#139791=CARTESIAN_POINT('Ctrl Pts',(1.67128584,1.521690237,7.322724176));
#139792=CARTESIAN_POINT('Ctrl Pts',(2.062402258,1.456414446,7.210859652));
#139793=CARTESIAN_POINT('Ctrl Pts',(0.993027302,1.586734015,7.18167089));
#139794=CARTESIAN_POINT('Ctrl Pts',(1.382560524,1.521690237,7.127809173));
#139795=CARTESIAN_POINT('Ctrl Pts',(1.763982709,1.456414446,7.032130901));
#139796=CARTESIAN_POINT('',(1.7594351956975,1.45719264061351,7.03327006337353));
#139797=CARTESIAN_POINT('Origin',(-0.0443700637135178,1.48214301195865,
-0.194387020949511));
#139798=CARTESIAN_POINT('Ctrl Pts',(1.82088906445054,1.49654505841197,7.27560052582954));
#139799=CARTESIAN_POINT('Ctrl Pts',(1.81060137241627,1.49030359595976,7.23518129027469));
#139800=CARTESIAN_POINT('Ctrl Pts',(1.80033004124374,1.48390865652201,7.19475682903767));
#139801=CARTESIAN_POINT('Ctrl Pts',(1.77984774251394,1.47080219290275,7.11399370280525));
#139802=CARTESIAN_POINT('Ctrl Pts',(1.76962488919469,1.4640830719819,7.07360818143262));
#139803=CARTESIAN_POINT('Ctrl Pts',(1.75943519192526,1.45719264079878,7.03327006541419));
#139804=CARTESIAN_POINT('Ctrl Pts',(1.57532743863952,1.456406735,7.33323531634185));
#139805=CARTESIAN_POINT('Ctrl Pts',(1.97755680933516,1.522118786,7.24682830281802));
#139806=CARTESIAN_POINT('Ctrl Pts',(2.36792273908022,1.586734015,7.11694728376987));
#139807=CARTESIAN_POINT('Ctrl Pts',(2.38143286751847,1.58897027584229,7.11245224689466));
#139808=CARTESIAN_POINT('Ctrl Pts',(2.39494299595673,1.59120653668464,7.10795721001934));
#139809=CARTESIAN_POINT('Ctrl Pts',(1.754820843,1.456406735,7.034422777));
#139810=CARTESIAN_POINT('Ctrl Pts',(2.140660288,1.522118786,6.938170516));
#139811=CARTESIAN_POINT('Ctrl Pts',(2.513657828,1.586734015,6.8002959));
#139812=CARTESIAN_POINT('Ctrl Pts',(2.5265668558853,1.58897027584229,6.79552421367031));
#139813=CARTESIAN_POINT('Ctrl Pts',(2.53947588377066,1.59120653668465,6.79075252734073));
#139814=CARTESIAN_POINT('Origin',(-0.0275930671526198,1.3393957380865,-0.190842484788214));
#139815=CARTESIAN_POINT('Ctrl Pts',(2.829645774,1.586734015,6.94572564900001));
#139816=CARTESIAN_POINT('Ctrl Pts',(3.206381346,1.521690237,6.792245902));
#139817=CARTESIAN_POINT('Ctrl Pts',(3.564306113,1.456414446,6.59891824));
#139818=CARTESIAN_POINT('Ctrl Pts',(2.513657828,1.586734015,6.80029590000001));
#139819=CARTESIAN_POINT('Ctrl Pts',(2.882505303,1.521690237,6.663955312));
#139820=CARTESIAN_POINT('Ctrl Pts',(3.234442049,1.456414446,6.488519448));
#139821=CARTESIAN_POINT('',(3.23024574016728,1.45719264061225,6.4906095589037));
#139822=CARTESIAN_POINT('Origin',(-0.0851200586044626,1.4821430323664,-0.180303803708292));
#139823=CARTESIAN_POINT('Ctrl Pts',(3.34235673751931,1.49654505837742,6.71406370518684));
#139824=CARTESIAN_POINT('Ctrl Pts',(3.32362058915717,1.49030358391892,6.67680092687681));
#139825=CARTESIAN_POINT('Ctrl Pts',(3.30489935139105,1.48390865070044,6.63952963836113));
#139826=CARTESIAN_POINT('Ctrl Pts',(3.26753424118067,1.47080218999584,6.56505781410445));
#139827=CARTESIAN_POINT('Ctrl Pts',(3.248868703834,1.46408307057618,6.52781410369618));
#139828=CARTESIAN_POINT('Ctrl Pts',(3.23024573750669,1.45719264080038,6.49060956132151));
#139829=CARTESIAN_POINT('Ctrl Pts',(3.11492598304595,1.456406735,6.82313951611896));
#139830=CARTESIAN_POINT('Ctrl Pts',(3.48917650019526,1.522118786,6.65228522632019));
#139831=CARTESIAN_POINT('Ctrl Pts',(3.84249531148225,1.586734015,6.4415236179946));
#139832=CARTESIAN_POINT('Ctrl Pts',(3.85472328050915,1.58897027583195,6.43422939437467));
#139833=CARTESIAN_POINT('Ctrl Pts',(3.86695124953596,1.59120653666397,6.4269351707547));
#139834=CARTESIAN_POINT('Ctrl Pts',(3.225987068,1.456406735,6.492727273));
#139835=CARTESIAN_POINT('Ctrl Pts',(3.58211441,1.522118786,6.31578126));
#139836=CARTESIAN_POINT('Ctrl Pts',(3.916752508,1.586734015,6.100946631));
#139837=CARTESIAN_POINT('Ctrl Pts',(3.92833395842618,1.58897027583195,6.09351144468842));
#139838=CARTESIAN_POINT('Ctrl Pts',(3.93991540885235,1.59120653666397,6.08607625837668));
#139839=CARTESIAN_POINT('Origin',(-0.0679733892134116,1.33939578365377,
-0.18044889177114));
#139840=CARTESIAN_POINT('Ctrl Pts',(4.256615929,1.586734015,6.175048246));
#139841=CARTESIAN_POINT('Ctrl Pts',(4.591550023,1.521690237,5.94416975800001));
#139842=CARTESIAN_POINT('Ctrl Pts',(4.899546976,1.456414446,5.678418744));
#139843=CARTESIAN_POINT('Ctrl Pts',(3.916752508,1.586734015,6.10094663100001));
#139844=CARTESIAN_POINT('Ctrl Pts',(4.247667337,1.521690237,5.888502306));
#139845=CARTESIAN_POINT('Ctrl Pts',(4.553662473,1.456414446,5.641512038));
#139846=CARTESIAN_POINT('',(4.55001358390391,1.45719264061043,5.64445536527957));
#139847=CARTESIAN_POINT('Origin',(-0.121890082462435,1.48214305403045,-0.157790240855409));
#139848=CARTESIAN_POINT('Ctrl Pts',(4.70753952467976,1.49654505838546,5.83858472753936));
#139849=CARTESIAN_POINT('Ctrl Pts',(4.68123102122198,1.49030358392642,5.80622085031352));
#139850=CARTESIAN_POINT('Ctrl Pts',(4.65493525026563,1.4839086506962,5.77384545647786));
#139851=CARTESIAN_POINT('Ctrl Pts',(4.60243447779945,1.47080219076287,5.70914714015477));
#139852=CARTESIAN_POINT('Ctrl Pts',(4.57619903173408,1.46408307092509,5.67678670369149));
#139853=CARTESIAN_POINT('Ctrl Pts',(4.55001358156978,1.45719264075695,5.64445536838016));
#139854=CARTESIAN_POINT('Ctrl Pts',(4.50887404986767,1.456406735,5.99400129611256));
#139855=CARTESIAN_POINT('Ctrl Pts',(4.8376461759817,1.522118786,5.74668868624035));
#139856=CARTESIAN_POINT('Ctrl Pts',(5.13739707470347,1.586734015,5.46490146661415));
#139857=CARTESIAN_POINT('Ctrl Pts',(5.14777111805187,1.58897027580677,5.45514912610781));
#139858=CARTESIAN_POINT('Ctrl Pts',(5.15814516140012,1.59120653661362,5.44539678560135));
#139859=CARTESIAN_POINT('Ctrl Pts',(4.546309723,1.456406735,5.647439057));
#139860=CARTESIAN_POINT('Ctrl Pts',(4.856072844,1.522118786,5.39807309299999));
#139861=CARTESIAN_POINT('Ctrl Pts',(5.136704194,1.586734015,5.116323878));
#139862=CARTESIAN_POINT('Ctrl Pts',(5.14641653115139,1.58897027580677,5.10657285279125));
#139863=CARTESIAN_POINT('Ctrl Pts',(5.15612886830264,1.59120653661362,5.0968218275825));
#139864=CARTESIAN_POINT('Origin',(-0.105175429545894,1.33939576646129,-0.161617879589773));
#139865=CARTESIAN_POINT('Ctrl Pts',(5.484551453,1.586734015,5.115632449));
#139866=CARTESIAN_POINT('Ctrl Pts',(5.762022925,1.521690237,4.818150842));
#139867=CARTESIAN_POINT('Ctrl Pts',(6.005690467,1.456414446,4.492402699));
#139868=CARTESIAN_POINT('Ctrl Pts',(5.136704194,1.586734015,5.11632387800001));
#139869=CARTESIAN_POINT('Ctrl Pts',(5.414213168,1.521690237,4.837709477));
#139870=CARTESIAN_POINT('Ctrl Pts',(5.659958701,1.456414446,4.530713796));
#139871=CARTESIAN_POINT('',(5.65702784900627,1.4571926405954,4.53437271261321));
#139872=CARTESIAN_POINT('Origin',(-0.152960641359311,1.48214303826057,-0.127898470071886));
#139873=CARTESIAN_POINT('Ctrl Pts',(5.85260299563806,1.49654505844387,4.69010001717245));
#139874=CARTESIAN_POINT('Ctrl Pts',(5.81995229347557,1.49030358399253,4.66414834014743));
#139875=CARTESIAN_POINT('Ctrl Pts',(5.7873115502117,1.48390865073091,4.6381826785139));
#139876=CARTESIAN_POINT('Ctrl Pts',(5.72213000906081,1.47080219440202,4.58628310167367));
#139877=CARTESIAN_POINT('Ctrl Pts',(5.68955138599843,1.46408307265874,4.56031907194432));
#139878=CARTESIAN_POINT('Ctrl Pts',(5.65702784741049,1.45719264071491,4.53437271658464));
#139879=CARTESIAN_POINT('Ctrl Pts',(5.69199217717728,1.456406735,4.88459023813095));
#139880=CARTESIAN_POINT('Ctrl Pts',(5.95991289298511,1.522118786,4.57238337002368));
#139881=CARTESIAN_POINT('Ctrl Pts',(6.192079860037,1.586734015,4.23274659681978));
#139882=CARTESIAN_POINT('Ctrl Pts',(6.2001148988587,1.58897027573975,4.22099214831824));
#139883=CARTESIAN_POINT('Ctrl Pts',(6.20814993768041,1.59120653647956,4.20923769981674));
#139884=CARTESIAN_POINT('Ctrl Pts',(5.654051988,1.456406735,4.538082868));
#139885=CARTESIAN_POINT('Ctrl Pts',(5.902966708,1.522118786,4.227957027));
#139886=CARTESIAN_POINT('Ctrl Pts',(6.116469301,1.586734015,3.892467507));
#139887=CARTESIAN_POINT('Ctrl Pts',(6.12385838673028,1.58897027573975,3.88085659028905));
#139888=CARTESIAN_POINT('Ctrl Pts',(6.13124747246068,1.59120653647956,3.86924567357812));
#139889=CARTESIAN_POINT('Origin',(-0.13745956902366,1.33939578570686,-0.135229751280372));
#139890=CARTESIAN_POINT('Ctrl Pts',(6.456035448,1.586734015,3.817015365));
#139891=CARTESIAN_POINT('Ctrl Pts',(6.663070038,1.521690237,3.466840548));
#139892=CARTESIAN_POINT('Ctrl Pts',(6.831014547,1.456414446,3.096326897));
#139893=CARTESIAN_POINT('Ctrl Pts',(6.116469301,1.586734015,3.892467507));
#139894=CARTESIAN_POINT('Ctrl Pts',(6.32759640899999,1.521690237,3.560710729));
#139895=CARTESIAN_POINT('Ctrl Pts',(6.501601551,1.456414446,3.208064411));
#139896=CARTESIAN_POINT('',(6.49952578032314,1.45719264059455,3.21226783095441));
#139897=CARTESIAN_POINT('Origin',(-0.176878902021876,1.48214302079141,-0.0920262527007942));
#139898=CARTESIAN_POINT('Ctrl Pts',(6.72400525554584,1.4965450583912,3.32231144235511));
#139899=CARTESIAN_POINT('Ctrl Pts',(6.68653913777695,1.49030359603181,3.30398547236691));
#139900=CARTESIAN_POINT('Ctrl Pts',(6.64907962791025,1.48390865650943,3.28564364915465));
#139901=CARTESIAN_POINT('Ctrl Pts',(6.57426505880495,1.4708021894492,3.24896952995088));
#139902=CARTESIAN_POINT('Ctrl Pts',(6.5368666223405,1.46408307028397,3.23061597316369));
#139903=CARTESIAN_POINT('Ctrl Pts',(6.49952577957866,1.45719264073368,3.21226783479966));
#139904=CARTESIAN_POINT('Ctrl Pts',(6.60895907756974,1.456406735,3.54678116859748));
#139905=CARTESIAN_POINT('Ctrl Pts',(6.80350070809704,1.522118786,3.1842784891296));
#139906=CARTESIAN_POINT('Ctrl Pts',(6.95722787297183,1.586734015,2.80267320064594));
#139907=CARTESIAN_POINT('Ctrl Pts',(6.96254819814243,1.58897027577753,2.78946626859066));
#139908=CARTESIAN_POINT('Ctrl Pts',(6.96786852331302,1.59120653655514,2.77625933653536));
#139909=CARTESIAN_POINT('Ctrl Pts',(6.497417067,1.456406735,3.216530967));
#139910=CARTESIAN_POINT('Ctrl Pts',(6.67384440999999,1.522118786,2.860146389));
#139911=CARTESIAN_POINT('Ctrl Pts',(6.810235101,1.586734015,2.486603681));
#139912=CARTESIAN_POINT('Ctrl Pts',(6.81495543020762,1.58897027577753,2.47367578583401));
#139913=CARTESIAN_POINT('Ctrl Pts',(6.81967575941525,1.59120653655514,2.46074789066802));
#139914=CARTESIAN_POINT('Origin',(-0.163316158578842,1.33939575347006,-0.102518366935395));
#139915=CARTESIAN_POINT('Ctrl Pts',(7.12564240000001,1.586734015,2.339918885));
#139916=CARTESIAN_POINT('Ctrl Pts',(7.252559402,1.521690237,1.953424644));
#139917=CARTESIAN_POINT('Ctrl Pts',(7.336927979,1.456414446,1.555470291));
#139918=CARTESIAN_POINT('Ctrl Pts',(6.81023510100001,1.586734015,2.486603681));
#139919=CARTESIAN_POINT('Ctrl Pts',(6.945108274,1.521690237,2.117217106));
#139920=CARTESIAN_POINT('Ctrl Pts',(7.039236739,1.456414446,1.7354095));
#139921=CARTESIAN_POINT('',(7.03811310899877,1.45719264060774,1.73996087620211));
#139922=CARTESIAN_POINT('Origin',(-0.192526489986935,1.48214308462136,-0.0518510129485178));
#139923=CARTESIAN_POINT('Ctrl Pts',(7.28100050240532,1.49654505835033,1.79917527769442));
#139924=CARTESIAN_POINT('Ctrl Pts',(7.24047070142308,1.4903035839255,1.78933184746777));
#139925=CARTESIAN_POINT('Ctrl Pts',(7.1999440667875,1.48390865067248,1.77947154348188));
#139926=CARTESIAN_POINT('Ctrl Pts',(7.11899482593458,1.47080219282059,1.75973777943903));
#139927=CARTESIAN_POINT('Ctrl Pts',(7.07852526065664,1.46408307191996,1.74985287418798));
#139928=CARTESIAN_POINT('Ctrl Pts',(7.03811310915023,1.45719264076508,1.73996088015336));
#139929=CARTESIAN_POINT('Ctrl Pts',(7.21689839543718,1.456406735,2.04312855315931));
#139930=CARTESIAN_POINT('Ctrl Pts',(7.32896439106467,1.522118786,1.6472802857093));
#139931=CARTESIAN_POINT('Ctrl Pts',(7.39706364334694,1.586734015,1.24154991981414));
#139932=CARTESIAN_POINT('Ctrl Pts',(7.39942048232618,1.58897027582894,1.22750804550049));
#139933=CARTESIAN_POINT('Ctrl Pts',(7.40177732130554,1.59120653665793,1.21346617118682));
#139934=CARTESIAN_POINT('Ctrl Pts',(7.036970144,1.456406735,1.744577653));
#139935=CARTESIAN_POINT('Ctrl Pts',(7.132660565,1.522118786,1.358598485));
#139936=CARTESIAN_POINT('Ctrl Pts',(7.185561877,1.586734015,0.964469032));
#139937=CARTESIAN_POINT('Ctrl Pts',(7.187392732259,1.58897027582894,0.950828652310581));
#139938=CARTESIAN_POINT('Ctrl Pts',(7.18922358751792,1.59120653665794,0.937188272621161));
#139939=CARTESIAN_POINT('Origin',(-0.181536210942589,1.33939575825133,-0.0650133800666799));
#139940=CARTESIAN_POINT('Ctrl Pts',(7.462062233,1.586734015,0.753410398000001));
#139941=CARTESIAN_POINT('Ctrl Pts',(7.502927149,1.521690237,0.348668774));
#139942=CARTESIAN_POINT('Ctrl Pts',(7.49977481399999,1.456414446,-0.058118378));
#139943=CARTESIAN_POINT('Ctrl Pts',(7.18556187700001,1.586734015,0.964469032000001));
#139944=CARTESIAN_POINT('Ctrl Pts',(7.237874596,1.521690237,0.574724763));
#139945=CARTESIAN_POINT('Ctrl Pts',(7.24772504,1.456414446,0.18160877));
#139946=CARTESIAN_POINT('',(7.24760609128638,1.45719264059485,0.186295284537503));
#139947=CARTESIAN_POINT('Origin',(-0.199171610313214,1.48214301715221,-0.00925123469859398));
#139948=CARTESIAN_POINT('Ctrl Pts',(7.49754425842133,1.49654505839625,0.191911676403582));
#139949=CARTESIAN_POINT('Ctrl Pts',(7.45584597507916,1.49030358395697,0.191011089299526));
#139950=CARTESIAN_POINT('Ctrl Pts',(7.41414715678101,1.48390865070444,0.19009334226442));
#139951=CARTESIAN_POINT('Ctrl Pts',(7.33084828706449,1.47080219265943,0.188222636638891));
#139952=CARTESIAN_POINT('Ctrl Pts',(7.28919991587746,1.46408307184296,0.187268595286479));
#139953=CARTESIAN_POINT('Ctrl Pts',(7.247606092197,1.4571926407666,0.18629528861405));
#139954=CARTESIAN_POINT('Ctrl Pts',(7.48710214575945,1.456406735,0.443644859291493));
#139955=CARTESIAN_POINT('Ctrl Pts',(7.51143615240203,1.522118786,0.0329758636742104));
#139956=CARTESIAN_POINT('Ctrl Pts',(7.49070876024206,1.586734015,-0.377890955082889));
#139957=CARTESIAN_POINT('Ctrl Pts',(7.49039304717479,1.58771821368654,-0.384149148230609));
#139958=CARTESIAN_POINT('Ctrl Pts',(7.49007733410756,1.58870241237309,-0.390407341378328));
#139959=CARTESIAN_POINT('Ctrl Pts',(7.247482319,1.456406735,0.191049828));
#139960=CARTESIAN_POINT('Ctrl Pts',(7.257961439,1.522118786,-0.206475974));
#139961=CARTESIAN_POINT('Ctrl Pts',(7.224899766,1.586734015,-0.602763118));
#139962=CARTESIAN_POINT('Ctrl Pts',(7.22439618107668,1.58771821368654,-0.60879923816325));
#139963=CARTESIAN_POINT('Ctrl Pts',(7.22389259615334,1.58870241237309,-0.6148353583265));
#139964=CARTESIAN_POINT('Origin',(-0.191268234113869,1.33939575786211,-0.0244684761353829));
#139965=CARTESIAN_POINT('Ctrl Pts',(7.44956433,1.586734015,-0.868326722));
#139966=CARTESIAN_POINT('Ctrl Pts',(7.402466362,1.521690237,-1.272390461));
#139967=CARTESIAN_POINT('Ctrl Pts',(7.311940513,1.456414446,-1.668989496));
#139968=CARTESIAN_POINT('Ctrl Pts',(7.224899766,1.586734015,-0.602763118000001));
#139969=CARTESIAN_POINT('Ctrl Pts',(7.192205945,1.521690237,-0.994641069999999));
#139970=CARTESIAN_POINT('Ctrl Pts',(7.117317773,1.456414446,-1.380683784));
#139971=CARTESIAN_POINT('',(7.11820906753265,1.4571926405863,-1.37608126762224));
#139972=CARTESIAN_POINT('Origin',(-0.19650394698959,1.48214304210119,0.0337810818111164));
#139973=CARTESIAN_POINT('Ctrl Pts',(7.36351117761109,1.49654505842827,-1.4243255016041));
#139974=CARTESIAN_POINT('Ctrl Pts',(7.32259417719388,1.490303583954,-1.41624113518447));
#139975=CARTESIAN_POINT('Ctrl Pts',(7.28167296572904,1.48390865070893,-1.40817341256504));
#139976=CARTESIAN_POINT('Ctrl Pts',(7.19991942750816,1.47080219210175,-1.39209358688636));
#139977=CARTESIAN_POINT('Ctrl Pts',(7.15903968301798,1.46408307152146,-1.38407215495896));
#139978=CARTESIAN_POINT('Ctrl Pts',(7.11820906898563,1.45719264066128,-1.37608126395452));
#139979=CARTESIAN_POINT('Ctrl Pts',(7.40776700316167,1.456406735,-1.17600372880381));
#139980=CARTESIAN_POINT('Ctrl Pts',(7.34326297149683,1.522118786,-1.58232117638735));
#139981=CARTESIAN_POINT('Ctrl Pts',(7.23470641998929,1.586734015,-1.97914621804622));
#139982=CARTESIAN_POINT('Ctrl Pts',(7.23094939922131,1.58897027576831,-1.99287988867284));
#139983=CARTESIAN_POINT('Ctrl Pts',(7.22719237845333,1.59120653653669,-2.00661355929947));
#139984=CARTESIAN_POINT('Ctrl Pts',(7.119110275,1.456406735,-1.371411276));
#139985=CARTESIAN_POINT('Ctrl Pts',(7.043888103,1.522118786,-1.761895846));
#139986=CARTESIAN_POINT('Ctrl Pts',(6.926409371,1.586734015,-2.141810735));
#139987=CARTESIAN_POINT('Ctrl Pts',(6.92234356354949,1.58897027576831,-2.15495916416633));
#139988=CARTESIAN_POINT('Ctrl Pts',(6.91827775609913,1.59120653653669,-2.16810759333264));
#139989=CARTESIAN_POINT('Origin',(-0.192056303861984,1.33939579070899,0.0172205636933778));
#139990=CARTESIAN_POINT('Ctrl Pts',(7.088733078,1.586734015,-2.449461849));
#139991=CARTESIAN_POINT('Ctrl Pts',(6.955874475,1.521690237,-2.833954131));
#139992=CARTESIAN_POINT('Ctrl Pts',(6.782208,1.456414446,-3.20182052));
#139993=CARTESIAN_POINT('Ctrl Pts',(6.92640937100001,1.586734015,-2.141810735));
#139994=CARTESIAN_POINT('Ctrl Pts',(6.810237738,1.521690237,-2.517498593));
#139995=CARTESIAN_POINT('Ctrl Pts',(6.654112638,1.456414446,-2.8784171));
#139996=CARTESIAN_POINT('',(6.65597249932013,1.45719264060419,-2.8741137892278));
#139997=CARTESIAN_POINT('Origin',(-0.184647872090671,1.48214305780332,0.0752338312691325));
#139998=CARTESIAN_POINT('Ctrl Pts',(6.88516849829515,1.4965450584155,-2.97396280252883));
#139999=CARTESIAN_POINT('Ctrl Pts',(6.84694601453562,1.49030358397952,-2.95727149861205));
#140000=CARTESIAN_POINT('Ctrl Pts',(6.80871583992957,1.48390865071542,-2.94059554396094));
#140001=CARTESIAN_POINT('Ctrl Pts',(6.73233034632222,1.47080219300501,-2.90731706378751));
#140002=CARTESIAN_POINT('Ctrl Pts',(6.69413071574009,1.46408307201041,-2.8906952306549));
#140003=CARTESIAN_POINT('Ctrl Pts',(6.65597250201484,1.457192640761,-2.87411378614891));
#140004=CARTESIAN_POINT('Ctrl Pts',(6.98177148812184,1.456406735,-2.74096034957496));
#140005=CARTESIAN_POINT('Ctrl Pts',(6.83142928431654,1.522118786,-3.12391186004801));
#140006=CARTESIAN_POINT('Ctrl Pts',(6.64010507143633,1.586734015,-3.48812290292871));
#140007=CARTESIAN_POINT('Ctrl Pts',(6.63348355470157,1.58897027571003,-3.50072783922566));
#140008=CARTESIAN_POINT('Ctrl Pts',(6.62686203796677,1.59120653642013,-3.51333277552261));
#140009=CARTESIAN_POINT('Ctrl Pts',(6.657856548,1.456406735,-2.869746712));
#140010=CARTESIAN_POINT('Ctrl Pts',(6.500450388,1.522118786,-3.234931426));
#140011=CARTESIAN_POINT('Ctrl Pts',(6.304047773,1.586734015,-3.580709661));
#140012=CARTESIAN_POINT('Ctrl Pts',(6.29725049845539,1.58897027571003,-3.59267665845998));
#140013=CARTESIAN_POINT('Ctrl Pts',(6.29045322391093,1.59120653642013,-3.60464365591992));
#140014=CARTESIAN_POINT('Origin',(-0.183864365343379,1.33939572752096,0.0581044355765459));
#140015=CARTESIAN_POINT('Ctrl Pts',(6.396440546,1.586734015,-3.916062862));
#140016=CARTESIAN_POINT('Ctrl Pts',(6.184033628,1.521690237,-4.263005256));
#140017=CARTESIAN_POINT('Ctrl Pts',(5.93534698,1.456414446,-4.584937975));
#140018=CARTESIAN_POINT('Ctrl Pts',(6.304047773,1.586734015,-3.580709661));
#140019=CARTESIAN_POINT('Ctrl Pts',(6.109830384,1.521690237,-3.922640679));
#140020=CARTESIAN_POINT('Ctrl Pts',(5.879768591,1.456414446,-4.24155883));
#140021=CARTESIAN_POINT('',(5.88251005465644,1.45719264060703,-4.23775594375922));
#140022=CARTESIAN_POINT('Origin',(-0.16415770266568,1.48214305229595,0.113168649877636));
#140023=CARTESIAN_POINT('Ctrl Pts',(6.08488299206125,1.49654505834768,-4.38454090746793));
#140024=CARTESIAN_POINT('Ctrl Pts',(6.05114226559013,1.4903035838881,-4.36002313261337));
#140025=CARTESIAN_POINT('Ctrl Pts',(6.01739072882777,1.4839086506801,-4.3355186951666));
#140026=CARTESIAN_POINT('Ctrl Pts',(5.94994497315982,1.47080219260878,-4.28659762264575));
#140027=CARTESIAN_POINT('Ctrl Pts',(5.91621163238358,1.46408307180186,-4.26215260797914));
#140028=CARTESIAN_POINT('Ctrl Pts',(5.88251005761056,1.45719264073823,-4.23775594102181));
#140029=CARTESIAN_POINT('Ctrl Pts',(6.22931609688172,1.456406735,-4.17775270925097));
#140030=CARTESIAN_POINT('Ctrl Pts',(6.00016555589557,1.522118786,-4.51943189804365));
#140031=CARTESIAN_POINT('Ctrl Pts',(5.73501978812084,1.586734015,-4.83399883832595));
#140032=CARTESIAN_POINT('Ctrl Pts',(5.72584338958945,1.58897027582164,-4.84488564837412));
#140033=CARTESIAN_POINT('Ctrl Pts',(5.71666699105796,1.59120653664335,-4.85577245842213));
#140034=CARTESIAN_POINT('Ctrl Pts',(5.885288847,1.456406735,-4.233895981));
#140035=CARTESIAN_POINT('Ctrl Pts',(5.65305883699999,1.522118786,-4.556705209));
#140036=CARTESIAN_POINT('Ctrl Pts',(5.386915907,1.586734015,-4.852178584));
#140037=CARTESIAN_POINT('Ctrl Pts',(5.37770499779902,1.58897027582164,-4.86240458710454));
#140038=CARTESIAN_POINT('Ctrl Pts',(5.36849408859803,1.59120653664335,-4.87263059020909));
#140039=CARTESIAN_POINT('Origin',(-0.167074862435231,1.33939576027358,0.0962713050185793));
#140040=CARTESIAN_POINT('Ctrl Pts',(5.405057563,1.586734015,-5.199553129));
#140041=CARTESIAN_POINT('Ctrl Pts',(5.123034241,1.521690237,-5.492722994));
#140042=CARTESIAN_POINT('Ctrl Pts',(4.810955731,1.456414446,-5.753668826));
#140043=CARTESIAN_POINT('Ctrl Pts',(5.386915907,1.586734015,-4.852178584));
#140044=CARTESIAN_POINT('Ctrl Pts',(5.123734151,1.521690237,-5.14436444699999));
#140045=CARTESIAN_POINT('Ctrl Pts',(4.8304931,1.456414446,-5.406369984));
#140046=CARTESIAN_POINT('',(4.83398797806342,1.45719264060821,-5.40324534124832));
#140047=CARTESIAN_POINT('Origin',(-0.135991943969288,1.48214304425118,0.145811955775491));
#140048=CARTESIAN_POINT('Ctrl Pts',(5.00007512009465,1.49654505843161,-5.59010275334889));
#140049=CARTESIAN_POINT('Ctrl Pts',(4.97239382994859,1.49030358396498,-5.5589049316866));
#140050=CARTESIAN_POINT('Ctrl Pts',(4.94469911487078,1.48390865069507,-5.52771781147434));
#140051=CARTESIAN_POINT('Ctrl Pts',(4.88934677262698,1.47080218895167,-5.4654416255449));
#140052=CARTESIAN_POINT('Ctrl Pts',(4.86165706264628,1.46408307004702,-5.43431646029439));
#140053=CARTESIAN_POINT('Ctrl Pts',(4.83398798131907,1.4571926407418,-5.40324533969528));
#140054=CARTESIAN_POINT('Ctrl Pts',(5.18558480998957,1.456406735,-5.41919799617496));
#140055=CARTESIAN_POINT('Ctrl Pts',(4.88834075513256,1.522118786,-5.70362832263702));
#140056=CARTESIAN_POINT('Ctrl Pts',(4.56177135477614,1.586734015,-5.95384235976158));
#140057=CARTESIAN_POINT('Ctrl Pts',(4.55046915307313,1.5889702758084,-5.96250198774084));
#140058=CARTESIAN_POINT('Ctrl Pts',(4.53916695137025,1.59120653661686,-5.97116161572024));
#140059=CARTESIAN_POINT('Ctrl Pts',(4.837531582,1.456406735,-5.400072981));
#140060=CARTESIAN_POINT('Ctrl Pts',(4.541336538,1.522118786,-5.66541252));
#140061=CARTESIAN_POINT('Ctrl Pts',(4.21789784,1.586734015,-5.896765029));
#140062=CARTESIAN_POINT('Ctrl Pts',(4.20670398840411,1.5889702758084,-5.90477188058608));
#140063=CARTESIAN_POINT('Ctrl Pts',(4.19551013680818,1.59120653661686,-5.91277873217229));
#140064=CARTESIAN_POINT('Origin',(-0.142473359438439,1.33939579211148,0.129936838327164));
#140065=CARTESIAN_POINT('Ctrl Pts',(4.160940096,1.586734015,-6.23991807));
#140066=CARTESIAN_POINT('Ctrl Pts',(3.822487468,1.521690237,-6.465607109));
#140067=CARTESIAN_POINT('Ctrl Pts',(3.461609539,1.456414446,-6.653364517));
#140068=CARTESIAN_POINT('Ctrl Pts',(4.21789784,1.586734015,-5.896765029));
#140069=CARTESIAN_POINT('Ctrl Pts',(3.898057804,1.521690237,-6.125543451));
#140070=CARTESIAN_POINT('Ctrl Pts',(3.55534912,1.456414446,-6.318385287));
#140071=CARTESIAN_POINT('',(3.55943399578583,1.45719264062358,-6.31608499155558));
#140072=CARTESIAN_POINT('Origin',(-0.101467299577748,1.48214306600203,0.171637231264682));
#140073=CARTESIAN_POINT('Ctrl Pts',(3.68146929256206,1.49654505838464,-6.53427760732435));
#140074=CARTESIAN_POINT('Ctrl Pts',(3.66114178509383,1.49030358395292,-6.49785851436745));
#140075=CARTESIAN_POINT('Ctrl Pts',(3.6407988659998,1.48390865069154,-6.46144698653651));
#140076=CARTESIAN_POINT('Ctrl Pts',(3.60012817905484,1.47080219192019,-6.38872768207194));
#140077=CARTESIAN_POINT('Ctrl Pts',(3.57977682462906,1.46408307147985,-6.35237772768102));
#140078=CARTESIAN_POINT('Ctrl Pts',(3.55943399940581,1.45719264075089,-6.31608499035852));
#140079=CARTESIAN_POINT('Ctrl Pts',(3.89938133908589,1.456406735,-6.40724760846988));
#140080=CARTESIAN_POINT('Ctrl Pts',(3.54794257412965,1.522118786,-6.62112942631615));
#140081=CARTESIAN_POINT('Ctrl Pts',(3.17521956189425,1.586734015,-6.79529083046107));
#140082=CARTESIAN_POINT('Ctrl Pts',(3.16232003499673,1.58897027586157,-6.80131836201544));
#140083=CARTESIAN_POINT('Ctrl Pts',(3.14942050809924,1.59120653672322,-6.8073458935697));
#140084=CARTESIAN_POINT('Ctrl Pts',(3.563576716,1.456406735,-6.313748569));
#140085=CARTESIAN_POINT('Ctrl Pts',(3.21726639,1.522118786,-6.509211438));
#140086=CARTESIAN_POINT('Ctrl Pts',(2.851655559,1.586734015,-6.665625295));
#140087=CARTESIAN_POINT('Ctrl Pts',(2.83900217674645,1.58897027586157,-6.67103860378233));
#140088=CARTESIAN_POINT('Ctrl Pts',(2.82634879449291,1.59120653672321,-6.6764519125648));
#140089=CARTESIAN_POINT('Origin',(-0.111209903498641,1.33939578981825,0.157526672287099));
#140090=CARTESIAN_POINT('Ctrl Pts',(2.722261695,1.586734015,-6.988511377));
#140091=CARTESIAN_POINT('Ctrl Pts',(2.343205429,1.521690237,-7.136166621));
#140092=CARTESIAN_POINT('Ctrl Pts',(1.950402333,1.456414446,-7.241956279));
#140093=CARTESIAN_POINT('Ctrl Pts',(2.851655559,1.586734015,-6.665625295));
#140094=CARTESIAN_POINT('Ctrl Pts',(2.490112606,1.521690237,-6.820298851));
#140095=CARTESIAN_POINT('Ctrl Pts',(2.113960967,1.456414446,-6.934959915));
#140096=CARTESIAN_POINT('',(2.11844483589611,1.45719264061025,-6.93359152692528));
#140097=CARTESIAN_POINT('Origin',(-0.0621981411917949,1.48214301209216,
0.189437027024965));
#140098=CARTESIAN_POINT('Ctrl Pts',(2.19072205301252,1.49654505837123,-7.17291690241065));
#140099=CARTESIAN_POINT('Ctrl Pts',(2.17869881975251,1.49030358392898,-7.13297945426369));
#140100=CARTESIAN_POINT('Ctrl Pts',(2.16665890893221,1.48390865067593,-7.09304608144557));
#140101=CARTESIAN_POINT('Ctrl Pts',(2.14257158065369,1.47080219181767,-7.01328391782613));
#140102=CARTESIAN_POINT('Ctrl Pts',(2.13051019526033,1.4640830714041,-6.97340886569849));
#140103=CARTESIAN_POINT('Ctrl Pts',(2.11844483965137,1.45719264069612,-6.93359152644189));
#140104=CARTESIAN_POINT('Ctrl Pts',(2.43084713209955,1.456406735,-7.09570144285708));
#140105=CARTESIAN_POINT('Ctrl Pts',(2.04164654045883,1.522118786,-7.22903387662134));
#140106=CARTESIAN_POINT('Ctrl Pts',(1.64019803211863,1.586734015,-7.3189990540958));
#140107=CARTESIAN_POINT('Ctrl Pts',(1.62630434806752,1.58897027583535,-7.32211264830641));
#140108=CARTESIAN_POINT('Ctrl Pts',(1.61241066401639,1.59120653667077,-7.32522624251717));
#140109=CARTESIAN_POINT('Ctrl Pts',(2.122992963,1.456406735,-6.932200291));
#140110=CARTESIAN_POINT('Ctrl Pts',(1.742760442,1.522118786,-7.048646864));
#140111=CARTESIAN_POINT('Ctrl Pts',(1.352073032,1.586734015,-7.122808331));
#140112=CARTESIAN_POINT('Ctrl Pts',(1.33855177753145,1.58897027583535,-7.12537497645977));
#140113=CARTESIAN_POINT('Ctrl Pts',(1.32503052306288,1.59120653667077,-7.1279416219196));
#140114=CARTESIAN_POINT('Origin',(-0.0747462306198937,1.33939577632165,
0.177750342394769));
#140115=CARTESIAN_POINT('Ctrl Pts',(1.156293362,1.586734015,-7.410329659));
#140116=CARTESIAN_POINT('Ctrl Pts',(0.754357708,1.521690237,-7.473046914));
#140117=CARTESIAN_POINT('Ctrl Pts',(0.347996481,1.456414446,-7.491922213));
#140118=CARTESIAN_POINT('Ctrl Pts',(1.352073032,1.586734015,-7.122808331));
#140119=CARTESIAN_POINT('Ctrl Pts',(0.965732511,1.521690237,-7.19614465799999));
#140120=CARTESIAN_POINT('Ctrl Pts',(0.573726349,1.456414446,-7.227263526));
#140121=CARTESIAN_POINT('',(0.578399550200102,1.45719264058788,-7.22689102927039));
#140122=CARTESIAN_POINT('Origin',(-0.0200205943984027,1.48214303746773,
0.198378610296187));
#140123=CARTESIAN_POINT('Ctrl Pts',(0.597539084743176,1.49654505840402,
-7.47615857517617));
#140124=CARTESIAN_POINT('Ctrl Pts',(0.594382318797104,1.49030358394784,
-7.43457020272796));
#140125=CARTESIAN_POINT('Ctrl Pts',(0.591208389122253,1.48390865067692,
-7.39298222514298));
#140126=CARTESIAN_POINT('Ctrl Pts',(0.584830715843341,1.4708021902267,-7.3099067833631));
#140127=CARTESIAN_POINT('Ctrl Pts',(0.581623276858751,1.46408307062406,
-7.26837115206612));
#140128=CARTESIAN_POINT('Ctrl Pts',(0.578399553874345,1.45719264066649,
-7.22689102998411));
#140129=CARTESIAN_POINT('Ctrl Pts',(0.848649214287756,1.456406735,-7.45236816437262));
#140130=CARTESIAN_POINT('Ctrl Pts',(0.439885384551297,1.522118786,-7.49891673678234));
#140131=CARTESIAN_POINT('Ctrl Pts',(0.0284826653430106,1.586734015,-7.50047901633372));
#140132=CARTESIAN_POINT('Ctrl Pts',(0.0142444776038436,1.58897027576919,
-7.50053308508075));
#140133=CARTESIAN_POINT('Ctrl Pts',(6.28986467648867E-6,1.59120653653846,
-7.50058715382782));
#140134=CARTESIAN_POINT('Ctrl Pts',(0.583140419,1.456406735,-7.226510033));
#140135=CARTESIAN_POINT('Ctrl Pts',(0.186764952,1.522118786,-7.258495397));
#140136=CARTESIAN_POINT('Ctrl Pts',(-0.210730926,1.586734015,-7.246936765));
#140137=CARTESIAN_POINT('Ctrl Pts',(-0.224487813527143,1.58897027576919,
-7.24653673368094));
#140138=CARTESIAN_POINT('Ctrl Pts',(-0.238244701054285,1.59120653653846,
-7.246136702362));
#140139=CARTESIAN_POINT('Origin',(-0.0347876382410184,1.33939576438634,
0.189663017003805));
#140140=CARTESIAN_POINT('Ctrl Pts',(-0.463741963,1.586734015,-7.485649163));
#140141=CARTESIAN_POINT('Ctrl Pts',(-0.869762941,1.521690237,-7.460495838));
#140142=CARTESIAN_POINT('Ctrl Pts',(-1.2706813,1.456414446,-7.391574192));
#140143=CARTESIAN_POINT('Ctrl Pts',(-0.210730926,1.586734015,-7.246936765));
#140144=CARTESIAN_POINT('Ctrl Pts',(-0.603804163,1.521690237,-7.235506737));
#140145=CARTESIAN_POINT('Ctrl Pts',(-0.993335076,1.456414446,-7.181628327));
#140146=CARTESIAN_POINT('',(-0.988691055730179,1.45719264059555,-7.18226913885259));
#140147=CARTESIAN_POINT('Origin',(0.0230930328052294,1.48214303776053,0.198044760086257));
#140148=CARTESIAN_POINT('Ctrl Pts',(-1.02358414735161,1.49654505839643,
-7.42982338229497));
#140149=CARTESIAN_POINT('Ctrl Pts',(-1.01772683905243,1.49030358395369,
-7.38852871155802));
#140150=CARTESIAN_POINT('Ctrl Pts',(-1.01188637805703,1.48390865069583,
-7.34723073675153));
#140151=CARTESIAN_POINT('Ctrl Pts',(-1.00025618222517,1.470802192435,-7.26472655507432));
#140152=CARTESIAN_POINT('Ctrl Pts',(-0.994459698903287,1.46408307172406,
-7.2234724918208));
#140153=CARTESIAN_POINT('Ctrl Pts',(-0.988691051854014,1.45719264074061,
-7.18226914059731));
#140154=CARTESIAN_POINT('Ctrl Pts',(-0.773230597839086,1.456406735,-7.46057043305704));
#140155=CARTESIAN_POINT('Ctrl Pts',(-1.18244432400898,1.522118786,-7.41815858538821));
#140156=CARTESIAN_POINT('Ctrl Pts',(-1.58456451966023,1.586734015,-7.33124491658723));
#140157=CARTESIAN_POINT('Ctrl Pts',(-1.59848144954698,1.5889702757532,-7.32823693179069));
#140158=CARTESIAN_POINT('Ctrl Pts',(-1.61239837943374,1.59120653650647,
-7.32522894699414));
#140159=CARTESIAN_POINT('Ctrl Pts',(-0.983979122,1.456406735,-7.182916197));
#140160=CARTESIAN_POINT('Ctrl Pts',(-1.37796346,1.522118786,-7.128944752));
#140161=CARTESIAN_POINT('Ctrl Pts',(-1.763681341,1.586734015,-7.032206491));
#140162=CARTESIAN_POINT('Ctrl Pts',(-1.77703060513542,1.5889702757532,-7.02885848806392));
#140163=CARTESIAN_POINT('Ctrl Pts',(-1.79037986927085,1.59120653650647,
-7.02551048512773));
#140164=CARTESIAN_POINT('Origin',(0.00679763605717421,1.33939574081864,
0.19270726971784));
#140165=CARTESIAN_POINT('Ctrl Pts',(-2.06209323,1.586734015,-7.21094803100001));
#140166=CARTESIAN_POINT('Ctrl Pts',(-2.453214441,1.521690237,-7.099100269));
#140167=CARTESIAN_POINT('Ctrl Pts',(-2.829943435,1.456414446,-6.945604377));
#140168=CARTESIAN_POINT('Ctrl Pts',(-1.763681341,1.586734015,-7.032206491));
#140169=CARTESIAN_POINT('Ctrl Pts',(-2.145107626,1.521690237,-6.936544564));
#140170=CARTESIAN_POINT('Ctrl Pts',(-2.513949257,1.456414446,-6.800188169));
#140171=CARTESIAN_POINT('',(-2.50955156696889,1.45719264059073,-6.80181232626542));
#140172=CARTESIAN_POINT('Origin',(0.0651268731420246,1.48214303842256,0.188450166502925));
#140173=CARTESIAN_POINT('Ctrl Pts',(-2.59684572190938,1.49654505838242,
-7.03607790590515));
#140174=CARTESIAN_POINT('Ctrl Pts',(-2.58224822063562,1.49030358394116,
-6.99700782975637));
#140175=CARTESIAN_POINT('Ctrl Pts',(-2.56766646253126,1.48390865068695,
-6.9579309050984));
#140176=CARTESIAN_POINT('Ctrl Pts',(-2.53857221501543,1.47080219291372,
-6.87985577640133));
#140177=CARTESIAN_POINT('Ctrl Pts',(-2.52404284554602,1.46408307195932,
-6.84081228116058));
#140178=CARTESIAN_POINT('Ctrl Pts',(-2.50955156324783,1.45719264075521,
-6.80181232858497));
#140179=CARTESIAN_POINT('Ctrl Pts',(-2.35895500654193,1.456406735,-7.11992472055498));
#140180=CARTESIAN_POINT('Ctrl Pts',(-2.74948424915749,1.522118786,-6.99053558333553));
#140181=CARTESIAN_POINT('Ctrl Pts',(-3.12351922935449,1.586734015,-6.81920995168709));
#140182=CARTESIAN_POINT('Ctrl Pts',(-3.13646416134242,1.58897027574851,
-6.81328056334937));
#140183=CARTESIAN_POINT('Ctrl Pts',(-3.14940909333042,1.5912065364971,-6.80735117501149));
#140184=CARTESIAN_POINT('Ctrl Pts',(-2.505088894,1.456406735,-6.803457182));
#140185=CARTESIAN_POINT('Ctrl Pts',(-2.878259831,1.522118786,-6.666052574));
#140186=CARTESIAN_POINT('Ctrl Pts',(-3.234163976,1.586734015,-6.488658057));
#140187=CARTESIAN_POINT('Ctrl Pts',(-3.24648142007655,1.58897027574851,
-6.48251863133349));
#140188=CARTESIAN_POINT('Ctrl Pts',(-3.25879886415312,1.59120653649709,
-6.47637920566687));
#140189=CARTESIAN_POINT('Origin',(0.0480650262539523,1.33939571431161,0.186740464814124));
#140190=CARTESIAN_POINT('Ctrl Pts',(-3.564023309,1.586734015,-6.599070984));
#140191=CARTESIAN_POINT('Ctrl Pts',(-3.921956361,1.521690237,-6.405758661));
#140192=CARTESIAN_POINT('Ctrl Pts',(-4.25688056,1.456414446,-6.17486582));
#140193=CARTESIAN_POINT('Ctrl Pts',(-3.234163976,1.586734015,-6.48865805700001));
#140194=CARTESIAN_POINT('Ctrl Pts',(-3.58610824,1.521690237,-6.313237276));
#140195=CARTESIAN_POINT('Ctrl Pts',(-3.917013965,1.456414446,-6.10077877));
#140196=CARTESIAN_POINT('',(-3.91306823593771,1.45719264060545,-6.10331032877246));
#140197=CARTESIAN_POINT('Origin',(0.104115509672377,1.4821430441907,0.170044049113139));
#140198=CARTESIAN_POINT('Ctrl Pts',(-4.04868167678958,1.49654505837857,
-6.31333324611067));
#140199=CARTESIAN_POINT('Ctrl Pts',(-4.02602654552554,1.49030358394781,
-6.27831463799634));
#140200=CARTESIAN_POINT('Ctrl Pts',(-4.00338531713499,1.48390865070025,
-6.24328595714916));
#140201=CARTESIAN_POINT('Ctrl Pts',(-3.9581874309852,1.47080219258203,-6.17329058298485));
#140202=CARTESIAN_POINT('Ctrl Pts',(-3.93560455346299,1.46408307182328,
-6.13828328903141));
#140203=CARTESIAN_POINT('Ctrl Pts',(-3.91306823295187,1.45719264080112,
-6.10331033194857));
#140204=CARTESIAN_POINT('Ctrl Pts',(-3.83437730066977,1.456406735,-6.44635924039643));
#140205=CARTESIAN_POINT('Ctrl Pts',(-4.1879613471737,1.522118786,-6.23604290637256));
#140206=CARTESIAN_POINT('Ctrl Pts',(-4.51642165067597,1.586734015,-5.98831630932468));
#140207=CARTESIAN_POINT('Ctrl Pts',(-4.5277892940278,1.58897027573085,-5.97974276916175));
#140208=CARTESIAN_POINT('Ctrl Pts',(-4.53915693737959,1.59120653646176,
-5.97116922899881));
#140209=CARTESIAN_POINT('Ctrl Pts',(-3.909063493,1.456406735,-6.105876072));
#140210=CARTESIAN_POINT('Ctrl Pts',(-4.243971972,1.522118786,-5.891463186));
#140211=CARTESIAN_POINT('Ctrl Pts',(-4.553420698,1.586734015,-5.64170718300001));
#140212=CARTESIAN_POINT('Ctrl Pts',(-4.56413037194033,1.58897027573085,
-5.63306340736922));
#140213=CARTESIAN_POINT('Ctrl Pts',(-4.57484004588063,1.59120653646176,
-5.62441963173858));
#140214=CARTESIAN_POINT('Origin',(0.087084894057271,1.33939575604422,0.172041892552222));
#140215=CARTESIAN_POINT('Ctrl Pts',(-4.899303619,1.586734015,-5.678628712));
#140216=CARTESIAN_POINT('Ctrl Pts',(-5.20731196,1.521690237,-5.412890898));
#140217=CARTESIAN_POINT('Ctrl Pts',(-5.484770682,1.456414446,-5.115397401));
#140218=CARTESIAN_POINT('Ctrl Pts',(-4.553420698,1.586734015,-5.641707183));
#140219=CARTESIAN_POINT('Ctrl Pts',(-4.859426419,1.521690237,-5.39473003));
#140220=CARTESIAN_POINT('Ctrl Pts',(-5.136923453,1.456414446,-5.116103736));
#140221=CARTESIAN_POINT('',(-5.13361418323162,1.45719264060118,-5.11942432355012));
#140222=CARTESIAN_POINT('Origin',(0.138235559677372,1.48214304625789,0.143686509911358));
#140223=CARTESIAN_POINT('Ctrl Pts',(-5.31120577594162,1.49654505840647,
-5.29538414122325));
#140224=CARTESIAN_POINT('Ctrl Pts',(-5.28155234347734,1.49030358394726,
-5.26605443207318));
#140225=CARTESIAN_POINT('Ctrl Pts',(-5.25191032365658,1.48390865070959,
-5.23671189715127));
#140226=CARTESIAN_POINT('Ctrl Pts',(-5.19272219896809,1.4708021917559,-5.17806918153808));
#140227=CARTESIAN_POINT('Ctrl Pts',(-5.16314176519753,1.46408307141407,
-5.1487349916414));
#140228=CARTESIAN_POINT('Ctrl Pts',(-5.13361418103969,1.45719264078779,
-5.11942432714059));
#140229=CARTESIAN_POINT('Ctrl Pts',(-5.13050837364047,1.456406735,-5.47136916785226));
#140230=CARTESIAN_POINT('Ctrl Pts',(-5.43061402642661,1.522118786,-5.18995979468923));
#140231=CARTESIAN_POINT('Ctrl Pts',(-5.69814121471094,1.586734015,-4.87741565142108));
#140232=CARTESIAN_POINT('Ctrl Pts',(-5.70740003131374,1.58897027576622,
-4.86659884838373));
#140233=CARTESIAN_POINT('Ctrl Pts',(-5.71665884791666,1.5912065365325,-4.8557820453464));
#140234=CARTESIAN_POINT('Ctrl Pts',(-5.130254628,1.456406735,-5.122790982));
#140235=CARTESIAN_POINT('Ctrl Pts',(-5.411240701,1.522118786,-4.841395528));
#140236=CARTESIAN_POINT('Ctrl Pts',(-5.65976453,1.586734015,-4.530956353));
#140237=CARTESIAN_POINT('Ctrl Pts',(-5.66836566160424,1.58897027576622,
-4.52021240055879));
#140238=CARTESIAN_POINT('Ctrl Pts',(-5.67696679320846,1.5912065365325,-4.50946844811759));
#140239=CARTESIAN_POINT('Origin',(0.122032764432546,1.3393957688585,0.149298916293734));
#140240=CARTESIAN_POINT('Ctrl Pts',(-6.005497937,1.586734015,-4.492660073));
#140241=CARTESIAN_POINT('Ctrl Pts',(-6.249179439,1.521690237,-4.166922373));
#140242=CARTESIAN_POINT('Ctrl Pts',(-6.456199023,1.456414446,-3.816738684));
#140243=CARTESIAN_POINT('Ctrl Pts',(-5.65976453000001,1.586734015,-4.530956353));
#140244=CARTESIAN_POINT('Ctrl Pts',(-5.905523219,1.521690237,-4.223971203));
#140245=CARTESIAN_POINT('Ctrl Pts',(-6.116636109,1.456414446,-3.892205378));
#140246=CARTESIAN_POINT('',(-6.11411803681458,1.45719264058743,-3.89615972708495));
#140247=CARTESIAN_POINT('Origin',(0.165892242204772,1.48214301587359,0.110610760436994));
#140248=CARTESIAN_POINT('Ctrl Pts',(-6.32538379675321,1.49654505840746,
-4.02982875897274));
#140249=CARTESIAN_POINT('Ctrl Pts',(-6.29011862453828,1.49030358395683,
-4.00755937353871));
#140250=CARTESIAN_POINT('Ctrl Pts',(-6.2548618407542,1.48390865067755,-3.98527500864475));
#140251=CARTESIAN_POINT('Ctrl Pts',(-6.1844510440732,1.47080219039292,-3.94072701982678));
#140252=CARTESIAN_POINT('Ctrl Pts',(-6.14925620457091,1.46408307071962,
-3.91843756826649));
#140253=CARTESIAN_POINT('Ctrl Pts',(-6.1141180357621,1.45719264069513,-3.89615973061763));
#140254=CARTESIAN_POINT('Ctrl Pts',(-6.18674257775374,1.456406735,-4.2405439538314));
#140255=CARTESIAN_POINT('Ctrl Pts',(-6.41933723072151,1.522118786,-3.90119993089596));
#140256=CARTESIAN_POINT('Ctrl Pts',(-6.61342203006909,1.586734015,-3.53845245862732));
#140257=CARTESIAN_POINT('Ctrl Pts',(-6.62013908773575,1.58897027575197,
-3.52589817463466));
#140258=CARTESIAN_POINT('Ctrl Pts',(-6.62685614540246,1.59120653650401,
-3.51334389064201));
#140259=CARTESIAN_POINT('Ctrl Pts',(-6.111560759,1.456406735,-3.90016988));
#140260=CARTESIAN_POINT('Ctrl Pts',(-6.325485828,1.522118786,-3.564949595));
#140261=CARTESIAN_POINT('Ctrl Pts',(-6.501464062,1.586734015,-3.208343039));
#140262=CARTESIAN_POINT('Ctrl Pts',(-6.50755447170662,1.58897027575197,
-3.19600128524589));
#140263=CARTESIAN_POINT('Ctrl Pts',(-6.51364488141335,1.59120653650401,
-3.18365953149176));
#140264=CARTESIAN_POINT('Origin',(0.151274700206816,1.33939575620768,0.119575041319626));
#140265=CARTESIAN_POINT('Ctrl Pts',(-6.830881846,1.586734015,-3.096619642));
#140266=CARTESIAN_POINT('Ctrl Pts',(-6.99884223300001,1.521690237,-2.726113188));
#140267=CARTESIAN_POINT('Ctrl Pts',(-7.125742672,1.456414446,-2.339613509));
#140268=CARTESIAN_POINT('Ctrl Pts',(-6.501464062,1.586734015,-3.208343039));
#140269=CARTESIAN_POINT('Ctrl Pts',(-6.675484317,1.521690237,-2.855704178));
#140270=CARTESIAN_POINT('Ctrl Pts',(-6.81034166,1.456414446,-2.486311822));
#140271=CARTESIAN_POINT('',(-6.8087325263123,1.4571926406148,-2.49071503215939));
#140272=CARTESIAN_POINT('Origin',(0.185791769945721,1.48214304416343,0.0723628059213374));
#140273=CARTESIAN_POINT('Ctrl Pts',(-7.04379390051593,1.49654505840368,
-2.575843062689));
#140274=CARTESIAN_POINT('Ctrl Pts',(-7.00456594895746,1.49030358396683,
-2.56167529283628));
#140275=CARTESIAN_POINT('Ctrl Pts',(-6.96534296957004,1.48390865070459,
-2.54749109047069));
#140276=CARTESIAN_POINT('Ctrl Pts',(-6.88700185505409,1.4708021933808,-2.51912085537668));
#140277=CARTESIAN_POINT('Ctrl Pts',(-6.84783826862204,1.46408307220057,
-2.50491836558355));
#140278=CARTESIAN_POINT('Ctrl Pts',(-6.80873252610584,1.45719264079019,
-2.4907150361556));
#140279=CARTESIAN_POINT('Ctrl Pts',(-6.95369157446804,1.456406735,-2.8114356170973));
#140280=CARTESIAN_POINT('Ctrl Pts',(-7.10789935959439,1.522118786,-2.43002429438231));
#140281=CARTESIAN_POINT('Ctrl Pts',(-7.21946658014416,1.586734015,-2.03403516072589));
#140282=CARTESIAN_POINT('Ctrl Pts',(-7.2233277967278,1.58897027572729,-2.02033042019118));
#140283=CARTESIAN_POINT('Ctrl Pts',(-7.22718901331137,1.59120653645465,
-2.00662567965648));
#140284=CARTESIAN_POINT('Ctrl Pts',(-6.8070971,1.456406735,-2.495181169));
#140285=CARTESIAN_POINT('Ctrl Pts',(-6.943958268,1.522118786,-2.121810582));
#140286=CARTESIAN_POINT('Ctrl Pts',(-7.03916236,1.586734015,-1.73571117));
#140287=CARTESIAN_POINT('Ctrl Pts',(-7.04245726702598,1.58897027572729,
-1.72234870165851));
#140288=CARTESIAN_POINT('Ctrl Pts',(-7.045752174052,1.59120653645465,-1.70898623331697));
#140289=CARTESIAN_POINT('Origin',(0.173442981648092,1.33939574964305,0.0842598250749746));
#140290=CARTESIAN_POINT('Ctrl Pts',(-7.33686131200001,1.586734015,-1.555784718));
#140291=CARTESIAN_POINT('Ctrl Pts',(-7.421246943,1.521690237,-1.157833981));
#140292=CARTESIAN_POINT('Ctrl Pts',(-7.462094514,1.456414446,-0.753090606));
#140293=CARTESIAN_POINT('Ctrl Pts',(-7.03916236,1.586734015,-1.73571117));
#140294=CARTESIAN_POINT('Ctrl Pts',(-7.133307187,1.521690237,-1.353907599));
#140295=CARTESIAN_POINT('Ctrl Pts',(-7.185603203,1.456414446,-0.964161089));
#140296=CARTESIAN_POINT('',(-7.18497825045877,1.45719264059852,-0.968807270208435));
#140297=CARTESIAN_POINT('Origin',(0.197003933959137,1.48214303945679,0.0307312683202327));
#140298=CARTESIAN_POINT('Ctrl Pts',(-7.4328440302926,1.49654505837467,-1.00141380765487));
#140299=CARTESIAN_POINT('Ctrl Pts',(-7.39148755465633,1.49030358392794,
-0.996010122351639));
#140300=CARTESIAN_POINT('Ctrl Pts',(-7.35013240261102,1.48390865068228,
-0.990589319895403));
#140301=CARTESIAN_POINT('Ctrl Pts',(-7.26752408917957,1.47080219197549,
-0.979723387895179));
#140302=CARTESIAN_POINT('Ctrl Pts',(-7.22622301479003,1.46408307149698,
-0.97427195849633));
#140303=CARTESIAN_POINT('Ctrl Pts',(-7.18497825071308,1.45719264073434,
-0.96880727432235));
#140304=CARTESIAN_POINT('Ctrl Pts',(-7.39549368163616,1.456406735,-1.25086767559283));
#140305=CARTESIAN_POINT('Ctrl Pts',(-7.46410401451051,1.522118786,-0.845223421831543));
#140306=CARTESIAN_POINT('Ctrl Pts',(-7.48793689720321,1.586734015,-0.434508640665181));
#140307=CARTESIAN_POINT('Ctrl Pts',(-7.48876172660557,1.58897027577494,
-0.42029426165538));
#140308=CARTESIAN_POINT('Ctrl Pts',(-7.48958655600797,1.59120653654989,
-0.40607988264558));
#140309=CARTESIAN_POINT('Ctrl Pts',(-7.184341147,1.456406735,-0.97352056));
#140310=CARTESIAN_POINT('Ctrl Pts',(-7.237738938,1.522118786,-0.579458064));
#140311=CARTESIAN_POINT('Ctrl Pts',(-7.24771725,1.586734015,-0.181919376));
#140312=CARTESIAN_POINT('Ctrl Pts',(-7.24806258821318,1.58897027577494,
-0.168161006831391));
#140313=CARTESIAN_POINT('Ctrl Pts',(-7.24840792642632,1.59120653654989,
-0.154402637662788));
#140314=CARTESIAN_POINT('Origin',(0.187501581422369,1.33939575027433,0.0450047815784362));
#140315=CARTESIAN_POINT('Ctrl Pts',(-7.499777297,1.586734015,0.05779697));
#140316=CARTESIAN_POINT('Ctrl Pts',(-7.496642395,1.521690237,0.464584256));
#140317=CARTESIAN_POINT('Ctrl Pts',(-7.44952710999999,1.456414446,0.868645977));
#140318=CARTESIAN_POINT('Ctrl Pts',(-7.24771725,1.586734015,-0.181919376));
#140319=CARTESIAN_POINT('Ctrl Pts',(-7.257584542,1.521690237,0.211196195));
#140320=CARTESIAN_POINT('Ctrl Pts',(-7.224873927,1.456414446,0.603072745000001));
#140321=CARTESIAN_POINT('',(-7.22526237690475,1.45719264059895,0.598400842763318));
#140322=CARTESIAN_POINT('Origin',(0.199004244131034,1.48214300852825,-0.0123372337775944));
#140323=CARTESIAN_POINT('Ctrl Pts',(-7.47434263483393,1.49654505840668,
0.619840443920158));
#140324=CARTESIAN_POINT('Ctrl Pts',(-7.43279141797426,1.49030358396172,
0.616227374350938));
#140325=CARTESIAN_POINT('Ctrl Pts',(-7.39123781394946,1.48390865069529,
0.612631306257495));
#140326=CARTESIAN_POINT('Ctrl Pts',(-7.30822498460246,1.47080219226751,
0.605484853522584));
#140327=CARTESIAN_POINT('Ctrl Pts',(-7.26671760915856,1.46408307162048,
0.601930321309041));
#140328=CARTESIAN_POINT('Ctrl Pts',(-7.22526237832533,1.45719264069052,
0.598400839016716));
#140329=CARTESIAN_POINT('Ctrl Pts',(-7.49149072463768,1.456406735,0.368189448021402));
#140330=CARTESIAN_POINT('Ctrl Pts',(-7.47129546192193,1.522118786,0.779099157187545));
#140331=CARTESIAN_POINT('Ctrl Pts',(-7.40627960745038,1.586734015,1.18533502103326));
#140332=CARTESIAN_POINT('Ctrl Pts',(-7.40402948149176,1.58897027575943,
1.19939438962868));
#140333=CARTESIAN_POINT('Ctrl Pts',(-7.40177935553306,1.59120653651885,
1.21345375822411));
#140334=CARTESIAN_POINT('Ctrl Pts',(-7.225653387,1.456406735,0.593660789));
#140335=CARTESIAN_POINT('Ctrl Pts',(-7.193090978,1.522118786,0.989989269));
#140336=CARTESIAN_POINT('Ctrl Pts',(-7.117376937,1.586734015,1.380378766));
#140337=CARTESIAN_POINT('Ctrl Pts',(-7.11475655877887,1.58897027575943,
1.39388970957387));
#140338=CARTESIAN_POINT('Ctrl Pts',(-7.11213618055764,1.59120653651885,
1.40740065314777));
#140339=CARTESIAN_POINT('Origin',(0.192792530964795,1.33939579133204,0.00364529811479691));
#140340=CARTESIAN_POINT('Ctrl Pts',(-7.312012032,1.586734015,1.668676136));
#140341=CARTESIAN_POINT('Ctrl Pts',(-7.221503179,1.521690237,2.06527905));
#140342=CARTESIAN_POINT('Ctrl Pts',(-7.088628098,1.456414446,2.449765639));
#140343=CARTESIAN_POINT('Ctrl Pts',(-7.117376937,1.586734015,1.380378766));
#140344=CARTESIAN_POINT('Ctrl Pts',(-7.042505309,1.521690237,1.766424689));
#140345=CARTESIAN_POINT('Ctrl Pts',(-6.926317576,1.456414446,2.142107568));
#140346=CARTESIAN_POINT('',(-6.92770126528305,1.45719264059855,2.13762839733776));
#140347=CARTESIAN_POINT('Origin',(0.191699739143811,1.48214301911425,-0.0548288895523261));
#140348=CARTESIAN_POINT('Ctrl Pts',(-7.16634928428777,1.49654505841316,
2.21211164520096));
#140349=CARTESIAN_POINT('Ctrl Pts',(-7.12654621497199,1.49030358397192,
2.19965076379803));
#140350=CARTESIAN_POINT('Ctrl Pts',(-7.08673715953174,1.48390865071391,
2.18720597323833));
#140351=CARTESIAN_POINT('Ctrl Pts',(-7.00720139359456,1.47080219120606,
2.1623812941064));
#140352=CARTESIAN_POINT('Ctrl Pts',(-6.96742856043393,1.46408307111354,
2.14998700724187));
#140353=CARTESIAN_POINT('Ctrl Pts',(-6.92770126721526,1.45719264069766,
2.13762839403927));
#140354=CARTESIAN_POINT('Ctrl Pts',(-7.23719398613241,1.456406735,1.97003044157164));
#140355=CARTESIAN_POINT('Ctrl Pts',(-7.12913743724507,1.522118786,2.3669919266526));
#140356=CARTESIAN_POINT('Ctrl Pts',(-6.97831291553588,1.586734015,2.74975373474379));
#140357=CARTESIAN_POINT('Ctrl Pts',(-6.97309304757981,1.5889702757851,2.76300069269339));
#140358=CARTESIAN_POINT('Ctrl Pts',(-6.96787317962392,1.5912065365702,2.77624765064298));
#140359=CARTESIAN_POINT('Ctrl Pts',(-6.929102105,1.456406735,2.133083219));
#140360=CARTESIAN_POINT('Ctrl Pts',(-6.812102079,1.522118786,2.513145805));
#140361=CARTESIAN_POINT('Ctrl Pts',(-6.654235988,1.586734015,2.878131931));
#140362=CARTESIAN_POINT('Ctrl Pts',(-6.64877241920881,1.5889702757851,2.8907636924796));
#140363=CARTESIAN_POINT('Ctrl Pts',(-6.64330885041767,1.5912065365702,2.90339545395922));
#140364=CARTESIAN_POINT('Origin',(0.189068793117005,1.33939575948771,-0.0378846249694881));
#140365=CARTESIAN_POINT('Ctrl Pts',(-6.78234521,1.586734015,3.201529861));
#140366=CARTESIAN_POINT('Ctrl Pts',(-6.608694501,1.521690237,3.569403691));
#140367=CARTESIAN_POINT('Ctrl Pts',(-6.396272715,1.456414446,3.916336982));
#140368=CARTESIAN_POINT('Ctrl Pts',(-6.654235988,1.586734015,2.878131931));
#140369=CARTESIAN_POINT('Ctrl Pts',(-6.498126356,1.521690237,3.239057128));
#140370=CARTESIAN_POINT('Ctrl Pts',(-6.303894313,1.456414446,3.580979822));
#140371=CARTESIAN_POINT('',(-6.3062085417898,1.45719264061766,3.57690282398186));
#140372=CARTESIAN_POINT('Origin',(0.17543108332008,1.48214304481658,-0.094756675136119));
#140373=CARTESIAN_POINT('Ctrl Pts',(-6.52326540639353,1.49654505841099,
3.70094696449352));
#140374=CARTESIAN_POINT('Ctrl Pts',(-6.48707163187202,1.4903035839601,3.6802209282024));
#140375=CARTESIAN_POINT('Ctrl Pts',(-6.45086855211468,1.48390865069852,
3.65950931972571));
#140376=CARTESIAN_POINT('Ctrl Pts',(-6.37852886526687,1.47080219210092,
3.61816719197017));
#140377=CARTESIAN_POINT('Ctrl Pts',(-6.34235030148423,1.46408307157444,
3.59751269169146));
#140378=CARTESIAN_POINT('Ctrl Pts',(-6.30620854453905,1.45719264077253,
3.57690282104796));
#140379=CARTESIAN_POINT('Ctrl Pts',(-6.64449410151412,1.456406735,3.47975500206342));
#140380=CARTESIAN_POINT('Ctrl Pts',(-6.45362886927911,1.522118786,3.84420678350785));
#140381=CARTESIAN_POINT('Ctrl Pts',(-6.22404806648052,1.586734015,4.18559701939759));
#140382=CARTESIAN_POINT('Ctrl Pts',(-6.2161025318132,1.58897027576657,4.19741215342132));
#140383=CARTESIAN_POINT('Ctrl Pts',(-6.20815699714588,1.59120653653314,
4.2092272874451));
#140384=CARTESIAN_POINT('Ctrl Pts',(-6.30855371000001,1.456406735,3.572765048));
#140385=CARTESIAN_POINT('Ctrl Pts',(-6.11258685800001,1.522118786,3.918790435));
#140386=CARTESIAN_POINT('Ctrl Pts',(-5.879950361,1.586734015,4.241306845));
#140387=CARTESIAN_POINT('Ctrl Pts',(-5.87189907217594,1.58897027576657,
4.25246877703087));
#140388=CARTESIAN_POINT('Ctrl Pts',(-5.86384778335191,1.59120653653313,
4.26363070906172));
#140389=CARTESIAN_POINT('Origin',(0.176504357918514,1.33939572459492,-0.0776430649301657));
#140390=CARTESIAN_POINT('Ctrl Pts',(-5.935543465,1.586734015,4.584683607));
#140391=CARTESIAN_POINT('Ctrl Pts',(-5.686870614,1.521690237,4.906626983));
#140392=CARTESIAN_POINT('Ctrl Pts',(-5.404834728,1.456414446,5.199784761));
#140393=CARTESIAN_POINT('Ctrl Pts',(-5.87995036100001,1.586734015,4.241306845));
#140394=CARTESIAN_POINT('Ctrl Pts',(-5.649902236,1.521690237,4.560234855));
#140395=CARTESIAN_POINT('Ctrl Pts',(-5.386707959,1.456414446,4.852409439));
#140396=CARTESIAN_POINT('',(-5.389844515688,1.45719264057876,4.8489252501941));
#140397=CARTESIAN_POINT('Origin',(0.150959951003083,1.48214302133659,-0.130254007742108));
#140398=CARTESIAN_POINT('Ctrl Pts',(-5.57516088824712,1.49654505841865,
5.01673011704007));
#140399=CARTESIAN_POINT('Ctrl Pts',(-5.5442687891568,1.49030358396378,4.98870805233087));
#140400=CARTESIAN_POINT('Ctrl Pts',(-5.51336450100249,1.4839086507277,4.96069807790661));
#140401=CARTESIAN_POINT('Ctrl Pts',(-5.45160341771219,1.47080219347429,
4.90477161763631));
#140402=CARTESIAN_POINT('Ctrl Pts',(-5.42071079214679,1.46408307220416,
4.87682268306431));
#140403=CARTESIAN_POINT('Ctrl Pts',(-5.38984451945149,1.45719264069583,
4.8489252475705));
#140404=CARTESIAN_POINT('Ctrl Pts',(-5.74110505755524,1.456406735,4.82677008554393));
#140405=CARTESIAN_POINT('Ctrl Pts',(-5.47635578817438,1.522118786,5.14167080416162));
#140406=CARTESIAN_POINT('Ctrl Pts',(-5.17875364692979,1.586734015,5.42572643982073));
#140407=CARTESIAN_POINT('Ctrl Pts',(-5.16845396967177,1.58897027580737,
5.4355572876714));
#140408=CARTESIAN_POINT('Ctrl Pts',(-5.15815429241373,1.59120653661473,
5.44538813552219));
#140409=CARTESIAN_POINT('Ctrl Pts',(-5.393024354,1.456406735,4.845388355));
#140410=CARTESIAN_POINT('Ctrl Pts',(-5.12725387,1.522118786,5.14119678));
#140411=CARTESIAN_POINT('Ctrl Pts',(-4.830724789,1.586734015,5.406162966));
#140412=CARTESIAN_POINT('Ctrl Pts',(-4.82046224915688,1.58897027580737,
5.4153331493484));
#140413=CARTESIAN_POINT('Ctrl Pts',(-4.81019970931389,1.59120653661473,
5.42450333269675));
#140414=CARTESIAN_POINT('Origin',(0.155686880664996,1.33939574493368,-0.113771102637439));
#140415=CARTESIAN_POINT('Ctrl Pts',(-4.811202304,1.586734015,5.753462644));
#140416=CARTESIAN_POINT('Ctrl Pts',(-4.499134977,1.521690237,6.01442185));
#140417=CARTESIAN_POINT('Ctrl Pts',(-4.160672677,1.456414446,6.240096384));
#140418=CARTESIAN_POINT('Ctrl Pts',(-4.830724789,1.586734015,5.406162966));
#140419=CARTESIAN_POINT('Ctrl Pts',(-4.537494967,1.521690237,5.66818106999999));
#140420=CARTESIAN_POINT('Ctrl Pts',(-4.217645127,1.456414446,5.89694578400001));
#140421=CARTESIAN_POINT('',(-4.22145735081421,1.45719264057815,5.8942173209189));
#140422=CARTESIAN_POINT('Origin',(0.119429677617468,1.48214300882117,-0.15966048512369));
#140423=CARTESIAN_POINT('Ctrl Pts',(-4.36636804309702,1.49654505833465,
6.09793654538808));
#140424=CARTESIAN_POINT('Ctrl Pts',(-4.34222209965503,1.49030358387838,
6.06392873275962));
#140425=CARTESIAN_POINT('Ctrl Pts',(-4.31806165314823,1.48390865066516,
6.02993010761874));
#140426=CARTESIAN_POINT('Ctrl Pts',(-4.26976703323237,1.47080219014011,
5.9620343526714));
#140427=CARTESIAN_POINT('Ctrl Pts',(-4.245604861298,1.4640830705707,5.92809785658239));
#140428=CARTESIAN_POINT('Ctrl Pts',(-4.22145735427668,1.45719264064155,
5.89421731921874));
#140429=CARTESIAN_POINT('Ctrl Pts',(-4.56926832085666,1.456406735,5.94809076502081));
#140430=CARTESIAN_POINT('Ctrl Pts',(-4.24301439628944,1.522118786,6.19871601337983));
#140431=CARTESIAN_POINT('Ctrl Pts',(-3.89130646372213,1.586734015,6.41215492265771));
#140432=CARTESIAN_POINT('Ctrl Pts',(-3.87913424555063,1.58897027580551,
6.41954180458288));
#140433=CARTESIAN_POINT('Ctrl Pts',(-3.86696202737906,1.59120653661107,
6.42692868650803));
#140434=CARTESIAN_POINT('Ctrl Pts',(-4.225323174,1.456406735,5.891446688));
#140435=CARTESIAN_POINT('Ctrl Pts',(-3.902176188,1.522118786,6.12320647800001));
#140436=CARTESIAN_POINT('Ctrl Pts',(-3.555619896,1.586734015,6.318232914));
#140437=CARTESIAN_POINT('Ctrl Pts',(-3.54362597034658,1.58897027580551,
6.32498256081882));
#140438=CARTESIAN_POINT('Ctrl Pts',(-3.5316320446931,1.59120653661108,6.33173220763764));
#140439=CARTESIAN_POINT('Origin',(0.127589615055193,1.33939577602722,-0.144579345888991));
#140440=CARTESIAN_POINT('Ctrl Pts',(-3.46189467,1.586734015,6.653216162));
#140441=CARTESIAN_POINT('Ctrl Pts',(-3.101024788,1.521690237,6.840989036));
#140442=CARTESIAN_POINT('Ctrl Pts',(-2.721962195,1.456414446,6.988628035));
#140443=CARTESIAN_POINT('Ctrl Pts',(-3.555619896,1.586734015,6.318232914));
#140444=CARTESIAN_POINT('Ctrl Pts',(-3.212919477,1.521690237,6.511089437));
#140445=CARTESIAN_POINT('Ctrl Pts',(-2.851369896,1.456414446,6.665747499));
#140446=CARTESIAN_POINT('',(-2.85567953178776,1.45719264062456,6.66390234040533));
#140447=CARTESIAN_POINT('Origin',(0.0823151945383094,1.48214303903916,-0.181601539638054));
#140448=CARTESIAN_POINT('Ctrl Pts',(-2.95340868090108,1.49654505841376,
6.89401023824042));
#140449=CARTESIAN_POINT('Ctrl Pts',(-2.93713793078994,1.49030358397024,
6.85560684540494));
#140450=CARTESIAN_POINT('Ctrl Pts',(-2.92085104149715,1.48390865071599,
6.81720930716423));
#140451=CARTESIAN_POINT('Ctrl Pts',(-2.88828110970201,1.47080219272414,
6.74051901626872));
#140452=CARTESIAN_POINT('Ctrl Pts',(-2.87197917614153,1.46408307188037,
6.70218177595652));
#140453=CARTESIAN_POINT('Ctrl Pts',(-2.8556795356562,1.45719264078122,6.66390233986534));
#140454=CARTESIAN_POINT('Ctrl Pts',(-3.18377767658021,1.456406735,6.79128533119686));
#140455=CARTESIAN_POINT('Ctrl Pts',(-2.81127436820566,1.522118786,6.96591615008536));
#140456=CARTESIAN_POINT('Ctrl Pts',(-2.42190611501465,1.586734015,7.09875816714877));
#140457=CARTESIAN_POINT('Ctrl Pts',(-2.4084305154338,1.58897027577805,7.10335568072313));
#140458=CARTESIAN_POINT('Ctrl Pts',(-2.39495491585294,1.59120653655611,
7.10795319429734));
#140459=CARTESIAN_POINT('Ctrl Pts',(-2.860050579,1.456406735,6.662027521));
#140460=CARTESIAN_POINT('Ctrl Pts',(-2.494637086,1.522118786,6.818901846));
#140461=CARTESIAN_POINT('Ctrl Pts',(-2.114258167,1.586734015,6.934869314));
#140462=CARTESIAN_POINT('Ctrl Pts',(-2.10109367821737,1.58897027577805,
6.93888281831208));
#140463=CARTESIAN_POINT('Ctrl Pts',(-2.08792918943474,1.59120653655611,
6.9428963226243));
#140464=CARTESIAN_POINT('Origin',(0.0935262382739294,1.33939574779353,-0.168626831068447));
#140465=CARTESIAN_POINT('Ctrl Pts',(-1.95071269,1.586734015,7.241872686));
#140466=CARTESIAN_POINT('Ctrl Pts',(-1.557914128,1.521690237,7.347679177));
#140467=CARTESIAN_POINT('Ctrl Pts',(-1.155975786,1.456414446,7.410379206));
#140468=CARTESIAN_POINT('Ctrl Pts',(-2.114258167,1.586734015,6.934869314));
#140469=CARTESIAN_POINT('Ctrl Pts',(-1.738111442,1.521690237,7.049546498));
#140470=CARTESIAN_POINT('Ctrl Pts',(-1.351767779,1.456414446,7.122866268));
#140471=CARTESIAN_POINT('',(-1.35637331164624,1.45719264058601,7.12199069254741));
#140472=CARTESIAN_POINT('Origin',(0.0413517804108662,1.48214301341937,-0.195051286303984));
#140473=CARTESIAN_POINT('Ctrl Pts',(-1.4023512112938,1.49654505835954,7.36772767377926));
#140474=CARTESIAN_POINT('Ctrl Pts',(-1.39471645654411,1.49030358393859,
7.32672440067643));
#140475=CARTESIAN_POINT('Ctrl Pts',(-1.38706468140528,1.48390865068783,
7.28572337574005));
#140476=CARTESIAN_POINT('Ctrl Pts',(-1.37174236273163,1.47080219302608,
7.20382449064787));
#140477=CARTESIAN_POINT('Ctrl Pts',(-1.36406293274997,1.46408307201767,
7.16287911879417));
#140478=CARTESIAN_POINT('Ctrl Pts',(-1.35637331617947,1.45719264075502,
7.12199069281731));
#140479=CARTESIAN_POINT('Ctrl Pts',(-1.64941712647212,1.456406735,7.31692694226868));
#140480=CARTESIAN_POINT('Ctrl Pts',(-1.24808227386318,1.522118786,7.40739779012271));
#140481=CARTESIAN_POINT('Ctrl Pts',(-0.839260127710371,1.586734015,7.45343136981124));
#140482=CARTESIAN_POINT('Ctrl Pts',(-0.82511125043235,1.58897027581419,
7.45502454052325));
#140483=CARTESIAN_POINT('Ctrl Pts',(-0.810962373154327,1.59120653662838,
7.45661771123534));
#140484=CARTESIAN_POINT('Ctrl Pts',(-1.361045197,1.456406735,7.121099351));
#140485=CARTESIAN_POINT('Ctrl Pts',(-0.970451525,1.522118786,7.195752943));
#140486=CARTESIAN_POINT('Ctrl Pts',(-0.574036077000001,1.586734015,7.227238932));
#140487=CARTESIAN_POINT('Ctrl Pts',(-0.560316581670197,1.58897027581419,
7.22832862686738));
#140488=CARTESIAN_POINT('Ctrl Pts',(-0.546597086340393,1.59120653662838,
7.22941832173478));
#140489=CARTESIAN_POINT('Origin',(0.0550898964041995,1.33939576732543,-0.184790043833353));
#140490=CARTESIAN_POINT('Ctrl Pts',(-0.348317552,1.586734015,7.491907293));
#140491=CARTESIAN_POINT('Ctrl Pts',(0.0580428659999999,1.521690237,7.510800007));
#140492=CARTESIAN_POINT('Ctrl Pts',(0.464062765,1.456414446,7.485629282));
#140493=CARTESIAN_POINT('Ctrl Pts',(-0.574036077,1.586734015,7.227238932));
#140494=CARTESIAN_POINT('Ctrl Pts',(-0.182031249,1.521690237,7.2583746));
#140495=CARTESIAN_POINT('Ctrl Pts',(0.211041498,1.456414446,7.246927727));
#140496=CARTESIAN_POINT('Origin',(-0.00154525971137284,1.48214304894328,
-0.19938049318742));
#140497=CARTESIAN_POINT('Ctrl Pts',(-1.35776704393169,4.30075163058632,
7.12172944830897));
#140498=CARTESIAN_POINT('Ctrl Pts',(-1.35390884396585,4.30138922829316,
7.12246068865448));
#140499=CARTESIAN_POINT('Ctrl Pts',(-1.350050644,4.302026826,7.12319192899999));
#140500=CARTESIAN_POINT('Ctrl Pts',(-0.962010097,4.36615356,7.196736822));
#140501=CARTESIAN_POINT('Ctrl Pts',(-0.568276727,4.431389364,7.227694069));
#140502=CARTESIAN_POINT('Ctrl Pts',(-1.16221715234734,4.30075163058632,
7.4094073516114));
#140503=CARTESIAN_POINT('Ctrl Pts',(-1.15820324967367,4.30138922829316,
7.4100325058057));
#140504=CARTESIAN_POINT('Ctrl Pts',(-1.154189347,4.302026826,7.41065766));
#140505=CARTESIAN_POINT('Ctrl Pts',(-0.750488916,4.36615356,7.473532881));
#140506=CARTESIAN_POINT('Ctrl Pts',(-0.342347366,4.431389364,7.492182478));
#140507=CARTESIAN_POINT('',(-0.572986203456379,4.43060907981178,7.22732224112228));
#140508=CARTESIAN_POINT('Ctrl Pts',(-0.572986202613025,4.43060907940012,
7.22732224306242));
#140509=CARTESIAN_POINT('Ctrl Pts',(-0.575775813424748,4.42401550332526,
7.26754705881263));
#140510=CARTESIAN_POINT('Ctrl Pts',(-0.57866334130313,4.41742229674867,
7.30876626432251));
#140511=CARTESIAN_POINT('Ctrl Pts',(-0.584752497706469,4.40420945810707,
7.39349824679339));
#140512=CARTESIAN_POINT('Ctrl Pts',(-0.587799206996747,4.39788077308853,
7.43509547553819));
#140513=CARTESIAN_POINT('Ctrl Pts',(-0.590897510188735,4.39169923734407,
7.47668644070131));
#140514=CARTESIAN_POINT('Origin',(-0.0051813612548729,4.55345288605838,
-0.19241258054202));
#140515=CARTESIAN_POINT('Ctrl Pts',(-2.117742488,4.431369595,6.93380608));
#140516=CARTESIAN_POINT('Ctrl Pts',(-2.10947844,4.429970133,6.936330109));
#140517=CARTESIAN_POINT('Ctrl Pts',(-2.1012084,4.428571429,6.938834431));
#140518=CARTESIAN_POINT('Ctrl Pts',(-1.730553477,4.365882895,7.05107565));
#140519=CARTESIAN_POINT('Ctrl Pts',(-1.350050644,4.302026826,7.123191929));
#140520=CARTESIAN_POINT('Ctrl Pts',(-2.424827999,4.431369595,7.097197276));
#140521=CARTESIAN_POINT('Ctrl Pts',(-2.416369214,4.429970133,7.100087304));
#140522=CARTESIAN_POINT('Ctrl Pts',(-2.407903564,4.428571429,7.102957161));
#140523=CARTESIAN_POINT('Ctrl Pts',(-2.028481621,4.365882895,7.231581257));
#140524=CARTESIAN_POINT('Ctrl Pts',(-1.637516375,4.302026826,7.319053226));
#140525=CARTESIAN_POINT('',(-2.11325074782748,4.43060907981219,6.93517636705374));
#140526=CARTESIAN_POINT('Origin',(0.0123907588393973,4.16114693626522,-0.190611787166877));
#140527=CARTESIAN_POINT('Ctrl Pts',(-2.18434923030009,4.39169923736146,
7.17486016828095));
#140528=CARTESIAN_POINT('Ctrl Pts',(-2.17238253565825,4.39788077311386,
7.1349076203884));
#140529=CARTESIAN_POINT('Ctrl Pts',(-2.16046488222165,4.4042094581219,7.09493786428154));
#140530=CARTESIAN_POINT('Ctrl Pts',(-2.13630354384551,4.41742211712242,
7.01349696440219));
#140531=CARTESIAN_POINT('Ctrl Pts',(-2.12462260024002,4.42401532021671,
6.97386214323707));
#140532=CARTESIAN_POINT('Ctrl Pts',(-2.11325074774409,4.4306090792906,6.9351763699027));
#140533=CARTESIAN_POINT('Ctrl Pts',(-2.85698451967887,4.30075163058632,
6.66334759239431));
#140534=CARTESIAN_POINT('Ctrl Pts',(-2.85337371733943,4.30138922829316,
6.66489113569716));
#140535=CARTESIAN_POINT('Ctrl Pts',(-2.849762915,4.302026826,6.666434679));
#140536=CARTESIAN_POINT('Ctrl Pts',(-2.486604518,4.36615356,6.821677381));
#140537=CARTESIAN_POINT('Ctrl Pts',(-2.108731308,4.431389364,6.93655190100001));
#140538=CARTESIAN_POINT('Ctrl Pts',(-2.72784872138814,4.30075163058632,
6.98633719228998));
#140539=CARTESIAN_POINT('Ctrl Pts',(-2.72406305119407,4.30138922829316,
6.98781060114499));
#140540=CARTESIAN_POINT('Ctrl Pts',(-2.720277381,4.302026826,6.98928401000001));
#140541=CARTESIAN_POINT('Ctrl Pts',(-2.339531555,4.36615356,7.137472902));
#140542=CARTESIAN_POINT('Ctrl Pts',(-1.944941241,4.431389364,7.243424851));
#140543=CARTESIAN_POINT('Origin',(0.0363027951225431,4.55345288672837,-0.189027909640508));
#140544=CARTESIAN_POINT('Ctrl Pts',(-3.558794191,4.431369595,6.316445512));
#140545=CARTESIAN_POINT('Ctrl Pts',(-3.551265944,4.429970133,6.320687056));
#140546=CARTESIAN_POINT('Ctrl Pts',(-3.543727607,4.428571429,6.324910643));
#140547=CARTESIAN_POINT('Ctrl Pts',(-3.205866935,4.365882895,6.514207577));
#140548=CARTESIAN_POINT('Ctrl Pts',(-2.849762915,4.302026826,6.666434679));
#140549=CARTESIAN_POINT('Ctrl Pts',(-3.89382449,4.431369595,6.410002406));
#140550=CARTESIAN_POINT('Ctrl Pts',(-3.886184737,4.429970133,6.414643255));
#140551=CARTESIAN_POINT('Ctrl Pts',(-3.878533944,4.428571429,6.419265881));
#140552=CARTESIAN_POINT('Ctrl Pts',(-3.535633054,4.365882895,6.626447319));
#140553=CARTESIAN_POINT('Ctrl Pts',(-3.172612246,4.302026826,6.795920213));
#140554=CARTESIAN_POINT('',(-3.55470203688038,4.43060907982634,6.3187493536364));
#140555=CARTESIAN_POINT('Origin',(0.053076451612849,4.16114717394356,-0.183490596981692));
#140556=CARTESIAN_POINT('Ctrl Pts',(-3.67566320760579,4.39169923737812,
6.53754540923891));
#140557=CARTESIAN_POINT('Ctrl Pts',(-3.65538767083827,4.39788077313931,
6.50109941524975));
#140558=CARTESIAN_POINT('Ctrl Pts',(-3.63515632942581,4.40420945817687,
6.46462607283171));
#140559=CARTESIAN_POINT('Ctrl Pts',(-3.5940520600491,4.417422253397,6.39028242292873));
#140560=CARTESIAN_POINT('Ctrl Pts',(-3.57412391075028,4.42401545916239,
6.35408531972618));
#140561=CARTESIAN_POINT('Ctrl Pts',(-3.55470203703904,4.43060907932611,
6.31874935621956));
#140562=CARTESIAN_POINT('Ctrl Pts',(-4.22261257419804,4.30075163058632,
5.89339500821418));
#140563=CARTESIAN_POINT('Ctrl Pts',(-4.21941800659903,4.30138922829316,
5.89567868010709));
#140564=CARTESIAN_POINT('Ctrl Pts',(-4.216223439,4.302026826,5.897962352));
#140565=CARTESIAN_POINT('Ctrl Pts',(-3.894928076,4.36615356,6.127643887));
#140566=CARTESIAN_POINT('Ctrl Pts',(-3.550583958,4.431389364,6.321064274));
#140567=CARTESIAN_POINT('Ctrl Pts',(-4.16592911596048,4.30075163058632,
6.23659367087182));
#140568=CARTESIAN_POINT('Ctrl Pts',(-4.16254869198024,4.30138922829316,
6.23884643943591));
#140569=CARTESIAN_POINT('Ctrl Pts',(-4.159168268,4.302026826,6.241099208));
#140570=CARTESIAN_POINT('Ctrl Pts',(-3.819180299,4.36615356,6.46767262400001));
#140571=CARTESIAN_POINT('Ctrl Pts',(-3.456591824,4.431389364,6.655972728));
#140572=CARTESIAN_POINT('Origin',(0.0760893310981942,4.55345288953098,-0.176804295814729));
#140573=CARTESIAN_POINT('Ctrl Pts',(-4.833440632,4.431369595,5.403734972));
#140574=CARTESIAN_POINT('Ctrl Pts',(-4.827000198,4.429970133,5.409495702));
#140575=CARTESIAN_POINT('Ctrl Pts',(-4.82054605,4.428571429,5.415241063));
#140576=CARTESIAN_POINT('Ctrl Pts',(-4.531277618,4.365882895,5.672742398));
#140577=CARTESIAN_POINT('Ctrl Pts',(-4.216223439,4.302026826,5.897962352));
#140578=CARTESIAN_POINT('Ctrl Pts',(-5.18075007600001,4.431369595,5.42308294700001));
#140579=CARTESIAN_POINT('Ctrl Pts',(-5.174286582,4.429970133,5.429257617));
#140580=CARTESIAN_POINT('Ctrl Pts',(-5.167808388,4.428571429,5.435416862));
#140581=CARTESIAN_POINT('Ctrl Pts',(-4.877462215,4.365882895,5.711468069));
#140582=CARTESIAN_POINT('Ctrl Pts',(-4.559360294,4.302026826,5.955017524));
#140583=CARTESIAN_POINT('',(-4.82993940821837,4.43060907984581,5.40686464364233));
#140584=CARTESIAN_POINT('Origin',(0.0912803947604635,4.16114721112737,-0.1677905457368));
#140585=CARTESIAN_POINT('Ctrl Pts',(-4.99510725948457,4.39169923740419,
5.59454229236904));
#140586=CARTESIAN_POINT('Ctrl Pts',(-4.96747094198499,4.3978807731843,5.56330702642334));
#140587=CARTESIAN_POINT('Ctrl Pts',(-4.93987190779603,4.40420945816489,
5.53203555112992));
#140588=CARTESIAN_POINT('Ctrl Pts',(-4.88374728278851,4.41742217412659,
5.46826659984238));
#140589=CARTESIAN_POINT('Ctrl Pts',(-4.8565037268247,4.42401537766957,5.43719972099938));
#140590=CARTESIAN_POINT('Ctrl Pts',(-4.82993941000097,4.43060907926912,
5.40686464621053));
#140591=CARTESIAN_POINT('Ctrl Pts',(-5.39079595785797,4.30075163058632,
4.84787382396709));
#140592=CARTESIAN_POINT('Ctrl Pts',(-5.38816699942899,4.30138922829316,
4.85079084248355));
#140593=CARTESIAN_POINT('Ctrl Pts',(-5.38553804100001,4.302026826,4.853707861));
#140594=CARTESIAN_POINT('Ctrl Pts',(-5.121129126,4.36615356,5.147088575));
#140595=CARTESIAN_POINT('Ctrl Pts',(-4.826415248,4.431389364,5.410010708));
#140596=CARTESIAN_POINT('Ctrl Pts',(-5.40921529476771,4.30075163058632,
5.19523396035998));
#140597=CARTESIAN_POINT('Ctrl Pts',(-5.40639818188385,4.30138922829316,
5.19816075168));
#140598=CARTESIAN_POINT('Ctrl Pts',(-5.403581069,4.302026826,5.201087543));
#140599=CARTESIAN_POINT('Ctrl Pts',(-5.12024841800001,4.36615356,5.495451162));
#140600=CARTESIAN_POINT('Ctrl Pts',(-4.806616016,4.431389364,5.757294719));
#140601=CARTESIAN_POINT('Origin',(0.112318141206794,4.55345288046685,-0.156313780444495));
#140602=CARTESIAN_POINT('Ctrl Pts',(-5.882080762,4.431369595,4.238351791));
#140603=CARTESIAN_POINT('Ctrl Pts',(-5.87702928800001,4.429970133,4.245362341));
#140604=CARTESIAN_POINT('Ctrl Pts',(-5.871961118,4.428571429,4.25236083));
#140605=CARTESIAN_POINT('Ctrl Pts',(-5.64481079600001,4.365882895,4.566026089));
#140606=CARTESIAN_POINT('Ctrl Pts',(-5.38553804100001,4.302026826,4.853707861));
#140607=CARTESIAN_POINT('Ctrl Pts',(-6.225429547,4.431369595,4.182586157));
#140608=CARTESIAN_POINT('Ctrl Pts',(-6.220444537,4.429970133,4.190005926));
#140609=CARTESIAN_POINT('Ctrl Pts',(-6.215441855,4.428571429,4.197413792));
#140610=CARTESIAN_POINT('Ctrl Pts',(-5.991226664,4.365882895,4.52942692));
#140611=CARTESIAN_POINT('Ctrl Pts',(-5.732917723,4.302026826,4.835664834));
#140612=CARTESIAN_POINT('',(-5.87933418163029,4.43060907985417,4.2421609519141));
#140613=CARTESIAN_POINT('Origin',(0.125218936516226,4.16114644057551,-0.144247389551539));
#140614=CARTESIAN_POINT('Ctrl Pts',(-6.08098564645014,4.39169923736635,
4.38994459618127));
#140615=CARTESIAN_POINT('Ctrl Pts',(-6.04728079196535,4.39788077313033,
4.36538058482446));
#140616=CARTESIAN_POINT('Ctrl Pts',(-6.01360456489737,4.40420945815512,
4.34077319563697));
#140617=CARTESIAN_POINT('Ctrl Pts',(-5.94508333958322,4.41742223651246,
4.29056002530658));
#140618=CARTESIAN_POINT('Ctrl Pts',(-5.91179827121222,4.42401544155975,
4.26607603671574));
#140619=CARTESIAN_POINT('Ctrl Pts',(-5.87933418351883,4.43060907933619,
4.2421609540683));
#140620=CARTESIAN_POINT('Ctrl Pts',(-6.30691171418917,4.30075163058632,
3.57567144780525));
#140621=CARTESIAN_POINT('Ctrl Pts',(-6.30497129209458,4.30138922829316,
3.57908541640262));
#140622=CARTESIAN_POINT('Ctrl Pts',(-6.30303087,4.302026826,3.582499385));
#140623=CARTESIAN_POINT('Ctrl Pts',(-6.107871869,4.36615356,3.925861122));
#140624=CARTESIAN_POINT('Ctrl Pts',(-5.876568725,4.431389364,4.245991053));
#140625=CARTESIAN_POINT('Ctrl Pts',(-6.399572578477,4.30075163058632,3.91095088387329));
#140626=CARTESIAN_POINT('Ctrl Pts',(-6.3974505017385,4.30138922829316,3.91441484443665));
#140627=CARTESIAN_POINT('Ctrl Pts',(-6.39532842500001,4.302026826,3.917878805));
#140628=CARTESIAN_POINT('Ctrl Pts',(-6.18189941,4.36615356,4.266268511));
#140629=CARTESIAN_POINT('Ctrl Pts',(-5.931888184,4.431389364,4.589412007));
#140630=CARTESIAN_POINT('Origin',(0.143295128420577,4.55345292751047,-0.128514236351981));
#140631=CARTESIAN_POINT('Ctrl Pts',(-6.65244799782001,4.431369595,2.87607070805));
#140632=CARTESIAN_POINT('Ctrl Pts',(-6.64902015702,4.429970133,2.8839994194));
#140633=CARTESIAN_POINT('Ctrl Pts',(-6.64557342641,4.428571429,2.89191993712));
#140634=CARTESIAN_POINT('Ctrl Pts',(-6.49109440281,4.365882895,3.24690960173));
#140635=CARTESIAN_POINT('Ctrl Pts',(-6.2996770758,4.302026826,3.58342236054));
#140636=CARTESIAN_POINT('Ctrl Pts',(-6.655681333,4.431369595,2.874787991));
#140637=CARTESIAN_POINT('Ctrl Pts',(-6.652255021,4.429970133,2.882720556));
#140638=CARTESIAN_POINT('Ctrl Pts',(-6.64880981,4.428571429,2.890644931));
#140639=CARTESIAN_POINT('Ctrl Pts',(-6.494398894,4.365882895,3.245807475));
#140640=CARTESIAN_POINT('Ctrl Pts',(-6.30303087,4.302026826,3.582499385));
#140641=CARTESIAN_POINT('Ctrl Pts',(-6.979014851,4.431369595,2.746516286));
#140642=CARTESIAN_POINT('Ctrl Pts',(-6.975741419,4.429970133,2.754834216));
#140643=CARTESIAN_POINT('Ctrl Pts',(-6.972448169,4.428571429,2.763144319));
#140644=CARTESIAN_POINT('Ctrl Pts',(-6.824848013,4.365882895,3.135594802));
#140645=CARTESIAN_POINT('Ctrl Pts',(-6.63841029,4.302026826,3.490201831));
#140646=CARTESIAN_POINT('',(-6.65381782292298,4.43060907982855,2.87909852931941));
#140647=CARTESIAN_POINT('Origin',(0.153300462456629,4.16114644726734,-0.113956670212826));
#140648=CARTESIAN_POINT('Ctrl Pts',(-6.88252390360049,4.39169923737952,
2.98007796986011));
#140649=CARTESIAN_POINT('Ctrl Pts',(-6.84432651354025,4.3978807731492,2.96333379889397));
#140650=CARTESIAN_POINT('Ctrl Pts',(-6.80614775662989,4.40420945817943,
2.94654111021513));
#140651=CARTESIAN_POINT('Ctrl Pts',(-6.7284342824622,4.41742221776468,2.91223198283376));
#140652=CARTESIAN_POINT('Ctrl Pts',(-6.69066405869933,4.42401542328448,
2.89547571962815));
#140653=CARTESIAN_POINT('Ctrl Pts',(-6.6538178243887,4.43060907942241,2.87909853129467));
#140654=CARTESIAN_POINT('Ctrl Pts',(-6.92812328853911,4.30075163058632,
2.13627464941378));
#140655=CARTESIAN_POINT('Ctrl Pts',(-6.92696213476955,4.30138922829316,
2.14002593470689));
#140656=CARTESIAN_POINT('Ctrl Pts',(-6.925800981,4.302026826,2.14377722));
#140657=CARTESIAN_POINT('Ctrl Pts',(-6.809017313,4.36615356,2.521064766));
#140658=CARTESIAN_POINT('Ctrl Pts',(-6.651940379,4.431389364,2.883433576));
#140659=CARTESIAN_POINT('Ctrl Pts',(-7.09069296127744,4.30075163058632,
2.44379609126981));
#140660=CARTESIAN_POINT('Ctrl Pts',(-7.08936514663872,4.30138922829316,
2.44763525013491));
#140661=CARTESIAN_POINT('Ctrl Pts',(-7.088037332,4.302026826,2.451474409));
#140662=CARTESIAN_POINT('Ctrl Pts',(-6.954491657,4.36615356,2.837599887));
#140663=CARTESIAN_POINT('Ctrl Pts',(-6.779791854,4.431389364,3.20693349));
#140664=CARTESIAN_POINT('Origin',(0.167571566098508,4.55345287895314,-0.0947053690531868));
#140665=CARTESIAN_POINT('Ctrl Pts',(-7.118069642,4.431369595,1.376802299));
#140666=CARTESIAN_POINT('Ctrl Pts',(-7.116428702,4.429970133,1.385285961));
#140667=CARTESIAN_POINT('Ctrl Pts',(-7.114767544,4.428571429,1.393765687));
#140668=CARTESIAN_POINT('Ctrl Pts',(-7.040316119,4.365882895,1.77381851));
#140669=CARTESIAN_POINT('Ctrl Pts',(-6.925800981,4.302026826,2.14377722));
#140670=CARTESIAN_POINT('Ctrl Pts',(-7.406269177,4.431369595,1.182022367));
#140671=CARTESIAN_POINT('Ctrl Pts',(-7.404860385,4.429970133,1.190849519));
#140672=CARTESIAN_POINT('Ctrl Pts',(-7.403430556,4.428571429,1.199673288));
#140673=CARTESIAN_POINT('Ctrl Pts',(-7.339347054,4.365882895,1.595145757));
#140674=CARTESIAN_POINT('Ctrl Pts',(-7.233498171,4.302026826,1.981540869));
#140675=CARTESIAN_POINT('',(-7.11717633793565,4.43060907981108,1.38141265923023));
#140676=CARTESIAN_POINT('Origin',(0.174211298471878,4.16114702584248,-0.0783366564974439));
#140677=CARTESIAN_POINT('Ctrl Pts',(-7.36224299279149,4.39169923741886,
1.43086620946198));
#140678=CARTESIAN_POINT('Ctrl Pts',(-7.32133913467307,4.39788077316404,
1.42272481765021));
#140679=CARTESIAN_POINT('Ctrl Pts',(-7.28044304443845,4.40420945813066,
1.41453203690386));
#140680=CARTESIAN_POINT('Ctrl Pts',(-7.19717121000547,4.41742218750417,
1.39773117588273));
#140681=CARTESIAN_POINT('Ctrl Pts',(-7.15668193244824,4.4240153913157,1.38948614686132));
#140682=CARTESIAN_POINT('Ctrl Pts',(-7.11717634035813,4.4306090793536,1.38141266056319));
#140683=CARTESIAN_POINT('Ctrl Pts',(-7.2253835183998,4.30075163058632,0.596988021858047));
#140684=CARTESIAN_POINT('Ctrl Pts',(-7.22505592719991,4.30138922829316,
0.600901217929024));
#140685=CARTESIAN_POINT('Ctrl Pts',(-7.224728336,4.302026826,0.604814414));
#140686=CARTESIAN_POINT('Ctrl Pts',(-7.191780674,4.36615356,0.998386223999999));
#140687=CARTESIAN_POINT('Ctrl Pts',(-7.116274695,4.431389364,1.38604995));
#140688=CARTESIAN_POINT('Ctrl Pts',(-7.45026042179122,4.30075163058632,
0.862372109285386));
#140689=CARTESIAN_POINT('Ctrl Pts',(-7.44978895639561,4.30138922829316,
0.866406951642693));
#140690=CARTESIAN_POINT('Ctrl Pts',(-7.449317491,4.302026826,0.870441794));
#140691=CARTESIAN_POINT('Ctrl Pts',(-7.401899604,4.36615356,1.276248245));
#140692=CARTESIAN_POINT('Ctrl Pts',(-7.310679993,4.431389364,1.674502328));
#140693=CARTESIAN_POINT('Origin',(0.184013027002503,4.55345292796302,-0.0564683324674287));
#140694=CARTESIAN_POINT('Ctrl Pts',(-7.247624926,4.431369595,-0.185561138));
#140695=CARTESIAN_POINT('Ctrl Pts',(-7.247846087,4.429970133,-0.176923066));
#140696=CARTESIAN_POINT('Ctrl Pts',(-7.248046656,4.428571429,-0.168284491));
#140697=CARTESIAN_POINT('Ctrl Pts',(-7.257035987,4.365882895,0.218887764));
#140698=CARTESIAN_POINT('Ctrl Pts',(-7.224728336,4.302026826,0.604814414));
#140699=CARTESIAN_POINT('Ctrl Pts',(-7.487214588,4.431369595,-0.437741604));
#140700=CARTESIAN_POINT('Ctrl Pts',(-7.48773631,4.429970133,-0.428817978));
#140701=CARTESIAN_POINT('Ctrl Pts',(-7.488236759,4.428571429,-0.419893133));
#140702=CARTESIAN_POINT('Ctrl Pts',(-7.510666384,4.365882895,-0.019890532));
#140703=CARTESIAN_POINT('Ctrl Pts',(-7.490355716,4.302026826,0.380225258));
#140704=CARTESIAN_POINT('',(-7.24774359797091,4.43060907983566,-0.180866531823111));
#140705=CARTESIAN_POINT('Origin',(0.186975432915708,4.16114763470212,-0.0390547221848561));
#140706=CARTESIAN_POINT('Ctrl Pts',(-7.49771178198432,4.39169923736833,
-0.185251264675212));
#140707=CARTESIAN_POINT('Ctrl Pts',(-7.45601407454653,4.39788077315963,
-0.184409194783559));
#140708=CARTESIAN_POINT('Ctrl Pts',(-7.41431290627343,4.40420945817067,
-0.183618982244392));
#140709=CARTESIAN_POINT('Ctrl Pts',(-7.32937619817061,4.41742219290252,
-0.182126064751352));
#140710=CARTESIAN_POINT('Ctrl Pts',(-7.28806110256997,4.42401539652318,
-0.181474331916151));
#140711=CARTESIAN_POINT('Ctrl Pts',(-7.24774360024735,4.43060907935805,
-0.180866530270858));
#140712=CARTESIAN_POINT('Ctrl Pts',(-7.18479284462103,4.30075163058632,
-0.970213102287846));
#140713=CARTESIAN_POINT('Ctrl Pts',(-7.18531413381051,4.30138922829316,
-0.966320972143922));
#140714=CARTESIAN_POINT('Ctrl Pts',(-7.185835423,4.302026826,-0.962428842));
#140715=CARTESIAN_POINT('Ctrl Pts',(-7.238264365,4.36615356,-0.570975749));
#140716=CARTESIAN_POINT('Ctrl Pts',(-7.24785991500001,4.431389364,-0.176143831));
#140717=CARTESIAN_POINT('Ctrl Pts',(-7.46146198490312,4.30075163058632,
-0.759375434223065));
#140718=CARTESIAN_POINT('Ctrl Pts',(-7.46186891395157,4.30138922829316,
-0.755333573111533));
#140719=CARTESIAN_POINT('Ctrl Pts',(-7.462275843,4.302026826,-0.751291712));
#140720=CARTESIAN_POINT('Ctrl Pts',(-7.503202952,4.36615356,-0.344779346));
#140721=CARTESIAN_POINT('Ctrl Pts',(-7.49972886,4.431389364,0.063773298));
#140722=CARTESIAN_POINT('Origin',(0.191849688360268,4.55345288722648,-0.0155907848465334));
#140723=CARTESIAN_POINT('Ctrl Pts',(-7.038289323,4.431369595,-1.739247943));
#140724=CARTESIAN_POINT('Ctrl Pts',(-7.040362243,4.429970133,-1.730859367));
#140725=CARTESIAN_POINT('Ctrl Pts',(-7.042415162,4.428571429,-1.722465874));
#140726=CARTESIAN_POINT('Ctrl Pts',(-7.134424917,4.365882895,-1.346277931));
#140727=CARTESIAN_POINT('Ctrl Pts',(-7.185835423,4.302026826,-0.962428842));
#140728=CARTESIAN_POINT('Ctrl Pts',(-7.218066166,4.431369595,-2.037037265));
#140729=CARTESIAN_POINT('Ctrl Pts',(-7.220494006,4.429970133,-2.028434422));
#140730=CARTESIAN_POINT('Ctrl Pts',(-7.222901333,4.428571429,-2.019825817));
#140731=CARTESIAN_POINT('Ctrl Pts',(-7.330795302,4.365882895,-1.633996761));
#140732=CARTESIAN_POINT('Ctrl Pts',(-7.396972553,4.302026826,-1.238869262));
#140733=CARTESIAN_POINT('',(-7.03941442235693,4.4306090798324,-1.73468860429048));
#140734=CARTESIAN_POINT('Origin',(0.191005240678206,4.16114639188231,0.00205339969632512));
#140735=CARTESIAN_POINT('Ctrl Pts',(-7.28259590116914,4.39169923740785,
-1.79270659508165));
#140736=CARTESIAN_POINT('Ctrl Pts',(-7.24205408327968,4.39788077315036,
-1.7829204379314));
#140737=CARTESIAN_POINT('Ctrl Pts',(-7.20149773745199,4.40420945814961,
-1.773184181719));
#140738=CARTESIAN_POINT('Ctrl Pts',(-7.1188672875784,4.41742226448833,-1.75346717962484));
#140739=CARTESIAN_POINT('Ctrl Pts',(-7.07865822430606,4.42401547082464,
-1.74394916249829));
#140740=CARTESIAN_POINT('Ctrl Pts',(-7.03941442481537,4.43060907931634,
-1.73468860419115));
#140741=CARTESIAN_POINT('Ctrl Pts',(-6.80824924266725,4.30075163058632,
-2.49204813906551));
#140742=CARTESIAN_POINT('Ctrl Pts',(-6.80959503733362,4.30138922829316,
-2.48835906653276));
#140743=CARTESIAN_POINT('Ctrl Pts',(-6.81094083200001,4.302026826,-2.484669994));
#140744=CARTESIAN_POINT('Ctrl Pts',(-6.946294858,4.36615356,-2.11363953));
#140745=CARTESIAN_POINT('Ctrl Pts',(-7.040543261,4.431389364,-1.730101323));
#140746=CARTESIAN_POINT('Ctrl Pts',(-7.12377387913241,4.30075163058632,
-2.3456154258534));
#140747=CARTESIAN_POINT('Ctrl Pts',(-7.12504017506621,4.30138922829316,
-2.3417555389267));
#140748=CARTESIAN_POINT('Ctrl Pts',(-7.126306471,4.302026826,-2.337895652));
#140749=CARTESIAN_POINT('Ctrl Pts',(-7.253664869,4.36615356,-1.949685438));
#140750=CARTESIAN_POINT('Ctrl Pts',(-7.33809874,4.431389364,-1.549937701));
#140751=CARTESIAN_POINT('Origin',(0.190715988738417,4.55345289011465,0.0260157603670164));
#140752=CARTESIAN_POINT('Ctrl Pts',(-6.499851134,4.431369595,-3.211609446));
#140753=CARTESIAN_POINT('Ctrl Pts',(-6.503678886,4.429970133,-3.203862607));
#140754=CARTESIAN_POINT('Ctrl Pts',(-6.507488162,4.428571429,-3.196106666));
#140755=CARTESIAN_POINT('Ctrl Pts',(-6.678216068,4.365882895,-2.848493166));
#140756=CARTESIAN_POINT('Ctrl Pts',(-6.810940832,4.302026826,-2.484669994));
#140757=CARTESIAN_POINT('Ctrl Pts',(-6.611408993,4.431369595,-3.541083327));
#140758=CARTESIAN_POINT('Ctrl Pts',(-6.615629428,4.429970133,-3.533203528));
#140759=CARTESIAN_POINT('Ctrl Pts',(-6.619831069,4.428571429,-3.525313691));
#140760=CARTESIAN_POINT('Ctrl Pts',(-6.80814437800001,4.365882895,-3.171699118));
#140761=CARTESIAN_POINT('Ctrl Pts',(-6.957715175,4.302026826,-2.800035633));
#140762=CARTESIAN_POINT('',(-6.50193005203167,4.43060907982022,-3.2073985659925));
#140763=CARTESIAN_POINT('Origin',(0.186097995353229,4.16114642092722,0.043065778632051));
#140764=CARTESIAN_POINT('Ctrl Pts',(-6.72695393012471,4.39169923738952,
-3.31633695786171));
#140765=CARTESIAN_POINT('Ctrl Pts',(-6.68946369205208,4.39788077312887,
-3.29806430321486));
#140766=CARTESIAN_POINT('Ctrl Pts',(-6.65194853850495,4.40420945811866,
-3.27983725979241));
#140767=CARTESIAN_POINT('Ctrl Pts',(-6.57548829283599,4.41742230292223,
-3.24281801837052));
#140768=CARTESIAN_POINT('Ctrl Pts',(-6.53826539478635,4.42401550976215,
-3.22487877186494));
#140769=CARTESIAN_POINT('Ctrl Pts',(-6.50193005463137,4.43060907935782,
-3.20739856646714));
#140770=CARTESIAN_POINT('Ctrl Pts',(-6.11335947344275,4.30075163058632,
-3.89735777600252));
#140771=CARTESIAN_POINT('Ctrl Pts',(-6.11546684572138,4.30138922829316,
-3.89404425800126));
#140772=CARTESIAN_POINT('Ctrl Pts',(-6.117574218,4.30202682600001,-3.89073074));
#140773=CARTESIAN_POINT('Ctrl Pts',(-6.329524324,4.36615356,-3.557471876));
#140774=CARTESIAN_POINT('Ctrl Pts',(-6.504018629,4.431389364,-3.2031612));
#140775=CARTESIAN_POINT('Ctrl Pts',(-6.45298602455971,4.30075163058632,
-3.8221770474411));
#140776=CARTESIAN_POINT('Ctrl Pts',(-6.45505247677986,4.30138922829316,
-3.81867961872055));
#140777=CARTESIAN_POINT('Ctrl Pts',(-6.457118929,4.30202682600001,-3.81518219));
#140778=CARTESIAN_POINT('Ctrl Pts',(-6.664953478,4.36615356,-3.463426406));
#140779=CARTESIAN_POINT('Ctrl Pts',(-6.83334728,4.431389364,-3.091175335));
#140780=CARTESIAN_POINT('Origin',(0.180664648443238,4.55345290995932,0.0664058816356417));
#140781=CARTESIAN_POINT('Ctrl Pts',(-5.65748713,4.431369595,-4.533799662));
#140782=CARTESIAN_POINT('Ctrl Pts',(-5.662890733,4.429970133,-4.527056793));
#140783=CARTESIAN_POINT('Ctrl Pts',(-5.668278248,4.428571429,-4.520301063));
#140784=CARTESIAN_POINT('Ctrl Pts',(-5.90974125700001,4.365882895,-4.217516027));
#140785=CARTESIAN_POINT('Ctrl Pts',(-6.11757421800001,4.302026826,-3.89073074));
#140786=CARTESIAN_POINT('Ctrl Pts',(-5.695609683,4.431369595,-4.879552268));
#140787=CARTESIAN_POINT('Ctrl Pts',(-5.701425371,4.429970133,-4.872763963));
#140788=CARTESIAN_POINT('Ctrl Pts',(-5.707224861,4.428571429,-4.865961815));
#140789=CARTESIAN_POINT('Ctrl Pts',(-5.96715219,4.365882895,-4.561096349));
#140790=CARTESIAN_POINT('Ctrl Pts',(-6.193122768,4.302026826,-4.23027545));
#140791=CARTESIAN_POINT('',(-5.66042265901053,4.43060907979696,-4.53013413550827));
#140792=CARTESIAN_POINT('Origin',(0.172489379695488,4.16114643978824,0.0820645868625702));
#140793=CARTESIAN_POINT('Ctrl Pts',(-5.85676706945755,4.39169923740779,
-4.68489909035697));
#140794=CARTESIAN_POINT('Ctrl Pts',(-5.82408141295841,4.39788077313851,
-4.65899434735462));
#140795=CARTESIAN_POINT('Ctrl Pts',(-5.79136161844954,4.40420945811769,
-4.63312879310501));
#140796=CARTESIAN_POINT('Ctrl Pts',(-5.72464727543306,4.41742225104424,
-4.58053855480103));
#140797=CARTESIAN_POINT('Ctrl Pts',(-5.69215102468486,4.42401545785814,
-4.55501688435888));
#140798=CARTESIAN_POINT('Ctrl Pts',(-5.66042266160367,4.43060907930436,
-4.5301341366984));
#140799=CARTESIAN_POINT('Ctrl Pts',(-5.13261580896174,4.30075163058632,
-5.12043129408338));
#140800=CARTESIAN_POINT('Ctrl Pts',(-5.13538622048087,4.30138922829316,
-5.11764826704169));
#140801=CARTESIAN_POINT('Ctrl Pts',(-5.138156632,4.302026826,-5.11486524));
#140802=CARTESIAN_POINT('Ctrl Pts',(-5.416792268,4.36615356,-4.834960791));
#140803=CARTESIAN_POINT('Ctrl Pts',(-5.663373315,4.431389364,-4.526444819));
#140804=CARTESIAN_POINT('Ctrl Pts',(-5.48046371397504,4.30075163058632,
-5.12001791827923));
#140805=CARTESIAN_POINT('Ctrl Pts',(-5.48323369748752,4.30138922829316,
-5.11704648363962));
#140806=CARTESIAN_POINT('Ctrl Pts',(-5.486003681,4.302026826,-5.114075049));
#140807=CARTESIAN_POINT('Ctrl Pts',(-5.76459627,4.36615356,-4.815221404));
#140808=CARTESIAN_POINT('Ctrl Pts',(-6.009076095,4.431389364,-4.487873047));
#140809=CARTESIAN_POINT('Origin',(0.162165348725356,4.55345290765384,0.103690775807935));
#140810=CARTESIAN_POINT('Ctrl Pts',(-4.550585316,4.431369595,-5.643994444));
#140811=CARTESIAN_POINT('Ctrl Pts',(-4.557312103,4.429970133,-5.638570835));
#140812=CARTESIAN_POINT('Ctrl Pts',(-4.564025943,4.428571429,-5.633131207));
#140813=CARTESIAN_POINT('Ctrl Pts',(-4.864933514,4.365882895,-5.389332525));
#140814=CARTESIAN_POINT('Ctrl Pts',(-5.138156632,4.302026826,-5.11486524));
#140815=CARTESIAN_POINT('Ctrl Pts',(-4.513489995,4.431369595,-5.989858769));
#140816=CARTESIAN_POINT('Ctrl Pts',(-4.520629,4.429970133,-5.984479372));
#140817=CARTESIAN_POINT('Ctrl Pts',(-4.527755162,4.428571429,-5.979082973));
#140818=CARTESIAN_POINT('Ctrl Pts',(-4.847142598,4.365882895,-5.737221784));
#140819=CARTESIAN_POINT('Ctrl Pts',(-5.138946823,4.302026826,-5.462712289));
#140820=CARTESIAN_POINT('',(-4.55424019369446,4.4306090798157,-5.64104566757866));
#140821=CARTESIAN_POINT('Origin',(0.150815320472325,4.16114637789378,0.117226175772075));
#140822=CARTESIAN_POINT('Ctrl Pts',(-4.71272429052055,4.39169923737066,
-5.83440054806061));
#140823=CARTESIAN_POINT('Ctrl Pts',(-4.68637156050115,4.39788077310936,
-5.80207499348842));
#140824=CARTESIAN_POINT('Ctrl Pts',(-4.65997706604305,4.40420945812496,
-5.76978037268453));
#140825=CARTESIAN_POINT('Ctrl Pts',(-4.60612778558633,4.41742225800792,
-5.70407801870093));
#140826=CARTESIAN_POINT('Ctrl Pts',(-4.57987769065069,4.4240154632115,-5.67216730675844));
#140827=CARTESIAN_POINT('Ctrl Pts',(-4.55424019597839,4.43060907930317,
-5.64104566923627));
#140828=CARTESIAN_POINT('Ctrl Pts',(-3.91187673525438,4.30075163058632,
-6.10407913568028));
#140829=CARTESIAN_POINT('Ctrl Pts',(-3.91518064462719,4.30138922829316,
-6.10195673084014));
#140830=CARTESIAN_POINT('Ctrl Pts',(-3.918484554,4.302026826,-6.099834326));
#140831=CARTESIAN_POINT('Ctrl Pts',(-4.250777025,4.36615356,-5.886372312));
#140832=CARTESIAN_POINT('Ctrl Pts',(-4.557914959,4.431389364,-5.638076909));
#140833=CARTESIAN_POINT('Ctrl Pts',(-4.25168101209463,4.30075163058632,
-6.17845244216063));
#140834=CARTESIAN_POINT('Ctrl Pts',(-4.25502500554731,4.30138922829316,
-6.17614594258032));
#140835=CARTESIAN_POINT('Ctrl Pts',(-4.258368999,4.302026826,-6.17383944300001));
#140836=CARTESIAN_POINT('Ctrl Pts',(-4.594692948,4.36615356,-5.941862001));
#140837=CARTESIAN_POINT('Ctrl Pts',(-4.903827191,4.431389364,-5.674722802));
#140838=CARTESIAN_POINT('Origin',(0.136083798206303,4.55345291224455,0.136127620145613));
#140839=CARTESIAN_POINT('Ctrl Pts',(-3.23090319,4.431369595,-6.490282319));
#140840=CARTESIAN_POINT('Ctrl Pts',(-3.238638624,4.429970133,-6.486431571));
#140841=CARTESIAN_POINT('Ctrl Pts',(-3.246364857,4.428571429,-6.482562396));
#140842=CARTESIAN_POINT('Ctrl Pts',(-3.592646886,4.365882895,-6.30914982500001));
#140843=CARTESIAN_POINT('Ctrl Pts',(-3.918484554,4.302026826,-6.099834326));
#140844=CARTESIAN_POINT('Ctrl Pts',(-3.120324531,4.431369595,-6.82008613));
#140845=CARTESIAN_POINT('Ctrl Pts',(-3.128453041,4.429970133,-6.816367176));
#140846=CARTESIAN_POINT('Ctrl Pts',(-3.136572664,4.428571429,-6.812628856));
#140847=CARTESIAN_POINT('Ctrl Pts',(-3.500486005,4.365882895,-6.64508110500001));
#140848=CARTESIAN_POINT('Ctrl Pts',(-3.844479437,4.302026826,-6.43971877199999));
#140849=CARTESIAN_POINT('',(-3.23510651809109,4.43060907984298,-6.48818817439076));
#140850=CARTESIAN_POINT('Origin',(0.122089187039252,4.16114645729476,0.146906377531372));
#140851=CARTESIAN_POINT('Ctrl Pts',(-3.34831976121393,4.3916992374112,-6.71109192096717));
#140852=CARTESIAN_POINT('Ctrl Pts',(-3.32953218197703,4.39788077316559,
-6.67385706182384));
#140853=CARTESIAN_POINT('Ctrl Pts',(-3.31069716493212,4.4042094581807,-6.63664343517182));
#140854=CARTESIAN_POINT('Ctrl Pts',(-3.27223093014627,4.41742225272145,
-6.56090119261109));
#140855=CARTESIAN_POINT('Ctrl Pts',(-3.25345441215866,4.42401545580878,
-6.52409355054411));
#140856=CARTESIAN_POINT('Ctrl Pts',(-3.23510652026311,4.43060907931498,
-6.48818817582034));
#140857=CARTESIAN_POINT('Ctrl Pts',(-2.50822265177515,4.30075163058632,
-6.80230702168494));
#140858=CARTESIAN_POINT('Ctrl Pts',(-2.51190557188757,4.30138922829316,
-6.80094448034247));
#140859=CARTESIAN_POINT('Ctrl Pts',(-2.515588492,4.302026826,-6.799581939));
#140860=CARTESIAN_POINT('Ctrl Pts',(-2.886000173,4.36615356,-6.66254360700001));
#140861=CARTESIAN_POINT('Ctrl Pts',(-3.239333565,4.431389364,-6.486078789));
#140862=CARTESIAN_POINT('Ctrl Pts',(-2.82409443206748,4.30075163058632,
-6.94798939631561));
#140863=CARTESIAN_POINT('Ctrl Pts',(-2.82785607403374,4.30138922829316,
-6.9464556811578));
#140864=CARTESIAN_POINT('Ctrl Pts',(-2.831617716,4.302026826,-6.944921966));
#140865=CARTESIAN_POINT('Ctrl Pts',(-3.20994689,4.36615356,-6.79066773500001));
#140866=CARTESIAN_POINT('Ctrl Pts',(-3.569280777,4.431389364,-6.596228827));
#140867=CARTESIAN_POINT('Origin',(0.103638799473347,4.5534529061386,0.162198973411815));
#140868=CARTESIAN_POINT('Ctrl Pts',(-1.760147622,4.431369595,-7.033091806));
#140869=CARTESIAN_POINT('Ctrl Pts',(-1.768530003,4.429970133,-7.030993976));
#140870=CARTESIAN_POINT('Ctrl Pts',(-1.776907359,4.428571429,-7.028876172));
#140871=CARTESIAN_POINT('Ctrl Pts',(-2.152372083,4.365882895,-6.933958291));
#140872=CARTESIAN_POINT('Ctrl Pts',(-2.515588492,4.302026826,-6.799581939));
#140873=CARTESIAN_POINT('Ctrl Pts',(-1.581256159,4.431369595,-7.331413844));
#140874=CARTESIAN_POINT('Ctrl Pts',(-1.589994095,4.429970133,-7.329529226));
#140875=CARTESIAN_POINT('Ctrl Pts',(-1.598727514,4.428571429,-7.327623785));
#140876=CARTESIAN_POINT('Ctrl Pts',(-1.990150577,4.365882895,-7.242223819));
#140877=CARTESIAN_POINT('Ctrl Pts',(-2.370248465,4.302026826,-7.115611162));
#140878=CARTESIAN_POINT('',(-1.7647028575926,4.43060907985456,-7.03195021221419));
#140879=CARTESIAN_POINT('Origin',(0.087654253277924,4.16114647010977,0.169717275906408));
#140880=CARTESIAN_POINT('Ctrl Pts',(-1.82735152120739,4.39169923740398,
-7.27398009430452));
#140881=CARTESIAN_POINT('Ctrl Pts',(-1.81700757923929,4.39788077317501,
-7.23357699113929));
#140882=CARTESIAN_POINT('Ctrl Pts',(-1.80661274423284,4.40420945816821,
-7.1931844266176));
#140883=CARTESIAN_POINT('Ctrl Pts',(-1.78532820116453,4.41742223458717,
-7.11094400505928));
#140884=CARTESIAN_POINT('Ctrl Pts',(-1.774903222269,4.42401543741975,-7.07096050504536));
#140885=CARTESIAN_POINT('Ctrl Pts',(-1.76470285943447,4.43060907931923,
-7.03195021485679));
#140886=CARTESIAN_POINT('Ctrl Pts',(-0.987286864787932,4.30075163058632,
-7.182466590834));
#140887=CARTESIAN_POINT('Ctrl Pts',(-0.991176586393966,4.30138922829316,
-7.181927623917));
#140888=CARTESIAN_POINT('Ctrl Pts',(-0.995066308,4.302026826,-7.181388657));
#140889=CARTESIAN_POINT('Ctrl Pts',(-1.386277161,4.36615356,-7.127181768));
#140890=CARTESIAN_POINT('Ctrl Pts',(-1.769284534,4.431389364,-7.030798834));
#140891=CARTESIAN_POINT('Ctrl Pts',(-1.2644563344217,4.30075163058632,-7.39264608882629));
#140892=CARTESIAN_POINT('Ctrl Pts',(-1.26845973471085,4.30138922829316,
-7.39195687291315));
#140893=CARTESIAN_POINT('Ctrl Pts',(-1.272463135,4.302026826,-7.391267657));
#140894=CARTESIAN_POINT('Ctrl Pts',(-1.675107283,4.36615356,-7.321949394));
#140895=CARTESIAN_POINT('Ctrl Pts',(-2.067838762,4.431389364,-7.209302522));
#140896=CARTESIAN_POINT('Origin',(0.0663477542198945,4.55345291749259,0.180685933335134));
#140897=CARTESIAN_POINT('Ctrl Pts',(-0.20947790199,4.431369595,-7.24451282641));
#140898=CARTESIAN_POINT('Ctrl Pts',(-0.21811226492,4.429970133,-7.24426316081));
#140899=CARTESIAN_POINT('Ctrl Pts',(-0.22674600806,4.428571429,-7.24399291339));
#140900=CARTESIAN_POINT('Ctrl Pts',(-0.61370172234,4.365882895,-7.23188071676));
#140901=CARTESIAN_POINT('Ctrl Pts',(-0.997165097989999,4.302026826,-7.17861468873));
#140902=CARTESIAN_POINT('Ctrl Pts',(-0.207089507,4.431369595,-7.247041737));
#140903=CARTESIAN_POINT('Ctrl Pts',(-0.215726884,4.429970133,-7.246794918));
#140904=CARTESIAN_POINT('Ctrl Pts',(-0.224363648,4.428571429,-7.24652751));
#140905=CARTESIAN_POINT('Ctrl Pts',(-0.611454754,4.365882895,-7.234542573));
#140906=CARTESIAN_POINT('Ctrl Pts',(-0.995066308,4.302026826,-7.181388657));
#140907=CARTESIAN_POINT('Ctrl Pts',(0.031749992,4.431369595,-7.499932796));
#140908=CARTESIAN_POINT('Ctrl Pts',(0.022811208,4.429970133,-7.499970637));
#140909=CARTESIAN_POINT('Ctrl Pts',(0.013872358,4.428571429,-7.499987171));
#140910=CARTESIAN_POINT('Ctrl Pts',(-0.38675792,4.365882895,-7.500728197));
#140911=CARTESIAN_POINT('Ctrl Pts',(-0.785187309,4.302026826,-7.458785484));
#140912=CARTESIAN_POINT('',(-0.211783652922208,4.43060907981772,-7.2469060743844));
#140913=CARTESIAN_POINT('Origin',(0.0491207418811837,4.16114636362922,0.18459210558284));
#140914=CARTESIAN_POINT('Ctrl Pts',(-0.22093835562386,4.39169923735867,
-7.4967450430742));
#140915=CARTESIAN_POINT('Ctrl Pts',(-0.219521722060892,4.39788077308784,
-7.45506290053831));
#140916=CARTESIAN_POINT('Ctrl Pts',(-0.218053119813242,4.40420945810867,
-7.41338010930172));
#140917=CARTESIAN_POINT('Ctrl Pts',(-0.214945473836398,4.41742216317101,
-7.32848733401049));
#140918=CARTESIAN_POINT('Ctrl Pts',(-0.213359497213433,4.42401536555907,
-7.2871975450429));
#140919=CARTESIAN_POINT('Ctrl Pts',(-0.211783654082422,4.43060907940009,
-7.24690607660022));
#140920=CARTESIAN_POINT('Ctrl Pts',(0.579813358054801,4.30075163058632,
-7.22678200501259));
#140921=CARTESIAN_POINT('Ctrl Pts',(0.5758987140274,4.30138922829316,-7.22709181400629));
#140922=CARTESIAN_POINT('Ctrl Pts',(0.57198407,4.302026826,-7.227401623));
#140923=CARTESIAN_POINT('Ctrl Pts',(0.178266631,4.36615356,-7.25856083));
#140924=CARTESIAN_POINT('Ctrl Pts',(-0.216505724,4.431389364,-7.246766539));
#140925=CARTESIAN_POINT('Ctrl Pts',(0.354306336144935,4.30075163058632,
-7.49163086539554));
#140926=CARTESIAN_POINT('Ctrl Pts',(0.350248372072468,4.30138922829316,
-7.49181837569778));
#140927=CARTESIAN_POINT('Ctrl Pts',(0.346190408,4.302026826,-7.49200588600001));
#140928=CARTESIAN_POINT('Ctrl Pts',(-0.061941522,4.36615356,-7.510864836));
#140929=CARTESIAN_POINT('Ctrl Pts',(-0.469706904,4.431389364,-7.48527724400001));
#140930=CARTESIAN_POINT('Origin',(0.0259544467066953,4.55345291197526,0.190724426768116));
#140931=CARTESIAN_POINT('Ctrl Pts',(1.355651883,4.431369595,-7.12212805100001));
#140932=CARTESIAN_POINT('Ctrl Pts',(1.347163385,4.429970133,-7.12374378300001));
#140933=CARTESIAN_POINT('Ctrl Pts',(1.338671059,4.428571429,-7.125339276));
#140934=CARTESIAN_POINT('Ctrl Pts',(0.95805352,4.365882895,-7.196847686));
#140935=CARTESIAN_POINT('Ctrl Pts',(0.57198407,4.302026826,-7.227401623));
#140936=CARTESIAN_POINT('Ctrl Pts',(1.64327155,4.431369595,-7.317763225));
#140937=CARTESIAN_POINT('Ctrl Pts',(1.634549884,4.429970133,-7.319721756));
#140938=CARTESIAN_POINT('Ctrl Pts',(1.625823574,4.428571429,-7.321659491));
#140939=CARTESIAN_POINT('Ctrl Pts',(1.234719107,4.365882895,-7.40850686));
#140940=CARTESIAN_POINT('Ctrl Pts',(0.836588333,4.302026826,-7.453195285));
#140941=CARTESIAN_POINT('',(1.35103832001141,4.4306090798317,-7.12300466238332));
#140942=CARTESIAN_POINT('Origin',(0.00829069334600696,4.16114701816254,
0.190833578894729));
#140943=CARTESIAN_POINT('Ctrl Pts',(1.39580564292763,4.39169923738768,-7.36897052522756));
#140944=CARTESIAN_POINT('Ctrl Pts',(1.38822872775217,4.39788077315009,-7.32795835342677));
#140945=CARTESIAN_POINT('Ctrl Pts',(1.38070242688303,4.40420945812951,-7.2869343768277));
#140946=CARTESIAN_POINT('Ctrl Pts',(1.36548790457561,4.41742222896235,-7.20335787923211));
#140947=CARTESIAN_POINT('Ctrl Pts',(1.35816072347522,4.42401543119208,-7.16269250411706));
#140948=CARTESIAN_POINT('Ctrl Pts',(1.35103831922291,4.43060907936442,-7.12300466481012));
#140949=CARTESIAN_POINT('Ctrl Pts',(2.11980215310686,4.30075163058632,-6.93318112482194));
#140950=CARTESIAN_POINT('Ctrl Pts',(2.11604563105343,4.30138922829316,-6.93432522341097));
#140951=CARTESIAN_POINT('Ctrl Pts',(2.112289109,4.302026826,-6.935469322));
#140952=CARTESIAN_POINT('Ctrl Pts',(1.734474873,4.36615356,-7.05053765600001));
#140953=CARTESIAN_POINT('Ctrl Pts',(1.346396652,4.431389364,-7.123883495));
#140954=CARTESIAN_POINT('Ctrl Pts',(1.95650203590071,4.30075163058632,-7.24031531054044));
#140955=CARTESIAN_POINT('Ctrl Pts',(1.95257925395036,4.30138922829316,-7.24137077927022));
#140956=CARTESIAN_POINT('Ctrl Pts',(1.948656472,4.302026826,-7.242426248));
#140957=CARTESIAN_POINT('Ctrl Pts',(1.554120557,4.36615356,-7.348580586));
#140958=CARTESIAN_POINT('Ctrl Pts',(1.150387927,4.431389364,-7.411248722));
#140959=CARTESIAN_POINT('Origin',(-0.0156524015817822,4.55345290941761,
0.191844575301596));
#140960=CARTESIAN_POINT('Ctrl Pts',(2.855004498,4.431369595,-6.664191573));
#140961=CARTESIAN_POINT('Ctrl Pts',(2.84706179,4.429970133,-6.667594306));
#140962=CARTESIAN_POINT('Ctrl Pts',(2.839110994,4.428571429,-6.670978097));
#140963=CARTESIAN_POINT('Ctrl Pts',(2.482764276,4.365882895,-6.8226362));
#140964=CARTESIAN_POINT('Ctrl Pts',(2.112289109,4.302026826,-6.935469322));
#140965=CARTESIAN_POINT('Ctrl Pts',(3.177955556,4.431369595,-6.793423179));
#140966=CARTESIAN_POINT('Ctrl Pts',(3.169858824,4.429970133,-6.797210821));
#140967=CARTESIAN_POINT('Ctrl Pts',(3.161753086,4.428571429,-6.800979152));
#140968=CARTESIAN_POINT('Ctrl Pts',(2.798462042,4.365882895,-6.969871977));
#140969=CARTESIAN_POINT('Ctrl Pts',(2.419246034,4.302026826,-7.099101959));
#140970=CARTESIAN_POINT('',(2.85068724288564,4.43060907986153,-6.66603946941678));
#140971=CARTESIAN_POINT('Origin',(-0.0329275039884303,4.16114638744478,
0.188156706573089));
#140972=CARTESIAN_POINT('Ctrl Pts',(2.94728332000655,4.39169923738661,-6.8966311360963));
#140973=CARTESIAN_POINT('Ctrl Pts',(2.93106714437857,4.39788077313744,-6.8582066190441));
#140974=CARTESIAN_POINT('Ctrl Pts',(2.91489786188011,4.40420945817505,-6.81975969218555));
#140975=CARTESIAN_POINT('Ctrl Pts',(2.88207248593745,4.41742226301248,-6.7414076377763));
#140976=CARTESIAN_POINT('Ctrl Pts',(2.86617475262101,4.42401546888816,-6.70326811363609));
#140977=CARTESIAN_POINT('Ctrl Pts',(2.85068724309641,4.43060907936564,-6.66603947211694));
#140978=CARTESIAN_POINT('Ctrl Pts',(3.56067135454208,4.30075163058632,-6.31539240121984));
#140979=CARTESIAN_POINT('Ctrl Pts',(3.55724860527104,4.30138922829316,-6.31731729260992));
#140980=CARTESIAN_POINT('Ctrl Pts',(3.553825856,4.30202682600001,-6.319242184));
#140981=CARTESIAN_POINT('Ctrl Pts',(3.209580998,4.36615356,-6.51283917600001));
#140982=CARTESIAN_POINT('Ctrl Pts',(2.846343018,4.431389364,-6.66789557700001));
#140983=CARTESIAN_POINT('Ctrl Pts',(3.46721387482592,4.30075163058632,-6.65045065775765));
#140984=CARTESIAN_POINT('Ctrl Pts',(3.46360969991296,4.30138922829316,-6.65232473237882));
#140985=CARTESIAN_POINT('Ctrl Pts',(3.460005525,4.30202682600001,-6.654198807));
#140986=CARTESIAN_POINT('Ctrl Pts',(3.097513685,4.36615356,-6.842684875));
#140987=CARTESIAN_POINT('Ctrl Pts',(2.716691897,4.431389364,-6.990678446));
#140988=CARTESIAN_POINT('Origin',(-0.0565274918812825,4.55345289725118,
0.183994782434824));
#140989=CARTESIAN_POINT('Ctrl Pts',(4.220860275,4.431369595,-5.894644903));
#140990=CARTESIAN_POINT('Ctrl Pts',(4.213834751,4.429970133,-5.89967553000001));
#140991=CARTESIAN_POINT('Ctrl Pts',(4.206797255,4.428571429,-5.904689396));
#140992=CARTESIAN_POINT('Ctrl Pts',(3.891383734,4.365882895,-6.129405827));
#140993=CARTESIAN_POINT('Ctrl Pts',(3.553825856,4.302026826,-6.319242184));
#140994=CARTESIAN_POINT('Ctrl Pts',(4.564041892,4.431369595,-5.951430215));
#140995=CARTESIAN_POINT('Ctrl Pts',(4.55694868800001,4.429970133,-5.956869862));
#140996=CARTESIAN_POINT('Ctrl Pts',(4.549842538,4.428571429,-5.962292586));
#140997=CARTESIAN_POINT('Ctrl Pts',(4.231352001,4.365882895,-6.205333626));
#140998=CARTESIAN_POINT('Ctrl Pts',(3.88878248,4.302026826,-6.413062515));
#140999=CARTESIAN_POINT('',(4.21704119835812,4.43060907984144,-5.89737767934635));
#141000=CARTESIAN_POINT('Origin',(-0.0726058677300551,4.16114640939035,
0.176679351281246));
#141001=CARTESIAN_POINT('Ctrl Pts',(4.36094930547041,4.39169923740635,-6.10181293976727));
#141002=CARTESIAN_POINT('Ctrl Pts',(4.33685211954446,4.39788077316035,-6.0677727649374));
#141003=CARTESIAN_POINT('Ctrl Pts',(4.31279591317222,4.40420945814279,-6.03370062390091));
#141004=CARTESIAN_POINT('Ctrl Pts',(4.26389471364212,4.41742223236811,-5.96423704339406));
#141005=CARTESIAN_POINT('Ctrl Pts',(4.24016977758101,4.42401544004617,-5.93040672751236));
#141006=CARTESIAN_POINT('Ctrl Pts',(4.2170411989522,4.43060907934584,-5.89737768176648));
#141007=CARTESIAN_POINT('Ctrl Pts',(4.83504752209277,4.30075163058632,-5.40230294817827));
#141008=CARTESIAN_POINT('Ctrl Pts',(4.83211858954639,4.30138922829316,-5.40491862658914));
#141009=CARTESIAN_POINT('Ctrl Pts',(4.829189657,4.302026826,-5.40753430500001));
#141010=CARTESIAN_POINT('Ctrl Pts',(4.53461068300001,4.36615356,-5.670607575));
#141011=CARTESIAN_POINT('Ctrl Pts',(4.213197547,4.431389364,-5.900124272));
#141012=CARTESIAN_POINT('Ctrl Pts',(4.81580264731597,4.30075163058632,-5.74961832426662));
#141013=CARTESIAN_POINT('Ctrl Pts',(4.81268560665798,4.30138922829316,-5.75222337513331));
#141014=CARTESIAN_POINT('Ctrl Pts',(4.809568566,4.302026826,-5.754828426));
#141015=CARTESIAN_POINT('Ctrl Pts',(4.496070517,4.36615356,-6.01683282500001));
#141016=CARTESIAN_POINT('Ctrl Pts',(4.155966373,4.431389364,-6.243231816));
#141017=CARTESIAN_POINT('Origin',(-0.0947593468897162,4.55345286736327,
0.1675413508447));
#141018=CARTESIAN_POINT('Ctrl Pts',(5.38587966315001,4.431369595,-4.84965435201));
#141019=CARTESIAN_POINT('Ctrl Pts',(5.38009960985,4.429970133,-4.85607350493001));
#141020=CARTESIAN_POINT('Ctrl Pts',(5.37430427041,4.428571429,-4.86247886236));
#141021=CARTESIAN_POINT('Ctrl Pts',(5.1145629917,4.365882895,-5.14956055579));
#141022=CARTESIAN_POINT('Ctrl Pts',(4.82571671579,4.302026826,-5.40733809408999));
#141023=CARTESIAN_POINT('Ctrl Pts',(5.38935331700001,4.431369595,-4.84947119));
#141024=CARTESIAN_POINT('Ctrl Pts',(5.383573482,4.429970133,-4.855894483));
#141025=CARTESIAN_POINT('Ctrl Pts',(5.377778351,4.428571429,-4.862303981));
#141026=CARTESIAN_POINT('Ctrl Pts',(5.118046414,4.365882895,-5.149571251));
#141027=CARTESIAN_POINT('Ctrl Pts',(4.829189657,4.302026826,-5.407534305));
#141028=CARTESIAN_POINT('Ctrl Pts',(5.736718702,4.431369595,-4.831154989));
#141029=CARTESIAN_POINT('Ctrl Pts',(5.730960697,4.429970133,-4.83799229));
#141030=CARTESIAN_POINT('Ctrl Pts',(5.72518641,4.428571429,-4.844815845));
#141031=CARTESIAN_POINT('Ctrl Pts',(5.46638864400001,4.365882895,-5.150640772));
#141032=CARTESIAN_POINT('Ctrl Pts',(5.176483778,4.302026826,-5.427155396));
#141033=CARTESIAN_POINT('',(5.38621099464683,4.43060907978048,-4.85296106368865));
#141034=CARTESIAN_POINT('Origin',(-0.108889318602821,4.16114639848255,0.156940670217498));
#141035=CARTESIAN_POINT('Ctrl Pts',(5.57070214744086,4.39169923734938,-5.02168075233251));
#141036=CARTESIAN_POINT('Ctrl Pts',(5.53985070913859,4.39788077309921,-4.99361660052216));
#141037=CARTESIAN_POINT('Ctrl Pts',(5.50903242037404,4.4042094581094,-4.96551242031131));
#141038=CARTESIAN_POINT('Ctrl Pts',(5.44634166948302,4.4174222782979,-4.90818497253391));
#141039=CARTESIAN_POINT('Ctrl Pts',(5.41589892139967,4.42401548178228,-4.88024577479643));
#141040=CARTESIAN_POINT('Ctrl Pts',(5.38621099577858,4.43060907934932,-4.85296106598922));
#141041=CARTESIAN_POINT('Ctrl Pts',(5.8833422403708,4.30075163058632,-4.23660781253323));
#141042=CARTESIAN_POINT('Ctrl Pts',(5.88104407818541,4.30138922829316,-4.23979197176662));
#141043=CARTESIAN_POINT('Ctrl Pts',(5.878745916,4.302026826,-4.242976131));
#141044=CARTESIAN_POINT('Ctrl Pts',(5.647607012,4.36615356,-4.563224667));
#141045=CARTESIAN_POINT('Ctrl Pts',(5.383047642,4.431389364,-4.856469714));
#141046=CARTESIAN_POINT('Ctrl Pts',(5.93920983909918,4.30075163058632,-4.57994022835198));
#141047=CARTESIAN_POINT('Ctrl Pts',(5.93672568204959,4.30138922829316,-4.58315444617599));
#141048=CARTESIAN_POINT('Ctrl Pts',(5.93424152499999,4.302026826,-4.58636866399999));
#141049=CARTESIAN_POINT('Ctrl Pts',(5.684396087,4.36615356,-4.909640359));
#141050=CARTESIAN_POINT('Ctrl Pts',(5.40091248,4.431389364,-5.20385860500001));
#141051=CARTESIAN_POINT('Origin',(-0.128560173577943,4.55345288250795,0.143253706416722));
#141052=CARTESIAN_POINT('Ctrl Pts',(6.30584618800001,4.431369595,-3.577541593));
#141053=CARTESIAN_POINT('Ctrl Pts',(6.3015823,4.429970133,-3.585057207));
#141054=CARTESIAN_POINT('Ctrl Pts',(6.297300509,4.428571429,-3.592562637));
#141055=CARTESIAN_POINT('Ctrl Pts',(6.105394932,4.365882895,-3.928948446));
#141056=CARTESIAN_POINT('Ctrl Pts',(5.878745916,4.302026826,-4.242976131));
#141057=CARTESIAN_POINT('Ctrl Pts',(6.641152922,4.431369595,-3.484980325));
#141058=CARTESIAN_POINT('Ctrl Pts',(6.636999353,4.429970133,-3.492895575));
#141059=CARTESIAN_POINT('Ctrl Pts',(6.632826928,4.428571429,-3.5008009));
#141060=CARTESIAN_POINT('Ctrl Pts',(6.44582303,4.365882895,-3.855109679));
#141061=CARTESIAN_POINT('Ctrl Pts',(6.222138449,4.302026826,-4.187480522));
#141062=CARTESIAN_POINT('',(6.30352755149585,4.43060907983456,-3.58162538195155));
#141063=CARTESIAN_POINT('Origin',(-0.140080817418023,4.16114641568227,0.129863282877415));
#141064=CARTESIAN_POINT('Ctrl Pts',(6.51997514917063,4.39169923735847,-3.70674035357318));
#141065=CARTESIAN_POINT('Ctrl Pts',(6.48381203713831,4.39788077312318,-3.6859644733829));
#141066=CARTESIAN_POINT('Ctrl Pts',(6.4476726947445,4.40420945814442,-3.66514237449988));
#141067=CARTESIAN_POINT('Ctrl Pts',(6.37412364237302,4.41742232677805,-3.62263171337457));
#141068=CARTESIAN_POINT('Ctrl Pts',(6.33838650801649,4.42401553650283,-3.6018899985056));
#141069=CARTESIAN_POINT('Ctrl Pts',(6.30352755295668,4.43060907926899,-3.58162538425232));
#141070=CARTESIAN_POINT('Ctrl Pts',(6.65653841463485,4.30075163058632,-2.87281360540941));
#141071=CARTESIAN_POINT('Ctrl Pts',(6.65497848231742,4.30138922829316,-2.87641735770471));
#141072=CARTESIAN_POINT('Ctrl Pts',(6.65341855,4.302026826,-2.88002111));
#141073=CARTESIAN_POINT('Ctrl Pts',(6.49652751400001,4.36615356,-3.242470445));
#141074=CARTESIAN_POINT('Ctrl Pts',(6.301192412,4.431389364,-3.58573203));
#141075=CARTESIAN_POINT('Ctrl Pts',(6.78490618103697,4.30075163058632,-3.1961092169402));
#141076=CARTESIAN_POINT('Ctrl Pts',(6.78317106401849,4.30138922829316,-3.1997823084701));
#141077=CARTESIAN_POINT('Ctrl Pts',(6.781435947,4.302026826,-3.2034554));
#141078=CARTESIAN_POINT('Ctrl Pts',(6.606925615,4.36615356,-3.572878566));
#141079=CARTESIAN_POINT('Ctrl Pts',(6.393317923,4.431389364,-3.921158749));
#141080=CARTESIAN_POINT('Origin',(-0.156349827180969,4.55345287947972,0.112267878198957));
#141081=CARTESIAN_POINT('Ctrl Pts',(6.9274847,4.431369595,-2.138330128));
#141082=CARTESIAN_POINT('Ctrl Pts',(6.924936134,4.429970133,-2.146586641));
#141083=CARTESIAN_POINT('Ctrl Pts',(6.922367894,4.428571429,-2.154837056));
#141084=CARTESIAN_POINT('Ctrl Pts',(6.807261968,4.365882895,-2.524612378));
#141085=CARTESIAN_POINT('Ctrl Pts',(6.65341854999999,4.302026826,-2.88002111));
#141086=CARTESIAN_POINT('Ctrl Pts',(7.235054212,4.431369595,-1.975851855));
#141087=CARTESIAN_POINT('Ctrl Pts',(7.232699295,4.429970133,-1.984474945));
#141088=CARTESIAN_POINT('Ctrl Pts',(7.230323831,4.428571429,-1.993092396));
#141089=CARTESIAN_POINT('Ctrl Pts',(7.123857894,4.365882895,-2.379317943));
#141090=CARTESIAN_POINT('Ctrl Pts',(6.976852841,4.302026826,-2.752003713));
#141091=CARTESIAN_POINT('',(6.92609816488622,4.43060907984139,-2.14281687848));
#141092=CARTESIAN_POINT('Origin',(-0.164720287169465,4.16114706774232,0.0967129603737812));
#141093=CARTESIAN_POINT('Ctrl Pts',(7.16438135887083,4.39169923737064,-2.21847689612214));
#141094=CARTESIAN_POINT('Ctrl Pts',(7.12459752024601,4.39788077311949,-2.20596074454318));
#141095=CARTESIAN_POINT('Ctrl Pts',(7.08482695982538,4.40420945813223,-2.19339434504391));
#141096=CARTESIAN_POINT('Ctrl Pts',(7.00385935975969,4.41742225301334,-2.16768857502343));
#141097=CARTESIAN_POINT('Ctrl Pts',(6.96449889674919,4.42401545667019,-2.15511422210393));
#141098=CARTESIAN_POINT('Ctrl Pts',(6.92609816709728,4.43060907932906,-2.14281688041309));
#141099=CARTESIAN_POINT('Ctrl Pts',(7.11848225152532,4.30075163058632,-1.37468982618827));
#141100=CARTESIAN_POINT('Ctrl Pts',(7.11773348976266,4.30138922829316,-1.37854466409414));
#141101=CARTESIAN_POINT('Ctrl Pts',(7.116984728,4.302026826,-1.382399502));
#141102=CARTESIAN_POINT('Ctrl Pts',(7.041677609,4.36615356,-1.770101908));
#141103=CARTESIAN_POINT('Ctrl Pts',(6.92470042800001,4.431389364,-2.147329501));
#141104=CARTESIAN_POINT('Ctrl Pts',(7.31334784967157,4.30075163058632,-1.66283169087053));
#141105=CARTESIAN_POINT('Ctrl Pts',(7.31244290483579,4.30138922829316,-1.66679190643526));
#141106=CARTESIAN_POINT('Ctrl Pts',(7.31153796,4.302026826,-1.670752122));
#141107=CARTESIAN_POINT('Ctrl Pts',(7.220522644,4.36615356,-2.069052943));
#141108=CARTESIAN_POINT('Ctrl Pts',(7.086778925,4.431389364,-2.455109868));
#141109=CARTESIAN_POINT('Origin',(-0.176829096811765,4.55345290497252,0.0760326273964132));
#141110=CARTESIAN_POINT('Ctrl Pts',(7.225201726,4.431369595,-0.599132722));
#141111=CARTESIAN_POINT('Ctrl Pts',(7.22448765,4.429970133,-0.607744069));
#141112=CARTESIAN_POINT('Ctrl Pts',(7.22375305,4.428571429,-0.616353689));
#141113=CARTESIAN_POINT('Ctrl Pts',(7.190829,4.365882895,-1.002228242));
#141114=CARTESIAN_POINT('Ctrl Pts',(7.116984728,4.302026826,-1.382399502));
#141115=CARTESIAN_POINT('Ctrl Pts',(7.490652408,4.431369595,-0.374334748));
#141116=CARTESIAN_POINT('Ctrl Pts',(7.490206258,4.429970133,-0.383262472));
#141117=CARTESIAN_POINT('Ctrl Pts',(7.489738828,4.428571429,-0.392189107));
#141118=CARTESIAN_POINT('Ctrl Pts',(7.468789081,4.365882895,-0.792271945));
#141119=CARTESIAN_POINT('Ctrl Pts',(7.405337348,4.302026826,-1.187846269));
#141120=CARTESIAN_POINT('',(7.22481212632807,4.430609079793,-0.6038126392582));
#141121=CARTESIAN_POINT('Origin',(-0.181662538350398,4.16114641014556,0.0590423734243478));
#141122=CARTESIAN_POINT('Ctrl Pts',(7.47378905908835,4.39169923737829,-0.626479925186403));
#141123=CARTESIAN_POINT('Ctrl Pts',(7.43224474213264,4.39788077308007,-0.622808743525736));
#141124=CARTESIAN_POINT('Ctrl Pts',(7.390702590998,4.4042094580625,-0.619085634240142));
#141125=CARTESIAN_POINT('Ctrl Pts',(7.30610202033978,4.41742224782026,-0.61138649412038));
#141126=CARTESIAN_POINT('Ctrl Pts',(7.26495866855288,4.42401545126193,-0.607567458551672));
#141127=CARTESIAN_POINT('Ctrl Pts',(7.22481212871226,4.43060907931025,-0.603812640279783));
#141128=CARTESIAN_POINT('Ctrl Pts',(7.24757376884405,4.30075163058632,0.187712921172618));
#141129=CARTESIAN_POINT('Ctrl Pts',(7.24767118892203,4.30138922829316,0.183787245586309));
#141130=CARTESIAN_POINT('Ctrl Pts',(7.247768609,4.302026826,0.17986157));
#141131=CARTESIAN_POINT('Ctrl Pts',(7.257566686,4.36615356,-0.214965374));
#141132=CARTESIAN_POINT('Ctrl Pts',(7.224417148,4.431389364,-0.608520231));
#141133=CARTESIAN_POINT('Ctrl Pts',(7.49982550189696,4.30075163058632,-0.051802003363299));
#141134=CARTESIAN_POINT('Ctrl Pts',(7.49979304344848,4.30138922829316,-0.0558641676816495));
#141135=CARTESIAN_POINT('Ctrl Pts',(7.499760585,4.302026826,-0.059926332));
#141136=CARTESIAN_POINT('Ctrl Pts',(7.496496059,4.36615356,-0.468480704));
#141137=CARTESIAN_POINT('Ctrl Pts',(7.448870021,4.431389364,-0.874262779));
#141138=CARTESIAN_POINT('Origin',(-0.189039560576475,4.55345292231119,0.0362419940865541));
#141139=CARTESIAN_POINT('Ctrl Pts',(7.18507635,4.431369595,0.968079464000001));
#141140=CARTESIAN_POINT('Ctrl Pts',(7.186230154,4.429970133,0.959515940000001));
#141141=CARTESIAN_POINT('Ctrl Pts',(7.187363542,4.428571429,0.95094969));
#141142=CARTESIAN_POINT('Ctrl Pts',(7.238160861,4.365882895,0.567018973000001));
#141143=CARTESIAN_POINT('Ctrl Pts',(7.247768609,4.302026826,0.17986157));
#141144=CARTESIAN_POINT('Ctrl Pts',(7.395996023,4.431369595,1.244685836));
#141145=CARTESIAN_POINT('Ctrl Pts',(7.3974795,4.429970133,1.235870928));
#141146=CARTESIAN_POINT('Ctrl Pts',(7.398941961,4.428571429,1.227052509));
#141147=CARTESIAN_POINT('Ctrl Pts',(7.464487991,4.365882895,0.83181981));
#141148=CARTESIAN_POINT('Ctrl Pts',(7.487556512,4.302026826,0.431853546));
#141149=CARTESIAN_POINT('',(7.18570190260038,4.43060907983529,0.96342520766656));
#141150=CARTESIAN_POINT('Origin',(-0.190105587267123,4.16114681587434,0.0186100314583489));
#141151=CARTESIAN_POINT('Ctrl Pts',(7.43373068926963,4.39169923741219,0.994810551909341));
#141152=CARTESIAN_POINT('Ctrl Pts',(7.39236845954255,4.39788077317017,0.989465103128073));
#141153=CARTESIAN_POINT('Ctrl Pts',(7.35099718228765,4.40420945818285,0.984170833502881));
#141154=CARTESIAN_POINT('Ctrl Pts',(7.2667195205937,4.41742223508709,0.973503360110972));
#141155=CARTESIAN_POINT('Ctrl Pts',(7.22571707860693,4.4240154411964,0.96838850065241));
#141156=CARTESIAN_POINT('Ctrl Pts',(7.18570190540487,4.43060907928109,0.96342520723106));
#141157=CARTESIAN_POINT('Ctrl Pts',(7.03777679268802,4.30075163058632,1.74133842106059));
#141158=CARTESIAN_POINT('Ctrl Pts',(7.03871583934401,4.30138922829316,1.73752546803029));
#141159=CARTESIAN_POINT('Ctrl Pts',(7.03965488600001,4.302026826,1.733712515));
#141160=CARTESIAN_POINT('Ctrl Pts',(7.134100011,4.36615356,1.350222703));
#141161=CARTESIAN_POINT('Ctrl Pts',(7.186328152,4.431389364,0.958742768));
#141162=CARTESIAN_POINT('Ctrl Pts',(7.33561964867258,4.30075163058632,1.56164988855367));
#141163=CARTESIAN_POINT('Ctrl Pts',(7.33646119433629,4.30138922829316,1.55767571777684));
#141164=CARTESIAN_POINT('Ctrl Pts',(7.33730274,4.302026826,1.553701547));
#141165=CARTESIAN_POINT('Ctrl Pts',(7.42194165,4.36615356,1.153997173));
#141166=CARTESIAN_POINT('Ctrl Pts',(7.462660234,4.431389364,0.747463866999999));
#141167=CARTESIAN_POINT('Origin',(-0.192410959441722,4.5534528786585,-0.00524326309890105));
#141168=CARTESIAN_POINT('Ctrl Pts',(6.808984789,4.431369595,2.49002533));
#141169=CARTESIAN_POINT('Ctrl Pts',(6.811952522,4.429970133,2.48191005));
#141170=CARTESIAN_POINT('Ctrl Pts',(6.814900903,4.428571429,2.47378772));
#141171=CARTESIAN_POINT('Ctrl Pts',(6.947044364,4.365882895,2.109753011));
#141172=CARTESIAN_POINT('Ctrl Pts',(7.039654886,4.302026826,1.733712515));
#141173=CARTESIAN_POINT('Ctrl Pts',(6.955511084,4.431369595,2.805506294));
#141174=CARTESIAN_POINT('Ctrl Pts',(6.958854823,4.429970133,2.797216377));
#141175=CARTESIAN_POINT('Ctrl Pts',(6.962178791,4.428571429,2.788918514));
#141176=CARTESIAN_POINT('Ctrl Pts',(7.11115573900001,4.365882895,2.417016594));
#141177=CARTESIAN_POINT('Ctrl Pts',(7.219665854,4.302026826,2.031360369));
#141178=CARTESIAN_POINT('',(6.81059624420884,4.43060907983355,2.48561436300287));
#141179=CARTESIAN_POINT('Origin',(-0.189663453657438,4.16114641601856,-0.0226926354563547));
#141180=CARTESIAN_POINT('Ctrl Pts',(7.04607933419032,4.3916992374152,2.56958479291152));
#141181=CARTESIAN_POINT('Ctrl Pts',(7.00683324387289,4.39788077317029,2.55547266099481));
#141182=CARTESIAN_POINT('Ctrl Pts',(6.96756731588636,4.40420945812354,2.54140856685183));
#141183=CARTESIAN_POINT('Ctrl Pts',(6.88755313080646,4.41742224818086,2.51287325847989));
#141184=CARTESIAN_POINT('Ctrl Pts',(6.8486088500697,4.42401545432448,2.49906367011868));
#141185=CARTESIAN_POINT('Ctrl Pts',(6.81059624670237,4.43060907928598,2.48561436286732));
#141186=CARTESIAN_POINT('Ctrl Pts',(6.4989011950665,4.30075163058632,3.21354087208441));
#141187=CARTESIAN_POINT('Ctrl Pts',(6.50063795953325,4.30138922829316,3.2100189310422));
#141188=CARTESIAN_POINT('Ctrl Pts',(6.50237472400001,4.302026826,3.20649699));
#141189=CARTESIAN_POINT('Ctrl Pts',(6.677050749,4.36615356,2.852275866));
#141190=CARTESIAN_POINT('Ctrl Pts',(6.812214438,4.431389364,2.481176021));
#141191=CARTESIAN_POINT('Ctrl Pts',(6.82840837392086,4.30075163058632,3.10208076685929));
#141192=CARTESIAN_POINT('Ctrl Pts',(6.83008457396043,4.30138922829316,3.09838041742964));
#141193=CARTESIAN_POINT('Ctrl Pts',(6.83176077400001,4.302026826,3.094680068));
#141194=CARTESIAN_POINT('Ctrl Pts',(7.000345499,4.36615356,2.722515424));
#141195=CARTESIAN_POINT('Ctrl Pts',(7.127504748,4.431389364,2.334239933));
#141196=CARTESIAN_POINT('Origin',(-0.186785148316219,4.55345291235534,-0.0464832497892625));
#141197=CARTESIAN_POINT('Ctrl Pts',(6.1137598519,4.431369595,3.89214433884));
#141198=CARTESIAN_POINT('Ctrl Pts',(6.11839869934,4.429970133,3.88485766207));
#141199=CARTESIAN_POINT('Ctrl Pts',(6.12302016393,4.428571429,3.87755994896));
#141200=CARTESIAN_POINT('Ctrl Pts',(6.33014957445,4.365882895,3.55048375274));
#141201=CARTESIAN_POINT('Ctrl Pts',(6.50125655478,4.302026826,3.2032031295));
#141202=CARTESIAN_POINT('Ctrl Pts',(6.114512667,4.431369595,3.895540379));
#141203=CARTESIAN_POINT('Ctrl Pts',(6.119155562,4.429970133,3.888252805));
#141204=CARTESIAN_POINT('Ctrl Pts',(6.123781072,4.428571429,3.880954185));
#141205=CARTESIAN_POINT('Ctrl Pts',(6.331091794,4.365882895,3.553837343));
#141206=CARTESIAN_POINT('Ctrl Pts',(6.502374724,4.302026826,3.20649699));
#141207=CARTESIAN_POINT('Ctrl Pts',(6.189794177,4.431369595,4.235144395));
#141208=CARTESIAN_POINT('Ctrl Pts',(6.194841828,4.429970133,4.227767098));
#141209=CARTESIAN_POINT('Ctrl Pts',(6.199871879,4.428571429,4.220377789));
#141210=CARTESIAN_POINT('Ctrl Pts',(6.425313749,4.365882895,3.889196369));
#141211=CARTESIAN_POINT('Ctrl Pts',(6.614191646,4.302026826,3.53588304));
#141212=CARTESIAN_POINT('',(6.11703467512379,4.43060907974158,3.89157895330898));
#141213=CARTESIAN_POINT('Origin',(-0.180351123952476,4.16114643519017,-0.0629342094358598));
#141214=CARTESIAN_POINT('Ctrl Pts',(6.3289611410797,4.39169923740138,4.02420810481511));
#141215=CARTESIAN_POINT('Ctrl Pts',(6.29366629386744,4.3978807731276,4.00198915746816));
#141216=CARTESIAN_POINT('Ctrl Pts',(6.25834174588008,4.40420945808978,3.97981286015401));
#141217=CARTESIAN_POINT('Ctrl Pts',(6.18633291490832,4.41742217123992,3.93474426914271));
#141218=CARTESIAN_POINT('Ctrl Pts',(6.15126776957677,4.42401537644418,3.91288566100586));
#141219=CARTESIAN_POINT('Ctrl Pts',(6.11703467769023,4.43060907925216,3.89157895377656));
#141220=CARTESIAN_POINT('Ctrl Pts',(5.65614420082141,4.30075163058632,4.53548172299218));
#141221=CARTESIAN_POINT('Ctrl Pts',(5.6585974739107,4.30138922829316,4.53241547599609));
#141222=CARTESIAN_POINT('Ctrl Pts',(5.661050747,4.302026826,4.529349229));
#141223=CARTESIAN_POINT('Ctrl Pts',(5.907790014,4.36615356,4.22095978));
#141224=CARTESIAN_POINT('Ctrl Pts',(6.119569149,4.431389364,3.887592241));
#141225=CARTESIAN_POINT('Ctrl Pts',(6.00190831268338,4.30075163058632,4.49746179671396));
#141226=CARTESIAN_POINT('Ctrl Pts',(6.00434078984169,4.30138922829316,4.49420829285698));
#141227=CARTESIAN_POINT('Ctrl Pts',(6.00677326700001,4.302026826,4.490954789));
#141228=CARTESIAN_POINT('Ctrl Pts',(6.251420972,4.36615356,4.16373188));
#141229=CARTESIAN_POINT('Ctrl Pts',(6.45907506200001,4.431389364,3.811869534));
#141230=CARTESIAN_POINT('Origin',(-0.172425869120202,4.55345290385811,-0.0855499160282613));
#141231=CARTESIAN_POINT('Ctrl Pts',(5.13412756255,4.431369595,5.11542581336999));
#141232=CARTESIAN_POINT('Ctrl Pts',(5.14022437574001,4.429970133,5.10930671053));
#141233=CARTESIAN_POINT('Ctrl Pts',(5.14630658595,4.428571429,5.10317309157));
#141234=CARTESIAN_POINT('Ctrl Pts',(5.4189051398,4.365882895,4.82827045646));
#141235=CARTESIAN_POINT('Ctrl Pts',(5.6606668026,4.302026826,4.5258920038));
#141236=CARTESIAN_POINT('Ctrl Pts',(5.134132729,4.431369595,5.118904289));
#141237=CARTESIAN_POINT('Ctrl Pts',(5.140233688,4.429970133,5.11278518));
#141238=CARTESIAN_POINT('Ctrl Pts',(5.146320044,4.428571429,5.106651545));
#141239=CARTESIAN_POINT('Ctrl Pts',(5.419104408,4.365882895,4.831748191));
#141240=CARTESIAN_POINT('Ctrl Pts',(5.661050747,4.302026826,4.529349229));
#141241=CARTESIAN_POINT('Ctrl Pts',(5.134649374,4.431369595,5.46675185200001));
#141242=CARTESIAN_POINT('Ctrl Pts',(5.141164914,4.429970133,5.460632127));
#141243=CARTESIAN_POINT('Ctrl Pts',(5.147665849,4.428571429,5.454496888));
#141244=CARTESIAN_POINT('Ctrl Pts',(5.439031228,4.365882895,5.179521645));
#141245=CARTESIAN_POINT('Ctrl Pts',(5.69944518700001,4.302026826,4.875071749));
#141246=CARTESIAN_POINT('',(5.13744736268223,4.43060907978605,5.11557763715302));
#141247=CARTESIAN_POINT('Origin',(-0.162605461209986,4.16114639537215,-0.100232851895971));
#141248=CARTESIAN_POINT('Ctrl Pts',(5.3159077588462,4.39169923738225,5.29066391793093));
#141249=CARTESIAN_POINT('Ctrl Pts',(5.28621450234274,4.39788077314604,5.26137708832544));
#141250=CARTESIAN_POINT('Ctrl Pts',(5.2564830708976,4.40420945815575,5.23212552680058));
#141251=CARTESIAN_POINT('Ctrl Pts',(5.19584578481867,4.41742225769839,5.17263045556358));
#141252=CARTESIAN_POINT('Ctrl Pts',(5.16629941639326,4.42401546239431,5.14374494205272));
#141253=CARTESIAN_POINT('Ctrl Pts',(5.13744736516035,4.43060907933145,5.11557763789017));
#141254=CARTESIAN_POINT('Ctrl Pts',(4.54891219022449,4.30075163058632,5.64534848929436));
#141255=CARTESIAN_POINT('Ctrl Pts',(4.55196725961225,4.30138922829316,5.64288131064718));
#141256=CARTESIAN_POINT('Ctrl Pts',(4.555022329,4.302026826,5.640414132));
#141257=CARTESIAN_POINT('Ctrl Pts',(4.862287584,4.36615356,5.392276306));
#141258=CARTESIAN_POINT('Ctrl Pts',(5.14077960699999,4.431389364,5.112228969));
#141259=CARTESIAN_POINT('Ctrl Pts',(4.89476568930713,4.30075163058632,5.68254651113073));
#141260=CARTESIAN_POINT('Ctrl Pts',(4.89784070365356,4.30138922829316,5.67989198306536));
#141261=CARTESIAN_POINT('Ctrl Pts',(4.900915718,4.302026826,5.677237455));
#141262=CARTESIAN_POINT('Ctrl Pts',(5.210186948,4.36615356,5.41025686));
#141263=CARTESIAN_POINT('Ctrl Pts',(5.488626205,4.431389364,5.111260352));
#141264=CARTESIAN_POINT('Origin',(-0.150003984782877,4.55345289786449,-0.120616314865278));
#141265=CARTESIAN_POINT('Ctrl Pts',(3.91368645,4.431369595,6.102913924));
#141266=CARTESIAN_POINT('Ctrl Pts',(3.9209602,4.429970133,6.098249402));
#141267=CARTESIAN_POINT('Ctrl Pts',(3.928222811,4.428571429,6.093567555));
#141268=CARTESIAN_POINT('Ctrl Pts',(4.253725723,4.365882895,5.883731863));
#141269=CARTESIAN_POINT('Ctrl Pts',(4.55502232900001,4.302026826,5.640414132));
#141270=CARTESIAN_POINT('Ctrl Pts',(3.839414072,4.431369595,6.442740068));
#141271=CARTESIAN_POINT('Ctrl Pts',(3.847092844,4.429970133,6.438164067));
#141272=CARTESIAN_POINT('Ctrl Pts',(3.854760685,4.428571429,6.433569776));
#141273=CARTESIAN_POINT('Ctrl Pts',(4.198425653,4.365882895,6.227658244));
#141274=CARTESIAN_POINT('Ctrl Pts',(4.518199006,4.302026826,5.986307521));
#141275=CARTESIAN_POINT('',(3.91763872170725,4.43060907983154,6.10037759560077));
#141276=CARTESIAN_POINT('Origin',(-0.137256717281262,4.16114637760005,-0.132844812216939));
#141277=CARTESIAN_POINT('Ctrl Pts',(4.05428843853699,4.39169923736995,6.30973416640578));
#141278=CARTESIAN_POINT('Ctrl Pts',(4.0315851965443,4.39788077312087,6.27474887425655));
#141279=CARTESIAN_POINT('Ctrl Pts',(4.0088370904528,4.40420945813757,6.23978981908078));
#141280=CARTESIAN_POINT('Ctrl Pts',(3.96240709071846,4.41742227513582,6.16865039165864));
#141281=CARTESIAN_POINT('Ctrl Pts',(3.93976101701759,4.42401548541367,6.1340885862235));
#141282=CARTESIAN_POINT('Ctrl Pts',(3.91763872389686,4.43060907925384,6.1003775976299));
#141283=CARTESIAN_POINT('Ctrl Pts',(3.22897810090943,4.30075163058632,6.49124503453277));
#141284=CARTESIAN_POINT('Ctrl Pts',(3.23249211495472,4.30138922829316,6.48949228676638));
#141285=CARTESIAN_POINT('Ctrl Pts',(3.236006129,4.302026826,6.487739539));
#141286=CARTESIAN_POINT('Ctrl Pts',(3.589429991,4.36615356,6.311455985));
#141287=CARTESIAN_POINT('Ctrl Pts',(3.921612925,4.431389364,6.097823552));
#141288=CARTESIAN_POINT('Ctrl Pts',(3.55874926241771,4.30075163058632,6.60192166698133));
#141289=CARTESIAN_POINT('Ctrl Pts',(3.56232302970886,4.30138922829316,6.59999023749066));
#141290=CARTESIAN_POINT('Ctrl Pts',(3.565896797,4.302026826,6.598058808));
#141291=CARTESIAN_POINT('Ctrl Pts',(3.925330374,4.36615356,6.403804243));
#141292=CARTESIAN_POINT('Ctrl Pts',(4.261535287,4.431389364,6.171654316));
#141293=CARTESIAN_POINT('Origin',(-0.120568015468438,4.55345288918264,-0.150042782148404));
#141294=CARTESIAN_POINT('Ctrl Pts',(2.510240543,4.431369595,6.801558087));
#141295=CARTESIAN_POINT('Ctrl Pts',(2.518346971,4.429970133,6.79856626));
#141296=CARTESIAN_POINT('Ctrl Pts',(2.526446244,4.428571429,6.795555119));
#141297=CARTESIAN_POINT('Ctrl Pts',(2.88944755,4.365882895,6.660598773));
#141298=CARTESIAN_POINT('Ctrl Pts',(3.236006129,4.302026826,6.487739539));
#141299=CARTESIAN_POINT('Ctrl Pts',(2.364652037,4.431369595,7.117472919));
#141300=CARTESIAN_POINT('Ctrl Pts',(2.373134987,4.429970133,7.114654611));
#141301=CARTESIAN_POINT('Ctrl Pts',(2.381611195,4.428571429,7.111816091));
#141302=CARTESIAN_POINT('Ctrl Pts',(2.76150636,4.365882895,6.984596466));
#141303=CARTESIAN_POINT('Ctrl Pts',(3.125686861,4.302026826,6.817630208));
#141304=CARTESIAN_POINT('',(2.51464564830737,4.43060907980155,6.79993067800396));
#141305=CARTESIAN_POINT('Origin',(-0.105490043542784,4.16114643440491,-0.159245170787863));
#141306=CARTESIAN_POINT('Ctrl Pts',(2.6030950961635,4.39169923736054,7.03376825860753));
#141307=CARTESIAN_POINT('Ctrl Pts',(2.58844344688307,4.39788077312132,6.99472037711179));
#141308=CARTESIAN_POINT('Ctrl Pts',(2.57374234231555,4.40420945811645,6.95568847492197));
#141309=CARTESIAN_POINT('Ctrl Pts',(2.54369085516498,4.41742221748141,6.87623151675625));
#141310=CARTESIAN_POINT('Ctrl Pts',(2.5290040057849,4.42401542249756,6.83760952313001));
#141311=CARTESIAN_POINT('Ctrl Pts',(2.51464565003509,4.43060907922589,6.79993068076175));
#141312=CARTESIAN_POINT('Ctrl Pts',(1.75806058539698,4.30075163058632,7.03361817669735));
#141313=CARTESIAN_POINT('Ctrl Pts',(1.76186923269849,4.30138922829316,7.03266181634867));
#141314=CARTESIAN_POINT('Ctrl Pts',(1.76567788,4.302026826,7.031705456));
#141315=CARTESIAN_POINT('Ctrl Pts',(2.148734641,4.36615356,6.935518997));
#141316=CARTESIAN_POINT('Ctrl Pts',(2.519075981,4.431389364,6.798290683));
#141317=CARTESIAN_POINT('Ctrl Pts',(2.05632967530983,4.30075163058632,7.21259830283048));
#141318=CARTESIAN_POINT('Ctrl Pts',(2.06023509015492,4.30138922829316,7.21148028341524));
#141319=CARTESIAN_POINT('Ctrl Pts',(2.064140505,4.302026826,7.210362264));
#141320=CARTESIAN_POINT('Ctrl Pts',(2.456929714,4.36615356,7.097916857));
#141321=CARTESIAN_POINT('Ctrl Pts',(2.835179715,4.431389364,6.94346858500001));
#141322=CARTESIAN_POINT('Origin',(-0.0854944270200353,4.55345285995928,
-0.172453402573198));
#141323=CARTESIAN_POINT('Ctrl Pts',(0.989418577999999,4.431369595,7.182168954));
#141324=CARTESIAN_POINT('Ctrl Pts',(0.997978637,4.429970133,7.180989716));
#141325=CARTESIAN_POINT('Ctrl Pts',(1.00653586,4.428571429,7.179790078));
#141326=CARTESIAN_POINT('Ctrl Pts',(1.390062022,4.365882895,7.126023487));
#141327=CARTESIAN_POINT('Ctrl Pts',(1.76567788,4.302026826,7.031705456));
#141328=CARTESIAN_POINT('Ctrl Pts',(0.779321499,4.431369595,7.459400646));
#141329=CARTESIAN_POINT('Ctrl Pts',(0.788211976,4.429970133,7.458471813));
#141330=CARTESIAN_POINT('Ctrl Pts',(0.797100213,4.428571429,7.45752179));
#141331=CARTESIAN_POINT('Ctrl Pts',(1.195462099,4.365882895,7.41494272));
#141332=CARTESIAN_POINT('Ctrl Pts',(1.587021072,4.302026826,7.330168082));
#141333=CARTESIAN_POINT('',(0.994070539475338,4.43060907984242,7.18152655971494));
#141334=CARTESIAN_POINT('Origin',(-0.0687907678335942,4.16114642128525,
-0.178199462025521));
#141335=CARTESIAN_POINT('Ctrl Pts',(1.03018392039923,4.3916992373849,7.42891116420171));
#141336=CARTESIAN_POINT('Ctrl Pts',(1.02426895890848,4.3978807731304,7.38762652911978));
#141337=CARTESIAN_POINT('Ctrl Pts',(1.01830226328049,4.40420945811811,7.34634686826014));
#141338=CARTESIAN_POINT('Ctrl Pts',(1.006034236914,4.41742224301326,7.2622872258476));
#141339=CARTESIAN_POINT('Ctrl Pts',(0.999993344785503,4.42401544886382,
7.22141095734852));
#141340=CARTESIAN_POINT('Ctrl Pts',(0.994070540471638,4.43060907935679,
7.18152656222649));
#141341=CARTESIAN_POINT('Ctrl Pts',(0.204938109066286,4.30075163058632,
7.24710715016635));
#141342=CARTESIAN_POINT('Ctrl Pts',(0.208863301533143,4.30138922829316,
7.24699189558317));
#141343=CARTESIAN_POINT('Ctrl Pts',(0.212788494,4.302026826,7.246876641));
#141344=CARTESIAN_POINT('Ctrl Pts',(0.607566848,4.36615356,7.235284849));
#141345=CARTESIAN_POINT('Ctrl Pts',(0.998749843,4.431389364,7.180877297));
#141346=CARTESIAN_POINT('Ctrl Pts',(0.457758398939834,4.30075163058632,
7.48602185797434));
#141347=CARTESIAN_POINT('Ctrl Pts',(0.461812848469918,4.30138922829316,
7.48576952598717));
#141348=CARTESIAN_POINT('Ctrl Pts',(0.465867298,4.302026826,7.485517194));
#141349=CARTESIAN_POINT('Ctrl Pts',(0.873645751,4.36615356,7.460138768));
#141350=CARTESIAN_POINT('Ctrl Pts',(1.27625429,4.431389364,7.390613979));
#141351=CARTESIAN_POINT('Origin',(-0.0464232246340045,4.55345293116766,
-0.186800079926107));
#141352=CARTESIAN_POINT('Ctrl Pts',(-0.57501968255,4.431369595,7.22469372692));
#141353=CARTESIAN_POINT('Ctrl Pts',(-0.56640894119,4.429970133,7.22537906312));
#141354=CARTESIAN_POINT('Ctrl Pts',(-0.55779659034,4.428571429,7.22604387274));
#141355=CARTESIAN_POINT('Ctrl Pts',(-0.17179966821,4.365882895,7.2558399507));
#141356=CARTESIAN_POINT('Ctrl Pts',(0.21517489952,4.302026826,7.24434585296));
#141357=CARTESIAN_POINT('Ctrl Pts',(-0.5776675,4.431369595,7.226949582));
#141358=CARTESIAN_POINT('Ctrl Pts',(-0.56905407,4.429970133,7.22763807400001));
#141359=CARTESIAN_POINT('Ctrl Pts',(-0.560439023,4.428571429,7.228306033));
#141360=CARTESIAN_POINT('Ctrl Pts',(-0.174321262,4.365882895,7.25824326300001));
#141361=CARTESIAN_POINT('Ctrl Pts',(0.212788494,4.302026826,7.246876641));
#141362=CARTESIAN_POINT('Ctrl Pts',(-0.842449245,4.431369595,7.45253509));
#141363=CARTESIAN_POINT('Ctrl Pts',(-0.833566951,4.429970133,7.453539162));
#141364=CARTESIAN_POINT('Ctrl Pts',(-0.824682289,4.428571429,7.454522059));
#141365=CARTESIAN_POINT('Ctrl Pts',(-0.426480641,4.365882895,7.498574493));
#141366=CARTESIAN_POINT('Ctrl Pts',(-0.025852058,4.302026826,7.499955445));
#141367=CARTESIAN_POINT('Origin',(-0.0288748555719586,4.16114642761327,
-0.188821302368569));
#141368=CARTESIAN_POINT('Ctrl Pts',(0.206355414,1.457192641,7.247062677));
#141369=CARTESIAN_POINT('Ctrl Pts',(0.603838305,1.522897175,7.235744609));
#141370=CARTESIAN_POINT('Ctrl Pts',(0.997699109,1.587500328,7.181023359));
#141371=CARTESIAN_POINT('Ctrl Pts',(0.459222278,1.457192641,7.485927791));
#141372=CARTESIAN_POINT('Ctrl Pts',(0.869806311,1.522897175,7.460740622));
#141373=CARTESIAN_POINT('Ctrl Pts',(1.275172863,1.587500328,7.390800645));
#141374=CARTESIAN_POINT('',(0.459222295417621,1.45719263974394,7.48592778870736));
#141375=CARTESIAN_POINT('',(1.02534975045092,1.54766053442819,7.429579834804));
#141376=CARTESIAN_POINT('Origin',(0.00737832284867054,1.3393599161851,-0.18767758211871));
#141377=CARTESIAN_POINT('Ctrl Pts',(0.993027301226868,1.58673401519535,
7.18167089033084));
#141378=CARTESIAN_POINT('Ctrl Pts',(0.998359708366294,1.57991285715115,
7.22293886439134));
#141379=CARTESIAN_POINT('Ctrl Pts',(1.00372395719946,1.57325083217545,7.26425318543439));
#141380=CARTESIAN_POINT('Ctrl Pts',(1.01449798875009,1.56023624973537,7.34687598194897));
#141381=CARTESIAN_POINT('Ctrl Pts',(1.019913657707,1.55387659346546,7.38822956347221));
#141382=CARTESIAN_POINT('Ctrl Pts',(1.02534975010316,1.54766054355296,7.42957983622142));
#141383=CARTESIAN_POINT('',(0.332788868614406,1.45719263730543,7.36649523297837));
#141384=CARTESIAN_POINT('Origin',(-1.07932326270932E-13,1.54874775200011,
-8.50014503228635E-13));
#141385=CARTESIAN_POINT('',(1.02275296019507,1.36645689999125,7.42993784473413));
#141386=CARTESIAN_POINT('Origin',(-0.00775337357056385,1.48213729927608,
-0.191983098392322));
#141387=CARTESIAN_POINT('',(1.58051349599227,1.45719264185526,7.33157405540269));
#141388=CARTESIAN_POINT('Origin',(-0.021854084256511,1.33929189546777,-0.190828900708343));
#141389=CARTESIAN_POINT('Origin',(-0.0367451552969436,1.48214297993429,
-0.189449351628988));
#141390=CARTESIAN_POINT('Ctrl Pts',(0.988391585,1.587508025,7.182310358));
#141391=CARTESIAN_POINT('Ctrl Pts',(1.377955312,1.52246862,7.128700657));
#141392=CARTESIAN_POINT('Ctrl Pts',(1.759435193,1.457192641,7.033270065));
#141393=CARTESIAN_POINT('Ctrl Pts',(1.77256190375125,1.45494649660808,7.02998630131967));
#141394=CARTESIAN_POINT('Ctrl Pts',(1.78568861450254,1.45270035221617,7.02670253763929));
#141395=CARTESIAN_POINT('Ctrl Pts',(0.777825679513265,1.587508025,7.4600781682574));
#141396=CARTESIAN_POINT('Ctrl Pts',(1.18245534777751,1.52246862,7.41788942109954));
#141397=CARTESIAN_POINT('Ctrl Pts',(1.58014807973878,1.457192641,7.33218324295674));
#141398=CARTESIAN_POINT('Ctrl Pts',(1.59383267418357,1.45494649660808,7.32923409605251));
#141399=CARTESIAN_POINT('Ctrl Pts',(1.60751726862837,1.45270035221618,7.32628494914832));
#141400=CARTESIAN_POINT('',(1.66997436233271,1.4571926425566,7.18242202083007));
#141401=CARTESIAN_POINT('Ctrl Pts',(1.759435193,1.457192641,7.033270065));
#141402=CARTESIAN_POINT('Ctrl Pts',(2.145192105,1.522897175,6.93676953500001));
#141403=CARTESIAN_POINT('Ctrl Pts',(2.518081211,1.587500328,6.798659207));
#141404=CARTESIAN_POINT('Ctrl Pts',(2.057739109,1.457192641,7.212191744));
#141405=CARTESIAN_POINT('Ctrl Pts',(2.453309419,1.522897175,7.099330006));
#141406=CARTESIAN_POINT('Ctrl Pts',(2.834163698,1.587500328,6.94388336100001));
#141407=CARTESIAN_POINT('',(2.05773912551659,1.45719263974394,7.21219173801661));
#141408=CARTESIAN_POINT('',(2.59851769117755,1.54766053444267,7.03546049931711));
#141409=CARTESIAN_POINT('Origin',(-0.0331393637470409,1.33935993853076,
-0.1848760404687));
#141410=CARTESIAN_POINT('Ctrl Pts',(2.51365782782729,1.58673401524756,6.80029589983965));
#141411=CARTESIAN_POINT('Ctrl Pts',(2.52773696267109,1.57991285627922,6.83945274689865));
#141412=CARTESIAN_POINT('Ctrl Pts',(2.54185715832421,1.57325083034138,6.87864801308967));
#141413=CARTESIAN_POINT('Ctrl Pts',(2.57014083739803,1.56023621136334,6.95702325605497));
#141414=CARTESIAN_POINT('Ctrl Pts',(2.58431978334036,1.55387651552159,6.99624606562961));
#141415=CARTESIAN_POINT('Ctrl Pts',(2.59851769119417,1.54766054358843,7.0354605007608));
#141416=CARTESIAN_POINT('',(1.90858717286608,1.45719263730543,7.12273089864083));
#141417=CARTESIAN_POINT('Origin',(-1.39211558947139E-13,1.54874775199994,
-1.9819215713035E-13));
#141418=CARTESIAN_POINT('',(2.59605857345536,1.36645689997628,7.03636837262591));
#141419=CARTESIAN_POINT('Origin',(-0.0488428478450981,1.48213730590088,
-0.185828051894329));
#141420=CARTESIAN_POINT('',(3.1196336713731,1.45719264185526,6.82040224533446));
#141421=CARTESIAN_POINT('Origin',(-0.0623657656572568,1.33929186513119,
-0.181669549898223));
#141422=CARTESIAN_POINT('Origin',(-0.0766119206329151,1.48214301573756,
-0.177120609940757));
#141423=CARTESIAN_POINT('Ctrl Pts',(2.509267959,1.587508025,6.801916959));
#141424=CARTESIAN_POINT('Ctrl Pts',(2.878199401,1.52246862,6.665815937));
#141425=CARTESIAN_POINT('Ctrl Pts',(3.230245738,1.457192641,6.490609561));
#141426=CARTESIAN_POINT('Ctrl Pts',(3.24235964108627,1.4549464966708,6.48458071526042));
#141427=CARTESIAN_POINT('Ctrl Pts',(3.2544735441726,1.45270035234162,6.47855186952078));
#141428=CARTESIAN_POINT('Ctrl Pts',(2.36333683583635,1.587508025,7.11845615730253));
#141429=CARTESIAN_POINT('Ctrl Pts',(2.74943715342077,1.52246862,6.99027034253071));
#141430=CARTESIAN_POINT('Ctrl Pts',(3.11940775568363,1.457192641,6.82107574407964));
#141431=CARTESIAN_POINT('Ctrl Pts',(3.1321384321587,1.4549464966708,6.81525376341134));
#141432=CARTESIAN_POINT('Ctrl Pts',(3.14486910863384,1.45270035234162,6.80943178274304));
#141433=CARTESIAN_POINT('',(3.17493971364809,1.4571926425566,6.65550586087452));
#141434=CARTESIAN_POINT('Ctrl Pts',(3.230245738,1.457192641,6.490609561));
#141435=CARTESIAN_POINT('Ctrl Pts',(3.586239107,1.522897175,6.313438827));
#141436=CARTESIAN_POINT('Ctrl Pts',(3.920720634,1.587500328,6.098397307));
#141437=CARTESIAN_POINT('Ctrl Pts',(3.560038347,1.457192641,6.601221627));
#141438=CARTESIAN_POINT('Ctrl Pts',(3.922098505,1.522897175,6.40596261));
#141439=CARTESIAN_POINT('Ctrl Pts',(4.26063218900001,1.587500328,6.172277809));
#141440=CARTESIAN_POINT('',(3.56003836181377,1.45719263974395,6.60122161761045));
#141441=CARTESIAN_POINT('',(4.05018183213464,1.54766053440617,6.31237085077319));
#141442=CARTESIAN_POINT('Origin',(-0.0721074795453386,1.33935992231088,
-0.173429776045458));
#141443=CARTESIAN_POINT('Ctrl Pts',(3.91675250729274,1.58673401518852,6.10094663167512));
#141444=CARTESIAN_POINT('Ctrl Pts',(3.93892001923704,1.57991286402647,6.13616137513056));
#141445=CARTESIAN_POINT('Ctrl Pts',(3.9611358874709,1.57325084614049,6.17140480742286));
#141446=CARTESIAN_POINT('Ctrl Pts',(4.00560673407309,1.56023620854231,6.24186762645686));
#141447=CARTESIAN_POINT('Ctrl Pts',(4.02788593933092,1.55387650989478,6.27712539084905));
#141448=CARTESIAN_POINT('Ctrl Pts',(4.05018183241762,1.54766054352542,6.31237085220247));
#141449=CARTESIAN_POINT('',(3.39514206259527,1.45719263730544,6.54591558357728));
#141450=CARTESIAN_POINT('Origin',(6.46184494801361E-13,1.54874775199939,
9.74480912629971E-13));
#141451=CARTESIAN_POINT('',(4.04797537329225,1.36645690002083,6.31378613588496));
#141452=CARTESIAN_POINT('Origin',(-0.0876483475473111,1.48213729582552,
-0.170983506854183));
#141453=CARTESIAN_POINT('',(4.5128832428005,1.45719264185525,5.99031600768223));
#141454=CARTESIAN_POINT('Origin',(-0.0999613416881162,1.33929187558694,
-0.164015522851519));
#141455=CARTESIAN_POINT('Origin',(-0.112896555986552,1.48214303935283,-0.156510462046193));
#141456=CARTESIAN_POINT('Ctrl Pts',(3.912813751,1.587508025,6.10347348200001));
#141457=CARTESIAN_POINT('Ctrl Pts',(4.243862085,1.52246862,5.891245072));
#141458=CARTESIAN_POINT('Ctrl Pts',(4.550013582,1.457192641,5.644455368));
#141459=CARTESIAN_POINT('Ctrl Pts',(4.56054824525312,1.45494649664329,5.63596334215186));
#141460=CARTESIAN_POINT('Ctrl Pts',(4.57108290850628,1.45270035228661,5.62747131630359));
#141461=CARTESIAN_POINT('Ctrl Pts',(3.83834098735086,1.587508025,6.44398304808587));
#141462=CARTESIAN_POINT('Ctrl Pts',(4.18785833294733,1.52246862,6.23579399132682));
#141463=CARTESIAN_POINT('Ctrl Pts',(4.51280739121253,1.457192641,5.99102232560795));
#141464=CARTESIAN_POINT('Ctrl Pts',(4.52398887794962,1.45494649664329,5.98259974039272));
#141465=CARTESIAN_POINT('Ctrl Pts',(4.53517036468666,1.45270035228661,5.97417715517737));
#141466=CARTESIAN_POINT('',(4.53144841205905,1.4571926425566,5.81738564461188));
#141467=CARTESIAN_POINT('Ctrl Pts',(4.550013582,1.457192641,5.644455368));
#141468=CARTESIAN_POINT('Ctrl Pts',(4.859597553,1.522897175,5.394898736));
#141469=CARTESIAN_POINT('Ctrl Pts',(5.14003151800001,1.587500328,5.112981126));
#141470=CARTESIAN_POINT('Ctrl Pts',(4.895874148,1.457192641,5.681585723));
#141471=CARTESIAN_POINT('Ctrl Pts',(5.207494623,1.522897175,5.413059522));
#141472=CARTESIAN_POINT('Ctrl Pts',(5.487878254,1.587500328,5.112063406));
#141473=CARTESIAN_POINT('',(4.89587416044907,1.45719263974395,5.68158571064541));
#141474=CARTESIAN_POINT('',(5.31246397217837,1.54766053441173,5.29412175647425));
#141475=CARTESIAN_POINT('Origin',(-0.107703978192127,1.33935986531226,-0.153874175233379));
#141476=CARTESIAN_POINT('Ctrl Pts',(5.13670419329786,1.5867340151723,5.11632387889823));
#141477=CARTESIAN_POINT('Ctrl Pts',(5.16592358955562,1.57991285945224,5.14594998118021));
#141478=CARTESIAN_POINT('Ctrl Pts',(5.19519638141006,1.57325083687793,5.17559370893319));
#141479=CARTESIAN_POINT('Ctrl Pts',(5.25377489534235,1.56023621089933,5.23484917606375));
#141480=CARTESIAN_POINT('Ctrl Pts',(5.28311259043306,1.55387651466602,5.26449325097607));
#141481=CARTESIAN_POINT('Ctrl Pts',(5.3124639727899,1.54766054354084,5.2941217577837));
#141482=CARTESIAN_POINT('',(4.72294388238488,1.45719263730544,5.66302053100106));
#141483=CARTESIAN_POINT('Origin',(-5.89805981832114E-13,1.54874775200067,
-4.53630188967935E-13));
#141484=CARTESIAN_POINT('',(5.31061334361147,1.36645689999454,5.29597827676676));
#141485=CARTESIAN_POINT('Origin',(-0.122355703598187,1.48213731350686,-0.14814434441156));
#141486=CARTESIAN_POINT('',(5.69511540948564,1.45719264185527,4.88012925152646));
#141487=CARTESIAN_POINT('Origin',(-0.132882732145188,1.33929190568236,-0.13869214103061));
#141488=CARTESIAN_POINT('Origin',(-0.143902244688174,1.48214299053564,-0.128581930462383));
#141489=CARTESIAN_POINT('Ctrl Pts',(5.133400721,1.587508025,5.11963837));
#141490=CARTESIAN_POINT('Ctrl Pts',(5.411086494,1.52246862,4.841206136));
#141491=CARTESIAN_POINT('Ctrl Pts',(5.657027848,1.457192641,4.534372715));
#141492=CARTESIAN_POINT('Ctrl Pts',(5.66549068205718,1.45494649666838,4.52381458688173));
#141493=CARTESIAN_POINT('Ctrl Pts',(5.67395351611424,1.45270035233679,4.51325645876339));
#141494=CARTESIAN_POINT('Ctrl Pts',(5.13386858061824,1.587508025,5.4681964540282));
#141495=CARTESIAN_POINT('Ctrl Pts',(5.43045991200896,1.52246862,5.18973884330391));
#141496=CARTESIAN_POINT('Ctrl Pts',(5.6951931687402,1.457192641,4.88083536198855));
#141497=CARTESIAN_POINT('Ctrl Pts',(5.70430263156415,1.45494649666838,4.87020600316158));
#141498=CARTESIAN_POINT('Ctrl Pts',(5.713412094388,1.45270035233679,4.85957664433463));
#141499=CARTESIAN_POINT('',(5.67607161911655,1.4571926425566,4.70725094112458));
#141500=CARTESIAN_POINT('Ctrl Pts',(5.657027848,1.457192641,4.534372715));
#141501=CARTESIAN_POINT('Ctrl Pts',(5.905726619,1.522897175,4.224099176));
#141502=CARTESIAN_POINT('Ctrl Pts',(6.119000241,1.587500328,3.888487631));
#141503=CARTESIAN_POINT('Ctrl Pts',(6.002784315,1.457192641,4.496285186));
#141504=CARTESIAN_POINT('Ctrl Pts',(6.249394081,1.522897175,4.167047787));
#141505=CARTESIAN_POINT('Ctrl Pts',(6.45851723100001,1.587500328,3.812814601));
#141506=CARTESIAN_POINT('',(6.00278432448469,1.45719263974395,4.49628517126952));
#141507=CARTESIAN_POINT('',(6.32634120131154,1.54766053441944,4.02832541346193));
#141508=CARTESIAN_POINT('Origin',(-0.138264419467786,1.33935989120299,-0.127123575016829));
#141509=CARTESIAN_POINT('Ctrl Pts',(6.1164693003912,1.5867340151904,3.89246750855191));
#141510=CARTESIAN_POINT('Ctrl Pts',(6.15137427891944,1.57991286352367,3.91511964903068));
#141511=CARTESIAN_POINT('Ctrl Pts',(6.18633519089036,1.57325084512343,3.93777752274988));
#141512=CARTESIAN_POINT('Ctrl Pts',(6.25628239279515,1.56023621035438,3.98305501161561));
#141513=CARTESIAN_POINT('Ctrl Pts',(6.29130679201329,1.55387651355754,4.00569928945281));
#141514=CARTESIAN_POINT('Ctrl Pts',(6.3263412021866,1.5476605435511,4.02832541461568));
#141515=CARTESIAN_POINT('',(5.82990609536158,1.45719263730544,4.51532893260281));
#141516=CARTESIAN_POINT('Origin',(3.81205483845903E-13,1.54874775199939,
2.8948198005363E-13));
#141517=CARTESIAN_POINT('',(6.32493293650937,1.36645689998581,4.03053635942365));
#141518=CARTESIAN_POINT('Origin',(-0.151342008501366,1.4821373052914,-0.118378126660252));
#141519=CARTESIAN_POINT('',(6.61105030969859,1.45719264185525,3.54175307414458));
#141520=CARTESIAN_POINT('Origin',(-0.159590726309623,1.33929188180681,-0.10688373894521));
#141521=CARTESIAN_POINT('Origin',(-0.168179198710835,1.48214303405179,-0.0946410250360736));
#141522=CARTESIAN_POINT('Ctrl Pts',(6.113955579,1.587508025,3.896414657));
#141523=CARTESIAN_POINT('Ctrl Pts',(6.325294513,1.52246862,3.564797781));
#141524=CARTESIAN_POINT('Ctrl Pts',(6.49952578,1.457192641,3.212267834));
#141525=CARTESIAN_POINT('Ctrl Pts',(6.50552107216591,1.45494649670994,3.20013729012063));
#141526=CARTESIAN_POINT('Ctrl Pts',(6.51151636433198,1.45270035241989,3.18800674624118));
#141527=CARTESIAN_POINT('Ctrl Pts',(6.18934218529096,1.587508025,4.23672307106577));
#141528=CARTESIAN_POINT('Ctrl Pts',(6.41913922064845,1.52246862,3.90101727579674));
#141529=CARTESIAN_POINT('Ctrl Pts',(6.61127804385332,1.457192641,3.54242596016866));
#141530=CARTESIAN_POINT('Ctrl Pts',(6.61788953443919,1.45494649670994,3.53008684479417));
#141531=CARTESIAN_POINT('Ctrl Pts',(6.62450102502494,1.45270035241989,3.51774772941973));
#141532=CARTESIAN_POINT('',(6.55528802638805,1.4571926425566,3.37701041498213));
#141533=CARTESIAN_POINT('Ctrl Pts',(6.49952578000001,1.457192641,3.212267834));
#141534=CARTESIAN_POINT('Ctrl Pts',(6.675710472,1.522897175,2.855785434));
#141535=CARTESIAN_POINT('Ctrl Pts',(6.81185131300001,1.587500328,2.482172775));
#141536=CARTESIAN_POINT('Ctrl Pts',(6.829010959,1.457192641,3.10074335));
#141537=CARTESIAN_POINT('Ctrl Pts',(6.999078818,1.522897175,2.726189529));
#141538=CARTESIAN_POINT('Ctrl Pts',(7.12716312,1.587500328,2.335282822));
#141539=CARTESIAN_POINT('',(6.82901096511129,1.45719263974395,3.10074333355966));
#141540=CARTESIAN_POINT('',(7.04440574696063,1.54766053442346,2.57416905094527));
#141541=CARTESIAN_POINT('Origin',(-0.162359327312468,1.33935990693384,-0.094428589318758));
#141542=CARTESIAN_POINT('Ctrl Pts',(6.81023510049718,1.58673401520783,2.48660368253255));
#141543=CARTESIAN_POINT('Ctrl Pts',(6.84919357949377,1.57991286024168,2.50122269723687));
#141544=CARTESIAN_POINT('Ctrl Pts',(6.88820791919594,1.57325083844524,2.51583528792782));
#141545=CARTESIAN_POINT('Ctrl Pts',(6.96625284006547,1.56023624971961,2.54501753047916));
#141546=CARTESIAN_POINT('Ctrl Pts',(7.00532597248801,1.55387659345106,2.55960308829892));
#141547=CARTESIAN_POINT('Ctrl Pts',(7.0444057480503,1.54766054354709,2.57416905191524));
#141548=CARTESIAN_POINT('',(6.66426837919014,1.45719263730544,3.15650557154141));
#141549=CARTESIAN_POINT('Origin',(7.84962372879505E-13,1.548747752,3.46944695195361E-13));
#141550=CARTESIAN_POINT('',(7.04350569482777,1.36645690003436,2.57663104150567));
#141551=CARTESIAN_POINT('Origin',(-0.173251244287309,1.48213728690228,-0.0830763464165341));
#141552=CARTESIAN_POINT('',(7.21785984476966,1.45719264185526,2.03776846088087));
#141553=CARTESIAN_POINT('Origin',(-0.178836261220207,1.33929187072181,-0.0700775177607763));
#141554=CARTESIAN_POINT('Origin',(-0.184592117991271,1.48214298945751,-0.0562747580030781));
#141555=CARTESIAN_POINT('Ctrl Pts',(6.80862866900001,1.587508025,2.490998925));
#141556=CARTESIAN_POINT('Ctrl Pts',(6.943738791,1.52246862,2.121703444));
#141557=CARTESIAN_POINT('Ctrl Pts',(7.038113109,1.457192641,1.739960879));
#141558=CARTESIAN_POINT('Ctrl Pts',(7.04136052648581,1.45494649649692,1.72682512865051));
#141559=CARTESIAN_POINT('Ctrl Pts',(7.04460794397148,1.45270035199387,1.71368937830096));
#141560=CARTESIAN_POINT('Ctrl Pts',(6.95540902714619,1.587508025,2.80714522552581));
#141561=CARTESIAN_POINT('Ctrl Pts',(7.10766671429717,1.52246862,2.42988847541039));
#141562=CARTESIAN_POINT('Ctrl Pts',(7.21822690527199,1.457192641,2.03837665916208));
#141563=CARTESIAN_POINT('Ctrl Pts',(7.22203127816718,1.45494649649693,2.02490474916662));
#141564=CARTESIAN_POINT('Ctrl Pts',(7.22583565106249,1.45270035199386,2.01143283917115));
#141565=CARTESIAN_POINT('',(7.12798645045437,1.4571926425566,1.88886463573798));
#141566=CARTESIAN_POINT('Ctrl Pts',(7.038113109,1.457192641,1.739960879));
#141567=CARTESIAN_POINT('Ctrl Pts',(7.133545523,1.522897175,1.353938339));
#141568=CARTESIAN_POINT('Ctrl Pts',(7.18618778900001,1.587500328,0.95979428));
#141569=CARTESIAN_POINT('Ctrl Pts',(7.335920641,1.457192641,1.560214201));
#141570=CARTESIAN_POINT('Ctrl Pts',(7.421494407,1.522897175,1.157857678));
#141571=CARTESIAN_POINT('Ctrl Pts',(7.462550783,1.587500328,0.748555814));
#141572=CARTESIAN_POINT('',(7.3359206434274,1.45719263974395,1.56021418364124));
#141573=CARTESIAN_POINT('',(7.43308170912172,1.54766053441375,0.999647404332543));
#141574=CARTESIAN_POINT('Origin',(-0.17886312272908,1.3393598776417,-0.057318495887754));
#141575=CARTESIAN_POINT('Ctrl Pts',(7.18556187684235,1.5867340152581,0.964469032973011));
#141576=CARTESIAN_POINT('Ctrl Pts',(7.22675217653307,1.57991286155787,0.970371340689533));
#141577=CARTESIAN_POINT('Ctrl Pts',(7.26799564895476,1.57325084106422,0.97625536603543));
#141578=CARTESIAN_POINT('Ctrl Pts',(7.35048949777617,1.56023621202256,0.987978029095562));
#141579=CARTESIAN_POINT('Ctrl Pts',(7.39178485552251,1.55387651687792,0.993823053896906));
#141580=CARTESIAN_POINT('Ctrl Pts',(7.43308171040408,1.54766054354744,0.999647404987986));
#141581=CARTESIAN_POINT('',(7.18701688006559,1.45719263730544,1.65008751793662));
#141582=CARTESIAN_POINT('Origin',(3.56485674313234E-13,1.54874775200056,
-3.28784308806229E-14));
#141583=CARTESIAN_POINT('',(7.43273195491697,1.36645690001638,1.002245319997));
#141584=CARTESIAN_POINT('Origin',(-0.187059724892573,1.48213730249397,-0.043890175824452));
#141585=CARTESIAN_POINT('',(7.48717027514498,1.45719264185527,0.438500058308726));
#141586=CARTESIAN_POINT('Origin',(-0.189719945583939,1.33929187097265,-0.0299946459976366));
#141587=CARTESIAN_POINT('Origin',(-0.192373778352274,1.48214300277812,-0.0152772230601544));
#141588=CARTESIAN_POINT('Ctrl Pts',(7.18493785,1.587508025,0.969106852));
#141589=CARTESIAN_POINT('Ctrl Pts',(7.23750156,1.52246862,0.579400611999999));
#141590=CARTESIAN_POINT('Ctrl Pts',(7.247606092,1.457192641,0.186295287));
#141591=CARTESIAN_POINT('Ctrl Pts',(7.24795378862651,1.4549464966273,0.172768545200744));
#141592=CARTESIAN_POINT('Ctrl Pts',(7.24830148525303,1.45270035225462,0.159241803401487));
#141593=CARTESIAN_POINT('Ctrl Pts',(7.39624867482026,1.587508025,1.24630839004406));
#141594=CARTESIAN_POINT('Ctrl Pts',(7.46384761147997,1.52246862,0.845140790845598));
#141595=CARTESIAN_POINT('Ctrl Pts',(7.48765949859589,1.457192641,0.439015130051796));
#141596=CARTESIAN_POINT('Ctrl Pts',(7.48847886487837,1.4549464966273,0.42504035890971));
#141597=CARTESIAN_POINT('Ctrl Pts',(7.48929823116085,1.45270035225462,0.411065587767622));
#141598=CARTESIAN_POINT('',(7.36738815040593,1.4571926425566,0.312397644926896));
#141599=CARTESIAN_POINT('Ctrl Pts',(7.247606092,1.457192641,0.186295287));
#141600=CARTESIAN_POINT('Ctrl Pts',(7.257823913,1.522897175,-0.211217409));
#141601=CARTESIAN_POINT('Ctrl Pts',(7.224506111,1.587500328,-0.60746313));
#141602=CARTESIAN_POINT('Ctrl Pts',(7.499810826,1.457192641,-0.053268829));
#141603=CARTESIAN_POINT('Ctrl Pts',(7.496889167,1.522897175,-0.464614311000001));
#141604=CARTESIAN_POINT('Ctrl Pts',(7.448997866,1.587500328,-0.873172832));
#141605=CARTESIAN_POINT('',(7.49981082465209,1.45719263974394,-0.0532688465116229));
#141606=CARTESIAN_POINT('',(7.47419503211715,1.54766053441069,-0.621616643533504));
#141607=CARTESIAN_POINT('Origin',(-0.1870030549888,1.33935990731118,-0.0175281510573762));
#141608=CARTESIAN_POINT('Ctrl Pts',(7.22489976603804,1.58673401514931,-0.602763116835093));
#141609=CARTESIAN_POINT('Ctrl Pts',(7.26639587926554,1.57991286177347,-0.605853498624341));
#141610=CARTESIAN_POINT('Ctrl Pts',(7.30793999166598,1.57325084160804,-0.6089731658026));
#141611=CARTESIAN_POINT('Ctrl Pts',(7.39102522824991,1.56023620913844,-0.615258312705757));
#141612=CARTESIAN_POINT('Ctrl Pts',(7.43261165127053,1.55387651110979,-0.61842722407249));
#141613=CARTESIAN_POINT('Ctrl Pts',(7.47419503351237,1.54766054353441,-0.621616643124316));
#141614=CARTESIAN_POINT('',(7.37370845920419,1.45719263730544,0.0665132063634968));
#141615=CARTESIAN_POINT('Origin',(-1.13971332371676E-12,1.54874775200017,
1.87861743305637E-13));
#141616=CARTESIAN_POINT('',(7.47441192966151,1.36645689996761,-0.619004279255739));
#141617=CARTESIAN_POINT('Origin',(-0.192121367400876,1.48213734012576,-0.00265175309706843));
#141618=CARTESIAN_POINT('',(7.4063889453873,1.45719264185525,-1.18127211997309));
#141619=CARTESIAN_POINT('Origin',(-0.19173213102862,1.33929187347829,0.0114907606312091));
#141620=CARTESIAN_POINT('Origin',(-0.191160650925758,1.48214304788297,0.0264346549692207));
#141621=CARTESIAN_POINT('Ctrl Pts',(7.225287322,1.587508025,-0.59809958));
#141622=CARTESIAN_POINT('Ctrl Pts',(7.19284679999999,1.52246862,-0.989994349));
#141623=CARTESIAN_POINT('Ctrl Pts',(7.118209069,1.457192641,-1.376081265));
#141624=CARTESIAN_POINT('Ctrl Pts',(7.11564078712196,1.45494649670151,-1.38936650312861));
#141625=CARTESIAN_POINT('Ctrl Pts',(7.11307250524391,1.45270035240304,-1.40265174125726));
#141626=CARTESIAN_POINT('Ctrl Pts',(7.49124795416804,1.587508025,-0.372804441566535));
#141627=CARTESIAN_POINT('Ctrl Pts',(7.47102728937974,1.52246862,-0.779124737500378));
#141628=CARTESIAN_POINT('Ctrl Pts',(7.40697745623856,1.457192641,-1.18087425891832));
#141629=CARTESIAN_POINT('Ctrl Pts',(7.40477350357891,1.45494649670151,-1.19469844678615));
#141630=CARTESIAN_POINT('Ctrl Pts',(7.40256955091918,1.45270035240304,-1.20852263465398));
#141631=CARTESIAN_POINT('',(7.2622989688385,1.4571926425566,-1.27867671243655));
#141632=CARTESIAN_POINT('Ctrl Pts',(7.118209069,1.457192641,-1.376081265));
#141633=CARTESIAN_POINT('Ctrl Pts',(7.042734524,1.522897175,-1.766496865));
#141634=CARTESIAN_POINT('Ctrl Pts',(6.925014556,1.587500328,-2.146316238));
#141635=CARTESIAN_POINT('Ctrl Pts',(7.313018193,1.457192641,-1.664261068));
#141636=CARTESIAN_POINT('Ctrl Pts',(7.221737721,1.522897175,-2.065361451));
#141637=CARTESIAN_POINT('Ctrl Pts',(7.087138087,1.587500328,-2.454072887));
#141638=CARTESIAN_POINT('',(7.31301818791927,1.45719263974395,-1.66426108481367));
#141639=CARTESIAN_POINT('',(7.16582330191368,1.54766053442354,-2.21381458832635));
#141640=CARTESIAN_POINT('Origin',(-0.186399158114623,1.33935990274223,0.0230818051578077));
#141641=CARTESIAN_POINT('Ctrl Pts',(6.92640937124286,1.58673401530334,-2.14181073366906));
#141642=CARTESIAN_POINT('Ctrl Pts',(6.96627100042353,1.57991285972098,-2.15374930543162));
#141643=CARTESIAN_POINT('Ctrl Pts',(7.00617321276576,1.57325083728514,-2.16572679693239));
#141644=CARTESIAN_POINT('Ctrl Pts',(7.08596481245988,1.56023620958924,-2.1897258615654));
#141645=CARTESIAN_POINT('Ctrl Pts',(7.12589774304569,1.55387651195406,-2.20176053641058));
#141646=CARTESIAN_POINT('Ctrl Pts',(7.16582330336277,1.54766054355409,-2.21381458823503));
#141647=CARTESIAN_POINT('',(7.21561362633324,1.45719263730544,-1.52017118865117));
#141648=CARTESIAN_POINT('Origin',(7.45931094670027E-14,1.54874775199967,
-2.84060969191202E-14));
#141649=CARTESIAN_POINT('',(7.16659671021182,1.36645689998289,-2.21130992592685));
#141650=CARTESIAN_POINT('Origin',(-0.188199584662476,1.48213731844567,0.0387106208168392));
#141651=CARTESIAN_POINT('',(6.97929310018135,1.45719264185527,-2.7458093262454));
#141652=CARTESIAN_POINT('Origin',(-0.184779512962319,1.33929189526918,0.0524389094193656));
#141653=CARTESIAN_POINT('Origin',(-0.181008753759127,1.48214299350174,0.066910520889546));
#141654=CARTESIAN_POINT('Ctrl Pts',(6.92779039,1.587508025,-2.137339541));
#141655=CARTESIAN_POINT('Ctrl Pts',(6.811862518,1.52246862,-2.513098274));
#141656=CARTESIAN_POINT('Ctrl Pts',(6.655972501,1.457192641,-2.874113787));
#141657=CARTESIAN_POINT('Ctrl Pts',(6.65060833047937,1.45494649664132,-2.88653631930577));
#141658=CARTESIAN_POINT('Ctrl Pts',(6.64524415995863,1.45270035228267,-2.89895885161157));
#141659=CARTESIAN_POINT('Ctrl Pts',(7.23596480473053,1.587508025,-1.9744853512695));
#141660=CARTESIAN_POINT('Ctrl Pts',(7.12887003486487,1.52246862,-2.36695926009757));
#141661=CARTESIAN_POINT('Ctrl Pts',(6.97995338037145,1.457192641,-2.74554727938565));
#141662=CARTESIAN_POINT('Ctrl Pts',(6.97482916303261,1.45494649664132,-2.75857448107319));
#141663=CARTESIAN_POINT('Ctrl Pts',(6.96970494569362,1.45270035228266,-2.77160168276073));
#141664=CARTESIAN_POINT('',(6.81763275884877,1.4571926425566,-2.80996156785876));
#141665=CARTESIAN_POINT('Ctrl Pts',(6.655972501,1.457192641,-2.874113787));
#141666=CARTESIAN_POINT('Ctrl Pts',(6.498334696,1.522897175,-3.23917689));
#141667=CARTESIAN_POINT('Ctrl Pts',(6.30171701800001,1.587500328,-3.584809985));
#141668=CARTESIAN_POINT('Ctrl Pts',(6.784276957,1.457192641,-3.19743431));
#141669=CARTESIAN_POINT('Ctrl Pts',(6.608905846,1.522897175,-3.569534585));
#141670=CARTESIAN_POINT('Ctrl Pts',(6.393891608,1.587500328,-3.920223221));
#141671=CARTESIAN_POINT('',(6.78427694842449,1.45719263974394,-3.19743432531899));
#141672=CARTESIAN_POINT('',(6.52238563870992,1.54766053439312,-3.70249702286805));
#141673=CARTESIAN_POINT('Origin',(-0.177079318188234,1.33935988613101,0.0626124614222701));
#141674=CARTESIAN_POINT('Ctrl Pts',(6.30404777361277,1.58673401525752,-3.58070966061121));
#141675=CARTESIAN_POINT('Ctrl Pts',(6.34041100652666,1.57991286218685,-3.60093817965368));
#141676=CARTESIAN_POINT('Ctrl Pts',(6.37680550545298,1.57325084234179,-3.62121343167707));
#141677=CARTESIAN_POINT('Ctrl Pts',(6.44957233621988,1.56023624969758,-3.66180413737314));
#141678=CARTESIAN_POINT('Ctrl Pts',(6.48598430483409,1.55387659341557,-3.68214170613826));
#141679=CARTESIAN_POINT('Ctrl Pts',(6.52238564015445,1.54766054350425,-3.70249702306713));
#141680=CARTESIAN_POINT('',(6.72012471968049,1.45719263730544,-3.03577406913007));
#141681=CARTESIAN_POINT('Origin',(8.23993651088983E-13,1.54874775200056,
-4.59051199830363E-13));
#141682=CARTESIAN_POINT('',(6.52367939340938,1.36645690002423,-3.70021717832745));
#141683=CARTESIAN_POINT('Origin',(-0.175478228337718,1.48213730287669,0.0782630889140629));
#141684=CARTESIAN_POINT('',(6.225853266432,1.45719264185525,-4.18195553973064));
#141685=CARTESIAN_POINT('Origin',(-0.169186457812871,1.33929186673091,0.0909349252721464));
#141686=CARTESIAN_POINT('Origin',(-0.1623930351778,1.48214304712937,0.104257681158234));
#141687=CARTESIAN_POINT('Ctrl Pts',(6.30635767900001,1.587508025,-3.57663988));
#141688=CARTESIAN_POINT('Ctrl Pts',(6.112363115,1.52246862,-3.918692517));
#141689=CARTESIAN_POINT('Ctrl Pts',(5.882510057,1.457192641,-4.237755942));
#141690=CARTESIAN_POINT('Ctrl Pts',(5.87460082057932,1.45494649663718,-4.24873490431392));
#141691=CARTESIAN_POINT('Ctrl Pts',(5.86669158415865,1.45270035227438,-4.25971386662783));
#141692=CARTESIAN_POINT('Ctrl Pts',(6.64233598321045,1.587508025,-3.48384152007118));
#141693=CARTESIAN_POINT('Ctrl Pts',(6.45337474141586,1.52246862,-3.8441173967213));
#141694=CARTESIAN_POINT('Ctrl Pts',(6.22655444195791,1.457192641,-4.18184156010638));
#141695=CARTESIAN_POINT('Ctrl Pts',(6.21874956266229,1.45494649663718,-4.19346263783506));
#141696=CARTESIAN_POINT('Ctrl Pts',(6.21094468336658,1.45270035227438,-4.20508371556375));
#141697=CARTESIAN_POINT('',(6.05418161852976,1.4571926425566,-4.20985574286674));
#141698=CARTESIAN_POINT('Ctrl Pts',(5.882510057,1.457192641,-4.237755942));
#141699=CARTESIAN_POINT('Ctrl Pts',(5.65007996,1.522897175,-4.560396605));
#141700=CARTESIAN_POINT('Ctrl Pts',(5.383758195,1.587500328,-4.855682001));
#141701=CARTESIAN_POINT('Ctrl Pts',(5.938310471,1.457192641,-4.58109907600001));
#141702=CARTESIAN_POINT('Ctrl Pts',(5.687048879,1.522897175,-4.906800249));
#141703=CARTESIAN_POINT('Ctrl Pts',(5.401673864,1.587500328,-5.203068274));
#141704=CARTESIAN_POINT('',(5.93831045932958,1.45719263974394,-4.58109908912447));
#141705=CARTESIAN_POINT('',(5.57396847218265,1.54766053441674,-5.01805481222604));
#141706=CARTESIAN_POINT('Origin',(-0.159479453596245,1.3393599059375,0.0992154203879853));
#141707=CARTESIAN_POINT('Ctrl Pts',(5.38691590761031,1.58673401520329,-4.85217858324993));
#141708=CARTESIAN_POINT('Ctrl Pts',(5.41808046339618,1.5799128602683,-4.87975119871157));
#141709=CARTESIAN_POINT('Ctrl Pts',(5.44926550910829,1.57325083849597,-4.90737617685212));
#141710=CARTESIAN_POINT('Ctrl Pts',(5.51160545057504,1.56023621236661,-4.96266075465083));
#141711=CARTESIAN_POINT('Ctrl Pts',(5.54279435303737,1.55387651759433,-4.99035051879934));
#141712=CARTESIAN_POINT('Ctrl Pts',(5.57396847350867,1.54766054355305,-5.01805481278384));
#141713=CARTESIAN_POINT('',(5.91041025046353,1.45719263730544,-4.40942752714433));
#141714=CARTESIAN_POINT('Origin',(-4.93528828915402E-13,1.5487477519995,
2.74953670942324E-13));
#141715=CARTESIAN_POINT('',(5.57572207888938,1.36645689999383,-5.01610638785686));
#141716=CARTESIAN_POINT('Origin',(-0.154551226723378,1.48213732987919,0.114155825250313));
#141717=CARTESIAN_POINT('',(5.18129945413096,1.45719264185526,-5.42255816067617));
#141718=CARTESIAN_POINT('Origin',(-0.145682930593092,1.33929190911084,0.125179275449958));
#141719=CARTESIAN_POINT('Origin',(-0.13618400097974,1.48214300333004,0.136729849610384));
#141720=CARTESIAN_POINT('Ctrl Pts',(5.390046691,1.587508025,-4.848700513));
#141721=CARTESIAN_POINT('Ctrl Pts',(5.127056407,1.52246862,-5.141053053));
#141722=CARTESIAN_POINT('Ctrl Pts',(4.833987981,1.457192641,-5.40324534));
#141723=CARTESIAN_POINT('Ctrl Pts',(4.82390350610173,1.45494649670983,-5.41226736797098));
#141724=CARTESIAN_POINT('Ctrl Pts',(4.81381903120335,1.45270035241968,-5.42128939594183));
#141725=CARTESIAN_POINT('Ctrl Pts',(5.73811891470674,1.587508025,-4.83029713217703));
#141726=CARTESIAN_POINT('Ctrl Pts',(5.47612681726766,1.52246862,-5.14152887785342));
#141727=CARTESIAN_POINT('Ctrl Pts',(5.18200873880599,1.457192641,-5.42259757783759));
#141728=CARTESIAN_POINT('Ctrl Pts',(5.17188814540104,1.45494649670983,-5.4322691425584));
#141729=CARTESIAN_POINT('Ctrl Pts',(5.16176755199595,1.45270035241968,-5.44194070727923));
#141730=CARTESIAN_POINT('',(5.00764367496653,1.4571926425566,-5.41290174300688));
#141731=CARTESIAN_POINT('Ctrl Pts',(4.833987981,1.457192641,-5.40324534));
#141732=CARTESIAN_POINT('Ctrl Pts',(4.537633764,1.522897175,-5.668377243));
#141733=CARTESIAN_POINT('Ctrl Pts',(4.214060823,1.587500328,-5.899507723));
#141734=CARTESIAN_POINT('Ctrl Pts',(4.814675187,1.457192641,-5.750556742));
#141735=CARTESIAN_POINT('Ctrl Pts',(4.499271827,1.522897175,-6.014629387));
#141736=CARTESIAN_POINT('Ctrl Pts',(4.156879854,1.587500328,-6.242623638));
#141737=CARTESIAN_POINT('',(4.81467517279107,1.45719263974395,-5.75055675229159));
#141738=CARTESIAN_POINT('',(4.36491873502114,1.54766053442457,-6.09897393559969));
#141739=CARTESIAN_POINT('Origin',(-0.134422621474323,1.3393598918314,0.131179301547834));
#141740=CARTESIAN_POINT('Ctrl Pts',(4.21789784076114,1.58673401530912,-5.89676502847127));
#141741=CARTESIAN_POINT('Ctrl Pts',(4.24240649244411,1.57991285950272,-5.93039247395833));
#141742=CARTESIAN_POINT('Ctrl Pts',(4.26692389901355,1.57325083682591,-5.96407546325322));
#141743=CARTESIAN_POINT('Ctrl Pts',(4.31592182297214,1.56023620921133,-6.03146877052655));
#141744=CARTESIAN_POINT('Ctrl Pts',(4.34042907888917,1.55387651117993,-6.06521587390367));
#141745=CARTESIAN_POINT('Ctrl Pts',(4.3649187362348,1.54766054355502,-6.09897393640046));
#141746=CARTESIAN_POINT('',(4.8243315668795,1.45719263730544,-5.57690105581019));
#141747=CARTESIAN_POINT('Origin',(-1.10350097115575E-12,1.54874775199972,
1.61632859874139E-12));
#141748=CARTESIAN_POINT('',(4.36705019674112,1.36645689997257,-6.09744803763054));
#141749=CARTESIAN_POINT('Origin',(-0.126397840611546,1.48213731061574,0.144710969876972));
#141750=CARTESIAN_POINT('',(3.894473836524,1.45719264185525,-6.40960798932386));
#141751=CARTESIAN_POINT('Origin',(-0.115367111514261,1.33929186087925,0.153570173473314));
#141752=CARTESIAN_POINT('Origin',(-0.103607175345854,1.48214303893616,0.162808640033903));
#141753=CARTESIAN_POINT('Ctrl Pts',(4.221703111,1.587508025,-5.8940413));
#141754=CARTESIAN_POINT('Ctrl Pts',(3.902014239,1.52246862,-6.123023663));
#141755=CARTESIAN_POINT('Ctrl Pts',(3.559433999,1.457192641,-6.316084991));
#141756=CARTESIAN_POINT('Ctrl Pts',(3.54764582377339,1.45494649662652,-6.32272822519221));
#141757=CARTESIAN_POINT('Ctrl Pts',(3.53585764854677,1.45270035225306,-6.32937145938454));
#141758=CARTESIAN_POINT('Ctrl Pts',(4.56559378165187,1.587508025,-5.95089341824206));
#141759=CARTESIAN_POINT('Ctrl Pts',(4.24282128944063,1.52246862,-6.19852818263438));
#141760=CARTESIAN_POINT('Ctrl Pts',(3.89515806501077,1.457192641,-6.40979896017689));
#141761=CARTESIAN_POINT('Ctrl Pts',(3.88319498445065,1.45494649662652,-6.41706878095212));
#141762=CARTESIAN_POINT('Ctrl Pts',(3.87123190389051,1.45270035225306,-6.4243386017273));
#141763=CARTESIAN_POINT('',(3.72695387773219,1.4571926425566,-6.36284647384276));
#141764=CARTESIAN_POINT('Ctrl Pts',(3.559433999,1.457192641,-6.316084991));
#141765=CARTESIAN_POINT('Ctrl Pts',(3.213012857,1.522897175,-6.511310861));
#141766=CARTESIAN_POINT('Ctrl Pts',(2.847318651,1.587500328,-6.667479022));
#141767=CARTESIAN_POINT('Ctrl Pts',(3.465911043,1.457192641,-6.651124765));
#141768=CARTESIAN_POINT('Ctrl Pts',(3.101113825,1.522897175,-6.84122114));
#141769=CARTESIAN_POINT('Ctrl Pts',(2.717714761,1.587500328,-6.99028085800001));
#141770=CARTESIAN_POINT('',(3.46591102690645,1.45719263974395,-6.65112477200129));
#141771=CARTESIAN_POINT('',(2.95177024883936,1.54766053440804,-6.89471181599442));
#141772=CARTESIAN_POINT('Origin',(-0.103080109074172,1.3393599228025,0.157009065809987));
#141773=CARTESIAN_POINT('Ctrl Pts',(2.85165556024229,1.58673401520964,-6.6656252952509));
#141774=CARTESIAN_POINT('Ctrl Pts',(2.8683622922353,1.57991286510536,-6.70373515343773));
#141775=CARTESIAN_POINT('Ctrl Pts',(2.88506563246328,1.57325084832053,-6.7419011346062));
#141776=CARTESIAN_POINT('Ctrl Pts',(2.91843047321997,1.56023620891076,-6.8182519981467));
#141777=CARTESIAN_POINT('Ctrl Pts',(2.93511013399784,1.55387651065815,-6.85647844996434));
#141778=CARTESIAN_POINT('Ctrl Pts',(2.95177024985786,1.54766054352959,-6.89471181703358));
#141779=CARTESIAN_POINT('',(3.51267250109602,1.45719263730544,-6.48360488878353));
#141780=CARTESIAN_POINT('Origin',(2.16623594062604E-13,1.54874775200028,
-3.87277016011822E-13));
#141781=CARTESIAN_POINT('',(2.95417990117129,1.36645689997214,-6.89367979427387));
#141782=CARTESIAN_POINT('Origin',(-0.0923341930573607,1.48213729937307,
0.168499597711493));
#141783=CARTESIAN_POINT('',(2.42554695194354,1.45719264185525,-7.09695167098787));
#141784=CARTESIAN_POINT('Origin',(-0.079656774793801,1.33929190696925,0.174780160197634));
#141785=CARTESIAN_POINT('Origin',(-0.0661858565428452,1.48214303095805,
0.181274761702213));
#141786=CARTESIAN_POINT('Ctrl Pts',(2.855957386,1.587508025,-6.663783266));
#141787=CARTESIAN_POINT('Ctrl Pts',(2.494518222,1.52246862,-6.818688491));
#141788=CARTESIAN_POINT('Ctrl Pts',(2.118444839,1.457192641,-6.933591527));
#141789=CARTESIAN_POINT('Ctrl Pts',(2.10550416565715,1.45494649660489,-6.93754533687381));
#141790=CARTESIAN_POINT('Ctrl Pts',(2.09256349231424,1.4527003522098,-6.94149914674754));
#141791=CARTESIAN_POINT('Ctrl Pts',(3.17958655851289,1.587508025,-6.79323254192744));
#141792=CARTESIAN_POINT('Ctrl Pts',(2.8111261534172,1.52246862,-6.96569119833659));
#141793=CARTESIAN_POINT('Ctrl Pts',(2.42617413046479,1.457192641,-7.09728526595308));
#141794=CARTESIAN_POINT('Ctrl Pts',(2.41292794339896,1.45494649660489,-7.10181341370261));
#141795=CARTESIAN_POINT('Ctrl Pts',(2.39968175633314,1.4527003522098,-7.10634156145212));
#141796=CARTESIAN_POINT('',(2.27199585988443,1.4571926425566,-7.01527157445221));
#141797=CARTESIAN_POINT('Ctrl Pts',(2.118444839,1.457192641,-6.933591527));
#141798=CARTESIAN_POINT('Ctrl Pts',(1.73815504,1.522897175,-7.04978282));
#141799=CARTESIAN_POINT('Ctrl Pts',(1.347439022,1.587500328,-7.123686411));
#141800=CARTESIAN_POINT('Ctrl Pts',(1.95508475,1.457192641,-7.24069358700001));
#141801=CARTESIAN_POINT('Ctrl Pts',(1.557951187,1.522897175,-7.347924996));
#141802=CARTESIAN_POINT('Ctrl Pts',(1.151472347,1.587500328,-7.411080315));
#141803=CARTESIAN_POINT('',(1.95508473278689,1.45719263974395,-7.2406935903715));
#141804=CARTESIAN_POINT('',(1.4006002665678,1.54766053440241,-7.3680606353879));
#141805=CARTESIAN_POINT('Origin',(-0.0669178377820953,1.33935992498632,
0.175497415683959));
#141806=CARTESIAN_POINT('Ctrl Pts',(1.35207303364076,1.58673401511228,-7.12280833072784));
#141807=CARTESIAN_POINT('Ctrl Pts',(1.36019668439255,1.57991286020301,-7.16361868427083));
#141808=CARTESIAN_POINT('Ctrl Pts',(1.36830495851984,1.57325083847865,-7.20448312315888));
#141809=CARTESIAN_POINT('Ctrl Pts',(1.38447655624212,1.56023620952076,-7.28622133522495));
#141810=CARTESIAN_POINT('Ctrl Pts',(1.3925486978465,1.55387651188962,-7.32713970373119));
#141811=CARTESIAN_POINT('Ctrl Pts',(1.40060026733081,1.54766054352305,-7.36806063662321));
#141812=CARTESIAN_POINT('',(2.03676477274322,1.45719263730544,-7.08714256325266));
#141813=CARTESIAN_POINT('Origin',(2.57064335096313E-13,1.548747752,-1.34397701301303E-12));
#141814=CARTESIAN_POINT('',(1.40317543654935,1.36645689995696,-7.36757074550127));
#141815=CARTESIAN_POINT('Origin',(-0.0539530301924446,1.48213733479762,
0.184409239511821));
#141816=CARTESIAN_POINT('',(0.843204186877448,1.45719264185526,-7.45244978108034));
#141817=CARTESIAN_POINT('Origin',(-0.040221868221116,1.33929184342171,0.18781761646123));
#141818=CARTESIAN_POINT('Origin',(-0.025669781634416,1.48214301518814,0.191264884919913));
#141819=CARTESIAN_POINT('Ctrl Pts',(1.356670267,1.587508025,-7.121934132));
#141820=CARTESIAN_POINT('Ctrl Pts',(0.970381306,1.52246862,-7.195519024));
#141821=CARTESIAN_POINT('Ctrl Pts',(0.578399553,1.457192641,-7.22689103));
#141822=CARTESIAN_POINT('Ctrl Pts',(0.5649114735089,1.45494649666579,-7.22797053971566));
#141823=CARTESIAN_POINT('Ctrl Pts',(0.551423394017799,1.45270035233161,
-7.22905004943133));
#141824=CARTESIAN_POINT('Ctrl Pts',(1.64490540234363,1.587508025,-7.31792766322871));
#141825=CARTESIAN_POINT('Ctrl Pts',(1.24798588253044,1.52246862,-7.40714623569068));
#141826=CARTESIAN_POINT('Ctrl Pts',(0.843744989249345,1.457192641,-7.45291040161445));
#141827=CARTESIAN_POINT('Ctrl Pts',(0.829835073136161,1.45494649666579,
-7.45448514508938));
#141828=CARTESIAN_POINT('Ctrl Pts',(0.815925157022971,1.45270035233161,
-7.4560598885642));
#141829=CARTESIAN_POINT('',(0.710801840462912,1.4571926425566,-7.33967037392361));
#141830=CARTESIAN_POINT('Ctrl Pts',(0.578399553,1.457192641,-7.22689103));
#141831=CARTESIAN_POINT('Ctrl Pts',(0.182023025,1.522897175,-7.258614769));
#141832=CARTESIAN_POINT('Ctrl Pts',(-0.215445357,1.587500328,-7.246798141));
#141833=CARTESIAN_POINT('Ctrl Pts',(0.352840867,1.457192641,-7.491695624));
#141834=CARTESIAN_POINT('Ctrl Pts',(-0.058059517,1.522897175,-7.511048045));
#141835=CARTESIAN_POINT('Ctrl Pts',(-0.468611634,1.587500328,-7.48534589300001));
#141836=CARTESIAN_POINT('Ctrl Pts',(-0.210730925521493,1.58673401525584,
-7.24693676521558));
#141837=CARTESIAN_POINT('Ctrl Pts',(-0.211570220744212,1.5799128597931,
-7.28853934333384));
#141838=CARTESIAN_POINT('Ctrl Pts',(-0.212436159925911,1.57325083749109,
-7.33019143731403));
#141839=CARTESIAN_POINT('Ctrl Pts',(-0.214213944260977,1.5602362096519,
-7.41349506349758));
#141840=CARTESIAN_POINT('Ctrl Pts',(-0.2151267644695,1.55387651209001,-7.45519205454709));
#141841=CARTESIAN_POINT('Ctrl Pts',(-0.216060227165612,1.54766054354964,
-7.49688712930759));
#141842=CARTESIAN_POINT('',(0.46562018740775,1.45719263730544,-7.35929332842941));
#141843=CARTESIAN_POINT('Ctrl Pts',(-0.206053246,1.587508025,-7.247071275));
#141844=CARTESIAN_POINT('Ctrl Pts',(-0.599129562,1.52246862,-7.235895084));
#141845=CARTESIAN_POINT('Ctrl Pts',(-0.988691053,1.457192641,-7.18226914));
#141846=CARTESIAN_POINT('Ctrl Pts',(-1.00209585148419,1.45494649664392,
-7.1804238729768));
#141847=CARTESIAN_POINT('Ctrl Pts',(-1.01550064996838,1.45270035228786,
-7.17857860595374));
#141848=CARTESIAN_POINT('Ctrl Pts',(0.0333102964716851,1.587508025,-7.50044461905109));
#141849=CARTESIAN_POINT('Ctrl Pts',(-0.373508820892593,1.52246862,-7.50225134758072));
#141850=CARTESIAN_POINT('Ctrl Pts',(-0.77813672912649,1.457192641,-7.46004573014393));
#141851=CARTESIAN_POINT('Ctrl Pts',(-0.79205996254731,1.45494649664392,
-7.45859343619367));
#141852=CARTESIAN_POINT('Ctrl Pts',(-0.80598319596813,1.45270035228786,
-7.45714114224333));
#141853=CARTESIAN_POINT('',(-0.883628482512665,1.4571926425566,-7.32087434385182));
#141854=CARTESIAN_POINT('Ctrl Pts',(-0.988691053000001,1.457192641,-7.18226914));
#141855=CARTESIAN_POINT('Ctrl Pts',(-1.382620184,1.522897175,-7.128041959));
#141856=CARTESIAN_POINT('Ctrl Pts',(-1.768255751,1.587500328,-7.031057645));
#141857=CARTESIAN_POINT('Ctrl Pts',(-1.265901463,1.457192641,-7.3923943));
#141858=CARTESIAN_POINT('Ctrl Pts',(-1.671355422,1.522897175,-7.322962836));
#141859=CARTESIAN_POINT('Ctrl Pts',(-2.066783856,1.587500328,-7.209605016));
#141860=CARTESIAN_POINT('',(-1.26590148003712,1.45719263974395,-7.39239429583215));
#141861=CARTESIAN_POINT('',(-1.82261798538781,1.54766053442901,-7.27516751052101));
#141862=CARTESIAN_POINT('Origin',(0.0129564616365227,1.3393598983656,0.187375177902643));
#141863=CARTESIAN_POINT('Ctrl Pts',(-1.76368133957537,1.58673401513823,
-7.03220649175476));
#141864=CARTESIAN_POINT('Ctrl Pts',(-1.77344433386828,1.57991286204784,
-7.07265598690311));
#141865=CARTESIAN_POINT('Ctrl Pts',(-1.78324399311111,1.57325084218189,
-7.11314811086283));
#141866=CARTESIAN_POINT('Ctrl Pts',(-1.8028879778074,1.56023624969878,-7.19412175345604));
#141867=CARTESIAN_POINT('Ctrl Pts',(-1.81274300853095,1.5538765934469,-7.23464738147635));
#141868=CARTESIAN_POINT('Ctrl Pts',(-1.82261798519599,1.54766054355515,
-7.27516751196777));
#141869=CARTESIAN_POINT('',(-1.12729628037134,1.45719263730544,-7.28733171653932));
#141870=CARTESIAN_POINT('Origin',(-6.00648003556969E-14,1.54874775200072,
-2.22044604925031E-13));
#141871=CARTESIAN_POINT('',(-1.82007512541694,1.36645689996024,-7.27580418490887));
#141872=CARTESIAN_POINT('Origin',(0.0284649540105197,1.4821373527878,0.190019460791293));
#141873=CARTESIAN_POINT('',(-2.36393104912784,1.45719264185525,-7.11771248581866));
#141874=CARTESIAN_POINT('Origin',(0.0423581924463326,1.33929188429066,0.187347329950757));
#141875=CARTESIAN_POINT('Origin',(0.0570127905286599,1.48214303509046,0.184365834749383));
#141876=CARTESIAN_POINT('Ctrl Pts',(-1.759141937,1.587508025,-7.033343419));
#141877=CARTESIAN_POINT('Ctrl Pts',(-2.140625797,1.52246862,-6.937928732));
#141878=CARTESIAN_POINT('Ctrl Pts',(-2.509551565,1.457192641,-6.801812328));
#141879=CARTESIAN_POINT('Ctrl Pts',(-2.5222462887854,1.45494649666663,-6.79712856692576));
#141880=CARTESIAN_POINT('Ctrl Pts',(-2.53494101257083,1.45270035233327,
-6.79244480585149));
#141881=CARTESIAN_POINT('Ctrl Pts',(-1.57984236134693,1.587508025,-7.33224912070202));
#141882=CARTESIAN_POINT('Ctrl Pts',(-1.97753866648013,1.52246862,-7.24655952393732));
#141883=CARTESIAN_POINT('Ctrl Pts',(-2.36363363973656,1.457192641,-7.1183576107052));
#141884=CARTESIAN_POINT('Ctrl Pts',(-2.37691915532143,1.45494649666663,
-7.11394618700318));
#141885=CARTESIAN_POINT('Ctrl Pts',(-2.39020467090635,1.45270035233327,
-7.10953476330116));
#141886=CARTESIAN_POINT('',(-2.43674132054344,1.4571926425566,-6.95976236583373));
#141887=CARTESIAN_POINT('Ctrl Pts',(-2.509551565,1.457192641,-6.801812328));
#141888=CARTESIAN_POINT('Ctrl Pts',(-2.88261361,1.522897175,-6.66416983));
#141889=CARTESIAN_POINT('Ctrl Pts',(-3.238384471,1.587500328,-6.486552707));
#141890=CARTESIAN_POINT('Ctrl Pts',(-2.825451647,1.457192641,-6.947432835));
#141891=CARTESIAN_POINT('Ctrl Pts',(-3.206500606,1.522897175,-6.792464023));
#141892=CARTESIAN_POINT('Ctrl Pts',(-3.568315562,1.587500328,-6.596751022));
#141893=CARTESIAN_POINT('',(-2.82545166272092,1.45719263974396,-6.94743282726797));
#141894=CARTESIAN_POINT('',(-3.34395215211899,1.54766053439511,-6.71326914643272));
#141895=CARTESIAN_POINT('Origin',(0.0529337710475369,1.33935993033793,0.180209392100278));
#141896=CARTESIAN_POINT('Ctrl Pts',(-3.23416397491896,1.58673401514799,
-6.48865805757573));
#141897=CARTESIAN_POINT('Ctrl Pts',(-3.25239416131963,1.57991286216089,
-6.5260631103915));
#141898=CARTESIAN_POINT('Ctrl Pts',(-3.27066931941682,1.57325084239135,
-6.56350191339419));
#141899=CARTESIAN_POINT('Ctrl Pts',(-3.3072610931085,1.56023620907719,-6.63835979603121));
#141900=CARTESIAN_POINT('Ctrl Pts',(-3.32559766007564,1.55387651099262,
-6.67581968015788));
#141901=CARTESIAN_POINT('Ctrl Pts',(-3.34395215225177,1.54766054351071,
-6.71326914788068));
#141902=CARTESIAN_POINT('',(-2.66750162710437,1.45719263730544,-6.87462257331105));
#141903=CARTESIAN_POINT('Origin',(6.51388665229291E-13,1.54874775200017,
1.46887710328336E-12));
#141904=CARTESIAN_POINT('',(-3.34160560871151,1.36645689996004,-6.7144375749348));
#141905=CARTESIAN_POINT('Origin',(0.0686481189057614,1.48213732606978,0.179457952751823));
#141906=CARTESIAN_POINT('',(-3.83876144062859,1.45719264185526,-6.44312902495316));
#141907=CARTESIAN_POINT('Origin',(0.0816420330951445,1.33929190588146,0.173861516083871));
#141908=CARTESIAN_POINT('Origin',(0.095313027403887,1.48214302028424,0.167799306102822));
#141909=CARTESIAN_POINT('Ctrl Pts',(-3.229975107,1.587508025,-6.490744241));
#141910=CARTESIAN_POINT('Ctrl Pts',(-3.582028749,1.52246862,-6.315552544));
#141911=CARTESIAN_POINT('Ctrl Pts',(-3.913068234,1.457192641,-6.103310331));
#141912=CARTESIAN_POINT('Ctrl Pts',(-3.92445929216235,1.4549464966363,-6.0960070831932));
#141913=CARTESIAN_POINT('Ctrl Pts',(-3.93585035032469,1.45270035227262,
-6.08870383538653));
#141914=CARTESIAN_POINT('Ctrl Pts',(-3.1191233455948,1.587508025,-6.8212058036725));
#141915=CARTESIAN_POINT('Ctrl Pts',(-3.48910100234763,1.52246862,-6.65202663174526));
#141916=CARTESIAN_POINT('Ctrl Pts',(-3.83860966728736,1.457192641,-6.44382300141562));
#141917=CARTESIAN_POINT('Ctrl Pts',(-3.85063624934469,1.4549464966363,-6.43665872111024));
#141918=CARTESIAN_POINT('Ctrl Pts',(-3.86266283140208,1.45270035227263,
-6.42949444080476));
#141919=CARTESIAN_POINT('',(-3.87591484165136,1.4571926425566,-6.27321963496368));
#141920=CARTESIAN_POINT('Ctrl Pts',(-3.913068234,1.457192641,-6.103310331));
#141921=CARTESIAN_POINT('Ctrl Pts',(-4.247819228,1.522897175,-5.888688526));
#141922=CARTESIAN_POINT('Ctrl Pts',(-4.557089932,1.587500328,-5.638743774));
#141923=CARTESIAN_POINT('Ctrl Pts',(-4.252886852,1.457192641,-6.177617131));
#141924=CARTESIAN_POINT('Ctrl Pts',(-4.591713385,1.522897175,-5.944357142));
#141925=CARTESIAN_POINT('Ctrl Pts',(-4.902996799,1.587500328,-5.675440282));
#141926=CARTESIAN_POINT('',(-4.2528868657407,1.45719263974395,-6.17761712005628));
#141927=CARTESIAN_POINT('',(-4.70892683314116,1.54766053440519,-5.83746577820715));
#141928=CARTESIAN_POINT('Origin',(0.0904358410859302,1.33935992808476,0.164616946156038));
#141929=CARTESIAN_POINT('Ctrl Pts',(-4.55342069736999,1.58673401524537,
-5.64170718417167));
#141930=CARTESIAN_POINT('Ctrl Pts',(-4.57926564391121,1.57991286459559,
-5.67431876527237));
#141931=CARTESIAN_POINT('Ctrl Pts',(-4.60516176487816,1.57325084723576,
-5.706953638461));
#141932=CARTESIAN_POINT('Ctrl Pts',(-4.65699029618465,1.56023620867294,
-5.77219526201295));
#141933=CARTESIAN_POINT('Ctrl Pts',(-4.68295093425734,1.55387651012817,
-5.8048375375051));
#141934=CARTESIAN_POINT('Ctrl Pts',(-4.70892683357838,1.54766054352409,
-5.8374657795963));
#141935=CARTESIAN_POINT('',(-4.08297756185057,1.45719263730544,-6.14046371846569));
#141936=CARTESIAN_POINT('Origin',(2.7148422399037E-13,1.54874775199939,
3.90312782094782E-13));
#141937=CARTESIAN_POINT('',(-4.7068863277423,1.36645689996666,-5.8391113271748));
#141938=CARTESIAN_POINT('Origin',(0.105621170002923,1.48213731632719,0.16050482919108));
#141939=CARTESIAN_POINT('',(-5.13409561478569,1.45719264185526,-5.46727201252331));
#141940=CARTESIAN_POINT('Origin',(0.117108542340334,1.33929187422864,0.15224631969547));
#141941=CARTESIAN_POINT('Origin',(0.129156500169967,1.48214300490656,0.143386714287882));
#141942=CARTESIAN_POINT('Ctrl Pts',(-4.549778231,1.587508025,-5.64464507700001));
#141943=CARTESIAN_POINT('Ctrl Pts',(-4.855940018,1.52246862,-5.397868138));
#141944=CARTESIAN_POINT('Ctrl Pts',(-5.133614182,1.457192641,-5.119424326));
#141945=CARTESIAN_POINT('Ctrl Pts',(-5.14316894137441,1.45494649658638,
-5.10984308306178));
#141946=CARTESIAN_POINT('Ctrl Pts',(-5.15272370074882,1.45270035217278,
-5.10026184012343));
#141947=CARTESIAN_POINT('Ctrl Pts',(-4.51255758975684,1.587508025,-5.99121048346444));
#141948=CARTESIAN_POINT('Ctrl Pts',(-4.83751685385146,1.52246862,-5.74645236734487));
#141949=CARTESIAN_POINT('Ctrl Pts',(-5.13409657423949,1.457192641,-5.46798239101524));
#141950=CARTESIAN_POINT('Ctrl Pts',(-5.14430187322309,1.45494649658638,
-5.45840024776324));
#141951=CARTESIAN_POINT('Ctrl Pts',(-5.1545071722067,1.45270035217278,-5.44881810451121));
#141952=CARTESIAN_POINT('',(-5.13385489337812,1.4571926425566,-5.29334812632913));
#141953=CARTESIAN_POINT('Ctrl Pts',(-5.133614182,1.457192641,-5.119424326));
#141954=CARTESIAN_POINT('Ctrl Pts',(-5.41440154,1.522897175,-4.837858691));
#141955=CARTESIAN_POINT('Ctrl Pts',(-5.662710933,1.587500328,-4.527273449));
#141956=CARTESIAN_POINT('Ctrl Pts',(-5.481461795,1.457192641,-5.118942917));
#141957=CARTESIAN_POINT('Ctrl Pts',(-5.762222749,1.522897175,-4.818298728));
#141958=CARTESIAN_POINT('Ctrl Pts',(-6.008419354,1.587500328,-4.488752262));
#141959=CARTESIAN_POINT('',(-5.48146180605169,1.45719263974395,-5.11894290336604));
#141960=CARTESIAN_POINT('',(-5.85371732860827,1.54766053443418,-4.68870899802457));
#141961=CARTESIAN_POINT('Origin',(0.123709297947897,1.33935991377548,0.14132727420044));
#141962=CARTESIAN_POINT('Ctrl Pts',(-5.65976452885599,1.58673401514067,
-4.53095635370605));
#141963=CARTESIAN_POINT('Ctrl Pts',(-5.69201580749368,1.57991285466834,
-4.557249632553));
#141964=CARTESIAN_POINT('Ctrl Pts',(-5.72432207704209,1.57325082725242,
-4.58355466254332));
#141965=CARTESIAN_POINT('Ctrl Pts',(-5.78896380224465,1.560236209744,-4.63612928610754));
#141966=CARTESIAN_POINT('Ctrl Pts',(-5.82133461356332,1.55387651227514,
-4.66242762888687));
#141967=CARTESIAN_POINT('Ctrl Pts',(-5.85371732934915,1.54766054357026,
-4.68870899927252));
#141968=CARTESIAN_POINT('',(-5.30753800421536,1.45719263730544,-5.11918360520642));
#141969=CARTESIAN_POINT('Origin',(9.69710423071035E-13,1.54874775199978,
7.9580439460436E-13));
#141970=CARTESIAN_POINT('',(-5.85207827353352,1.36645689999347,-4.69075472315437));
#141971=CARTESIAN_POINT('Origin',(0.137655674484553,1.48213726869552,0.134046934225625));
#141972=CARTESIAN_POINT('',(-6.18936518382049,1.45719264185526,-4.2357714367106));
#141973=CARTESIAN_POINT('Origin',(0.147099097618275,1.33929186443815,0.123512037903616));
#141974=CARTESIAN_POINT('Origin',(0.156960848221607,1.482142982868,0.112269617512034));
#141975=CARTESIAN_POINT('Ctrl Pts',(-5.65683878100001,1.587508025,-4.534608583));
#141976=CARTESIAN_POINT('Ctrl Pts',(-5.902792929,1.52246862,-4.227785417));
#141977=CARTESIAN_POINT('Ctrl Pts',(-6.11411803600001,1.457192641,-3.89615973));
#141978=CARTESIAN_POINT('Ctrl Pts',(-6.12138972626193,1.45494649662288,
-3.88474850057724));
#141979=CARTESIAN_POINT('Ctrl Pts',(-6.12866141652386,1.45270035224577,
-3.87333727115454));
#141980=CARTESIAN_POINT('Ctrl Pts',(-5.69498965629825,1.587508025,-4.88107282024414));
#141981=CARTESIAN_POINT('Ctrl Pts',(-5.95973579320592,1.52246862,-4.57218037652381));
#141982=CARTESIAN_POINT('Ctrl Pts',(-6.18951883121766,1.457192641,-4.23646500068588));
#141983=CARTESIAN_POINT('Ctrl Pts',(-6.19742565830312,1.45494649662288,
-4.2249130451993));
#141984=CARTESIAN_POINT('Ctrl Pts',(-6.20533248538868,1.45270035224577,
-4.2133610897127));
#141985=CARTESIAN_POINT('',(-6.15174159578327,1.4571926425566,-4.0659655425065));
#141986=CARTESIAN_POINT('Ctrl Pts',(-6.11411803599999,1.457192641,-3.89615973));
#141987=CARTESIAN_POINT('Ctrl Pts',(-6.327812453,1.522897175,-3.560815961));
#141988=CARTESIAN_POINT('Ctrl Pts',(-6.503549865,1.587500328,-3.20411285));
#141989=CARTESIAN_POINT('Ctrl Pts',(-6.45372967700001,1.457192641,-3.820912621));
#141990=CARTESIAN_POINT('Ctrl Pts',(-6.663296982,1.522897175,-3.46694202));
#141991=CARTESIAN_POINT('Ctrl Pts',(-6.83289489800001,1.587500328,-3.092175175));
#141992=CARTESIAN_POINT('',(-6.4537296848518,1.45719263974395,-3.82091260531775));
#141993=CARTESIAN_POINT('',(-6.72479450781096,1.54766053411122,-3.32071339617971));
#141994=CARTESIAN_POINT('Origin',(0.151198256987238,1.33935992429777,0.111429286576262));
#141995=CARTESIAN_POINT('Ctrl Pts',(-6.50146406158762,1.58673401527825,
-3.20834303966898));
#141996=CARTESIAN_POINT('Ctrl Pts',(-6.53861356713749,1.579912860971,-3.2270885076737));
#141997=CARTESIAN_POINT('Ctrl Pts',(-6.57581930002437,1.57325083984644,
-3.24583362870954));
#141998=CARTESIAN_POINT('Ctrl Pts',(-6.65025181673889,1.56023620668024,
-3.28328307158585));
#141999=CARTESIAN_POINT('Ctrl Pts',(-6.68751920262667,1.55387650601835,
-3.30200781611423));
#142000=CARTESIAN_POINT('Ctrl Pts',(-6.72479450885229,1.54766054352925,
-3.32071339723427));
#142001=CARTESIAN_POINT('',(-6.2839238683453,1.45719263730544,-3.85853615620902));
#142002=CARTESIAN_POINT('Ctrl Pts',(-6.499391838,1.587508025,-3.212538831));
#142003=CARTESIAN_POINT('Ctrl Pts',(-6.673637803,1.52246862,-2.860016149));
#142004=CARTESIAN_POINT('Ctrl Pts',(-6.808732526,1.457192641,-2.490715035));
#142005=CARTESIAN_POINT('Ctrl Pts',(-6.81338107273537,1.45494652485023,
-2.47800755502054));
#142006=CARTESIAN_POINT('Ctrl Pts',(-6.81802961947073,1.45270040870047,
-2.46530007504108));
#142007=CARTESIAN_POINT('Ctrl Pts',(-6.61113033294257,1.587508025,-3.54270160823892));
#142008=CARTESIAN_POINT('Ctrl Pts',(-6.8032841072071,1.52246862,-3.18411830528917));
#142009=CARTESIAN_POINT('Ctrl Pts',(-6.955526062239,1.457192641,-2.80685520692023));
#142010=CARTESIAN_POINT('Ctrl Pts',(-6.96076463727239,1.45494652485023,
-2.79387375875293));
#142011=CARTESIAN_POINT('Ctrl Pts',(-6.96600321230576,1.45270040870047,
-2.78089231058564));
#142012=CARTESIAN_POINT('',(-6.95522691796392,1.45719264137165,-2.80621090518347));
#142013=CARTESIAN_POINT('Origin',(0.177429031347391,1.48214211412438,0.0759042936399814));
#142014=CARTESIAN_POINT('',(-6.88197969794138,1.4571926425566,-2.64846292855763));
#142015=CARTESIAN_POINT('Origin',(2.9316826744008E-13,1.54874775200017,
1.08637057683048E-13));
#142016=CARTESIAN_POINT('',(-6.72363354338728,1.36645689999664,-3.32306364210357));
#142017=CARTESIAN_POINT('Origin',(0.163253390778436,1.48213728905676,0.101321039931211));
#142018=CARTESIAN_POINT('Origin',(0.170211330103566,1.33929193126131,0.0890023750191199));
#142019=CARTESIAN_POINT('Ctrl Pts',(-6.808732526,1.457192641,-2.490715035));
#142020=CARTESIAN_POINT('Ctrl Pts',(-6.94534188900001,1.522897175,-2.117273434));
#142021=CARTESIAN_POINT('Ctrl Pts',(-7.040290033,1.587500328,-1.731131494));
#142022=CARTESIAN_POINT('Ctrl Pts',(-7.124228332,1.457192641,-2.344220698));
#142023=CARTESIAN_POINT('Ctrl Pts',(-7.252802854,1.522897175,-1.953474957));
#142024=CARTESIAN_POINT('Ctrl Pts',(-7.337871871,1.587500328,-1.551011413));
#142025=CARTESIAN_POINT('',(-7.12422833628606,1.45719263974321,-2.34422068100311));
#142026=CARTESIAN_POINT('',(-6.96648043642576,1.45719263730326,-2.41746784510099));
#142027=CARTESIAN_POINT('',(-7.28142776962645,1.54766053439865,-1.79744492686919));
#142028=CARTESIAN_POINT('Origin',(0.171617199416872,1.33935992031392,0.0763209337251755));
#142029=CARTESIAN_POINT('Ctrl Pts',(-7.03916236014505,1.58673401520612,
-1.73571117070114));
#142030=CARTESIAN_POINT('Ctrl Pts',(-7.07947305391297,1.57991286063993,
-1.74603233503983));
#142031=CARTESIAN_POINT('Ctrl Pts',(-7.11983858607961,1.57325083925278,
-1.75634107332856));
#142032=CARTESIAN_POINT('Ctrl Pts',(-7.20058116476357,1.5602362496801,-1.77691410944693));
#142033=CARTESIAN_POINT('Ctrl Pts',(-7.2410022248956,1.55387659341529,-1.78718961737455));
#142034=CARTESIAN_POINT('Ctrl Pts',(-7.28142777080766,1.54766054350339,
-1.79744492773161));
#142035=CARTESIAN_POINT('Origin',(2.97071395261028E-13,1.54874775199939,
9.81202966099382E-14));
#142036=CARTESIAN_POINT('',(-7.39586996682369,1.45719264185526,-1.24543505334299));
#142037=CARTESIAN_POINT('Origin',(0.189594667274074,1.48214300128502,0.0359870116380092));
#142038=CARTESIAN_POINT('',(-7.28079918149878,1.36645690001541,-1.79998979818328));
#142039=CARTESIAN_POINT('Origin',(0.181217841331761,1.48213730043766,0.0638576089250154));
#142040=CARTESIAN_POINT('Origin',(0.185364917278654,1.33929188297289,0.050331179048184));
#142041=CARTESIAN_POINT('Ctrl Pts',(-7.03804055500001,1.587508025,-1.740254334));
#142042=CARTESIAN_POINT('Ctrl Pts',(-7.13243079,1.52246862,-1.358515705));
#142043=CARTESIAN_POINT('Ctrl Pts',(-7.184978251,1.457192641,-0.968807273));
#142044=CARTESIAN_POINT('Ctrl Pts',(-7.18678640753855,1.4549464965433,-0.955397417679967));
#142045=CARTESIAN_POINT('Ctrl Pts',(-7.18859456407698,1.45270035208663,
-0.941987562359948));
#142046=CARTESIAN_POINT('Ctrl Pts',(-7.21814190790164,1.587508025,-2.03867762345543));
#142047=CARTESIAN_POINT('Ctrl Pts',(-7.32871842370705,1.52246862,-1.64717041658003));
#142048=CARTESIAN_POINT('Ctrl Pts',(-7.39630063339368,1.457192641,-1.24600000010623));
#142049=CARTESIAN_POINT('Ctrl Pts',(-7.3986261351783,1.4549464965433,-1.23219573824825));
#142050=CARTESIAN_POINT('Ctrl Pts',(-7.40095163696292,1.45270035208663,
-1.2183914763903));
#142051=CARTESIAN_POINT('',(-7.29042407893858,1.4571926425566,-1.10712113202695));
#142052=CARTESIAN_POINT('Ctrl Pts',(-7.18497825100001,1.457192641,-0.968807273));
#142053=CARTESIAN_POINT('Ctrl Pts',(-7.238114857,1.522897175,-0.574729554));
#142054=CARTESIAN_POINT('Ctrl Pts',(-7.247834064,1.587500328,-0.177204354));
#142055=CARTESIAN_POINT('Ctrl Pts',(-7.461605988,1.457192641,-0.757915620000001));
#142056=CARTESIAN_POINT('Ctrl Pts',(-7.50317572500001,1.522897175,-0.348665576));
#142057=CARTESIAN_POINT('Ctrl Pts',(-7.499738111,1.587500328,0.062675918));
#142058=CARTESIAN_POINT('',(-7.46160598853109,1.45719263974396,-0.757915602491484));
#142059=CARTESIAN_POINT('',(-7.49758956218103,1.54766053442178,-0.190129930142415));
#142060=CARTESIAN_POINT('Origin',(0.184011793195198,1.33935989717502,0.0376439855327804));
#142061=CARTESIAN_POINT('Ctrl Pts',(-7.24771725059273,1.58673401519803,
-0.181919376803811));
#142062=CARTESIAN_POINT('Ctrl Pts',(-7.28930422196723,1.57991286491238,
-0.18333362947525));
#142063=CARTESIAN_POINT('Ctrl Pts',(-7.33094207499939,1.57325084793404,
-0.184723957980302));
#142064=CARTESIAN_POINT('Ctrl Pts',(-7.41421984954447,1.56023620870582,
-0.187458750645032));
#142065=CARTESIAN_POINT('Ctrl Pts',(-7.45590511399854,1.55387651022022,
-0.18880469894532));
#142066=CARTESIAN_POINT('Ctrl Pts',(-7.4975895635242,1.54766054354907,-0.190129930705154));
#142067=CARTESIAN_POINT('',(-7.32329212215043,1.45719263730543,-0.863361424018223));
#142068=CARTESIAN_POINT('Origin',(-2.48412401759879E-12,1.54874775199939,
-1.02673945734377E-13));
#142069=CARTESIAN_POINT('',(-7.49752274173799,1.36645690002332,-0.192750431785836));
#142070=CARTESIAN_POINT('Origin',(0.190708686305372,1.48213731107654,0.0234081809724727));
#142071=CARTESIAN_POINT('',(-7.4906903586766,1.45719264185525,0.373575949174442));
#142072=CARTESIAN_POINT('Origin',(0.191850856540546,1.33929189026274,0.00930648937180201));
#142073=CARTESIAN_POINT('Origin',(0.192898202986575,1.48214301628634,-0.0056115938680452));
#142074=CARTESIAN_POINT('Ctrl Pts',(-7.24759831800001,1.587508025,-0.186597478));
#142075=CARTESIAN_POINT('Ctrl Pts',(-7.257719241,1.52246862,0.206507424));
#142076=CARTESIAN_POINT('Ctrl Pts',(-7.225262378,1.457192641,0.59840084));
#142077=CARTESIAN_POINT('Ctrl Pts',(-7.22414553838937,1.45494649666465,
0.611885879824641));
#142078=CARTESIAN_POINT('Ctrl Pts',(-7.22302869877862,1.45270035232932,
0.625370919649284));
#142079=CARTESIAN_POINT('Ctrl Pts',(-7.48764118811158,1.587508025,-0.439327329442798));
#142080=CARTESIAN_POINT('Ctrl Pts',(-7.51147000933402,1.52246862,-0.0332026618115801));
#142081=CARTESIAN_POINT('Ctrl Pts',(-7.49123240332272,1.457192641,0.373116791162346));
#142082=CARTESIAN_POINT('Ctrl Pts',(-7.49053602795158,1.45494649666465,
0.387098230454708));
#142083=CARTESIAN_POINT('Ctrl Pts',(-7.48983965258032,1.45270035232932,
0.401079669747064));
#142084=CARTESIAN_POINT('',(-7.35797633236851,1.4571926425566,0.485988418560827));
#142085=CARTESIAN_POINT('Ctrl Pts',(-7.225262378,1.457192641,0.59840084));
#142086=CARTESIAN_POINT('Ctrl Pts',(-7.192441619,1.522897175,0.994688041));
#142087=CARTESIAN_POINT('Ctrl Pts',(-7.116477429,1.587500328,1.385008664));
#142088=CARTESIAN_POINT('Ctrl Pts',(-7.450087241,1.457192641,0.86382875));
#142089=CARTESIAN_POINT('Ctrl Pts',(-7.402708438,1.522897175,1.27244702));
#142090=CARTESIAN_POINT('Ctrl Pts',(-7.310924932,1.587500328,1.673432593));
#142091=CARTESIAN_POINT('',(-7.45008723775429,1.45719263974396,0.863828767210929));
#142092=CARTESIAN_POINT('',(-7.36317239925506,1.54766053442505,1.42607533061921));
#142093=CARTESIAN_POINT('Origin',(0.187802206685309,1.33935989621408,-0.00279323486872568));
#142094=CARTESIAN_POINT('Ctrl Pts',(-7.11737693722939,1.58673401523545,
1.38037876479302));
#142095=CARTESIAN_POINT('Ctrl Pts',(-7.15829567894936,1.57991286024203,
1.38793755122839));
#142096=CARTESIAN_POINT('Ctrl Pts',(-7.19925897331848,1.57325083844015,
1.39553064135406));
#142097=CARTESIAN_POINT('Ctrl Pts',(-7.2811773413793,1.56023624971792,1.41076198743301));
#142098=CARTESIAN_POINT('Ctrl Pts',(-7.32217707587334,1.55387659344704,
1.4184085517289));
#142099=CARTESIAN_POINT('Ctrl Pts',(-7.36317240068876,1.54766054355037,
1.42607533035161));
#142100=CARTESIAN_POINT('',(-7.33767480725555,1.45719263730543,0.73111481752593));
#142101=CARTESIAN_POINT('Origin',(-3.37837396946483E-13,1.54874775200022,
4.32054565735474E-14));
#142102=CARTESIAN_POINT('',(-7.36367047181139,1.36645689998334,1.42350173056156));
#142103=CARTESIAN_POINT('Origin',(0.191281723351053,1.48213728127495,-0.0181357654416722));
#142104=CARTESIAN_POINT('',(-7.23525439421974,1.45719264185526,1.97511895503844));
#142105=CARTESIAN_POINT('Origin',(0.189366035974033,1.33929190661057,-0.0321533450512154));
#142106=CARTESIAN_POINT('Origin',(0.187181716114306,1.48214299980185,-0.0469477408946925));
#142107=CARTESIAN_POINT('Ctrl Pts',(-7.118266439,1.587508025,1.375784468));
#142108=CARTESIAN_POINT('Ctrl Pts',(-7.043644806,1.52246862,1.761874495));
#142109=CARTESIAN_POINT('Ctrl Pts',(-6.927701267,1.457192641,2.137628395));
#142110=CARTESIAN_POINT('Ctrl Pts',(-6.92371165326549,1.45494649650072,
2.15055807554245));
#142111=CARTESIAN_POINT('Ctrl Pts',(-6.91972203953099,1.45270035200146,
2.16348775608497));
#142112=CARTESIAN_POINT('Ctrl Pts',(-7.40702668670085,1.587508025,1.18056542134086));
#142113=CARTESIAN_POINT('Ctrl Pts',(-7.34299360589532,1.52246862,1.58231761286301));
#142114=CARTESIAN_POINT('Ctrl Pts',(-7.23588247160926,1.457192641,1.97478705544074));
#142115=CARTESIAN_POINT('Ctrl Pts',(-7.2321967806587,1.45494649650072,1.988291917307));
#142116=CARTESIAN_POINT('Ctrl Pts',(-7.22851108970826,1.45270035200146,
2.00179677917319));
#142117=CARTESIAN_POINT('',(-7.08147779032799,1.4571926425566,2.05637369070155));
#142118=CARTESIAN_POINT('Ctrl Pts',(-6.927701267,1.457192641,2.137628395));
#142119=CARTESIAN_POINT('Ctrl Pts',(-6.810457805,1.522897175,2.517595128));
#142120=CARTESIAN_POINT('Ctrl Pts',(-6.65236221900001,1.587500328,2.882460217));
#142121=CARTESIAN_POINT('Ctrl Pts',(-7.090210694,1.457192641,2.445181447));
#142122=CARTESIAN_POINT('Ctrl Pts',(-6.956098733,1.522897175,2.834061408));
#142123=CARTESIAN_POINT('Ctrl Pts',(-6.78026102800001,1.587500328,3.20594142));
#142124=CARTESIAN_POINT('',(-7.09021068713113,1.45719263974395,2.44518146316404));
#142125=CARTESIAN_POINT('',(-6.88446147870823,1.54766053440234,2.97559889400155));
#142126=CARTESIAN_POINT('Origin',(0.182810596389243,1.33935993317304,-0.0430996776829071));
#142127=CARTESIAN_POINT('Ctrl Pts',(-6.65423598875174,1.58673401519076,
2.8781319295331));
#142128=CARTESIAN_POINT('Ctrl Pts',(-6.69257316710717,1.57991285848942,
2.89431032002908));
#142129=CARTESIAN_POINT('Ctrl Pts',(-6.73094648358784,1.57325083489832,
2.9105317901649));
#142130=CARTESIAN_POINT('Ctrl Pts',(-6.8076755759705,1.56023620896865,2.94301715641383));
#142131=CARTESIAN_POINT('Ctrl Pts',(-6.84607324461083,1.55387651075103,
2.95929879432475));
#142132=CARTESIAN_POINT('Ctrl Pts',(-6.884461480162,1.54766054352115,2.9755988940552));
#142133=CARTESIAN_POINT('',(-7.00895597346562,1.45719263730543,2.29140494251679));
#142134=CARTESIAN_POINT('Origin',(9.87925019568792E-13,1.54874775199989,
-3.72531866466019E-13));
#142135=CARTESIAN_POINT('',(-6.88550115471298,1.36645690001127,2.97319253421908));
#142136=CARTESIAN_POINT('Origin',(0.182911044278466,1.48213728633115,-0.0588316746106976));
#142137=CARTESIAN_POINT('',(-6.64150597624838,1.45719264185525,3.48430759351434));
#142138=CARTESIAN_POINT('Origin',(0.178026527221111,1.3392919067952,-0.0721096143840466));
#142139=CARTESIAN_POINT('Origin',(0.172713603740644,1.4821430259791,-0.0860888809879978));
#142140=CARTESIAN_POINT('Ctrl Pts',(-6.656092333,1.587508025,2.873836261));
#142141=CARTESIAN_POINT('Ctrl Pts',(-6.500217369,1.52246862,3.234858274));
#142142=CARTESIAN_POINT('Ctrl Pts',(-6.306208544,1.457192641,3.576902822));
#142143=CARTESIAN_POINT('Ctrl Pts',(-6.29953270679689,1.45494649673786,
3.58867256349837));
#142144=CARTESIAN_POINT('Ctrl Pts',(-6.29285686959388,1.45270035247575,
3.6004423049968));
#142145=CARTESIAN_POINT('Ctrl Pts',(-6.98006785141597,1.587508025,2.74525624586515));
#142146=CARTESIAN_POINT('Ctrl Pts',(-6.8311669814129,1.52246862,3.12385047355734));
#142147=CARTESIAN_POINT('Ctrl Pts',(-6.64219071806767,1.457192641,3.48411847163471));
#142148=CARTESIAN_POINT('Ctrl Pts',(-6.63568805114341,1.45494649673787,
3.49651528144297));
#142149=CARTESIAN_POINT('Ctrl Pts',(-6.62918538421904,1.45270035247575,
3.50891209125129));
#142150=CARTESIAN_POINT('',(-6.47385721741239,1.4571926425566,3.53060521441202));
#142151=CARTESIAN_POINT('Ctrl Pts',(-6.306208544,1.457192641,3.576902822));
#142152=CARTESIAN_POINT('Ctrl Pts',(-6.110024554,1.522897175,3.922782265));
#142153=CARTESIAN_POINT('Ctrl Pts',(-5.877189946,1.587500328,4.245131134));
#142154=CARTESIAN_POINT('Ctrl Pts',(-6.398803776,1.457192641,3.912200178));
#142155=CARTESIAN_POINT('Ctrl Pts',(-6.184229582,1.522897175,4.263158233));
#142156=CARTESIAN_POINT('Ctrl Pts',(-5.932559655,1.587500328,4.58854398900001));
#142157=CARTESIAN_POINT('',(-6.39880376581881,1.45719263974394,3.91220019230033));
#142158=CARTESIAN_POINT('',(-6.08384079107012,1.54766053443313,4.38598675995203));
#142159=CARTESIAN_POINT('Origin',(0.169271559227505,1.3393598742129,-0.0813909837261839));
#142160=CARTESIAN_POINT('Ctrl Pts',(-5.87995036175847,1.5867340152341,4.24130684477094));
#142161=CARTESIAN_POINT('Ctrl Pts',(-5.91391334078849,1.57991286287284,
4.26534833798605));
#142162=CARTESIAN_POINT('Ctrl Pts',(-5.9479023493887,1.57325084375826,4.28943967034669));
#142163=CARTESIAN_POINT('Ctrl Pts',(-6.01585420760897,1.56023620959703,
4.33766006384379));
#142164=CARTESIAN_POINT('Ctrl Pts',(-6.04985408564389,1.55387651199764,
4.36181540730131));
#142165=CARTESIAN_POINT('Ctrl Pts',(-6.08384079247201,1.54766054356863,
4.38598676033019));
#142166=CARTESIAN_POINT('',(-6.3525061485046,1.45719263730543,3.74455151950157));
#142167=CARTESIAN_POINT('Origin',(9.04224611852911E-13,1.54874775199961,
-6.71771666072019E-13));
#142168=CARTESIAN_POINT('',(-6.08537345586261,1.3664568999914,4.38386015927589));
#142169=CARTESIAN_POINT('Origin',(0.1659877218699,1.48213730823444,-0.0967767643559736));
#142170=CARTESIAN_POINT('',(-5.73720811971245,1.45719264185525,4.83057388182145));
#142171=CARTESIAN_POINT('Origin',(0.158363050588438,1.33929187171589,-0.108694257324458));
#142172=CARTESIAN_POINT('Origin',(0.150168911388342,1.48214300824914,-0.121204356352433));
#142173=CARTESIAN_POINT('Ctrl Pts',(-5.882686747,1.587508025,4.237510666));
#142174=CARTESIAN_POINT('Ctrl Pts',(-5.652846992,1.52246862,4.556583674));
#142175=CARTESIAN_POINT('Ctrl Pts',(-5.389844518,1.457192641,4.848925249));
#142176=CARTESIAN_POINT('Ctrl Pts',(-5.38079461137339,1.45494649667319,
4.85898471314341));
#142177=CARTESIAN_POINT('Ctrl Pts',(-5.3717447047468,1.4527003523464,4.86904417728667));
#142178=CARTESIAN_POINT('Ctrl Pts',(-6.22672880019407,1.587508025,4.18158193886891));
#142179=CARTESIAN_POINT('Ctrl Pts',(-5.99992258232298,1.52246862,4.51931555899604));
#142180=CARTESIAN_POINT('Ctrl Pts',(-5.73791750828063,1.457192641,4.83053638075679));
#142181=CARTESIAN_POINT('Ctrl Pts',(-5.72890192215432,1.45494649667319,
4.84124547917079));
#142182=CARTESIAN_POINT('Ctrl Pts',(-5.71988633602798,1.4527003523464,4.85195457758482));
#142183=CARTESIAN_POINT('',(-5.56352627571132,1.4571926425566,4.83974956272915));
#142184=CARTESIAN_POINT('Ctrl Pts',(-5.389844518,1.457192641,4.848925249));
#142185=CARTESIAN_POINT('Ctrl Pts',(-5.12389334400001,1.522897175,5.144544464));
#142186=CARTESIAN_POINT('Ctrl Pts',(-4.827206802,1.587500328,5.409304437));
#142187=CARTESIAN_POINT('Ctrl Pts',(-5.408195905,1.457192641,5.19628877700001));
#142188=CARTESIAN_POINT('Ctrl Pts',(-5.123192728,1.522897175,5.492914519));
#142189=CARTESIAN_POINT('Ctrl Pts',(-4.807458386,1.587500328,5.756591341));
#142190=CARTESIAN_POINT('',(-5.40819589198951,1.45719263974395,5.19628878876201));
#142191=CARTESIAN_POINT('',(-4.99874646949496,1.54766053441164,5.59129076007773));
#142192=CARTESIAN_POINT('Origin',(0.147817494022358,1.33935992725899,-0.1158765739251));
#142193=CARTESIAN_POINT('Ctrl Pts',(-4.83072478992621,1.58673401522937,
5.406162965312));
#142194=CARTESIAN_POINT('Ctrl Pts',(-4.85872552726679,1.57991286184182,
5.43694342298225));
#142195=CARTESIAN_POINT('Ctrl Pts',(-4.88674097219751,1.57325084166877,
5.46777815078991));
#142196=CARTESIAN_POINT('Ctrl Pts',(-4.9427381876837,1.56023620910422,5.52947881162374));
#142197=CARTESIAN_POINT('Ctrl Pts',(-4.97075048493763,1.55387651101871,
5.56037838786652));
#142198=CARTESIAN_POINT('Ctrl Pts',(-4.99874647078971,1.54766054353552,
5.5912907607398));
#142199=CARTESIAN_POINT('',(-5.3990201960811,1.45719263730543,5.02260702957445));
#142200=CARTESIAN_POINT('Origin',(3.33934269125535E-13,1.5487477520005,
-3.63424568217141E-13));
#142201=CARTESIAN_POINT('',(-5.00070045811103,1.36645689998942,5.58954335527285));
#142202=CARTESIAN_POINT('Origin',(0.141302887539335,1.48213731600747,-0.130196646736684));
#142203=CARTESIAN_POINT('',(-4.56464478872102,1.45719264185524,5.95096790420931));
#142204=CARTESIAN_POINT('Origin',(0.131294734058009,1.33929188265673,-0.140196623232732));
#142205=CARTESIAN_POINT('Origin',(0.120602720415548,1.48214303576771,-0.150652559824696));
#142206=CARTESIAN_POINT('Ctrl Pts',(-4.834213266,1.587508025,5.403043781));
#142207=CARTESIAN_POINT('Ctrl Pts',(-4.541155773,1.52246862,5.665248286));
#142208=CARTESIAN_POINT('Ctrl Pts',(-4.221457354,1.457192641,5.89421732));
#142209=CARTESIAN_POINT('Ctrl Pts',(-4.21045654185964,1.4549464966978,5.90209613697032));
#142210=CARTESIAN_POINT('Ctrl Pts',(-4.19945572971929,1.45270035239562,
5.90997495394052));
#142211=CARTESIAN_POINT('Ctrl Pts',(-5.18223483045369,1.587508025,5.4223815082615));
#142212=CARTESIAN_POINT('Ctrl Pts',(-4.88812847159532,1.52246862,5.70346247133777));
#142213=CARTESIAN_POINT('Ctrl Pts',(-4.56534565379732,1.457192641,5.95108377746541));
#142214=CARTESIAN_POINT('Ctrl Pts',(-4.55423870759519,1.4549464966978,5.95960441850951));
#142215=CARTESIAN_POINT('Ctrl Pts',(-4.54313176139316,1.45270035239562,
5.96812505955364));
#142216=CARTESIAN_POINT('',(-4.39305102980428,1.4571926425566,5.92259260020826));
#142217=CARTESIAN_POINT('Ctrl Pts',(-4.221457354,1.457192641,5.89421732));
#142218=CARTESIAN_POINT('Ctrl Pts',(-3.898174577,1.522897175,6.125753481));
#142219=CARTESIAN_POINT('Ctrl Pts',(-3.551508834,1.587500328,6.320544676));
#142220=CARTESIAN_POINT('Ctrl Pts',(-4.164706805,1.457192641,6.237404687));
#142221=CARTESIAN_POINT('Ctrl Pts',(-3.822601077,1.522897175,6.465828226));
#142222=CARTESIAN_POINT('Ctrl Pts',(-3.457565706,1.587500328,6.65546688));
#142223=CARTESIAN_POINT('',(-4.16470678976563,1.45719263974395,6.23740469568957));
#142224=CARTESIAN_POINT('',(-3.67991631912743,1.54766053440482,6.53515221826147));
#142225=CARTESIAN_POINT('Origin',(0.119451572345765,1.33935994579391,-0.144943851805711));
#142226=CARTESIAN_POINT('Ctrl Pts',(-3.55561989709399,1.58673401518731,
6.31823291346998));
#142227=CARTESIAN_POINT('Ctrl Pts',(-3.57634910582028,1.57991286122881,
6.35431307522638));
#142228=CARTESIAN_POINT('Ctrl Pts',(-3.59708101208162,1.57325084046458,
6.39044940037043));
#142229=CARTESIAN_POINT('Ctrl Pts',(-3.63850521952105,1.56023620976,6.46274527001499));
#142230=CARTESIAN_POINT('Ctrl Pts',(-3.65922010693531,1.55387651235248,
6.49894424315467));
#142231=CARTESIAN_POINT('Ctrl Pts',(-3.67991632024148,1.54766054352706,
6.53515221919074));
#142232=CARTESIAN_POINT('',(-4.19308206087856,1.45719263730543,6.06581101637234));
#142233=CARTESIAN_POINT('Origin',(-2.08166817117217E-13,1.54874775199961,
4.32813507256213E-13));
#142234=CARTESIAN_POINT('',(-3.68220026482123,1.36645690002958,6.53386571702019));
#142235=CARTESIAN_POINT('Origin',(0.110010924704643,1.48213728422803,-0.157528746971618));
#142236=CARTESIAN_POINT('',(-3.17864374056536,1.45719264185526,6.79310128094016));
#142237=CARTESIAN_POINT('Origin',(0.0980868957313646,1.33929187957912,-0.165143190374958));
#142238=CARTESIAN_POINT('Origin',(0.0853972507623617,1.48214300224995,-0.173056429922132));
#142239=CARTESIAN_POINT('Ctrl Pts',(-3.559697347,1.587508025,6.315936573));
#142240=CARTESIAN_POINT('Ctrl Pts',(-3.217125156,1.52246862,6.509012185));
#142241=CARTESIAN_POINT('Ctrl Pts',(-2.855679535,1.457192641,6.66390234));
#142242=CARTESIAN_POINT('Ctrl Pts',(-2.84324220287946,1.45494649667524,
6.66923210522061));
#142243=CARTESIAN_POINT('Ctrl Pts',(-2.83080487075887,1.4527003523505,6.67456187044107));
#142244=CARTESIAN_POINT('Ctrl Pts',(-3.89542532096169,1.587508025,6.40963654464227));
#142245=CARTESIAN_POINT('Ctrl Pts',(-3.54777090608225,1.52246862,6.62092181761493));
#142246=CARTESIAN_POINT('Ctrl Pts',(-3.17930331049195,1.457192641,6.79336511042453));
#142247=CARTESIAN_POINT('Ctrl Pts',(-3.16662435245302,1.45494649667524,
6.79929887854907));
#142248=CARTESIAN_POINT('Ctrl Pts',(-3.153945394414,1.4527003523505,6.80523264667356));
#142249=CARTESIAN_POINT('',(-3.01716159975711,1.4571926425566,6.72850178992045));
#142250=CARTESIAN_POINT('Ctrl Pts',(-2.855679535,1.457192641,6.66390234));
#142251=CARTESIAN_POINT('Ctrl Pts',(-2.4901815,1.522897175,6.820529074));
#142252=CARTESIAN_POINT('Ctrl Pts',(-2.109746259,1.587500328,6.936243271));
#142253=CARTESIAN_POINT('Ctrl Pts',(-2.726480643,1.457192641,6.986866487));
#142254=CARTESIAN_POINT('Ctrl Pts',(-2.343268848,1.522897175,7.136406991));
#142255=CARTESIAN_POINT('Ctrl Pts',(-1.946001096,1.587500328,7.243140185));
#142256=CARTESIAN_POINT('',(-2.72648062626192,1.45719263974396,6.98686649220436));
#142257=CARTESIAN_POINT('',(-2.18901737115193,1.54766053442488,7.1734372219873));
#142258=CARTESIAN_POINT('Origin',(0.0855002844435065,1.33935992351952,-0.167233897191608));
#142259=CARTESIAN_POINT('Ctrl Pts',(-2.11425816793634,1.58673401521377,
6.93486931377602));
#142260=CARTESIAN_POINT('Ctrl Pts',(-2.12674657914192,1.57991285703008,
6.974562133025));
#142261=CARTESIAN_POINT('Ctrl Pts',(-2.13922555206339,1.57325083195643,
7.01431038546371));
#142262=CARTESIAN_POINT('Ctrl Pts',(-2.16413971704552,1.56023624975565,
7.09382070150504));
#142263=CARTESIAN_POINT('Ctrl Pts',(-2.17658850712719,1.55387659347072,
7.13362617601876));
#142264=CARTESIAN_POINT('Ctrl Pts',(-2.18901737205927,1.54766054355077,
7.17343722312894));
#142265=CARTESIAN_POINT('',(-2.79108006804675,1.45719263730543,6.82538442206834));
#142266=CARTESIAN_POINT('Origin',(1.88868018446975E-13,1.54874775200011,
-8.56086035394554E-13));
#142267=CARTESIAN_POINT('',(-2.19152447924759,1.36645689997044,7.17267177913987));
#142268=CARTESIAN_POINT('Origin',(0.0735749316633463,1.48213731777391,-0.177494984800044));
#142269=CARTESIAN_POINT('',(-1.64401284267834,1.45719264185524,7.31759679238916));
#142270=CARTESIAN_POINT('Origin',(0.0602927793857641,1.33929186759675,-0.182368014253653));
#142271=CARTESIAN_POINT('Origin',(0.046198706450094,1.48214301892206,-0.187368375610238));
#142272=CARTESIAN_POINT('Ctrl Pts',(-2.118733935,1.587508025,6.933503192));
#142273=CARTESIAN_POINT('Ctrl Pts',(-1.742665343,1.52246862,7.048421908));
#142274=CARTESIAN_POINT('Ctrl Pts',(-1.356373314,1.457192641,7.121990693));
#142275=CARTESIAN_POINT('Ctrl Pts',(-1.34308101774021,1.45494649666779,
7.12452219251923));
#142276=CARTESIAN_POINT('Ctrl Pts',(-1.32978872148043,1.4527003523356,7.12705369203845));
#142277=CARTESIAN_POINT('Ctrl Pts',(-2.42647005135815,1.587508025,7.09718409979056));
#142278=CARTESIAN_POINT('Ctrl Pts',(-2.04152351582573,1.52246862,7.22879421816179));
#142279=CARTESIAN_POINT('Ctrl Pts',(-1.64460027668501,1.457192641,7.31799624172302));
#142280=CARTESIAN_POINT('Ctrl Pts',(-1.63094216082715,1.45494649666779,
7.32106568047695));
#142281=CARTESIAN_POINT('Ctrl Pts',(-1.61728404496923,1.45270035233559,
7.32413511923084));
#142282=CARTESIAN_POINT('',(-1.50019304561873,1.4571926425566,7.21979371444933));
#142283=CARTESIAN_POINT('Ctrl Pts',(-1.356373314,1.457192641,7.121990693));
#142284=CARTESIAN_POINT('Ctrl Pts',(-0.965750302,1.522897175,7.196384307));
#142285=CARTESIAN_POINT('Ctrl Pts',(-0.569334295,1.587500328,7.22761084000001));
#142286=CARTESIAN_POINT('Ctrl Pts',(-1.160767276,1.457192641,7.409630175));
#142287=CARTESIAN_POINT('Ctrl Pts',(-0.754367972,1.522897175,7.473295298));
#142288=CARTESIAN_POINT('Ctrl Pts',(-0.343443638,1.587500328,7.49213230400001));
#142289=CARTESIAN_POINT('',(-1.16076725851918,1.45719263974395,7.4096301764929));
#142290=CARTESIAN_POINT('',(-0.59576240422708,1.54766053440468,7.47630027399342));
#142291=CARTESIAN_POINT('Origin',(0.0475509340222015,1.33935995780179,-0.181703625814522));
#142292=CARTESIAN_POINT('Ctrl Pts',(-0.574036078207936,1.58673401524647,
7.22723893192767));
#142293=CARTESIAN_POINT('Ctrl Pts',(-0.577699733054604,1.57991285914198,
7.26868838164303));
#142294=CARTESIAN_POINT('Ctrl Pts',(-0.581342253842358,1.5732508361904,
7.31018993810145));
#142295=CARTESIAN_POINT('Ctrl Pts',(-0.5885815969205,1.56023620877839,7.39319744444684));
#142296=CARTESIAN_POINT('Ctrl Pts',(-0.592182365966404,1.55387651034652,
7.434748705256));
#142297=CARTESIAN_POINT('Ctrl Pts',(-0.595762404863382,1.54766054352378,
7.47630027530278));
#142298=CARTESIAN_POINT('',(-1.25857027269469,1.45719263730543,7.26581043786369));
#142299=CARTESIAN_POINT('Origin',(6.04950930929021E-14,1.54874775200061,
7.50267903359969E-14));
#142300=CARTESIAN_POINT('',(-0.598375444936869,1.36645689998177,7.47609168110421));
#142301=CARTESIAN_POINT('Origin',(0.0336986056209087,1.48213727193679,-0.189161605056248));
#142302=CARTESIAN_POINT('',(-0.0325097326105792,1.45719264185525,7.49992961001097));
#142303=CARTESIAN_POINT('Origin',(0.0196794318992366,1.33929185017855,-0.191065540471456));
#142304=CARTESIAN_POINT('Origin',(0.00483994282569893,1.48214301066781,
-0.192919282835899));
#142305=CARTESIAN_POINT('Ctrl Pts',(-0.57870088,1.587508025,7.226866907));
#142306=CARTESIAN_POINT('Ctrl Pts',(-0.186720435,1.52246862,7.258255257));
#142307=CARTESIAN_POINT('Ctrl Pts',(0.206355414,1.457192641,7.247062677));
#142308=CARTESIAN_POINT('Ctrl Pts',(0.21988114116028,1.45494649668887,7.24667754068678));
#142309=CARTESIAN_POINT('Ctrl Pts',(0.23340686832056,1.45270035237775,7.24629240437358));
#142310=CARTESIAN_POINT('Ctrl Pts',(-0.844055740452744,1.587508025,7.45287521505935));
#142311=CARTESIAN_POINT('Ctrl Pts',(-0.439816755395308,1.52246862,7.49865623502241));
#142312=CARTESIAN_POINT('Ctrl Pts',(-0.0329975629266414,1.457192641,7.50044600138326));
#142313=CARTESIAN_POINT('Ctrl Pts',(-0.0189989277652717,1.45494649668887,
7.50050758718543));
#142314=CARTESIAN_POINT('Ctrl Pts',(-0.00500029260390189,1.45270035237775,
7.5005691729876));
#142315=CARTESIAN_POINT('',(0.0869228665809933,1.4571926425566,7.37349610888705));
#142316=CARTESIAN_POINT('Ctrl Pts',(-1.642244642,4.301266351,7.317993751));
#142317=CARTESIAN_POINT('Ctrl Pts',(-1.243612454,4.365380951,7.407451544));
#142318=CARTESIAN_POINT('Ctrl Pts',(-0.837621771000001,4.430609079,7.453079214));
#142319=CARTESIAN_POINT('Ctrl Pts',(-0.833550507349874,4.43126318491329,
7.45353676704762));
#142320=CARTESIAN_POINT('Ctrl Pts',(-0.829479243699748,4.43191729082659,
7.45399432009524));
#142321=CARTESIAN_POINT('Ctrl Pts',(-1.354652431,4.301266351,7.122318217));
#142322=CARTESIAN_POINT('Ctrl Pts',(-0.966679253,4.365380951,7.196110035));
#142323=CARTESIAN_POINT('Ctrl Pts',(-0.572986203,4.430609079,7.22732224400001));
#142324=CARTESIAN_POINT('Ctrl Pts',(-0.569038259682857,4.43126318491329,
7.22763523919241));
#142325=CARTESIAN_POINT('Ctrl Pts',(-0.565090316365713,4.43191729082659,
7.22794823438482));
#142326=CARTESIAN_POINT('',(-0.837621778443153,4.43060908007271,7.45307921003498));
#142327=CARTESIAN_POINT('',(-0.705304006274358,4.43060908208283,7.34020072714797));
#142328=CARTESIAN_POINT('',(-1.39540249029647,4.34096089506028,7.36904687802678));
#142329=CARTESIAN_POINT('Origin',(0.00129585974664434,4.55349066438059,
-0.187514887673611));
#142330=CARTESIAN_POINT('Ctrl Pts',(-1.35005064267087,4.30202682666956,
7.12319192941445));
#142331=CARTESIAN_POINT('Ctrl Pts',(-1.35748387767582,4.30883434438056,
7.16413036593558));
#142332=CARTESIAN_POINT('Ctrl Pts',(-1.36498789722174,4.31547777947418,
7.20511000407318));
#142333=CARTESIAN_POINT('Ctrl Pts',(-1.38010626519058,4.32844538542126,
7.28704728890771));
#142334=CARTESIAN_POINT('Ctrl Pts',(-1.38772947470995,4.33477714733287,
7.32805291775489));
#142335=CARTESIAN_POINT('Ctrl Pts',(-1.39540248946664,4.3409608950497,7.3690468781837));
#142336=CARTESIAN_POINT('Ctrl Pts',(-1.95752567888767,4.43188407004788,
7.24003864400306));
#142337=CARTESIAN_POINT('Ctrl Pts',(-1.95359317694383,4.43124657452394,
7.24109731250152));
#142338=CARTESIAN_POINT('Ctrl Pts',(-1.949660675,4.430609079,7.242155981));
#142339=CARTESIAN_POINT('Ctrl Pts',(-1.943374636,4.429590053,7.243848245));
#142340=CARTESIAN_POINT('Ctrl Pts',(-1.93708567,4.428571429,7.245529595));
#142341=CARTESIAN_POINT('Ctrl Pts',(-1.547673393,4.365498301,7.349638609));
#142342=CARTESIAN_POINT('Ctrl Pts',(-1.149345823,4.301245526,7.411410404));
#142343=CARTESIAN_POINT('Ctrl Pts',(-2.12078237088003,4.43188407004788,
6.93288137335172));
#142344=CARTESIAN_POINT('Ctrl Pts',(-2.11701655944001,4.43124657452394,
6.93402887167586));
#142345=CARTESIAN_POINT('Ctrl Pts',(-2.113250748,4.430609079,6.93517637));
#142346=CARTESIAN_POINT('Ctrl Pts',(-2.107231161,4.429590053,6.937010627));
#142347=CARTESIAN_POINT('Ctrl Pts',(-2.1012084,4.428571429,6.938834431));
#142348=CARTESIAN_POINT('Ctrl Pts',(-1.728279509,4.365498301,7.05176425));
#142349=CARTESIAN_POINT('Ctrl Pts',(-1.345394953,4.301245526,7.124072741));
#142350=CARTESIAN_POINT('',(-1.94966066672091,4.43060908088842,7.2421559806126));
#142351=CARTESIAN_POINT('Origin',(0.00564046052463463,4.16161686280091,
-0.183011846437567));
#142352=CARTESIAN_POINT('',(-2.03145569497605,4.43060908179129,7.0886661802354));
#142353=CARTESIAN_POINT('Origin',(3.81747584932146E-13,4.52171036999889,
-1.76074432811646E-12));
#142354=CARTESIAN_POINT('',(-1.40181135465044,4.52063234085899,7.36783040844133));
#142355=CARTESIAN_POINT('Origin',(0.0613272168278398,4.69624338552546,-0.17289401675978));
#142356=CARTESIAN_POINT('Origin',(0.0306516469109547,4.5535636689927,-0.189451099243872));
#142357=CARTESIAN_POINT('Ctrl Pts',(-3.177002213,4.301266351,6.79386907));
#142358=CARTESIAN_POINT('Ctrl Pts',(-2.806920605,4.365380951,6.966929527));
#142359=CARTESIAN_POINT('Ctrl Pts',(-2.420230359,4.430609079,7.098766443));
#142360=CARTESIAN_POINT('Ctrl Pts',(-2.41635263961303,4.43126318491329,
7.10008850004794));
#142361=CARTESIAN_POINT('Ctrl Pts',(-2.41247492022606,4.43191729082659,
7.10141055709587));
#142362=CARTESIAN_POINT('Ctrl Pts',(-2.854069293,4.301266351,6.66459214600001));
#142363=CARTESIAN_POINT('Ctrl Pts',(-2.491029771,4.365380951,6.820061517));
#142364=CARTESIAN_POINT('Ctrl Pts',(-2.113250748,4.430609079,6.93517637));
#142365=CARTESIAN_POINT('Ctrl Pts',(-2.10946239011761,4.43126318491329,
6.93633073864991));
#142366=CARTESIAN_POINT('Ctrl Pts',(-2.10567403223522,4.43191729082659,
6.93748510729981));
#142367=CARTESIAN_POINT('',(-2.42023036541207,4.43060908007271,7.09876643752801));
#142368=CARTESIAN_POINT('',(-2.26674057192561,4.43060908208283,7.01697140054785));
#142369=CARTESIAN_POINT('',(-2.94690600724563,4.34096089499786,6.89679236925532));
#142370=CARTESIAN_POINT('Origin',(0.0415756784798843,4.55349067515581,-0.182852214336201));
#142371=CARTESIAN_POINT('Ctrl Pts',(-2.84976291363964,4.30202682662798,
6.66643467952211));
#142372=CARTESIAN_POINT('Ctrl Pts',(-2.86582299171485,4.30883437576907,
6.70481824956525));
#142373=CARTESIAN_POINT('Ctrl Pts',(-2.88196106599946,4.31547784262711,
6.74322686106965));
#142374=CARTESIAN_POINT('Ctrl Pts',(-2.91433991142714,4.32844538539627,
6.81999812150008));
#142375=CARTESIAN_POINT('Ctrl Pts',(-2.93059989259798,4.33477714729532,
6.85840629676247));
#142376=CARTESIAN_POINT('Ctrl Pts',(-2.94690600618894,4.34096089499144,
6.896792369698));
#142377=CARTESIAN_POINT('Ctrl Pts',(-3.46815410914429,4.43188407004788,
6.64996040604056));
#142378=CARTESIAN_POINT('Ctrl Pts',(-3.46454113007215,4.43124657452394,
6.65183969552028));
#142379=CARTESIAN_POINT('Ctrl Pts',(-3.460928151,4.430609079,6.65371898500001));
#142380=CARTESIAN_POINT('Ctrl Pts',(-3.455152864,4.429590053,6.656722998));
#142381=CARTESIAN_POINT('Ctrl Pts',(-3.44937237,4.428571429,6.65971698));
#142382=CARTESIAN_POINT('Ctrl Pts',(-3.091444697,4.365498301,6.845104111));
#142383=CARTESIAN_POINT('Ctrl Pts',(-2.715708914,4.301245526,6.99106037));
#142384=CARTESIAN_POINT('Ctrl Pts',(-3.56156421782437,4.43188407004788,
6.31488893800863));
#142385=CARTESIAN_POINT('Ctrl Pts',(-3.55813312741219,4.43124657452394,
6.31681914700431));
#142386=CARTESIAN_POINT('Ctrl Pts',(-3.554702037,4.430609079,6.318749356));
#142387=CARTESIAN_POINT('Ctrl Pts',(-3.549217496,4.429590053,6.321834763));
#142388=CARTESIAN_POINT('Ctrl Pts',(-3.543727607,4.428571429,6.324910643));
#142389=CARTESIAN_POINT('Ctrl Pts',(-3.20379416,4.365498301,6.515368914));
#142390=CARTESIAN_POINT('Ctrl Pts',(-2.84540542,4.301245526,6.668295734));
#142391=CARTESIAN_POINT('',(-3.46092814283634,4.43060908088845,6.6537189864983));
#142392=CARTESIAN_POINT('Origin',(0.0448507385774199,4.16161693133534,-0.17752059842843));
#142393=CARTESIAN_POINT('',(-3.50781507888034,4.43060908179129,6.48623417867685));
#142394=CARTESIAN_POINT('Origin',(1.97324795392362E-13,4.52171037000089,
-4.11129463806503E-13));
#142395=CARTESIAN_POINT('',(-2.95290353040656,4.52063234086375,6.89422662374213));
#142396=CARTESIAN_POINT('Origin',(0.0970604625450294,4.69624336322254,-0.155668159305726));
#142397=CARTESIAN_POINT('Origin',(0.0706614301360553,4.55356366994914,-0.178432672195805));
#142398=CARTESIAN_POINT('Ctrl Pts',(-4.563206691,4.301266351,5.95207062200001));
#142399=CARTESIAN_POINT('Ctrl Pts',(-4.238980268,4.365380951,6.200641628));
#142400=CARTESIAN_POINT('Ctrl Pts',(-3.889671666,4.430609079,6.412523242));
#142401=CARTESIAN_POINT('Ctrl Pts',(-3.8861688087337,4.43126318491329,6.4146479851267));
#142402=CARTESIAN_POINT('Ctrl Pts',(-3.88266595146739,4.43191729082659,
6.4167727282534));
#142403=CARTESIAN_POINT('Ctrl Pts',(-4.220033046,4.301266351,5.895237153));
#142404=CARTESIAN_POINT('Ctrl Pts',(-3.898902506,4.365380951,6.125114502));
#142405=CARTESIAN_POINT('Ctrl Pts',(-3.554702037,4.430609079,6.318749356));
#142406=CARTESIAN_POINT('Ctrl Pts',(-3.55125040395404,4.43126318491329,
6.32069112110816));
#142407=CARTESIAN_POINT('Ctrl Pts',(-3.54779877090807,4.43191729082659,
6.32263288621632));
#142408=CARTESIAN_POINT('',(-3.88967167115354,4.43060908007263,6.41252323525665));
#142409=CARTESIAN_POINT('',(-3.72218686821525,4.43060908208281,6.36563628922607));
#142410=CARTESIAN_POINT('',(-4.36061547382111,4.34096089500174,6.10205151464986));
#142411=CARTESIAN_POINT('Origin',(0.0799114620200347,4.55349070799973,-0.169639663486321));
#142412=CARTESIAN_POINT('Ctrl Pts',(-4.21622343834095,4.30202682667494,
5.89796235369777));
#142413=CARTESIAN_POINT('Ctrl Pts',(-4.24015925232632,4.30883434132914,
5.93199592261722));
#142414=CARTESIAN_POINT('Ctrl Pts',(-4.26417660738963,4.31547777332414,
5.96603716179003));
#142415=CARTESIAN_POINT('Ctrl Pts',(-4.31230226225936,4.32844538539751,
6.03405342154499));
#142416=CARTESIAN_POINT('Ctrl Pts',(-4.33643871635989,4.33477714726343,
6.06806821949402));
#142417=CARTESIAN_POINT('Ctrl Pts',(-4.36061547322445,4.34096089498421,
6.10205151507753));
#142418=CARTESIAN_POINT('Ctrl Pts',(-4.81661550888204,4.43188407004788,
5.74893741316841));
#142419=CARTESIAN_POINT('Ctrl Pts',(-4.81349099094102,4.43124657452394,
5.7515494490842));
#142420=CARTESIAN_POINT('Ctrl Pts',(-4.81036647300001,4.430609079,5.75416148500001));
#142421=CARTESIAN_POINT('Ctrl Pts',(-4.805371983,4.429590053,5.758336781));
#142422=CARTESIAN_POINT('Ctrl Pts',(-4.800370252,4.428571429,5.762503401));
#142423=CARTESIAN_POINT('Ctrl Pts',(-4.490663482,4.365498301,6.020500154));
#142424=CARTESIAN_POINT('Ctrl Pts',(-4.155088474,4.301245526,6.243816123));
#142425=CARTESIAN_POINT('Ctrl Pts',(-4.8358112798721,4.43188407004788,5.40161931776974));
#142426=CARTESIAN_POINT('Ctrl Pts',(-4.83287534443605,4.43124657452394,
5.40424198188487));
#142427=CARTESIAN_POINT('Ctrl Pts',(-4.829939409,4.430609079,5.406864646));
#142428=CARTESIAN_POINT('Ctrl Pts',(-4.825246365,4.429590053,5.411056931));
#142429=CARTESIAN_POINT('Ctrl Pts',(-4.82054605,4.428571429,5.415241063));
#142430=CARTESIAN_POINT('Ctrl Pts',(-4.529502956,4.365498301,5.674322168));
#142431=CARTESIAN_POINT('Ctrl Pts',(-4.212367892,4.301245526,5.90071663));
#142432=CARTESIAN_POINT('',(-4.81036646532986,4.43060908088843,5.75416148814806));
#142433=CARTESIAN_POINT('Origin',(0.0819638448501125,4.16161699509913,-0.163728679574764));
#142434=CARTESIAN_POINT('',(-4.82015292799161,4.43060908179129,5.58051307673596));
#142435=CARTESIAN_POINT('Origin',(-4.33680868994202E-14,4.52171037,1.34441069388203E-13));
#142436=CARTESIAN_POINT('',(-4.3659212187363,4.52063234082487,6.09825646507154));
#142437=CARTESIAN_POINT('Origin',(0.128255209085647,4.69624332240152,-0.131163488074278));
#142438=CARTESIAN_POINT('Origin',(0.107367251794376,4.55356365553789,-0.159071021084871));
#142439=CARTESIAN_POINT('Ctrl Pts',(-5.73604069600001,4.301266351,4.831959968));
#142440=CARTESIAN_POINT('Ctrl Pts',(-5.47282992599999,4.365380951,5.144418618));
#142441=CARTESIAN_POINT('Ctrl Pts',(-5.17723624800001,4.430609079,5.426437582));
#142442=CARTESIAN_POINT('Ctrl Pts',(-5.17427204254692,4.43126318491329,
5.42926566058618));
#142443=CARTESIAN_POINT('Ctrl Pts',(-5.17130783709384,4.43191729082659,
5.43209373917236));
#142444=CARTESIAN_POINT('Ctrl Pts',(-5.388672745,4.301266351,4.850227423));
#142445=CARTESIAN_POINT('Ctrl Pts',(-5.124466893,4.365380951,5.143763941));
#142446=CARTESIAN_POINT('Ctrl Pts',(-4.829939409,4.430609079,5.40686464600001));
#142447=CARTESIAN_POINT('Ctrl Pts',(-4.82698589531168,4.43126318491329,
5.40950301279372));
#142448=CARTESIAN_POINT('Ctrl Pts',(-4.82403238162336,4.43191729082659,
5.41214137958745));
#142449=CARTESIAN_POINT('',(-5.17723625158181,4.43060908007265,5.42643757430715));
#142450=CARTESIAN_POINT('',(-5.00358784272338,4.43060908208283,5.41665110086127));
#142451=CARTESIAN_POINT('',(-5.57042740767327,4.34096089499433,5.02198551318363));
#142452=CARTESIAN_POINT('Origin',(0.114510668632672,4.55349064898209,-0.148494951778445));
#142453=CARTESIAN_POINT('Ctrl Pts',(-5.38553804049223,4.30202682659519,
4.85370786275825));
#142454=CARTESIAN_POINT('Ctrl Pts',(-5.41623061531528,4.30883437574001,
4.88180039567836));
#142455=CARTESIAN_POINT('Ctrl Pts',(-5.44700449218597,4.31547784259929,
4.90988290582544));
#142456=CARTESIAN_POINT('Ctrl Pts',(-5.50862617915739,4.32844539111283,
4.96596311513484));
#142457=CARTESIAN_POINT('Ctrl Pts',(-5.53951054287518,4.33477715879874,
4.99399406931061));
#142458=CARTESIAN_POINT('Ctrl Pts',(-5.57042740683775,4.34096089498869,
5.02198551401675));
#142459=CARTESIAN_POINT('Ctrl Pts',(-5.93985732264998,4.43188407004788,
4.57910049458699));
#142460=CARTESIAN_POINT('Ctrl Pts',(-5.93736736432499,4.43124657452394,
4.58232314179349));
#142461=CARTESIAN_POINT('Ctrl Pts',(-5.934877406,4.430609079,4.585545789));
#142462=CARTESIAN_POINT('Ctrl Pts',(-5.930897249,4.429590053,4.590697137));
#142463=CARTESIAN_POINT('Ctrl Pts',(-5.926908156,4.428571429,4.595841568));
#142464=CARTESIAN_POINT('Ctrl Pts',(-5.679903833,4.365498301,4.9143843));
#142465=CARTESIAN_POINT('Ctrl Pts',(-5.400180715,4.301245526,5.204617973));
#142466=CARTESIAN_POINT('Ctrl Pts',(-5.88394118241646,4.43188407004788,
4.23577597926324));
#142467=CARTESIAN_POINT('Ctrl Pts',(-5.88163768270823,4.43124657452394,
4.23896846663162));
#142468=CARTESIAN_POINT('Ctrl Pts',(-5.879334183,4.430609079,4.242160954));
#142469=CARTESIAN_POINT('Ctrl Pts',(-5.875652077,4.429590053,4.247264092));
#142470=CARTESIAN_POINT('Ctrl Pts',(-5.871961118,4.428571429,4.25236083));
#142471=CARTESIAN_POINT('Ctrl Pts',(-5.643417229,4.365498301,4.567950425));
#142472=CARTESIAN_POINT('Ctrl Pts',(-5.382364723,4.301245526,4.857226574));
#142473=CARTESIAN_POINT('',(-5.93487739907786,4.43060908088836,4.58554579351896));
#142474=CARTESIAN_POINT('Origin',(0.115244392964607,4.16161693384168,-0.142280995222945));
#142475=CARTESIAN_POINT('',(-5.90710578421114,4.43060908179129,4.41385338526969));
#142476=CARTESIAN_POINT('Origin',(1.12366713156398E-12,4.52171036999933,
-1.00397121172158E-12));
#142477=CARTESIAN_POINT('',(-5.57479328396169,4.52063234083233,5.01713861086988));
#142478=CARTESIAN_POINT('Origin',(0.153452966462989,4.69624336495175,-0.100525882028337));
#142479=CARTESIAN_POINT('Origin',(0.139052551697806,4.55356366360523,-0.132271185767189));
#142480=CARTESIAN_POINT('Ctrl Pts',(-6.640663814,4.301266351,3.485912235));
#142481=CARTESIAN_POINT('Ctrl Pts',(-6.450776138,4.365380951,3.847648312));
#142482=CARTESIAN_POINT('Ctrl Pts',(-6.222719017,4.430609079,4.186617732));
#142483=CARTESIAN_POINT('Ctrl Pts',(-6.22043206632414,4.43126318491329,
4.19001690822728));
#142484=CARTESIAN_POINT('Ctrl Pts',(-6.21814511564828,4.43191729082659,
4.19341608445456));
#142485=CARTESIAN_POINT('Ctrl Pts',(-6.305344095,4.301266351,3.578426449));
#142486=CARTESIAN_POINT('Ctrl Pts',(-6.110416904,4.365380951,3.921896695));
#142487=CARTESIAN_POINT('Ctrl Pts',(-5.879334183,4.430609079,4.242160954));
#142488=CARTESIAN_POINT('Ctrl Pts',(-5.87701689168871,4.43126318491329,
4.24537255537584));
#142489=CARTESIAN_POINT('Ctrl Pts',(-5.87469960037743,4.43191729082659,
4.24858415675168));
#142490=CARTESIAN_POINT('',(-6.2227190188456,4.43060908007265,4.18661772371591));
#142491=CARTESIAN_POINT('',(-6.05102661106641,4.43060908208283,4.21438932711084));
#142492=CARTESIAN_POINT('',(-6.51977234665285,4.34096089500476,3.7070970509502));
#142493=CARTESIAN_POINT('Origin',(0.143755514817397,4.55349071186133,-0.120406833930994));
#142494=CARTESIAN_POINT('Ctrl Pts',(-6.30303086914785,4.30202682657719,
3.58249938692523));
#142495=CARTESIAN_POINT('Ctrl Pts',(-6.33904493287761,4.30883437572862,
3.6033371356933));
#142496=CARTESIAN_POINT('Ctrl Pts',(-6.375136243243,4.31547784259418,3.62414761850538));
#142497=CARTESIAN_POINT('Ctrl Pts',(-6.44737283600404,4.32844539096959,
3.66566986209409));
#142498=CARTESIAN_POINT('Ctrl Pts',(-6.48356096590171,4.33477715846729,
3.68640624225615));
#142499=CARTESIAN_POINT('Ctrl Pts',(-6.51977234599395,4.34096089499908,
3.70709705188124));
#142500=CARTESIAN_POINT('Ctrl Pts',(-6.78535800869693,4.43188407004788,
3.19514992667573));
#142501=CARTESIAN_POINT('Ctrl Pts',(-6.78361903784846,4.43124657452394,
3.19883249733787));
#142502=CARTESIAN_POINT('Ctrl Pts',(-6.78188006700001,4.430609079,3.202515068));
#142503=CARTESIAN_POINT('Ctrl Pts',(-6.779100351,4.429590053,3.208401596));
#142504=CARTESIAN_POINT('Ctrl Pts',(-6.776310422,4.428571429,3.21428329));
#142505=CARTESIAN_POINT('Ctrl Pts',(-6.603558194,4.365498301,3.578477299));
#142506=CARTESIAN_POINT('Ctrl Pts',(-6.392766507,4.301245526,3.922057672));
#142507=CARTESIAN_POINT('Ctrl Pts',(-6.65694453501887,4.43188407004788,
2.87187246525371));
#142508=CARTESIAN_POINT('Ctrl Pts',(-6.65538118000943,4.43124657452394,
2.87548549812686));
#142509=CARTESIAN_POINT('Ctrl Pts',(-6.653817825,4.430609079,2.879098531));
#142510=CARTESIAN_POINT('Ctrl Pts',(-6.651318828,4.429590053,2.884873904));
#142511=CARTESIAN_POINT('Ctrl Pts',(-6.64880981,4.428571429,2.890644931));
#142512=CARTESIAN_POINT('Ctrl Pts',(-6.49345158400001,4.365498301,3.247986396));
#142513=CARTESIAN_POINT('Ctrl Pts',(-6.300688161,4.301245526,3.586618002));
#142514=CARTESIAN_POINT('',(-6.78188006127967,4.43060908088839,3.20251507398212));
#142515=CARTESIAN_POINT('Origin',(0.143136257140021,4.16161698237671,-0.114180401131374));
#142516=CARTESIAN_POINT('',(-6.71784893891177,4.43060908179129,3.04080681515956));
#142517=CARTESIAN_POINT('Origin',(8.00574884163296E-13,4.52171036999978,
-5.12393946716649E-13));
#142518=CARTESIAN_POINT('',(-6.52299421048894,4.52063234083094,3.7014249322747));
#142519=CARTESIAN_POINT('Origin',(0.171475441869195,4.69624338813449,-0.0651878064923755));
#142520=CARTESIAN_POINT('Origin',(0.164236088590776,4.55356368309189,-0.0992866306841322));
#142521=CARTESIAN_POINT('Ctrl Pts',(-7.234776872,4.301266351,1.976867121));
#142522=CARTESIAN_POINT('Ctrl Pts',(-7.127091228,4.365380951,2.370966246));
#142523=CARTESIAN_POINT('Ctrl Pts',(-6.977234361,4.430609079,2.751036289));
#142524=CARTESIAN_POINT('Ctrl Pts',(-6.97573160036808,4.43126318491329,
2.75484762116933));
#142525=CARTESIAN_POINT('Ctrl Pts',(-6.97422883973616,4.43191729082659,
2.75865895333867));
#142526=CARTESIAN_POINT('Ctrl Pts',(-6.927184563,4.301266351,2.139302231));
#142527=CARTESIAN_POINT('Ctrl Pts',(-6.810650611,4.365380951,2.516645918));
#142528=CARTESIAN_POINT('Ctrl Pts',(-6.653817825,4.430609079,2.879098531));
#142529=CARTESIAN_POINT('Ctrl Pts',(-6.65224511003996,4.43126318491329,
2.88273319605511));
#142530=CARTESIAN_POINT('Ctrl Pts',(-6.65067239507992,4.43191729082659,
2.88636786111022));
#142531=CARTESIAN_POINT('',(-6.97723436100188,4.43060908007269,2.75103628054129));
#142532=CARTESIAN_POINT('',(-6.81552610039196,4.43060908208281,2.8150673921034));
#142533=CARTESIAN_POINT('',(-7.16425997738659,4.34096089501395,2.21886885033756));
#142534=CARTESIAN_POINT('Origin',(0.166278515907661,4.55349069049514,-0.0866886118381799));
#142535=CARTESIAN_POINT('Ctrl Pts',(-6.92580098057473,4.30202682665899,
2.14377722136203));
#142536=CARTESIAN_POINT('Ctrl Pts',(-6.96545255544565,4.308834375779,2.15638583604463));
#142537=CARTESIAN_POINT('Ctrl Pts',(-7.00517370965433,4.31547784262409,
2.16895121645212));
#142538=CARTESIAN_POINT('Ctrl Pts',(-7.08464747199278,4.32844538542488,
2.19397395014918));
#142539=CARTESIAN_POINT('Ctrl Pts',(-7.1244472145633,4.33477714731917,2.20644613531202));
#142540=CARTESIAN_POINT('Ctrl Pts',(-7.16425997706287,4.34096089501268,
2.21886885134477));
#142541=CARTESIAN_POINT('Ctrl Pts',(-7.31358289534331,4.43188407004788,
1.66179769895285));
#142542=CARTESIAN_POINT('Ctrl Pts',(-7.31267622467166,4.43124657452394,
1.66576800047642));
#142543=CARTESIAN_POINT('Ctrl Pts',(-7.311769554,4.430609079,1.669738302));
#142544=CARTESIAN_POINT('Ctrl Pts',(-7.310320256,4.429590053,1.676084763));
#142545=CARTESIAN_POINT('Ctrl Pts',(-7.308859943,4.428571429,1.682428699));
#142546=CARTESIAN_POINT('Ctrl Pts',(-7.218437514,4.365498301,2.075244676));
#142547=CARTESIAN_POINT('Ctrl Pts',(-7.086433643,4.301245526,2.456106313));
#142548=CARTESIAN_POINT('Ctrl Pts',(-7.11867655828793,4.43188407004788,
1.37368338701899));
#142549=CARTESIAN_POINT('Ctrl Pts',(-7.11792644914396,4.43124657452394,
1.3775480240095));
#142550=CARTESIAN_POINT('Ctrl Pts',(-7.11717634,4.430609079,1.381412661));
#142551=CARTESIAN_POINT('Ctrl Pts',(-7.115977303,4.429590053,1.387590219));
#142552=CARTESIAN_POINT('Ctrl Pts',(-7.114767544,4.428571429,1.393765687));
#142553=CARTESIAN_POINT('Ctrl Pts',(-7.03985936,4.365498301,1.776150134));
#142554=CARTESIAN_POINT('Ctrl Pts',(-6.92439842400001,4.301245526,2.148303159));
#142555=CARTESIAN_POINT('',(-7.3117695495973,4.43060908088835,1.66973830899428));
#142556=CARTESIAN_POINT('Origin',(0.164335220526527,4.16161696526441,-0.0807408649835453));
#142557=CARTESIAN_POINT('',(-7.21447294344383,4.43060908179129,1.52557549831721));
#142558=CARTESIAN_POINT('Origin',(9.12898229232795E-13,4.52171037000067,
-3.59304599961696E-13));
#142559=CARTESIAN_POINT('',(-7.16618717794668,4.52063234083,2.21263673771566));
#142560=CARTESIAN_POINT('Origin',(0.181479818420224,4.69624337504075,-0.0268015869758415));
#142561=CARTESIAN_POINT('Origin',(0.181740147018993,4.55356363980172,-0.0616594868090475));
#142562=CARTESIAN_POINT('Ctrl Pts',(-7.490599804,4.301266351,0.375385897));
#142563=CARTESIAN_POINT('Ctrl Pts',(-7.470151454,4.365380951,0.783420434));
#142564=CARTESIAN_POINT('Ctrl Pts',(-7.405501982,4.430609079,1.186819448));
#142565=CARTESIAN_POINT('Ctrl Pts',(-7.40485367883351,4.43126318491329,
1.1908647224631));
#142566=CARTESIAN_POINT('Ctrl Pts',(-7.40420537566703,4.43191729082659,
1.19490999692619));
#142567=CARTESIAN_POINT('Ctrl Pts',(-7.225117579,4.301266351,0.600146619));
#142568=CARTESIAN_POINT('Ctrl Pts',(-7.192425865,4.365380951,0.993719575));
#142569=CARTESIAN_POINT('Ctrl Pts',(-7.11717634000001,4.430609079,1.381412661));
#142570=CARTESIAN_POINT('Ctrl Pts',(-7.11642173978711,4.43126318491329,
1.38530043683952));
#142571=CARTESIAN_POINT('Ctrl Pts',(-7.11566713957423,4.43191729082659,
1.38918821267904));
#142572=CARTESIAN_POINT('',(-7.40550198018438,4.43060908007269,1.18681943973392));
#142573=CARTESIAN_POINT('',(-7.26133916437191,4.43060908208281,1.28411603543277));
#142574=CARTESIAN_POINT('',(-7.47375477405679,4.34096089500807,0.62688880836363));
#142575=CARTESIAN_POINT('Origin',(0.181026394718455,4.55349067138657,-0.0489168858748047));
#142576=CARTESIAN_POINT('Ctrl Pts',(-7.22472833593329,4.30202682669847,
0.604814415005951));
#142577=CARTESIAN_POINT('Ctrl Pts',(-7.26616317342456,4.30883434543173,
0.608604313929139));
#142578=CARTESIAN_POINT('Ctrl Pts',(-7.30765664832846,4.31547778156078,
0.612337031069097));
#142579=CARTESIAN_POINT('Ctrl Pts',(-7.39065189691945,4.32844538539013,
0.619690272258531));
#142580=CARTESIAN_POINT('Ctrl Pts',(-7.43220229482626,4.33477714728864,
0.623315096574982));
#142581=CARTESIAN_POINT('Ctrl Pts',(-7.47375477396737,4.34096089499539,
0.62688880942525));
#142582=CARTESIAN_POINT('Ctrl Pts',(-7.49983277261798,4.43188407004788,
0.050741656424082));
#142583=CARTESIAN_POINT('Ctrl Pts',(-7.49980079730899,4.43124657452394,
0.0548140422120409));
#142584=CARTESIAN_POINT('Ctrl Pts',(-7.49976882200001,4.430609079,0.058886428));
#142585=CARTESIAN_POINT('Ctrl Pts',(-7.49971771,4.429590053,0.065396069));
#142586=CARTESIAN_POINT('Ctrl Pts',(-7.499655298,4.428571429,0.071905611));
#142587=CARTESIAN_POINT('Ctrl Pts',(-7.495790718,4.365498301,0.474975919));
#142588=CARTESIAN_POINT('Ctrl Pts',(-7.44874701800001,4.301245526,0.875310152000001));
#142589=CARTESIAN_POINT('Ctrl Pts',(-7.24754717756366,4.43188407004788,
-0.1887376018885));
#142590=CARTESIAN_POINT('Ctrl Pts',(-7.24764538878184,4.43124657452394,
-0.18480206644425));
#142591=CARTESIAN_POINT('Ctrl Pts',(-7.2477436,4.430609079,-0.180866531));
#142592=CARTESIAN_POINT('Ctrl Pts',(-7.247900589,4.429590053,-0.174575643));
#142593=CARTESIAN_POINT('Ctrl Pts',(-7.248046656,4.428571429,-0.168284491));
#142594=CARTESIAN_POINT('Ctrl Pts',(-7.257091136,4.365498301,0.221263065));
#142595=CARTESIAN_POINT('Ctrl Pts',(-7.224331513,4.301245526,0.609536047));
#142596=CARTESIAN_POINT('',(-7.49976881958266,4.43060908088848,0.0588864359526545));
#142597=CARTESIAN_POINT('Origin',(0.177850049580502,4.1616169083973,-0.0435259824795542));
#142598=CARTESIAN_POINT('',(-7.37375621114217,4.43060908179128,-0.0609900343115401));
#142599=CARTESIAN_POINT('Origin',(6.74807432154978E-13,4.52171036999867,
-9.36242457259123E-14));
#142600=CARTESIAN_POINT('',(-7.47429719740143,4.52063234084568,0.620388107456563));
#142601=CARTESIAN_POINT('Origin',(0.182998526927772,4.69624334770116,0.0128378233019234));
#142602=CARTESIAN_POINT('Origin',(0.190745673159929,4.55356367069499,-0.0211491355950279));
#142603=CARTESIAN_POINT('Ctrl Pts',(-7.396170615,4.301266351,-1.243647954));
#142604=CARTESIAN_POINT('Ctrl Pts',(-7.4639157,4.365380951,-0.840757247));
#142605=CARTESIAN_POINT('Ctrl Pts',(-7.48749656,4.430609079,-0.432891753));
#142606=CARTESIAN_POINT('Ctrl Pts',(-7.48773302822988,4.43126318491329,
-0.428801688795589));
#142607=CARTESIAN_POINT('Ctrl Pts',(-7.48796949645976,4.43191729082659,
-0.424711624591177));
#142608=CARTESIAN_POINT('Ctrl Pts',(-7.185212128,4.301266351,-0.967071182));
#142609=CARTESIAN_POINT('Ctrl Pts',(-7.23789128,4.365380951,-0.575671991));
#142610=CARTESIAN_POINT('Ctrl Pts',(-7.2477436,4.430609079,-0.180866531));
#142611=CARTESIAN_POINT('Ctrl Pts',(-7.24784239879999,4.43126318491329,
-0.176907432465295));
#142612=CARTESIAN_POINT('Ctrl Pts',(-7.24794119759997,4.43191729082659,
-0.172948333930589));
#142613=CARTESIAN_POINT('',(-7.48749655645112,4.43060908007267,-0.43289176068817));
#142614=CARTESIAN_POINT('',(-7.36762007919418,4.43060908208281,-0.306879161346311));
#142615=CARTESIAN_POINT('',(-7.4337851039095,4.34096089504206,-0.994403857097817));
#142616=CARTESIAN_POINT('Origin',(0.187309731765656,4.55349068566599,-0.0088579242423243));
#142617=CARTESIAN_POINT('Ctrl Pts',(-7.18583542313158,4.30202682672418,
-0.962428840202224));
#142618=CARTESIAN_POINT('Ctrl Pts',(-7.22711623438974,4.30883434230733,
-0.967634809921265));
#142619=CARTESIAN_POINT('Ctrl Pts',(-7.26844201754806,4.31547777524972,
-0.972909229457909));
#142620=CARTESIAN_POINT('Ctrl Pts',(-7.3510776533894,4.32844538542671,-0.983569433400221));
#142621=CARTESIAN_POINT('Ctrl Pts',(-7.39243585617379,4.33477714732437,
-0.988961462826314));
#142622=CARTESIAN_POINT('Ctrl Pts',(-7.43378510403677,4.34096089502777,
-0.994403856147091));
#142623=CARTESIAN_POINT('Ctrl Pts',(-7.33539880555815,4.43188407004788,
-1.56268700811032));
#142624=CARTESIAN_POINT('Ctrl Pts',(-7.33624302077908,4.43124657452394,
-1.55870295855516));
#142625=CARTESIAN_POINT('Ctrl Pts',(-7.33708723600001,4.430609079,-1.554718909));
#142626=CARTESIAN_POINT('Ctrl Pts',(-7.3384367,4.429590053,-1.548350472));
#142627=CARTESIAN_POINT('Ctrl Pts',(-7.339775105,4.428571429,-1.541979703));
#142628=CARTESIAN_POINT('Ctrl Pts',(-7.422649079,4.365498301,-1.147502184));
#142629=CARTESIAN_POINT('Ctrl Pts',(-7.462765261,4.301245526,-0.746414538));
#142630=CARTESIAN_POINT('Ctrl Pts',(-7.03753054804688,4.43188407004788,
-1.74233342918306));
#142631=CARTESIAN_POINT('Ctrl Pts',(-7.03847248652344,4.43124657452394,
-1.73851101659153));
#142632=CARTESIAN_POINT('Ctrl Pts',(-7.039414425,4.430609079,-1.734688604));
#142633=CARTESIAN_POINT('Ctrl Pts',(-7.040920098,4.429590053,-1.728578541));
#142634=CARTESIAN_POINT('Ctrl Pts',(-7.042415162,4.428571429,-1.722465874));
#142635=CARTESIAN_POINT('Ctrl Pts',(-7.134989397,4.365498301,-1.343970018));
#142636=CARTESIAN_POINT('Ctrl Pts',(-7.186462889,4.301245526,-0.957732292));
#142637=CARTESIAN_POINT('',(-7.3370872353543,4.43060908088849,-1.5547189007123));
#142638=CARTESIAN_POINT('Origin',(0.183048813547394,4.16161690417072,-0.0042758664672185));
#142639=CARTESIAN_POINT('',(-7.18825083433387,4.43060908179129,-1.64470373974391));
#142640=CARTESIAN_POINT('Origin',(-1.4658413372004E-13,4.52171037000022,
-7.2478915230656E-14));
#142641=CARTESIAN_POINT('',(-7.43291738723039,4.52063234080555,-1.00086918069252));
#142642=CARTESIAN_POINT('Origin',(0.175960374723824,4.69624334626897,0.0518769504692056));
#142643=CARTESIAN_POINT('Origin',(0.190832825460228,4.55356370548195,0.0203500376732782));
#142644=CARTESIAN_POINT('Ctrl Pts',(-6.955904708,4.301266351,-2.804530209));
#142645=CARTESIAN_POINT('Ctrl Pts',(-7.10867554300001,4.365380951,-2.425622053));
#142646=CARTESIAN_POINT('Ctrl Pts',(-7.21938412,4.430609079,-2.032361415));
#142647=CARTESIAN_POINT('Ctrl Pts',(-7.22049430263268,4.43126318491329,
-2.02841780789876));
#142648=CARTESIAN_POINT('Ctrl Pts',(-7.22160448526537,4.43191729082659,
-2.02447420079753));
#142649=CARTESIAN_POINT('Ctrl Pts',(-6.809334144,4.301266351,-2.489069809));
#142650=CARTESIAN_POINT('Ctrl Pts',(-6.944920943,4.365380951,-2.118145774));
#142651=CARTESIAN_POINT('Ctrl Pts',(-7.039414425,4.430609079,-1.734688604));
#142652=CARTESIAN_POINT('Ctrl Pts',(-7.04036200309613,4.43126318491329,
-1.73084330581221));
#142653=CARTESIAN_POINT('Ctrl Pts',(-7.04130958119224,4.43191729082659,
-1.72699800762441));
#142654=CARTESIAN_POINT('',(-7.21938411488067,4.43060908007265,-2.03236142178627));
#142655=CARTESIAN_POINT('',(-7.12939926755412,4.43060908208283,-1.88352502822083));
#142656=CARTESIAN_POINT('',(-7.0462199040165,4.34096089499886,-2.56919930375094));
#142657=CARTESIAN_POINT('Origin',(0.184834718843788,4.55349068833185,0.0316152152728183));
#142658=CARTESIAN_POINT('Ctrl Pts',(-6.81094083279843,4.30202682665829,
-2.48466999264095));
#142659=CARTESIAN_POINT('Ctrl Pts',(-6.85013758511489,4.30883437579503,
-2.49862847264263));
#142660=CARTESIAN_POINT('Ctrl Pts',(-6.88936356481079,4.31547784265374,
-2.51266347876292));
#142661=CARTESIAN_POINT('Ctrl Pts',(-6.96777522301014,4.32844539106519,
-2.54083853787839));
#142662=CARTESIAN_POINT('Ctrl Pts',(-7.00700740500025,4.33477715869623,
-2.55499530959718));
#142663=CARTESIAN_POINT('Ctrl Pts',(-7.04621990433313,4.34096089499308,
-2.56919930263159));
#142664=CARTESIAN_POINT('Ctrl Pts',(-6.82796974558505,4.43188407004788,
-3.10304616523142));
#142665=CARTESIAN_POINT('Ctrl Pts',(-6.82965067579253,4.43124657452394,
-3.09933674161571));
#142666=CARTESIAN_POINT('Ctrl Pts',(-6.831331606,4.430609079,-3.095627318));
#142667=CARTESIAN_POINT('Ctrl Pts',(-6.834018545,4.429590053,-3.089697866));
#142668=CARTESIAN_POINT('Ctrl Pts',(-6.836695187,4.428571429,-3.08376376));
#142669=CARTESIAN_POINT('Ctrl Pts',(-7.002432618,4.365498301,-2.716324361));
#142670=CARTESIAN_POINT('Ctrl Pts',(-7.127832894,4.301245526,-2.333237714));
#142671=CARTESIAN_POINT('Ctrl Pts',(-6.49844681077687,4.43188407004788,
-3.21445968164217));
#142672=CARTESIAN_POINT('Ctrl Pts',(-6.50018843288844,4.43124657452394,
-3.21092912382109));
#142673=CARTESIAN_POINT('Ctrl Pts',(-6.501930055,4.430609079,-3.207398566));
#142674=CARTESIAN_POINT('Ctrl Pts',(-6.504714009,4.429590053,-3.201755028));
#142675=CARTESIAN_POINT('Ctrl Pts',(-6.507488162,4.428571429,-3.196106666));
#142676=CARTESIAN_POINT('Ctrl Pts',(-6.679263483,4.365498301,-2.846360558));
#142677=CARTESIAN_POINT('Ctrl Pts',(-6.81256324800001,4.301245526,-2.480218134));
#142678=CARTESIAN_POINT('',(-6.83133160688307,4.4306090808884,-3.09562730976748));
#142679=CARTESIAN_POINT('Origin',(0.179688418953942,4.16161694203418,0.0351741913904707));
#142680=CARTESIAN_POINT('',(-6.6666308378463,4.43060908179129,-3.15151292645983));
#142681=CARTESIAN_POINT('Origin',(3.08347097854877E-13,4.52171036999956,
1.82579645846559E-13));
#142682=CARTESIAN_POINT('',(-7.0439826208049,4.52063234083322,-2.57532693793605));
#142683=CARTESIAN_POINT('Origin',(0.160694476196667,4.69624331874441,0.0884903518980124));
#142684=CARTESIAN_POINT('Origin',(0.181996628585891,4.55356368147533,0.0608976860971794));
#142685=CARTESIAN_POINT('Ctrl Pts',(-6.19038842800001,4.301266351,-4.234275748));
#142686=CARTESIAN_POINT('Ctrl Pts',(-6.421041618,4.365380951,-3.897067468));
#142687=CARTESIAN_POINT('Ctrl Pts',(-6.61370130300001,4.430609079,-3.536800117));
#142688=CARTESIAN_POINT('Ctrl Pts',(-6.61563328913966,4.43126318491329,
-3.53318736569346));
#142689=CARTESIAN_POINT('Ctrl Pts',(-6.61756527527932,4.43191729082659,
-3.52957461438691));
#142690=CARTESIAN_POINT('Ctrl Pts',(-6.115059263,4.301266351,-3.894682299));
#142691=CARTESIAN_POINT('Ctrl Pts',(-6.327213821,4.365380951,-3.561577415));
#142692=CARTESIAN_POINT('Ctrl Pts',(-6.501930055,4.430609079,-3.207398566));
#142693=CARTESIAN_POINT('Ctrl Pts',(-6.50368210469561,4.43126318491329,
-3.20384687002776));
#142694=CARTESIAN_POINT('Ctrl Pts',(-6.50543415439122,4.43191729082659,
-3.20029517405553));
#142695=CARTESIAN_POINT('',(-6.61370129655518,4.4306090800727,-3.53680012247357));
#142696=CARTESIAN_POINT('',(-6.55781567014535,4.43060908208281,-3.37209935871988));
#142697=CARTESIAN_POINT('',(-6.32918129308567,4.34096089502838,-4.02386184619341));
#142698=CARTESIAN_POINT('Origin',(0.173717228485566,4.55349068084526,0.0706101777306029));
#142699=CARTESIAN_POINT('Ctrl Pts',(-6.11757421903206,4.30202682671395,
-3.89073073857304));
#142700=CARTESIAN_POINT('Ctrl Pts',(-6.15285373557848,4.30883434169922,
-3.91278890945845));
#142701=CARTESIAN_POINT('Ctrl Pts',(-6.1881453258119,4.31547777403924,-3.93492808668518));
#142702=CARTESIAN_POINT('Ctrl Pts',(-6.25866730050807,4.32844538540129,
-3.97930083251753));
#142703=CARTESIAN_POINT('Ctrl Pts',(-6.29393893432853,4.3347771473131,-4.00156036445915));
#142704=CARTESIAN_POINT('Ctrl Pts',(-6.32918129360728,4.34096089502917,
-4.0238618453689));
#142705=CARTESIAN_POINT('Ctrl Pts',(-6.00127240686538,4.43188407004787,
-4.49831033178264));
#142706=CARTESIAN_POINT('Ctrl Pts',(-6.00371145443269,4.43124657452394,
-4.49504898289132));
#142707=CARTESIAN_POINT('Ctrl Pts',(-6.006150502,4.430609079,-4.491787634));
#142708=CARTESIAN_POINT('Ctrl Pts',(-6.010049279,4.429590053,-4.486574422));
#142709=CARTESIAN_POINT('Ctrl Pts',(-6.013939,4.428571429,-4.48135445));
#142710=CARTESIAN_POINT('Ctrl Pts',(-6.254790191,4.365498301,-4.158134229));
#142711=CARTESIAN_POINT('Ctrl Pts',(-6.459610984,4.301245526,-3.810961288));
#142712=CARTESIAN_POINT('Ctrl Pts',(-5.6555029236423,4.43188407004787,-4.53628137163683));
#142713=CARTESIAN_POINT('Ctrl Pts',(-5.65796279282115,4.43124657452394,
-4.53320775381842));
#142714=CARTESIAN_POINT('Ctrl Pts',(-5.660422662,4.430609079,-4.530134136));
#142715=CARTESIAN_POINT('Ctrl Pts',(-5.664354722,4.429590053,-4.525221009));
#142716=CARTESIAN_POINT('Ctrl Pts',(-5.668278248,4.428571429,-4.520301063));
#142717=CARTESIAN_POINT('Ctrl Pts',(-5.911222633,4.365498301,-4.215658441));
#142718=CARTESIAN_POINT('Ctrl Pts',(-6.120115721,4.301245526,-3.886731733));
#142719=CARTESIAN_POINT('',(-6.00615050467743,4.43060908088841,-4.49178762615972));
#142720=CARTESIAN_POINT('Origin',(0.16792599438362,4.16161688467452,0.0729795274135941));
#142721=CARTESIAN_POINT('',(-5.83328659251519,4.43060908179128,-4.51096087140242));
#142722=CARTESIAN_POINT('Origin',(-3.89445420356793E-13,4.52171037000067,
-2.85795692667179E-13));
#142723=CARTESIAN_POINT('',(-6.3256790556746,4.52063234084172,-4.02936527022594));
#142724=CARTESIAN_POINT('Origin',(0.137914834917369,4.69624337037489,0.120966140177844));
#142725=CARTESIAN_POINT('Origin',(0.164650191390726,4.55356366224679,0.0985976551418527));
#142726=CARTESIAN_POINT('Ctrl Pts',(-5.135416465,4.301266351,-5.46603126));
#142727=CARTESIAN_POINT('Ctrl Pts',(-5.433166924,4.365380951,-5.18629034));
#142728=CARTESIAN_POINT('Ctrl Pts',(-5.698769164,4.430609079,-4.87586197700001));
#142729=CARTESIAN_POINT('Ctrl Pts',(-5.70143261611943,4.43126318491329,
-4.87274900972471));
#142730=CARTESIAN_POINT('Ctrl Pts',(-5.70409606823886,4.43191729082659,
-4.86963604244942));
#142731=CARTESIAN_POINT('Ctrl Pts',(-5.134851007,4.301266351,-5.118183773));
#142732=CARTESIAN_POINT('Ctrl Pts',(-5.413653213,4.365380951,-4.838473655));
#142733=CARTESIAN_POINT('Ctrl Pts',(-5.660422662,4.430609079,-4.530134136));
#142734=CARTESIAN_POINT('Ctrl Pts',(-5.66289725939779,4.43126318491329,
-4.52704211559617));
#142735=CARTESIAN_POINT('Ctrl Pts',(-5.66537185679557,4.43191729082659,
-4.52395009519234));
#142736=CARTESIAN_POINT('',(-5.69876915651853,4.43060908007267,-4.87586198098007));
#142737=CARTESIAN_POINT('',(-5.67959590065063,4.43060908208281,-4.70299807141377));
#142738=CARTESIAN_POINT('',(-5.31619719916678,4.34096089504047,-5.29037308150137));
#142739=CARTESIAN_POINT('Origin',(0.15447676254813,4.55349068328005,0.106303469704071));
#142740=CARTESIAN_POINT('Ctrl Pts',(-5.13815663368765,4.30202682676978,
-5.11486523948491));
#142741=CARTESIAN_POINT('Ctrl Pts',(-5.16786948420241,4.30883434269612,
-5.1439917597904));
#142742=CARTESIAN_POINT('Ctrl Pts',(-5.197576712673,4.31547777600314,-5.17319998864913));
#142743=CARTESIAN_POINT('Ctrl Pts',(-5.25691108520785,4.32844538540515,
-5.23169545552141));
#142744=CARTESIAN_POINT('Ctrl Pts',(-5.28657294641733,4.33477714730095,
-5.2610169306122));
#142745=CARTESIAN_POINT('Ctrl Pts',(-5.31619719980772,4.34096089502036,
-5.29037308085881));
#142746=CARTESIAN_POINT('Ctrl Pts',(-4.89396224110399,4.43188407004788,
-5.68323850498272));
#142747=CARTESIAN_POINT('Ctrl Pts',(-4.897045358552,4.43124657452394,-5.68057772849136));
#142748=CARTESIAN_POINT('Ctrl Pts',(-4.900128476,4.430609079,-5.677916952));
#142749=CARTESIAN_POINT('Ctrl Pts',(-4.905056788,4.429590053,-5.673663745));
#142750=CARTESIAN_POINT('Ctrl Pts',(-4.909977709,4.428571429,-5.669401988));
#142751=CARTESIAN_POINT('Ctrl Pts',(-5.214680727,4.365498301,-5.405514363));
#142752=CARTESIAN_POINT('Ctrl Pts',(-5.489344843,4.301245526,-5.110488548));
#142753=CARTESIAN_POINT('Ctrl Pts',(-4.5481140040602,4.43188407004788,-5.64599158717323));
#142754=CARTESIAN_POINT('Ctrl Pts',(-4.5511771000301,4.43124657452394,-5.64351862808662));
#142755=CARTESIAN_POINT('Ctrl Pts',(-4.554240196,4.430609079,-5.64104566900001));
#142756=CARTESIAN_POINT('Ctrl Pts',(-4.559136504,4.429590053,-5.637092685));
#142757=CARTESIAN_POINT('Ctrl Pts',(-4.564025943,4.428571429,-5.633131207));
#142758=CARTESIAN_POINT('Ctrl Pts',(-4.866779581,4.365498301,-5.387836821));
#142759=CARTESIAN_POINT('Ctrl Pts',(-5.141498385,4.301245526,-5.111506076));
#142760=CARTESIAN_POINT('',(-4.90012848048857,4.43060908088848,-5.67791694500558));
#142761=CARTESIAN_POINT('Origin',(0.148311530019222,4.1616169810395,0.107372446471978));
#142762=CARTESIAN_POINT('',(-4.72718434919243,4.43060908179128,-5.65948129948078));
#142763=CARTESIAN_POINT('Origin',(9.66240976119082E-13,4.52171037000022,
9.49327422228308E-13));
#142764=CARTESIAN_POINT('',(-5.31159376899682,4.52063234084897,-5.2949949607014));
#142765=CARTESIAN_POINT('Origin',(0.10868640088724,4.69624337596615,0.147785719463314));
#142766=CARTESIAN_POINT('Origin',(0.139605180238045,4.55356367210724,0.131687433562332));
#142767=CARTESIAN_POINT('Ctrl Pts',(-3.840318136,4.301266351,-6.44220122400001));
#142768=CARTESIAN_POINT('Ctrl Pts',(-4.191243384,4.365380951,-6.233008039));
#142769=CARTESIAN_POINT('Ctrl Pts',(-4.517368912,4.430609079,-5.98693394900001));
#142770=CARTESIAN_POINT('Ctrl Pts',(-4.52063929002373,4.43126318491329,
-5.98446632464357));
#142771=CARTESIAN_POINT('Ctrl Pts',(-4.52390966804747,4.43191729082659,
-5.98199870028714));
#142772=CARTESIAN_POINT('Ctrl Pts',(-3.914542826,4.301266351,-6.102364662));
#142773=CARTESIAN_POINT('Ctrl Pts',(-4.246956198,4.365380951,-5.889128244));
#142774=CARTESIAN_POINT('Ctrl Pts',(-4.554240196,4.430609079,-5.641045669));
#142775=CARTESIAN_POINT('Ctrl Pts',(-4.55732163166763,4.43126318491329,
-5.63855790361001));
#142776=CARTESIAN_POINT('Ctrl Pts',(-4.56040306733527,4.43191729082659,
-5.63607013822001));
#142777=CARTESIAN_POINT('',(-4.51736890386037,4.43060908007272,-5.98693395125152));
#142778=CARTESIAN_POINT('',(-4.53580453873334,4.43060908208281,-5.81398982091035));
#142779=CARTESIAN_POINT('',(-4.05463363269045,4.34096089497448,-6.30951235068825));
#142780=CARTESIAN_POINT('Origin',(0.128012933467711,4.55349069865086,0.137025874071772));
#142781=CARTESIAN_POINT('Ctrl Pts',(-3.91848455494606,4.30202682656254,
-6.09983432463177));
#142782=CARTESIAN_POINT('Ctrl Pts',(-3.94124150545646,4.30883437570018,
-6.13466743762631));
#142783=CARTESIAN_POINT('Ctrl Pts',(-3.96397541205488,4.31547784255736,
-6.16957916015969));
#142784=CARTESIAN_POINT('Ctrl Pts',(-4.00934755056748,4.32844538537555,
-6.23946181292879));
#142785=CARTESIAN_POINT('Ctrl Pts',(-4.03201268352545,4.33477714727357,
-6.27447419159833));
#142786=CARTESIAN_POINT('Ctrl Pts',(-4.05463363371516,4.34096089497142,
-6.3095123500129));
#142787=CARTESIAN_POINT('Ctrl Pts',(-3.55781583914299,4.43188407004788,
-6.6024247660727));
#142788=CARTESIAN_POINT('Ctrl Pts',(-3.5613988635715,4.43124657452394,-6.60048897553635));
#142789=CARTESIAN_POINT('Ctrl Pts',(-3.564981888,4.430609079,-6.598553185));
#142790=CARTESIAN_POINT('Ctrl Pts',(-3.570709293,4.429590053,-6.595458856));
#142791=CARTESIAN_POINT('Ctrl Pts',(-3.576431317,4.428571429,-6.592354589));
#142792=CARTESIAN_POINT('Ctrl Pts',(-3.930738587,4.365498301,-6.400138652));
#142793=CARTESIAN_POINT('Ctrl Pts',(-4.262403038,4.301245526,-6.171055043));
#142794=CARTESIAN_POINT('Ctrl Pts',(-3.22806032850427,4.43188407004788,
-6.49170151124601));
#142795=CARTESIAN_POINT('Ctrl Pts',(-3.23158342425213,4.43124657452394,
-6.48994484362301));
#142796=CARTESIAN_POINT('Ctrl Pts',(-3.23510652,4.430609079,-6.488188176));
#142797=CARTESIAN_POINT('Ctrl Pts',(-3.24073813,4.429590053,-6.485380172));
#142798=CARTESIAN_POINT('Ctrl Pts',(-3.246364857,4.428571429,-6.482562396));
#142799=CARTESIAN_POINT('Ctrl Pts',(-3.594771326,4.365498301,-6.308085939));
#142800=CARTESIAN_POINT('Ctrl Pts',(-3.922470298,4.301245526,-6.09727207499999));
#142801=CARTESIAN_POINT('',(-3.56498189383822,4.43060908088846,-6.59855317909686));
#142802=CARTESIAN_POINT('Origin',(0.121762194606682,4.16161690396173,0.136744722697717));
#142803=CARTESIAN_POINT('',(-3.40004421925281,4.43060908179128,-6.54337067257439));
#142804=CARTESIAN_POINT('Origin',(-1.6154612370034E-13,4.52171037000156,
-3.25260651745651E-13));
#142805=CARTESIAN_POINT('',(-4.04914426134536,4.52063234081332,-6.31303657114383));
#142806=CARTESIAN_POINT('Origin',(0.0743757746014689,4.69624335400154,0.167694862273235));
#142807=CARTESIAN_POINT('Origin',(0.108032464906547,4.55356370820857,0.158619752400417));
#142808=CARTESIAN_POINT('Ctrl Pts',(-2.365650799,4.301266351,-7.11714102000001));
#142809=CARTESIAN_POINT('Ctrl Pts',(-2.75334196,4.365380951,-6.98827721));
#142810=CARTESIAN_POINT('Ctrl Pts',(-3.124741511,4.430609079,-6.818063544));
#142811=CARTESIAN_POINT('Ctrl Pts',(-3.12846589570875,4.43126318491329,
-6.8163566459352));
#142812=CARTESIAN_POINT('Ctrl Pts',(-3.1321902804175,4.43191729082659,-6.81464974787039));
#142813=CARTESIAN_POINT('Ctrl Pts',(-2.511194972,4.301266351,-6.801205762));
#142814=CARTESIAN_POINT('Ctrl Pts',(-2.881676231,4.365380951,-6.66441374200001));
#142815=CARTESIAN_POINT('Ctrl Pts',(-3.23510652,4.430609079,-6.488188176));
#142816=CARTESIAN_POINT('Ctrl Pts',(-3.23865070943269,4.43126318491329,
-6.48642099076369));
#142817=CARTESIAN_POINT('Ctrl Pts',(-3.24219489886538,4.43191729082659,
-6.48465380552737));
#142818=CARTESIAN_POINT('',(-3.12474150257614,4.43060908007272,-6.81806354444139));
#142819=CARTESIAN_POINT('',(-3.17992399802989,4.43060908208281,-6.65312586835001));
#142820=CARTESIAN_POINT('',(-2.60347990415908,4.34096089503555,-7.03362583523939));
#142821=CARTESIAN_POINT('Origin',(0.0955636390403675,4.55349066841947,0.161341518445375));
#142822=CARTESIAN_POINT('Ctrl Pts',(-2.51558849342807,4.30202682662507,
-6.79958193799661));
#142823=CARTESIAN_POINT('Ctrl Pts',(-2.53032530952334,4.30883437575032,
-6.83849274378294));
#142824=CARTESIAN_POINT('Ctrl Pts',(-2.54502272159871,4.31547784256747,
-6.87747536732137));
#142825=CARTESIAN_POINT('Ctrl Pts',(-2.57431138013896,4.32844538540733,
-6.95547787121539));
#142826=CARTESIAN_POINT('Ctrl Pts',(-2.58891998835045,4.33477714728761,
-6.99454401342095));
#142827=CARTESIAN_POINT('Ctrl Pts',(-2.60347990497689,4.34096089501081,
-7.03362583493863));
#142828=CARTESIAN_POINT('Ctrl Pts',(-2.05530992479785,4.43188407004787,
-7.21288898031392));
#142829=CARTESIAN_POINT('Ctrl Pts',(-2.05922531739893,4.43124657452394,
-7.21176869215696));
#142830=CARTESIAN_POINT('Ctrl Pts',(-2.06314071,4.430609079,-7.210648404));
#142831=CARTESIAN_POINT('Ctrl Pts',(-2.0693994,4.429590053,-7.208857642));
#142832=CARTESIAN_POINT('Ctrl Pts',(-2.075654973,4.428571429,-7.207056017));
#142833=CARTESIAN_POINT('Ctrl Pts',(-2.46299948,4.365498301,-7.095499572));
#142834=CARTESIAN_POINT('Ctrl Pts',(-2.836156005,4.301245526,-6.943069863));
#142835=CARTESIAN_POINT('Ctrl Pts',(-1.75706614025099,4.43188407004787,
-7.03386668559917));
#142836=CARTESIAN_POINT('Ctrl Pts',(-1.7608844996255,4.43124657452394,-7.03290844979958));
#142837=CARTESIAN_POINT('Ctrl Pts',(-1.764702859,4.430609079,-7.031950214));
#142838=CARTESIAN_POINT('Ctrl Pts',(-1.770806443,4.429590053,-7.03041849));
#142839=CARTESIAN_POINT('Ctrl Pts',(-1.776907359,4.428571429,-7.028876172));
#142840=CARTESIAN_POINT('Ctrl Pts',(-2.154675559,4.365498301,-6.93337597));
#142841=CARTESIAN_POINT('Ctrl Pts',(-2.52003186,4.301245526,-6.79793640900001));
#142842=CARTESIAN_POINT('',(-2.06314071700553,4.43060908088848,-7.21064839953072));
#142843=CARTESIAN_POINT('Origin',(0.0895193861963639,4.16161692514811,0.159722981985705));
#142844=CARTESIAN_POINT('',(-1.91392180109997,4.43060908179128,-7.12129930453859));
#142845=CARTESIAN_POINT('Origin',(2.83844128756705E-13,4.52171036999956,
6.29270940910587E-13));
#142846=CARTESIAN_POINT('',(-2.59736126722513,4.52063234085742,-7.03588760899641));
#142847=CARTESIAN_POINT('Origin',(0.0365874470749949,4.69624336608352,0.179762794924447));
#142848=CARTESIAN_POINT('Origin',(0.0714082026967897,4.55356366313828,0.178135238051541));
#142849=CARTESIAN_POINT('Ctrl Pts',(-0.780368259,4.301266351,-7.459291212));
#142850=CARTESIAN_POINT('Ctrl Pts',(-1.186697327,4.365380951,-7.416782306));
#142851=CARTESIAN_POINT('Ctrl Pts',(-1.586004669,4.430609079,-7.330388065));
#142852=CARTESIAN_POINT('Ctrl Pts',(-1.59000891228632,4.43126318491329,
-7.3295217058748));
#142853=CARTESIAN_POINT('Ctrl Pts',(-1.59401315557265,4.43191729082659,
-7.3286553467496));
#142854=CARTESIAN_POINT('Ctrl Pts',(-0.990426433,4.301266351,-7.182030039));
#142855=CARTESIAN_POINT('Ctrl Pts',(-1.381652286,4.365380951,-7.12807866));
#142856=CARTESIAN_POINT('Ctrl Pts',(-1.764702859,4.430609079,-7.03195021400001));
#142857=CARTESIAN_POINT('Ctrl Pts',(-1.76854407984401,4.43126318491329,
-7.03098624052886));
#142858=CARTESIAN_POINT('Ctrl Pts',(-1.77238530068803,4.43191729082659,
-7.03002226705771));
#142859=CARTESIAN_POINT('',(-1.58600466065801,4.43060908007271,-7.33038806363038));
#142860=CARTESIAN_POINT('',(-1.67535374514333,4.43060908208281,-7.18116914389923));
#142861=CARTESIAN_POINT('',(-1.03059034903994,4.34096089506838,-7.42885479274644));
#142862=CARTESIAN_POINT('Origin',(0.0586457274098809,4.55349069186996,0.178112571906096));
#142863=CARTESIAN_POINT('Ctrl Pts',(-0.995066310316856,4.30202682665611,
-7.18138865679072));
#142864=CARTESIAN_POINT('Ctrl Pts',(-1.00109391475538,4.30883437581194,
-7.22255772940696));
#142865=CARTESIAN_POINT('Ctrl Pts',(-1.00706759779501,4.31547784268671,
-7.26378847026125));
#142866=CARTESIAN_POINT('Ctrl Pts',(-1.01890327495275,4.32844538967593,
-7.34626354102029));
#142867=CARTESIAN_POINT('Ctrl Pts',(-1.02477228040847,4.334777155855,-7.38755678749405));
#142868=CARTESIAN_POINT('Ctrl Pts',(-1.03059034988965,4.34096089506402,
-7.42885479258455));
#142869=CARTESIAN_POINT('Ctrl Pts',(-0.45670000052831,4.43188407004788,
-7.48608652399922));
#142870=CARTESIAN_POINT('Ctrl Pts',(-0.460764682764155,4.43124657452394,
-7.48583412099961));
#142871=CARTESIAN_POINT('Ctrl Pts',(-0.464829365,4.430609079,-7.485581718));
#142872=CARTESIAN_POINT('Ctrl Pts',(-0.471326692,4.429590053,-7.485178256));
#142873=CARTESIAN_POINT('Ctrl Pts',(-0.477823308,4.428571429,-7.484763516));
#142874=CARTESIAN_POINT('Ctrl Pts',(-0.880093255,4.365498301,-7.459082817));
#142875=CARTESIAN_POINT('Ctrl Pts',(-1.277293469,4.301245526,-7.39043445200001));
#142876=CARTESIAN_POINT('Ctrl Pts',(-0.203913492723738,4.43188407004788,
-7.24713607501221));
#142877=CARTESIAN_POINT('Ctrl Pts',(-0.207848573361869,4.43124657452394,
-7.24702107600611));
#142878=CARTESIAN_POINT('Ctrl Pts',(-0.211783654,4.430609079,-7.246906077));
#142879=CARTESIAN_POINT('Ctrl Pts',(-0.218073815,4.429590053,-7.246722253));
#142880=CARTESIAN_POINT('Ctrl Pts',(-0.224363648,4.428571429,-7.24652751));
#142881=CARTESIAN_POINT('Ctrl Pts',(-0.613829558,4.365498301,-7.234469046));
#142882=CARTESIAN_POINT('Ctrl Pts',(-0.999759533999999,4.301245526,-7.180736792));
#142883=CARTESIAN_POINT('',(-0.464829372801399,4.43060908088847,-7.48558171513932));
#142884=CARTESIAN_POINT('Origin',(0.0530907540069721,4.16161691772973,0.175232768417251));
#142885=CARTESIAN_POINT('',(-0.338306526670948,4.43060908179128,-7.3662438967114));
#142886=CARTESIAN_POINT('Origin',(2.08058396899968E-13,4.52171036999933,
1.10935566288717E-12));
#142887=CARTESIAN_POINT('',(-1.02412854774876,4.52063234084464,-7.42974836164533));
#142888=CARTESIAN_POINT('Origin',(-0.00291160711715602,4.69624333806754,
0.183425348602292));
#142889=CARTESIAN_POINT('Origin',(0.0314449105638315,4.55356367649074,0.189321198648889));
#142890=CARTESIAN_POINT('Ctrl Pts',(0.841403432,4.301266351,-7.452653237));
#142891=CARTESIAN_POINT('Ctrl Pts',(0.435435954,4.365380951,-7.498486904));
#142892=CARTESIAN_POINT('Ctrl Pts',(0.026891988,4.430609079,-7.499951788));
#142893=CARTESIAN_POINT('Ctrl Pts',(0.0227951200966196,4.43126318491329,
-7.49996647781735));
#142894=CARTESIAN_POINT('Ctrl Pts',(0.0186982521932392,4.43191729082659,
-7.49998116763471));
#142895=CARTESIAN_POINT('Ctrl Pts',(0.576653346,4.301266351,-7.22703057400001));
#142896=CARTESIAN_POINT('Ctrl Pts',(0.182976184,4.365380951,-7.258442542));
#142897=CARTESIAN_POINT('Ctrl Pts',(-0.211783654,4.430609079,-7.246906077));
#142898=CARTESIAN_POINT('Ctrl Pts',(-0.215742295038517,4.43126318491329,
-7.24679038963925));
#142899=CARTESIAN_POINT('Ctrl Pts',(-0.219700936077033,4.43191729082659,
-7.24667470227851));
#142900=CARTESIAN_POINT('',(0.0268919958281766,4.43060908007272,-7.49995178486281));
#142901=CARTESIAN_POINT('',(-0.0924458136384814,4.43060908208281,-7.37342893274275));
#142902=CARTESIAN_POINT('',(0.590488465954577,4.3409608949906,-7.47671875698683));
#142903=CARTESIAN_POINT('Origin',(0.0189856734592331,4.55349069303058,0.186555619209687));
#142904=CARTESIAN_POINT('Ctrl Pts',(0.571984068188108,4.30202682662381,
-7.22740162320937));
#142905=CARTESIAN_POINT('Ctrl Pts',(0.574947519445653,4.30883437575215,
-7.26890394261364));
#142906=CARTESIAN_POINT('Ctrl Pts',(0.577976888267639,4.31547784260444,
-7.31045489694304));
#142907=CARTESIAN_POINT('Ctrl Pts',(0.584147625599597,4.32844539120785,
-7.39354607766314));
#142908=CARTESIAN_POINT('Ctrl Pts',(0.587292662433661,4.33477715900784,
-7.43513558513006));
#142909=CARTESIAN_POINT('Ctrl Pts',(0.590488464761412,4.34096089498466,
-7.47671875703932));
#142910=CARTESIAN_POINT('Ctrl Pts',(1.16326470617875,4.43188407004787,-7.40924298180975));
#142911=CARTESIAN_POINT('Ctrl Pts',(1.15924079508937,4.43124657452393,-7.40987026640487));
#142912=CARTESIAN_POINT('Ctrl Pts',(1.155216884,4.430609079,-7.410497551));
#142913=CARTESIAN_POINT('Ctrl Pts',(1.148784729,4.429590053,-7.411500255));
#142914=CARTESIAN_POINT('Ctrl Pts',(1.142350843,4.428571429,-7.412491791));
#142915=CARTESIAN_POINT('Ctrl Pts',(0.743965153,4.365498301,-7.47388764));
#142916=CARTESIAN_POINT('Ctrl Pts',(0.341293891,4.301245526,-7.492230541));
#142917=CARTESIAN_POINT('Ctrl Pts',(1.35877392498202,4.43188407004787,-7.12153743297934));
#142918=CARTESIAN_POINT('Ctrl Pts',(1.35490612249101,4.43124657452393,-7.12227104898968));
#142919=CARTESIAN_POINT('Ctrl Pts',(1.35103832,4.430609079,-7.123004665));
#142920=CARTESIAN_POINT('Ctrl Pts',(1.344855702,4.429590053,-7.12417733800001));
#142921=CARTESIAN_POINT('Ctrl Pts',(1.338671059,4.428571429,-7.125339276));
#142922=CARTESIAN_POINT('Ctrl Pts',(0.955718432,4.365498301,-7.19728639000001));
#142923=CARTESIAN_POINT('Ctrl Pts',(0.567260438,4.301245526,-7.227773903));
#142924=CARTESIAN_POINT('',(1.15521687582595,4.4306090808884,-7.41049754966774));
#142925=CARTESIAN_POINT('Origin',(0.0141796548106751,4.16161692684402,0.182548867422564));
#142926=CARTESIAN_POINT('',(1.25312758506097,4.43060908179128,-7.26675111092108));
#142927=CARTESIAN_POINT('Origin',(4.85976683157682E-14,4.52171036999889,
4.54931231574918E-13));
#142928=CARTESIAN_POINT('',(0.59699128478794,4.52063234082281,-7.47620233853116));
#142929=CARTESIAN_POINT('Origin',(-0.0422745649116112,4.6962433242186,0.178510930585105));
#142930=CARTESIAN_POINT('Origin',(-0.00998869204440783,4.55356365368728,
0.191654495980108));
#142931=CARTESIAN_POINT('Ctrl Pts',(2.423832035,4.301266351,-7.097537479));
#142932=CARTESIAN_POINT('Ctrl Pts',(2.037208734,4.365380951,-7.229570588));
#142933=CARTESIAN_POINT('Ctrl Pts',(1.638531205,4.430609079,-7.3188261));
#142934=CARTESIAN_POINT('Ctrl Pts',(1.6345332774615,4.43126318491329,-7.31972115187383));
#142935=CARTESIAN_POINT('Ctrl Pts',(1.630535349923,4.43191729082659,-7.32061620374768));
#142936=CARTESIAN_POINT('Ctrl Pts',(2.116769455,4.301266351,-6.934103192));
#142937=CARTESIAN_POINT('Ctrl Pts',(1.739048891,4.365380951,-7.049409718));
#142938=CARTESIAN_POINT('Ctrl Pts',(1.35103832,4.430609079,-7.123004665));
#142939=CARTESIAN_POINT('Ctrl Pts',(1.34714736042944,4.43126318491329,-7.12374267314921));
#142940=CARTESIAN_POINT('Ctrl Pts',(1.34325640085888,4.43191729082659,-7.1244806812984));
#142941=CARTESIAN_POINT('',(1.63853121200172,4.43060908007271,-7.31882609525449));
#142942=CARTESIAN_POINT('',(1.49478478146104,4.43060908208281,-7.22091537857492));
#142943=CARTESIAN_POINT('',(2.18395669669526,4.34096089502823,-7.1749796617874));
#142944=CARTESIAN_POINT('Origin',(-0.021562133991038,4.55349069234491,0.186275393138425));
#142945=CARTESIAN_POINT('Ctrl Pts',(2.11228910713819,4.30202682661483,-6.93546932305721));
#142946=CARTESIAN_POINT('Ctrl Pts',(2.12410504656257,4.30883437576042,-6.97536428675135));
#142947=CARTESIAN_POINT('Ctrl Pts',(2.13599581749022,4.31547784262358,-7.01529257801128));
#142948=CARTESIAN_POINT('Ctrl Pts',(2.15988442355864,4.32844538540125,-7.09511457087793));
#142949=CARTESIAN_POINT('Ctrl Pts',(2.17189643383093,4.33477714729008,-7.13505560883328));
#142950=CARTESIAN_POINT('Ctrl Pts',(2.1839566958225,4.34096089501118,-7.17497966205368));
#142951=CARTESIAN_POINT('Ctrl Pts',(2.72883644918952,4.43188407004788,-6.98595147272629));
#142952=CARTESIAN_POINT('Ctrl Pts',(2.72504146259476,4.43124657452394,-6.98742911336314));
#142953=CARTESIAN_POINT('Ctrl Pts',(2.721246476,4.430609079,-6.988906754));
#142954=CARTESIAN_POINT('Ctrl Pts',(2.715180253,4.429590053,-6.991268738));
#142955=CARTESIAN_POINT('Ctrl Pts',(2.709109939,4.428571429,-6.993620188));
#142956=CARTESIAN_POINT('Ctrl Pts',(2.333236578,4.365498301,-7.139221784));
#142957=CARTESIAN_POINT('Ctrl Pts',(1.943922727,4.301245526,-7.243698257));
#142958=CARTESIAN_POINT('Ctrl Pts',(2.85792658132718,4.43188407004788,-6.66294361747869));
#142959=CARTESIAN_POINT('Ctrl Pts',(2.85430691216359,4.43124657452394,-6.66449154473935));
#142960=CARTESIAN_POINT('Ctrl Pts',(2.850687243,4.430609079,-6.666039472));
#142961=CARTESIAN_POINT('Ctrl Pts',(2.844901262,4.429590053,-6.66851380800001));
#142962=CARTESIAN_POINT('Ctrl Pts',(2.839110994,4.428571429,-6.670978097));
#142963=CARTESIAN_POINT('Ctrl Pts',(2.48057809,4.365498301,-6.823566622));
#142964=CARTESIAN_POINT('Ctrl Pts',(2.107755942,4.301245526,-6.93684834));
#142965=CARTESIAN_POINT('',(2.72124646772514,4.43060908088843,-6.98890675455777));
#142966=CARTESIAN_POINT('Origin',(-0.0253944807870607,4.16161700236696,
0.181329183444667));
#142967=CARTESIAN_POINT('',(2.78596684358495,4.43060908179128,-6.82747311949418));
#142968=CARTESIAN_POINT('Origin',(-9.20379224222945E-13,4.52171036999956,
2.86532950144469E-12));
#142969=CARTESIAN_POINT('',(2.19019646746151,4.52063234082816,-7.1730774032274));
#142970=CARTESIAN_POINT('Origin',(-0.0796607088715576,4.69624335133068,
0.165249406375639));
#142971=CARTESIAN_POINT('Origin',(-0.0509551821821491,4.55356366255728,
0.185026366182512));
#142972=CARTESIAN_POINT('Ctrl Pts',(3.892924945,4.301266351,-6.410548758));
#142973=CARTESIAN_POINT('Ctrl Pts',(3.543723898,4.365380951,-6.622607587));
#142974=CARTESIAN_POINT('Ctrl Pts',(3.173554525,4.430609079,-6.795480239));
#142975=CARTESIAN_POINT('Ctrl Pts',(3.16984247648315,4.43126318491329,-6.7972138013049));
#142976=CARTESIAN_POINT('Ctrl Pts',(3.1661304279663,4.43191729082659,-6.79894736360979));
#142977=CARTESIAN_POINT('Ctrl Pts',(3.557907777,4.301266351,-6.31694485100001));
#142978=CARTESIAN_POINT('Ctrl Pts',(3.213805605,4.365380951,-6.510754331));
#142979=CARTESIAN_POINT('Ctrl Pts',(2.850687243,4.430609079,-6.666039472));
#142980=CARTESIAN_POINT('Ctrl Pts',(2.84704590183182,4.43126318491329,-6.6675966672176));
#142981=CARTESIAN_POINT('Ctrl Pts',(2.84340456066365,4.43191729082659,-6.6691538624352));
#142982=CARTESIAN_POINT('',(3.17355453084134,4.43060908007268,-6.7954802328551));
#142983=CARTESIAN_POINT('',(3.01212090167401,4.43060908208281,-6.73075984759061));
#142984=CARTESIAN_POINT('',(3.67530553870476,4.34096089505283,-6.53774649241647));
#142985=CARTESIAN_POINT('Origin',(-0.0611017768781913,4.55349067999031,
0.177285242002856));
#142986=CARTESIAN_POINT('Ctrl Pts',(3.55382585549295,4.30202682665132,-6.31924218533956));
#142987=CARTESIAN_POINT('Ctrl Pts',(3.57394168121668,4.30883434154526,-6.35566416610688));
#142988=CARTESIAN_POINT('Ctrl Pts',(3.59413774087051,4.31547777379272,-6.39210258844027));
#142989=CARTESIAN_POINT('Ctrl Pts',(3.63462742824362,4.32844538541138,-6.46492342997811));
#142990=CARTESIAN_POINT('Ctrl Pts',(3.65494474691591,4.33477714732342,-6.50134844167838));
#142991=CARTESIAN_POINT('Ctrl Pts',(3.67530553792546,4.34096089503749,-6.53774649285502));
#142992=CARTESIAN_POINT('Ctrl Pts',(4.16681083229605,4.43188407004787,-6.23600463637641));
#142993=CARTESIAN_POINT('Ctrl Pts',(4.16342221964803,4.43124657452394,-6.2382635406882));
#142994=CARTESIAN_POINT('Ctrl Pts',(4.160033607,4.430609079,-6.240522445));
#142995=CARTESIAN_POINT('Ctrl Pts',(4.154616966,4.429590053,-6.244133266));
#142996=CARTESIAN_POINT('Ctrl Pts',(4.149194064,4.428571429,-6.247734679));
#142997=CARTESIAN_POINT('Ctrl Pts',(3.813408453,4.365498301,-6.470733852));
#142998=CARTESIAN_POINT('Ctrl Pts',(3.455655896,4.301245526,-6.656458693));
#142999=CARTESIAN_POINT('Ctrl Pts',(4.2234457685604,4.43188407004787,-5.89279796219158));
#143000=CARTESIAN_POINT('Ctrl Pts',(4.2202434837802,4.43124657452394,-5.89508782209579));
#143001=CARTESIAN_POINT('Ctrl Pts',(4.217041199,4.430609079,-5.897377682));
#143002=CARTESIAN_POINT('Ctrl Pts',(4.2119224,4.429590053,-5.90103798500001));
#143003=CARTESIAN_POINT('Ctrl Pts',(4.206797255,4.428571429,-5.904689396));
#143004=CARTESIAN_POINT('Ctrl Pts',(3.889448673,4.365498301,-6.130784462));
#143005=CARTESIAN_POINT('Ctrl Pts',(3.549695121,4.301245526,-6.321563458));
#143006=CARTESIAN_POINT('',(4.16003359904532,4.43060908088844,-6.24052244736554));
#143007=CARTESIAN_POINT('Origin',(-0.0637811806429589,4.16161696907178,
0.171630745914088));
#143008=CARTESIAN_POINT('',(4.18853738885309,4.43060908179128,-6.06895007326361));
#143009=CARTESIAN_POINT('Origin',(-2.25730892311482E-13,4.52171037000022,
4.59701721133854E-13));
#143010=CARTESIAN_POINT('',(3.68099049779537,4.52063234084953,-6.53454734113602));
#143011=CARTESIAN_POINT('Origin',(-0.113322216422975,4.6962433515151,0.144261627847397));
#143012=CARTESIAN_POINT('Origin',(-0.089539248214478,4.55356366861275,0.169746975297933));
#143013=CARTESIAN_POINT('Ctrl Pts',(5.179989011,4.301266351,-5.423809901));
#143014=CARTESIAN_POINT('Ctrl Pts',(4.884538471,4.365380951,-5.705978816));
#143015=CARTESIAN_POINT('Ctrl Pts',(4.560185962,4.430609079,-5.954385274));
#143016=CARTESIAN_POINT('Ctrl Pts',(4.55693336376311,4.43126318491329,-5.95687628728));
#143017=CARTESIAN_POINT('Ctrl Pts',(4.55368076552623,4.43191729082659,-5.95936730056002));
#143018=CARTESIAN_POINT('Ctrl Pts',(4.832682286,4.301266351,-5.404413189));
#143019=CARTESIAN_POINT('Ctrl Pts',(4.53828834,4.365380951,-5.66766330700001));
#143020=CARTESIAN_POINT('Ctrl Pts',(4.217041199,4.430609079,-5.897377682));
#143021=CARTESIAN_POINT('Ctrl Pts',(4.2138197413099,4.43126318491329,-5.89968125157441));
#143022=CARTESIAN_POINT('Ctrl Pts',(4.2105982836198,4.43191729082659,-5.90198482114881));
#143023=CARTESIAN_POINT('',(4.5601859663393,4.43060908007276,-5.95438526676242));
#143024=CARTESIAN_POINT('',(4.38861359606048,4.43060908208281,-5.92588146647616));
#143025=CARTESIAN_POINT('',(4.99480117906598,4.34096089499077,-5.59481556261796));
#143026=CARTESIAN_POINT('Origin',(-0.0977841513231226,4.55349066656064,
0.160005103683161));
#143027=CARTESIAN_POINT('Ctrl Pts',(4.82918965631123,4.30202682667343,-5.40753430549404));
#143028=CARTESIAN_POINT('Ctrl Pts',(4.85666484375131,4.3088343438705,-5.43878046339275));
#143029=CARTESIAN_POINT('Ctrl Pts',(4.88422192483148,4.31547777844033,-5.47002543166698));
#143030=CARTESIAN_POINT('Ctrl Pts',(4.93941931908904,4.32844539121672,-5.5324396823216));
#143031=CARTESIAN_POINT('Ctrl Pts',(4.96709195863958,4.33477715901929,-5.56364550569783));
#143032=CARTESIAN_POINT('Ctrl Pts',(4.99480117811663,4.34096089498488,-5.59481556334787));
#143033=CARTESIAN_POINT('Ctrl Pts',(5.40994977202152,4.43188407004788,-5.19446915376555));
#143034=CARTESIAN_POINT('Ctrl Pts',(5.40712598101076,4.43124657452394,-5.19740369788278));
#143035=CARTESIAN_POINT('Ctrl Pts',(5.40430219,4.430609079,-5.200338242));
#143036=CARTESIAN_POINT('Ctrl Pts',(5.399788407,4.429590053,-5.205029062));
#143037=CARTESIAN_POINT('Ctrl Pts',(5.395266487,4.428571429,-5.209712039));
#143038=CARTESIAN_POINT('Ctrl Pts',(5.115269587,4.365498301,-5.499681596));
#143039=CARTESIAN_POINT('Ctrl Pts',(4.805806437,4.301245526,-5.757970518));
#143040=CARTESIAN_POINT('Ctrl Pts',(5.39148132667975,4.43188407004788,-4.84711162513905));
#143041=CARTESIAN_POINT('Ctrl Pts',(5.38884616133987,4.43124657452394,-4.85003634556952));
#143042=CARTESIAN_POINT('Ctrl Pts',(5.38621099600001,4.430609079,-4.852961066));
#143043=CARTESIAN_POINT('Ctrl Pts',(5.381998728,4.429590053,-4.857636183));
#143044=CARTESIAN_POINT('Ctrl Pts',(5.377778351,4.428571429,-4.862303981));
#143045=CARTESIAN_POINT('Ctrl Pts',(5.116452959,4.365498301,-5.15133363500001));
#143046=CARTESIAN_POINT('Ctrl Pts',(4.825654501,4.301245526,-5.410689294));
#143047=CARTESIAN_POINT('',(5.40430218280887,4.4306090808885,-5.20033824619336));
#143048=CARTESIAN_POINT('Origin',(-0.0991855536857289,4.16161699807092,
0.153907044168407));
#143049=CARTESIAN_POINT('',(5.39525658128275,4.43060908179127,-5.02664966657648));
#143050=CARTESIAN_POINT('Origin',(-1.36175792864179E-13,4.52171037000067,
1.70870262383715E-13));
#143051=CARTESIAN_POINT('',(4.99966550416853,4.52063234088266,-5.59046910769365));
#143052=CARTESIAN_POINT('Origin',(-0.141684595591913,4.69624335486042,0.116527713020292));
#143053=CARTESIAN_POINT('Origin',(-0.123936256214732,4.55356364505988,0.146529879876864));
#143054=CARTESIAN_POINT('Ctrl Pts',(6.22484254900001,4.301266351,-4.183459721));
#143055=CARTESIAN_POINT('Ctrl Pts',(5.996957454,4.365380951,-4.522544817));
#143056=CARTESIAN_POINT('Ctrl Pts',(5.733588172,4.430609079,-4.834869871));
#143057=CARTESIAN_POINT('Ctrl Pts',(5.73094711192334,4.43126318491329,-4.83800185824163));
#143058=CARTESIAN_POINT('Ctrl Pts',(5.72830605184669,4.43191729082659,-4.84113384548325));
#143059=CARTESIAN_POINT('Ctrl Pts',(5.881485942,4.301266351,-4.239177174));
#143060=CARTESIAN_POINT('Ctrl Pts',(5.650565757,4.365380951,-4.559558646));
#143061=CARTESIAN_POINT('Ctrl Pts',(5.386210996,4.430609079,-4.852961066));
#143062=CARTESIAN_POINT('Ctrl Pts',(5.38356005356643,4.43126318491329,-4.85590329757679));
#143063=CARTESIAN_POINT('Ctrl Pts',(5.38090911113287,4.43191729082659,-4.85884552915358));
#143064=CARTESIAN_POINT('',(5.73358817469224,4.4306090800727,-4.83486986299197));
#143065=CARTESIAN_POINT('',(5.5598995967194,4.43060908208281,-4.84391545390054));
#143066=CARTESIAN_POINT('',(6.0807454673922,4.34096089504328,-4.39027727584636));
#143067=CARTESIAN_POINT('Origin',(-0.129894276797609,4.55349069609996,0.135243500745896));
#143068=CARTESIAN_POINT('Ctrl Pts',(5.87874591497346,4.30202682664127,-4.24297613265704));
#143069=CARTESIAN_POINT('Ctrl Pts',(5.91229590573509,4.30883437579162,-4.26758553485663));
#143070=CARTESIAN_POINT('Ctrl Pts',(5.9459256381493,4.31547784262217,-4.29217618267673));
#143071=CARTESIAN_POINT('Ctrl Pts',(6.01324942856366,4.32844539019364,-4.34126516762885));
#143072=CARTESIAN_POINT('Ctrl Pts',(6.04698342047828,4.33477715688986,-4.36579261205998));
#143073=CARTESIAN_POINT('Ctrl Pts',(6.08074546675362,4.34096089503838,-4.39027727658286));
#143074=CARTESIAN_POINT('Ctrl Pts',(6.40012547593568,4.43188407004788,-3.91004606778592));
#143075=CARTESIAN_POINT('Ctrl Pts',(6.39799854296784,4.43124657452394,-3.91351903539296));
#143076=CARTESIAN_POINT('Ctrl Pts',(6.39587161,4.430609079,-3.916992003));
#143077=CARTESIAN_POINT('Ctrl Pts',(6.392471743,4.429590053,-3.922543484));
#143078=CARTESIAN_POINT('Ctrl Pts',(6.389062245,4.428571429,-3.928089055));
#143079=CARTESIAN_POINT('Ctrl Pts',(6.1779464,4.365498301,-4.271470342));
#143080=CARTESIAN_POINT('Ctrl Pts',(5.93124281,4.301245526,-4.590246042));
#143081=CARTESIAN_POINT('Ctrl Pts',(6.30741720870541,4.43188407004788,-3.57477973384486));
#143082=CARTESIAN_POINT('Ctrl Pts',(6.30547238085271,4.43124657452394,-3.57820255892243));
#143083=CARTESIAN_POINT('Ctrl Pts',(6.303527553,4.430609079,-3.581625384));
#143084=CARTESIAN_POINT('Ctrl Pts',(6.300418778,4.429590053,-3.587096713));
#143085=CARTESIAN_POINT('Ctrl Pts',(6.297300509,4.428571429,-3.592562637));
#143086=CARTESIAN_POINT('Ctrl Pts',(6.104217591,4.365498301,-3.931012172));
#143087=CARTESIAN_POINT('Ctrl Pts',(5.875971639,4.301245526,-4.246817313));
#143088=CARTESIAN_POINT('',(6.39587160368013,4.43060908088839,-3.91699200834876));
#143089=CARTESIAN_POINT('Origin',(-0.129952104088461,4.16161691724407,0.128986828453043));
#143090=CARTESIAN_POINT('',(6.34969957276025,4.43060908179128,-3.74930870830136));
#143091=CARTESIAN_POINT('Origin',(7.65446733774766E-13,4.52171036999978,
-5.46871575801688E-13));
#143092=CARTESIAN_POINT('',(6.08456170863532,4.52063234083347,-4.38498675147079));
#143093=CARTESIAN_POINT('Origin',(-0.163422130634084,4.69624337618487,0.0833453740582352));
#143094=CARTESIAN_POINT('Origin',(-0.152538369419406,4.55356363696838,0.116461520178344));
#143095=CARTESIAN_POINT('Ctrl Pts',(6.97862936700001,4.301266351,-2.747495615));
#143096=CARTESIAN_POINT('Ctrl Pts',(6.828965371,4.365380951,-3.127641648));
#143097=CARTESIAN_POINT('Ctrl Pts',(6.638894171,4.430609079,-3.489281327));
#143098=CARTESIAN_POINT('Ctrl Pts',(6.63698814211831,4.43126318491329,-3.49290783997482));
#143099=CARTESIAN_POINT('Ctrl Pts',(6.63508211323662,4.43191729082659,-3.49653435294964));
#143100=CARTESIAN_POINT('Ctrl Pts',(6.65527785200001,4.301266351,-2.875721945));
#143101=CARTESIAN_POINT('Ctrl Pts',(6.498628999,4.365380951,-3.238254091));
#143102=CARTESIAN_POINT('Ctrl Pts',(6.303527553,4.430609079,-3.581625384));
#143103=CARTESIAN_POINT('Ctrl Pts',(6.30157108094671,4.43126318491329,-3.58506870209134));
#143104=CARTESIAN_POINT('Ctrl Pts',(6.29961460889341,4.43191729082659,-3.58851202018267));
#143105=CARTESIAN_POINT('',(6.63889417191426,4.43060908007269,-3.48928131859345));
#143106=CARTESIAN_POINT('',(6.47121087128357,4.43060908208281,-3.53545333850757));
#143107=CARTESIAN_POINT('',(6.88236085627095,4.34096089503935,-2.98045450270494));
#143108=CARTESIAN_POINT('Origin',(-0.155930962172045,4.55349066752806,0.104158239654767));
#143109=CARTESIAN_POINT('Ctrl Pts',(6.65341855005723,4.30202682672195,-2.88002111094166));
#143110=CARTESIAN_POINT('Ctrl Pts',(6.69147429397009,4.30883434710691,-2.89684283187069));
#143111=CARTESIAN_POINT('Ctrl Pts',(6.72960386510242,4.31547778490924,-2.91362908767087));
#143112=CARTESIAN_POINT('Ctrl Pts',(6.80590665479749,4.3284453854024,-2.94709791124446));
#143113=CARTESIAN_POINT('Ctrl Pts',(6.84412460925024,4.33477714731954,-2.96380009312779));
#143114=CARTESIAN_POINT('Ctrl Pts',(6.88236085589657,4.34096089503806,-2.98045450356496));
#143115=CARTESIAN_POINT('Ctrl Pts',(7.09103842230695,4.43188407004788,-2.44279357166386));
#143116=CARTESIAN_POINT('Ctrl Pts',(7.08970780165348,4.43124657452394,-2.44664257133193));
#143117=CARTESIAN_POINT('Ctrl Pts',(7.08837718100001,4.430609079,-2.450491571));
#143118=CARTESIAN_POINT('Ctrl Pts',(7.086250206,4.429590053,-2.456644133));
#143119=CARTESIAN_POINT('Ctrl Pts',(7.084112554,4.428571429,-2.462792993));
#143120=CARTESIAN_POINT('Ctrl Pts',(6.951749306,4.365498301,-2.843529882));
#143121=CARTESIAN_POINT('Ctrl Pts',(6.779340862,4.301245526,-3.207886762));
#143122=CARTESIAN_POINT('Ctrl Pts',(6.92842527283416,4.43188407004788,-2.13529511646555));
#143123=CARTESIAN_POINT('Ctrl Pts',(6.92726171991709,4.43124657452394,-2.13905599823277));
#143124=CARTESIAN_POINT('Ctrl Pts',(6.926098167,4.430609079,-2.14281688));
#143125=CARTESIAN_POINT('Ctrl Pts',(6.924238247,4.429590053,-2.148828587));
#143126=CARTESIAN_POINT('Ctrl Pts',(6.922367894,4.428571429,-2.154837056));
#143127=CARTESIAN_POINT('Ctrl Pts',(6.806555793,4.365498301,-2.52688095));
#143128=CARTESIAN_POINT('Ctrl Pts',(6.651534875,4.301245526,-2.884368874));
#143129=CARTESIAN_POINT('',(7.08837717605875,4.43060908088843,-2.45049157765917));
#143130=CARTESIAN_POINT('Origin',(-0.154642244386126,4.16161685423742,0.0980353349978125));
#143131=CARTESIAN_POINT('',(7.00723766864643,4.43060908179128,-2.29665424183409));
#143132=CARTESIAN_POINT('Origin',(1.25333771139324E-13,4.52171037000133,
-1.06902334207071E-13));
#143133=CARTESIAN_POINT('',(6.88495056955131,4.52063234088447,-2.9744672892662));
#143134=CARTESIAN_POINT('Origin',(-0.177518215075657,4.69624335632667,0.0462658936315824));
#143135=CARTESIAN_POINT('Origin',(-0.174007811928394,4.55356365656574,0.080947440733857));
#143136=CARTESIAN_POINT('Ctrl Pts',(7.406103233,4.301266351,-1.183061667));
#143137=CARTESIAN_POINT('Ctrl Pts',(7.341658458,4.365380951,-1.586493433));
#143138=CARTESIAN_POINT('Ctrl Pts',(7.233772858,4.430609079,-1.980537866));
#143139=CARTESIAN_POINT('Ctrl Pts',(7.23269098410475,4.43126318491329,-1.98448933297642));
#143140=CARTESIAN_POINT('Ctrl Pts',(7.2316091102095,4.43191729082659,-1.98844079995283));
#143141=CARTESIAN_POINT('Ctrl Pts',(7.117876367,4.301266351,-1.377801155));
#143142=CARTESIAN_POINT('Ctrl Pts',(7.042823572,4.365380951,-1.765532373));
#143143=CARTESIAN_POINT('Ctrl Pts',(6.926098167,4.430609079,-2.14281688));
#143144=CARTESIAN_POINT('Ctrl Pts',(6.92492764777796,4.43126318491329,-2.14660027888924));
#143145=CARTESIAN_POINT('Ctrl Pts',(6.92375712855592,4.43191729082659,-2.15038367777849));
#143146=CARTESIAN_POINT('',(7.23377285707386,4.43060908007274,-1.98053785761356));
#143147=CARTESIAN_POINT('',(7.07993551791367,4.43060908208281,-2.06167735440911));
#143148=CARTESIAN_POINT('',(7.36216470049487,4.34096089500721,-1.43126898997882));
#143149=CARTESIAN_POINT('Origin',(-0.174676265156352,4.5534907088828,0.0682025180186771));
#143150=CARTESIAN_POINT('Ctrl Pts',(7.11698472797653,4.30202682668443,-1.38239950366295));
#143151=CARTESIAN_POINT('Ctrl Pts',(7.15776689795272,4.30883434300015,-1.39064707707501));
#143152=CARTESIAN_POINT('Ctrl Pts',(7.19861354231777,4.3154777766733,-1.39884414345425));
#143153=CARTESIAN_POINT('Ctrl Pts',(7.28032730928822,4.32844539088522,-1.41512765746602));
#143154=CARTESIAN_POINT('Ctrl Pts',(7.32124226296971,4.33477715833814,-1.42322362860611));
#143155=CARTESIAN_POINT('Ctrl Pts',(7.36216470022103,4.34096089500162,-1.43126899106953));
#143156=CARTESIAN_POINT('Ctrl Pts',(7.45038229297625,4.43188407004787,-0.861318764735012));
#143157=CARTESIAN_POINT('Ctrl Pts',(7.44991020298812,4.43124657452393,-0.865363820867506));
#143158=CARTESIAN_POINT('Ctrl Pts',(7.449438113,4.430609079,-0.869408877000001));
#143159=CARTESIAN_POINT('Ctrl Pts',(7.448683485,4.429590053,-0.875874832));
#143160=CARTESIAN_POINT('Ctrl Pts',(7.447917633,4.428571429,-0.882339467));
#143161=CARTESIAN_POINT('Ctrl Pts',(7.400496141,4.365498301,-1.282629125));
#143162=CARTESIAN_POINT('Ctrl Pts',(7.310444469,4.301245526,-1.675530263));
#143163=CARTESIAN_POINT('Ctrl Pts',(7.22546787182032,4.43188407004787,-0.595966473717372));
#143164=CARTESIAN_POINT('Ctrl Pts',(7.22514000041016,4.43124657452393,-0.599889557358686));
#143165=CARTESIAN_POINT('Ctrl Pts',(7.224812129,4.430609079,-0.603812641));
#143166=CARTESIAN_POINT('Ctrl Pts',(7.224288032,4.429590053,-0.610083625));
#143167=CARTESIAN_POINT('Ctrl Pts',(7.22375305,4.428571429,-0.616353689));
#143168=CARTESIAN_POINT('Ctrl Pts',(7.190627011,4.365498301,-1.004595582));
#143169=CARTESIAN_POINT('Ctrl Pts',(7.116079733,4.301245526,-1.387050553));
#143170=CARTESIAN_POINT('',(7.44943810973751,4.43060908088848,-0.869408884644942));
#143171=CARTESIAN_POINT('Origin',(-0.172101497542194,4.16161689916212,0.0624998054184125));
#143172=CARTESIAN_POINT('',(7.33712511928294,4.43060908179128,-0.736610776103072));
#143173=CARTESIAN_POINT('Origin',(-2.99673480474993E-13,4.52171037000022,
6.90094682787024E-14));
#143174=CARTESIAN_POINT('',(7.36340679369017,4.52063234083055,-1.42486504209282));
#143175=CARTESIAN_POINT('Origin',(-0.183313845500021,4.69624335980962,0.00702306773572942));
#143176=CARTESIAN_POINT('Origin',(-0.1873408563391,4.55356370368071,0.041648395163872));
#143177=CARTESIAN_POINT('Ctrl Pts',(7.487275942,4.301266351,0.436690929));
#143178=CARTESIAN_POINT('Ctrl Pts',(7.511063754,4.365380951,0.028837453));
#143179=CARTESIAN_POINT('Ctrl Pts',(7.490408365,4.430609079,-0.379186656));
#143180=CARTESIAN_POINT('Ctrl Pts',(7.49020123331463,4.43126318491329,-0.383278310791366));
#143181=CARTESIAN_POINT('Ctrl Pts',(7.48999410162926,4.43191729082659,-0.387369965582731));
#143182=CARTESIAN_POINT('Ctrl Pts',(7.247650894,4.301266351,0.184544087));
#143183=CARTESIAN_POINT('Ctrl Pts',(7.257703542,4.365380951,-0.210256324));
#143184=CARTESIAN_POINT('Ctrl Pts',(7.224812129,4.430609079,-0.603812641));
#143185=CARTESIAN_POINT('Ctrl Pts',(7.22448229479504,4.43126318491329,-0.607759213162297));
#143186=CARTESIAN_POINT('Ctrl Pts',(7.22415246059009,4.43191729082659,-0.611705785324594));
#143187=CARTESIAN_POINT('',(7.35761024829061,4.43060908208281,-0.491499629179973));
#143188=CARTESIAN_POINT('Ctrl Pts',(7.24776860954439,4.30202682668585,0.179861568603662));
#143189=CARTESIAN_POINT('Ctrl Pts',(7.2893702940003,4.30883434207202,0.180573779782587));
#143190=CARTESIAN_POINT('Ctrl Pts',(7.33102408727948,4.31547777481083,0.181349177265882));
#143191=CARTESIAN_POINT('Ctrl Pts',(7.41432788288339,4.32844538541458,0.183012406880999));
#143192=CARTESIAN_POINT('Ctrl Pts',(7.45602662296787,4.33477714731221,0.183901219773324));
#143193=CARTESIAN_POINT('Ctrl Pts',(7.49772190592654,4.34096089501742,0.184841069557451));
#143194=CARTESIAN_POINT('Ctrl Pts',(7.46135457079931,4.43188407004788,0.760430350372509));
#143195=CARTESIAN_POINT('Ctrl Pts',(7.46176308489966,4.43124657452394,0.756378380186254));
#143196=CARTESIAN_POINT('Ctrl Pts',(7.462171599,4.430609079,0.75232641));
#143197=CARTESIAN_POINT('Ctrl Pts',(7.46282460200001,4.429590053,0.745849403));
#143198=CARTESIAN_POINT('Ctrl Pts',(7.463466361,4.428571429,0.739371272));
#143199=CARTESIAN_POINT('Ctrl Pts',(7.503204002,4.365498301,0.338245945));
#143200=CARTESIAN_POINT('Ctrl Pts',(7.499719818,4.301245526,-0.064827831));
#143201=CARTESIAN_POINT('Ctrl Pts',(7.18465562199158,4.43188407004788,0.971228900272083));
#143202=CARTESIAN_POINT('Ctrl Pts',(7.1851787634958,4.43124657452394,0.967327053636041));
#143203=CARTESIAN_POINT('Ctrl Pts',(7.18570190500001,4.430609079,0.963425207));
#143204=CARTESIAN_POINT('Ctrl Pts',(7.186538138,4.429590053,0.95718817));
#143205=CARTESIAN_POINT('Ctrl Pts',(7.187363542,4.428571429,0.95094969));
#143206=CARTESIAN_POINT('Ctrl Pts',(7.238472502,4.365498301,0.564663559));
#143207=CARTESIAN_POINT('Ctrl Pts',(7.247884611,4.301245526,0.175124711));
#143208=CARTESIAN_POINT('',(7.32393675399974,4.43060908179128,0.857875791427671));
#143209=CARTESIAN_POINT('Ctrl Pts',(7.21835195,4.301266351,2.036024343));
#143210=CARTESIAN_POINT('Ctrl Pts',(7.329260058,4.365380951,1.642819931));
#143211=CARTESIAN_POINT('Ctrl Pts',(7.396800703,4.430609079,1.239894901));
#143212=CARTESIAN_POINT('Ctrl Pts',(7.39747799877158,4.43126318491329,1.23585437963571));
#143213=CARTESIAN_POINT('Ctrl Pts',(7.39815529454315,4.43191729082659,1.23181385827142));
#143214=CARTESIAN_POINT('Ctrl Pts',(7.03853332,4.301266351,1.738260252));
#143215=CARTESIAN_POINT('Ctrl Pts',(7.13322136,4.365380951,1.354851078));
#143216=CARTESIAN_POINT('Ctrl Pts',(7.185701905,4.430609079,0.963425207));
#143217=CARTESIAN_POINT('Ctrl Pts',(7.18622817849381,4.43126318491329,0.959499998892894));
#143218=CARTESIAN_POINT('Ctrl Pts',(7.18675445198762,4.43191729082659,0.955574790785788));
#143219=CARTESIAN_POINT('',(7.39680069863646,4.43060908007275,1.23989490820429));
#143220=CARTESIAN_POINT('',(7.29125130110721,4.43060908208281,1.10166007314573));
#143221=CARTESIAN_POINT('',(7.28269396809365,4.340960895,1.79230816784698));
#143222=CARTESIAN_POINT('Origin',(-0.187169460194456,4.55349066545353,-0.0114457567602202));
#143223=CARTESIAN_POINT('Ctrl Pts',(7.03965488667234,4.30202682673479,1.73371251360448));
#143224=CARTESIAN_POINT('Ctrl Pts',(7.08013084537838,4.30883434259959,1.74335120698511));
#143225=CARTESIAN_POINT('Ctrl Pts',(7.12064411130631,4.3154777757409,1.75306281112323));
#143226=CARTESIAN_POINT('Ctrl Pts',(7.2016427944238,4.32844539098669,1.77259501597001));
#143227=CARTESIAN_POINT('Ctrl Pts',(7.24217561132369,4.33477715851113,1.78242705484932));
#143228=CARTESIAN_POINT('Ctrl Pts',(7.28269396836801,4.34096089499022,1.79230816672803));
#143229=CARTESIAN_POINT('Ctrl Pts',(7.12344219883282,4.43188407004788,2.34662258804663));
#143230=CARTESIAN_POINT('Ctrl Pts',(7.12471221641641,4.43124657452394,2.34275316902332));
#143231=CARTESIAN_POINT('Ctrl Pts',(7.125982234,4.430609079,2.33888375));
#143232=CARTESIAN_POINT('Ctrl Pts',(7.128012336,4.429590053,2.332698548));
#143233=CARTESIAN_POINT('Ctrl Pts',(7.130031697,4.428571429,2.326509831));
#143234=CARTESIAN_POINT('Ctrl Pts',(7.255070382,4.365498301,1.94330501));
#143235=CARTESIAN_POINT('Ctrl Pts',(7.338316604,4.301245526,1.548905879));
#143236=CARTESIAN_POINT('Ctrl Pts',(6.80789686203716,4.43188407004788,2.49301069013488));
#143237=CARTESIAN_POINT('Ctrl Pts',(6.80924655451859,4.43124657452394,2.48931252656744));
#143238=CARTESIAN_POINT('Ctrl Pts',(6.810596247,4.430609079,2.485614363));
#143239=CARTESIAN_POINT('Ctrl Pts',(6.81275370800001,4.429590053,2.47970291));
#143240=CARTESIAN_POINT('Ctrl Pts',(6.814900903,4.428571429,2.47378772));
#143241=CARTESIAN_POINT('Ctrl Pts',(6.947855064,4.365498301,2.107519659));
#143242=CARTESIAN_POINT('Ctrl Pts',(7.04078646,4.301245526,1.729111338));
#143243=CARTESIAN_POINT('',(7.12598223423435,4.43060908088847,2.33888374169329));
#143244=CARTESIAN_POINT('Origin',(-0.182438076329164,4.16161690204204,-0.0155402565911994));
#143245=CARTESIAN_POINT('',(6.96828924612303,4.43060908179128,2.4122490402567));
#143246=CARTESIAN_POINT('Origin',(-3.29163779566599E-13,4.52171036999978,
-1.60245081093358E-13));
#143247=CARTESIAN_POINT('',(7.28113231366844,4.52063234086887,1.79864177448102));
#143248=CARTESIAN_POINT('Origin',(-0.169320101021773,4.69624337824747,-0.0705975350664123));
#143249=CARTESIAN_POINT('Origin',(-0.18751371703438,4.55356369516498,-0.0408633449075055));
#143250=CARTESIAN_POINT('Ctrl Pts',(6.611905843,4.301266351,3.540155522));
#143251=CARTESIAN_POINT('Ctrl Pts',(6.804748307,4.365380951,3.179985975));
#143252=CARTESIAN_POINT('Ctrl Pts',(6.95732686,4.430609079,2.80100035));
#143253=CARTESIAN_POINT('Ctrl Pts',(6.95885691362593,4.43126318491329,2.79719989234521));
#143254=CARTESIAN_POINT('Ctrl Pts',(6.96038696725186,4.43191729082659,2.79339943469041));
#143255=CARTESIAN_POINT('Ctrl Pts',(6.500301751,4.301266351,3.210697299));
#143256=CARTESIAN_POINT('Ctrl Pts',(6.675197676,4.365380951,2.856607148));
#143257=CARTESIAN_POINT('Ctrl Pts',(6.810596247,4.430609079,2.485614363));
#143258=CARTESIAN_POINT('Ctrl Pts',(6.81195402022849,4.43126318491329,2.48189405732976));
#143259=CARTESIAN_POINT('Ctrl Pts',(6.81331179345697,4.43191729082659,2.47817375165952));
#143260=CARTESIAN_POINT('',(6.95732685418665,4.43060908007271,2.8010003561233));
#143261=CARTESIAN_POINT('',(6.88396154655906,4.43060908208281,2.6433073745763));
#143262=CARTESIAN_POINT('',(6.7271353543509,4.34096089503984,3.3159689269679));
#143263=CARTESIAN_POINT('Origin',(-0.180332952993478,4.55349066696634,-0.0514140168539484));
#143264=CARTESIAN_POINT('Ctrl Pts',(6.50237472517852,4.30202682664099,3.20649698852999));
#143265=CARTESIAN_POINT('Ctrl Pts',(6.53983233913287,4.30883434160489,3.22461146676558));
#143266=CARTESIAN_POINT('Ctrl Pts',(6.57731071430891,4.31547777390474,3.24280517099429));
#143267=CARTESIAN_POINT('Ctrl Pts',(6.65221682469093,4.32844538541513,3.27929303563529));
#143268=CARTESIAN_POINT('Ctrl Pts',(6.68968837343744,4.33477714732117,3.29760854678755));
#143269=CARTESIAN_POINT('Ctrl Pts',(6.72713535476946,4.34096089503156,3.315968926117));
#143270=CARTESIAN_POINT('Ctrl Pts',(6.45244558794698,4.43188407004788,3.82308936021777));
#143271=CARTESIAN_POINT('Ctrl Pts',(6.45451772397349,4.43124657452394,3.81958342260888));
#143272=CARTESIAN_POINT('Ctrl Pts',(6.45658986000001,4.430609079,3.816077485));
#143273=CARTESIAN_POINT('Ctrl Pts',(6.459902135,4.429590053,3.810473302));
#143274=CARTESIAN_POINT('Ctrl Pts',(6.463204676,4.428571429,3.804863377));
#143275=CARTESIAN_POINT('Ctrl Pts',(6.667697735,4.365498301,3.457497292));
#143276=CARTESIAN_POINT('Ctrl Pts',(6.833781861,4.301245526,3.090214471));
#143277=CARTESIAN_POINT('Ctrl Pts',(6.11280841197593,4.43188407004788,3.89822207217764));
#143278=CARTESIAN_POINT('Ctrl Pts',(6.11492154498796,4.43124657452394,3.89490051308882));
#143279=CARTESIAN_POINT('Ctrl Pts',(6.117034678,4.430609079,3.891578954));
#143280=CARTESIAN_POINT('Ctrl Pts',(6.120412486,4.429590053,3.886269497));
#143281=CARTESIAN_POINT('Ctrl Pts',(6.123781072,4.428571429,3.880954185));
#143282=CARTESIAN_POINT('Ctrl Pts',(6.332363645,4.365498301,3.551830482));
#143283=CARTESIAN_POINT('Ctrl Pts',(6.50446896,4.301245526,3.202246641));
#143284=CARTESIAN_POINT('',(6.45658986212607,4.43060908088851,3.81607747694991));
#143285=CARTESIAN_POINT('Origin',(-0.174832079332926,4.16161692141043,-0.0543957308709359));
#143286=CARTESIAN_POINT('',(6.2868122779834,4.43060908179128,3.85382820484524));
#143287=CARTESIAN_POINT('Origin',(1.20519913493489E-12,4.52171036999911,
5.35595873207839E-13));
#143288=CARTESIAN_POINT('',(6.72424867213751,4.52063234084617,3.32181874799288));
#143289=CARTESIAN_POINT('Origin',(-0.150185083091728,4.69624336268068,-0.105345803530265));
#143290=CARTESIAN_POINT('Origin',(-0.174345382848101,4.55356368596386,-0.0802179147523208));
#143291=CARTESIAN_POINT('Ctrl Pts',(5.696294368,4.301266351,4.878752963));
#143292=CARTESIAN_POINT('Ctrl Pts',(5.962054088,4.365380951,4.568459409));
#143293=CARTESIAN_POINT('Ctrl Pts',(6.192536146,4.430609079,4.231134137));
#143294=CARTESIAN_POINT('Ctrl Pts',(6.19484741387888,4.43126318491329,4.22775144824465));
#143295=CARTESIAN_POINT('Ctrl Pts',(6.19715868175776,4.43191729082659,4.22436875948929));
#143296=CARTESIAN_POINT('Ctrl Pts',(5.658123296,4.301266351,4.53300571));
#143297=CARTESIAN_POINT('Ctrl Pts',(5.905049168,4.365380951,4.224791444));
#143298=CARTESIAN_POINT('Ctrl Pts',(6.117034678,4.430609079,3.891578954));
#143299=CARTESIAN_POINT('Ctrl Pts',(6.11916046299299,4.43126318491329,3.88823750811193));
#143300=CARTESIAN_POINT('Ctrl Pts',(6.12128624798599,4.43191729082659,3.88489606222386));
#143301=CARTESIAN_POINT('',(6.19253613901402,4.43060908007276,4.23113414170784));
#143302=CARTESIAN_POINT('',(6.15478540133549,4.43060908208281,4.06135656166154));
#143303=CARTESIAN_POINT('',(5.85702336818681,4.34096089503826,4.68457866470363));
#143304=CARTESIAN_POINT('Origin',(-0.165064523379462,4.55349069367169,-0.0889783509120712));
#143305=CARTESIAN_POINT('Ctrl Pts',(5.66105074783569,4.30202682668129,4.52934922739746));
#143306=CARTESIAN_POINT('Ctrl Pts',(5.69373871051027,4.30883437580268,4.55509260828656));
#143307=CARTESIAN_POINT('Ctrl Pts',(5.72642993561914,4.31547784263449,4.58091784164831));
#143308=CARTESIAN_POINT('Ctrl Pts',(5.79174062469475,4.32844538544317,4.63265496595597));
#143309=CARTESIAN_POINT('Ctrl Pts',(5.8243988159226,4.33477714732765,4.65859754598103));
#143310=CARTESIAN_POINT('Ctrl Pts',(5.8570233687867,4.3409608950263,4.6845786639532));
#143311=CARTESIAN_POINT('Ctrl Pts',(5.47973979224387,4.43188407004788,5.12079272560908));
#143312=CARTESIAN_POINT('Ctrl Pts',(5.48251715612193,4.43124657452394,5.11781420230454));
#143313=CARTESIAN_POINT('Ctrl Pts',(5.48529452,4.430609079,5.11483567900001));
#143314=CARTESIAN_POINT('Ctrl Pts',(5.48973409,4.429590053,5.110074559));
#143315=CARTESIAN_POINT('Ctrl Pts',(5.494165387,4.428571429,5.10530574));
#143316=CARTESIAN_POINT('Ctrl Pts',(5.768550952,4.365498301,4.810020844));
#143317=CARTESIAN_POINT('Ctrl Pts',(6.009707074,4.301245526,4.487028069));
#143318=CARTESIAN_POINT('Ctrl Pts',(5.13189183273128,4.43188407004788,5.12115692153224));
#143319=CARTESIAN_POINT('Ctrl Pts',(5.13466959886564,4.43124657452394,5.11836727976612));
#143320=CARTESIAN_POINT('Ctrl Pts',(5.137447365,4.430609079,5.11557763800001));
#143321=CARTESIAN_POINT('Ctrl Pts',(5.141887578,4.429590053,5.111118442));
#143322=CARTESIAN_POINT('Ctrl Pts',(5.146320044,4.428571429,5.106651545));
#143323=CARTESIAN_POINT('Ctrl Pts',(5.42077793999999,4.365498301,4.830061659));
#143324=CARTESIAN_POINT('Ctrl Pts',(5.66400972,4.301245526,4.525648449));
#143325=CARTESIAN_POINT('',(5.48529452372975,4.43060908088849,5.11483567156938));
#143326=CARTESIAN_POINT('Origin',(-0.159051130077427,4.16161688519082,-0.0907077120393646));
#143327=CARTESIAN_POINT('',(5.31137095442371,4.43060908179128,5.11520664611903));
#143328=CARTESIAN_POINT('Origin',(7.09501901674514E-13,4.52171036999911,
6.53557069574262E-13));
#143329=CARTESIAN_POINT('',(5.85294663643186,4.52063234086129,4.68967116858934));
#143330=CARTESIAN_POINT('Origin',(-0.124027660144729,4.69624335798661,-0.135168275660474));
#143331=CARTESIAN_POINT('Origin',(-0.15302475186547,4.55356366957091,-0.115821519450654));
#143332=CARTESIAN_POINT('Ctrl Pts',(4.514330499,4.30126635099999,5.989225338));
#143333=CARTESIAN_POINT('Ctrl Pts',(4.840580846,4.365380951,5.743316758));
#143334=CARTESIAN_POINT('Ctrl Pts',(5.138189324,4.43060907900001,5.463424793));
#143335=CARTESIAN_POINT('Ctrl Pts',(5.1411737338133,4.43126318491329,5.4606180439026));
#143336=CARTESIAN_POINT('Ctrl Pts',(5.14415814362659,4.43191729082658,5.45781129480519));
#143337=CARTESIAN_POINT('Ctrl Pts',(4.551377285,4.30126635099999,5.643355811));
#143338=CARTESIAN_POINT('Ctrl Pts',(4.858787124,4.365380951,5.39542918700001));
#143339=CARTESIAN_POINT('Ctrl Pts',(5.13744736500001,4.43060907900001,5.115577638));
#143340=CARTESIAN_POINT('Ctrl Pts',(5.14024176240226,4.43126318491329,5.11277129419316));
#143341=CARTESIAN_POINT('Ctrl Pts',(5.14303615980453,4.43191729082658,5.1099649503863));
#143342=CARTESIAN_POINT('',(5.13818931615188,4.43060908007285,5.46342479611677));
#143343=CARTESIAN_POINT('',(5.13781833060832,4.4306090820833,5.28950122899332));
#143344=CARTESIAN_POINT('',(4.71304347885007,4.34096089504838,5.83414271038548));
#143345=CARTESIAN_POINT('Origin',(-0.142077824150623,4.55349070797828,-0.122382224788236));
#143346=CARTESIAN_POINT('Ctrl Pts',(4.55502233006115,4.30202682664792,5.64041413156312));
#143347=CARTESIAN_POINT('Ctrl Pts',(4.58141200045756,4.30883437577953,5.67258259200198));
#143348=CARTESIAN_POINT('Ctrl Pts',(4.60778726118877,4.31547784264405,5.70483169273335));
#143349=CARTESIAN_POINT('Ctrl Pts',(4.66044906993919,4.3284453854127,5.76939909879075));
#143350=CARTESIAN_POINT('Ctrl Pts',(4.68676684300026,4.33477714733193,5.80175570146899));
#143351=CARTESIAN_POINT('Ctrl Pts',(4.71304347955343,4.34096089504684,5.83414270979538));
#143352=CARTESIAN_POINT('Ctrl Pts',(4.25080745523902,4.43188407004788,6.17905351246968));
#143353=CARTESIAN_POINT('Ctrl Pts',(4.25416018011951,4.43124657452394,6.17674167673485));
#143354=CARTESIAN_POINT('Ctrl Pts',(4.257512905,4.430609079,6.174429841));
#143355=CARTESIAN_POINT('Ctrl Pts',(4.26287218,4.429590053,6.17073441));
#143356=CARTESIAN_POINT('Ctrl Pts',(4.268225031,4.428571429,6.167029681));
#143357=CARTESIAN_POINT('Ctrl Pts',(4.599673138,4.365498301,5.937633167));
#143358=CARTESIAN_POINT('Ctrl Pts',(4.904625063,4.301245526,5.674033221));
#143359=CARTESIAN_POINT('Ctrl Pts',(3.91101369546929,4.43188407004788,6.10463216359984));
#143360=CARTESIAN_POINT('Ctrl Pts',(3.91432620973464,4.43124657452394,6.10250488029992));
#143361=CARTESIAN_POINT('Ctrl Pts',(3.917638724,4.430609079,6.100377597));
#143362=CARTESIAN_POINT('Ctrl Pts',(3.922933723,4.429590053,6.09697717));
#143363=CARTESIAN_POINT('Ctrl Pts',(3.928222811,4.428571429,6.093567555));
#143364=CARTESIAN_POINT('Ctrl Pts',(4.255722683,4.365498301,5.882444522));
#143365=CARTESIAN_POINT('Ctrl Pts',(4.558707681,4.301245526,5.637435967));
#143366=CARTESIAN_POINT('',(4.25751291014934,4.43060908088846,6.17442983449011));
#143367=CARTESIAN_POINT('Origin',(-0.135833122815991,4.16161692292354,-0.122778312928644));
#143368=CARTESIAN_POINT('',(4.08757582880652,4.43060908179129,6.13740370947171));
#143369=CARTESIAN_POINT('Origin',(3.38704758684472E-13,4.52171036999933,
4.64038529823796E-13));
#143370=CARTESIAN_POINT('',(4.70796732118483,4.5206323408538,5.8382397777685));
#143371=CARTESIAN_POINT('Origin',(-0.0920707914317653,4.69624335804417,
-0.158670405151131));
#143372=CARTESIAN_POINT('Origin',(-0.124548980264571,4.55356367804712,-0.146009561469306));
#143373=CARTESIAN_POINT('Ctrl Pts',(3.121281553,4.301266351,6.819648192));
#143374=CARTESIAN_POINT('Ctrl Pts',(3.492767424,4.365380951,6.649623));
#143375=CARTESIAN_POINT('Ctrl Pts',(3.84358648,4.430609079,6.440251778));
#143376=CARTESIAN_POINT('Ctrl Pts',(3.84710448405839,4.43126318491329,6.43815220901676));
#143377=CARTESIAN_POINT('Ctrl Pts',(3.85062248811679,4.43191729082659,6.43605264003352));
#143378=CARTESIAN_POINT('Ctrl Pts',(3.231813931,4.301266351,6.489828867));
#143379=CARTESIAN_POINT('Ctrl Pts',(3.585333593,4.365380951,6.313782657));
#143380=CARTESIAN_POINT('Ctrl Pts',(3.917638724,4.430609079,6.100377597));
#143381=CARTESIAN_POINT('Ctrl Pts',(3.92097107091642,4.43126318491329,6.09823757679779));
#143382=CARTESIAN_POINT('Ctrl Pts',(3.92430341783284,4.43191729082659,6.09609755659558));
#143383=CARTESIAN_POINT('',(3.84358647165648,4.43060908007268,6.44025177936701));
#143384=CARTESIAN_POINT('',(3.88061258553502,4.43060908208283,6.27031469768996));
#143385=CARTESIAN_POINT('',(3.34868691448851,4.34096089503725,6.71090872740062));
#143386=CARTESIAN_POINT('Origin',(-0.112447375425123,4.5534906635389,-0.150063190805616));
#143387=CARTESIAN_POINT('Ctrl Pts',(3.23600613130859,4.30202682662047,6.48773953814593));
#143388=CARTESIAN_POINT('Ctrl Pts',(3.25486355746509,4.30883437577991,6.524828917158));
#143389=CARTESIAN_POINT('Ctrl Pts',(3.27368957563181,4.3154778426473,6.561993953406));
#143390=CARTESIAN_POINT('Ctrl Pts',(3.31124009666575,4.32844538546329,6.63637254221788));
#143391=CARTESIAN_POINT('Ctrl Pts',(3.32998686152247,4.33477714735077,6.67363020876695));
#143392=CARTESIAN_POINT('Ctrl Pts',(3.34868691534333,4.34096089503295,6.71090872692928));
#143393=CARTESIAN_POINT('Ctrl Pts',(2.8231120869345,4.43188407004788,6.94838862489945));
#143394=CARTESIAN_POINT('Ctrl Pts',(2.82688340296725,4.43124657452394,6.94685157544973));
#143395=CARTESIAN_POINT('Ctrl Pts',(2.830654719,4.430609079,6.945314526));
#143396=CARTESIAN_POINT('Ctrl Pts',(2.836683105,4.429590053,6.942857578));
#143397=CARTESIAN_POINT('Ctrl Pts',(2.842707217,4.428571429,6.940390168));
#143398=CARTESIAN_POINT('Ctrl Pts',(3.21571972,4.365498301,6.787608363));
#143399=CARTESIAN_POINT('Ctrl Pts',(3.570208235,4.301245526,6.595726886));
#143400=CARTESIAN_POINT('Ctrl Pts',(2.50726090509375,4.43188407004788,6.80266159234725));
#143401=CARTESIAN_POINT('Ctrl Pts',(2.51095327754687,4.43124657452394,6.80129613617363));
#143402=CARTESIAN_POINT('Ctrl Pts',(2.51464565,4.430609079,6.79993068000001));
#143403=CARTESIAN_POINT('Ctrl Pts',(2.520547846,4.429590053,6.797748021));
#143404=CARTESIAN_POINT('Ctrl Pts',(2.526446244,4.428571429,6.795555119));
#143405=CARTESIAN_POINT('Ctrl Pts',(2.891674563,4.365498301,6.659770816));
#143406=CARTESIAN_POINT('Ctrl Pts',(3.240245538,4.301245526,6.485623243));
#143407=CARTESIAN_POINT('',(2.83065472529914,4.4306090808884,6.94531452062695));
#143408=CARTESIAN_POINT('Origin',(-0.106263705412877,4.16161698010819,-0.149107937770643));
#143409=CARTESIAN_POINT('',(2.67265020052035,4.43060908179129,6.87262259676995));
#143410=CARTESIAN_POINT('Origin',(1.00830802041152E-13,4.52171037000067,
1.05384451165591E-13));
#143411=CARTESIAN_POINT('',(3.34284868628253,4.52063234082776,6.71381878362209));
#143412=CARTESIAN_POINT('Origin',(-0.0558087578785244,4.69624333376681,
-0.174753222616125));
#143413=CARTESIAN_POINT('Origin',(-0.0902493206332439,4.55356364651545,
-0.1693702105606));
#143414=CARTESIAN_POINT('Ctrl Pts',(1.582284951,4.301266351,7.331191877));
#143415=CARTESIAN_POINT('Ctrl Pts',(1.981636079,4.365380951,7.24500026));
#143416=CARTESIAN_POINT('Ctrl Pts',(2.369261804,4.430609079,7.115939748));
#143417=CARTESIAN_POINT('Ctrl Pts',(2.37314890434522,4.43126318491329,7.1146455326567));
#143418=CARTESIAN_POINT('Ctrl Pts',(2.37703600469045,4.43191729082659,7.11335131731341));
#143419=CARTESIAN_POINT('Ctrl Pts',(1.761134548,4.301266351,7.032844738));
#143420=CARTESIAN_POINT('Ctrl Pts',(2.144233849,4.365380951,6.936910668));
#143421=CARTESIAN_POINT('Ctrl Pts',(2.51464565,4.430609079,6.79993068));
#143422=CARTESIAN_POINT('Ctrl Pts',(2.51836012957832,4.43126318491329,6.79855704836437));
#143423=CARTESIAN_POINT('Ctrl Pts',(2.52207460915663,4.43191729082659,6.79718341672875));
#143424=CARTESIAN_POINT('',(2.36926179550939,4.43060908007261,7.11593974757192));
#143425=CARTESIAN_POINT('',(2.44195370872942,4.43060908208283,6.95793522041224));
#143426=CARTESIAN_POINT('',(1.82774947215013,4.34096089505207,7.27388011084953));
#143427=CARTESIAN_POINT('Origin',(-0.0775593168197178,4.55349067875258,
-0.170727809510166));
#143428=CARTESIAN_POINT('Ctrl Pts',(1.76567788092872,4.30202682669698,7.0317054563247));
#143429=CARTESIAN_POINT('Ctrl Pts',(1.77612131104473,4.30883437583179,7.07198149539299));
#143430=CARTESIAN_POINT('Ctrl Pts',(1.7865178033652,4.31547784268845,7.11232467109287));
#143431=CARTESIAN_POINT('Ctrl Pts',(1.80720122363574,4.32844539001279,7.19303660981282));
#143432=CARTESIAN_POINT('Ctrl Pts',(1.81750041065261,4.33477715653016,7.23345324471115));
#143433=CARTESIAN_POINT('Ctrl Pts',(1.82774947305039,4.34096089504731,7.27388011060104));
#143434=CARTESIAN_POINT('Ctrl Pts',(1.26341113293498,4.43188407004788,7.39282480932989));
#143435=CARTESIAN_POINT('Ctrl Pts',(1.26742469796749,4.43124657452394,7.39213441616495));
#143436=CARTESIAN_POINT('Ctrl Pts',(1.271438263,4.430609079,7.391444023));
#143437=CARTESIAN_POINT('Ctrl Pts',(1.27785388,4.429590053,7.39034044099999));
#143438=CARTESIAN_POINT('Ctrl Pts',(1.284267572,4.428571429,7.389225724));
#143439=CARTESIAN_POINT('Ctrl Pts',(1.681402823,4.365498301,7.320202535));
#143440=CARTESIAN_POINT('Ctrl Pts',(2.068852438,4.301245526,7.209011693));
#143441=CARTESIAN_POINT('Ctrl Pts',(0.986271382025895,4.43188407004788,
7.18260612530439));
#143442=CARTESIAN_POINT('Ctrl Pts',(0.990170961512947,4.43124657452394,
7.18206634365219));
#143443=CARTESIAN_POINT('Ctrl Pts',(0.994070541000001,4.430609079,7.18152656200001));
#143444=CARTESIAN_POINT('Ctrl Pts',(1.000303954,4.429590053,7.18066373));
#143445=CARTESIAN_POINT('Ctrl Pts',(1.00653586,4.428571429,7.179790078));
#143446=CARTESIAN_POINT('Ctrl Pts',(1.392414954,4.365498301,7.125693629));
#143447=CARTESIAN_POINT('Ctrl Pts',(1.770273114,4.301245526,7.030549986));
#143448=CARTESIAN_POINT('',(1.27143827033362,4.43060908088841,7.39144401914613));
#143449=CARTESIAN_POINT('Origin',(-0.0717255340483477,4.16161688001676,
-0.168465422945171));
#143450=CARTESIAN_POINT('',(1.13275441898507,4.43060908179129,7.28648528985951));
#143451=CARTESIAN_POINT('Origin',(-6.66784336078585E-13,4.52171037000022,
-2.37527011948124E-12));
#143452=CARTESIAN_POINT('',(1.82142216213809,4.5206323408504,7.2754670852764));
#143453=CARTESIAN_POINT('Origin',(-0.0169371445773164,4.69624335525984,
-0.182664612581106));
#143454=CARTESIAN_POINT('Origin',(-0.0517297821939336,4.55356365816114,
-0.184811503839296));
#143455=CARTESIAN_POINT('Ctrl Pts',(-0.030697537,4.301266351,7.499937177));
#143456=CARTESIAN_POINT('Ctrl Pts',(0.377845634,4.365380951,7.50160936));
#143457=CARTESIAN_POINT('Ctrl Pts',(0.784153080000001,4.430609079,7.458894285));
#143458=CARTESIAN_POINT('Ctrl Pts',(0.788227520140971,4.43126318491329,
7.45846593937671));
#143459=CARTESIAN_POINT('Ctrl Pts',(0.792301960281942,4.43191729082659,
7.45803759375342));
#143460=CARTESIAN_POINT('Ctrl Pts',(0.208106472,4.301266351,7.247012605));
#143461=CARTESIAN_POINT('Ctrl Pts',(0.602872113,4.365380951,7.235676446));
#143462=CARTESIAN_POINT('Ctrl Pts',(0.994070541,4.430609079,7.181526562));
#143463=CARTESIAN_POINT('Ctrl Pts',(0.99799346831482,4.43126318491329,7.1809835484196));
#143464=CARTESIAN_POINT('Ctrl Pts',(1.00191639562964,4.43191729082659,7.18044053483919));
#143465=CARTESIAN_POINT('',(0.784153071844491,4.43060908007267,7.45889428273967));
#143466=CARTESIAN_POINT('',(0.88911179127818,4.43060908208281,7.32021042583468));
#143467=CARTESIAN_POINT('',(0.221348495881175,4.34096089505548,7.49673294460434));
#143468=CARTESIAN_POINT('Origin',(-0.0390445919689369,4.55349070825684,
-0.183409434825865));
#143469=CARTESIAN_POINT('Ctrl Pts',(0.21278849589644,4.30202682676222,7.24687664212485));
#143470=CARTESIAN_POINT('Ctrl Pts',(0.214329606545709,4.30883437589522,
7.28845607848061));
#143471=CARTESIAN_POINT('Ctrl Pts',(0.215810444399962,4.31547784270417,
7.33009099135692));
#143472=CARTESIAN_POINT('Ctrl Pts',(0.218659615826445,4.32844538543538,
7.41336222423957));
#143473=CARTESIAN_POINT('Ctrl Pts',(0.220029630859861,4.33477714733755,
7.4550479288828));
#143474=CARTESIAN_POINT('Ctrl Pts',(0.221348496731302,4.34096089504884,
7.49673294457843));
#143475=CARTESIAN_POINT('Ctrl Pts',(-0.355365520534916,4.43188407004788,
7.49158071955885));
#143476=CARTESIAN_POINT('Ctrl Pts',(-0.351297376267458,4.43124657452394,
7.49176926577943));
#143477=CARTESIAN_POINT('Ctrl Pts',(-0.347229232,4.430609079,7.491957812));
#143478=CARTESIAN_POINT('Ctrl Pts',(-0.340726371,4.429590053,7.4922592));
#143479=CARTESIAN_POINT('Ctrl Pts',(-0.334222997,4.428571429,7.492549298));
#143480=CARTESIAN_POINT('Ctrl Pts',(0.0684653979999999,4.365498301,7.510512173));
#143481=CARTESIAN_POINT('Ctrl Pts',(0.470759401,4.301245526,7.485211125));
#143482=CARTESIAN_POINT('Ctrl Pts',(-0.580835096616911,4.43188407004788,
7.22669998041423));
#143483=CARTESIAN_POINT('Ctrl Pts',(-0.576910649808455,4.43124657452394,
7.22701111220711));
#143484=CARTESIAN_POINT('Ctrl Pts',(-0.572986203,4.430609079,7.227322244));
#143485=CARTESIAN_POINT('Ctrl Pts',(-0.56671304,4.429590053,7.227819583));
#143486=CARTESIAN_POINT('Ctrl Pts',(-0.560439023,4.428571429,7.228306033));
#143487=CARTESIAN_POINT('Ctrl Pts',(-0.17195243,4.365498301,7.258426928));
#143488=CARTESIAN_POINT('Ctrl Pts',(0.217524687,4.301245526,7.246736025));
#143489=CARTESIAN_POINT('',(-0.347229223945432,4.43060908088847,7.49195780997297));
#143490=CARTESIAN_POINT('Origin',(-0.033833535587145,4.16161693833491,-0.179945668173186));
#143491=CARTESIAN_POINT('',(-0.460107700344399,4.43060908179129,7.35964002907253));
#143492=CARTESIAN_POINT('Origin',(-7.78999260930835E-14,4.52171037,-6.21464685268691E-13));
#143493=CARTESIAN_POINT('',(0.214827962322351,4.52063234084998,7.49692263181169));
#143494=CARTESIAN_POINT('Origin',(0.0227263342201872,4.69624336296937,-0.182035181962907));
#143495=CARTESIAN_POINT('Origin',(-0.0107913587415697,4.5535636867977,-0.191610899041212));
#143496=CARTESIAN_POINT('Ctrl Pts',(0.459222278,1.457192641,7.485927791));
#143497=CARTESIAN_POINT('Ctrl Pts',(0.867908719,1.391489877,7.460857029));
#143498=CARTESIAN_POINT('Ctrl Pts',(1.271436929,1.326325889,7.39144425200001));
#143499=CARTESIAN_POINT('Ctrl Pts',(0.206355414,1.457192641,7.247062677));
#143500=CARTESIAN_POINT('Ctrl Pts',(0.602001262,1.391489877,7.235796918));
#143501=CARTESIAN_POINT('Ctrl Pts',(0.994069244,1.326325889,7.181526741));
#143502=CARTESIAN_POINT('',(0.989408722995935,1.327100493755,7.18217031262266));
#143503=CARTESIAN_POINT('Origin',(-0.00146137519289088,1.48213100741133,
-0.19802956343801));
#143504=CARTESIAN_POINT('Ctrl Pts',(1.02275296161726,1.36645689999221,7.42993784454118));
#143505=CARTESIAN_POINT('Ctrl Pts',(1.01715038410679,1.3602037253843,7.38860919103333));
#143506=CARTESIAN_POINT('Ctrl Pts',(1.01156636885775,1.35380222444785,7.34727742039455));
#143507=CARTESIAN_POINT('Ctrl Pts',(1.00045203418451,1.3406937976234,7.26470168845419));
#143508=CARTESIAN_POINT('Ctrl Pts',(0.99491552916717,1.33397958626036,7.22341179540039));
#143509=CARTESIAN_POINT('Ctrl Pts',(0.989408718103665,1.32710049397599,
7.18217031323905));
#143510=CARTESIAN_POINT('Ctrl Pts',(0.774029191421309,1.326318298,7.4604791102964));
#143511=CARTESIAN_POINT('Ctrl Pts',(1.18058200259849,1.391911284,7.41829901202036));
#143512=CARTESIAN_POINT('Ctrl Pts',(1.58014381986716,1.457192641,7.33219034515019));
#143513=CARTESIAN_POINT('Ctrl Pts',(1.59395607906417,1.45944932065418,7.32921369629509));
#143514=CARTESIAN_POINT('Ctrl Pts',(1.60776833826125,1.46170600030836,7.32623704743983));
#143515=CARTESIAN_POINT('Ctrl Pts',(0.984741244,1.326318298,7.182811753));
#143516=CARTESIAN_POINT('Ctrl Pts',(1.376162796,1.391911284,7.129149071));
#143517=CARTESIAN_POINT('Ctrl Pts',(1.759435193,1.457192641,7.033270065));
#143518=CARTESIAN_POINT('Ctrl Pts',(1.77268435110679,1.45944932065418,7.02995567001732));
#143519=CARTESIAN_POINT('Ctrl Pts',(1.78593350921352,1.46170600030836,7.02664127503467));
#143520=CARTESIAN_POINT('Origin',(-0.0291612959423751,1.3392876514148,-0.196987598544058));
#143521=CARTESIAN_POINT('Ctrl Pts',(2.057739109,1.457192641,7.212191744));
#143522=CARTESIAN_POINT('Ctrl Pts',(2.451481215,1.391489877,7.099851618));
#143523=CARTESIAN_POINT('Ctrl Pts',(2.830653465,1.326325889,6.945315037));
#143524=CARTESIAN_POINT('Ctrl Pts',(1.759435193,1.457192641,7.033270065));
#143525=CARTESIAN_POINT('Ctrl Pts',(2.143409256,1.391489877,6.93721553));
#143526=CARTESIAN_POINT('Ctrl Pts',(2.514644423,1.326325889,6.799931134));
#143527=CARTESIAN_POINT('',(2.51023121227607,1.32710049351293,6.80156153103146));
#143528=CARTESIAN_POINT('Origin',(-0.0439977657526675,1.4821309558917,-0.193085713929088));
#143529=CARTESIAN_POINT('Ctrl Pts',(2.59605857473254,1.36645689997716,7.03636837215754));
#143530=CARTESIAN_POINT('Ctrl Pts',(2.58170254353218,1.36020372535455,6.99721034804451));
#143531=CARTESIAN_POINT('Ctrl Pts',(2.56736397060224,1.35380222442514,6.95804528949166));
#143532=CARTESIAN_POINT('Ctrl Pts',(2.53875794295237,1.34069370655608,6.8797888422382));
#143533=CARTESIAN_POINT('Ctrl Pts',(2.52447487737159,1.33397954118742,6.84065475640743));
#143534=CARTESIAN_POINT('Ctrl Pts',(2.51023120578947,1.32710049367512,6.80156153336633));
#143535=CARTESIAN_POINT('Ctrl Pts',(2.35971529781516,1.326318298,7.11966385829024));
#143536=CARTESIAN_POINT('Ctrl Pts',(2.74769565534651,1.391911284,6.99107307035004));
#143537=CARTESIAN_POINT('Ctrl Pts',(3.11940512216234,1.457192641,6.82108359598844));
#143538=CARTESIAN_POINT('Ctrl Pts',(3.13225456683688,1.45944932063809,6.81520731211336));
#143539=CARTESIAN_POINT('Ctrl Pts',(3.14510401151136,1.46170600027619,6.80933102823831));
#143540=CARTESIAN_POINT('Ctrl Pts',(2.505810746,1.326318298,6.803191347));
#143541=CARTESIAN_POINT('Ctrl Pts',(2.876545188,1.391911284,6.66663920500001));
#143542=CARTESIAN_POINT('Ctrl Pts',(3.230245738,1.457192641,6.490609561));
#143543=CARTESIAN_POINT('Ctrl Pts',(3.24247264114429,1.45944932063809,6.48452447742378));
#143544=CARTESIAN_POINT('Ctrl Pts',(3.25469954428865,1.46170600027619,6.47843939384745));
#143545=CARTESIAN_POINT('Origin',(-0.070826101358471,1.33928759921943,-0.186113500958953));
#143546=CARTESIAN_POINT('Ctrl Pts',(3.560038347,1.457192641,6.601221627));
#143547=CARTESIAN_POINT('Ctrl Pts',(3.920425175,1.391489877,6.406865037));
#143548=CARTESIAN_POINT('Ctrl Pts',(4.25751179100001,1.326325889,6.174430609));
#143549=CARTESIAN_POINT('Ctrl Pts',(3.230245738,1.457192641,6.490609561));
#143550=CARTESIAN_POINT('Ctrl Pts',(3.584593815,1.391489877,6.314257655));
#143551=CARTESIAN_POINT('Ctrl Pts',(3.917637623,1.326325889,6.100378304));
#143552=CARTESIAN_POINT('',(3.91367807781615,1.32710049352139,6.10291929359378));
#143553=CARTESIAN_POINT('Origin',(-0.0844767839124982,1.48213098853565,
-0.179113172646292));
#143554=CARTESIAN_POINT('Ctrl Pts',(4.04797537440471,1.3664569000217,6.31378613517479));
#143555=CARTESIAN_POINT('Ctrl Pts',(4.02553716157696,1.36020372539197,6.2786297262122));
#143556=CARTESIAN_POINT('Ctrl Pts',(4.00311448672758,1.35380222447382,6.24346269436484));
#143557=CARTESIAN_POINT('Ctrl Pts',(3.95835474007353,1.34069379762387,6.17318577769116));
#143558=CARTESIAN_POINT('Ctrl Pts',(3.93599276743408,1.33397958600384,6.13803680249688));
#143559=CARTESIAN_POINT('Ctrl Pts',(3.91367807236571,1.32710049371077,6.10291929702005));
#143560=CARTESIAN_POINT('Ctrl Pts',(3.83506373905256,1.326318298,6.44594103746665));
#143561=CARTESIAN_POINT('Ctrl Pts',(4.18633011316466,1.391911284,6.23695232226448));
#143562=CARTESIAN_POINT('Ctrl Pts',(4.51280650719234,1.457192641,5.99103056004904));
#143563=CARTESIAN_POINT('Ctrl Pts',(4.52409231142524,1.45944932059043,5.98252940984112));
#143564=CARTESIAN_POINT('Ctrl Pts',(4.53537811565822,1.46170600018087,5.97402825963307));
#143565=CARTESIAN_POINT('Ctrl Pts',(3.909711322,1.326318298,6.105461275));
#143566=CARTESIAN_POINT('Ctrl Pts',(4.242423525,1.391911284,5.8924047));
#143567=CARTESIAN_POINT('Ctrl Pts',(4.550013582,1.457192641,5.644455368));
#143568=CARTESIAN_POINT('Ctrl Pts',(4.56064651360178,1.45944932059043,5.63588412771487));
#143569=CARTESIAN_POINT('Ctrl Pts',(4.57127944520359,1.46170600018087,5.62731288742987));
#143570=CARTESIAN_POINT('Origin',(-0.109179050594557,1.33928761673774,-0.166536633005492));
#143571=CARTESIAN_POINT('Ctrl Pts',(4.895874148,1.457192641,5.681585723));
#143572=CARTESIAN_POINT('Ctrl Pts',(5.20605441,1.391489877,5.414300567));
#143573=CARTESIAN_POINT('Ctrl Pts',(5.485293597,1.326325889,5.114836669));
#143574=CARTESIAN_POINT('Ctrl Pts',(4.550013582,1.457192641,5.644455368));
#143575=CARTESIAN_POINT('Ctrl Pts',(4.858166752,1.391489877,5.396052109));
#143576=CARTESIAN_POINT('Ctrl Pts',(5.137446442,1.326325889,5.115578565));
#143577=CARTESIAN_POINT('',(5.1341257059355,1.32710049403695,5.11891133457276));
#143578=CARTESIAN_POINT('Origin',(-0.121005727499927,1.48213091705073,-0.156765495076171));
#143579=CARTESIAN_POINT('Ctrl Pts',(5.3106133446011,1.36645689999546,5.29597827577827));
#143580=CARTESIAN_POINT('Ctrl Pts',(5.2811421360205,1.3602037253731,5.26646735662183));
#143581=CARTESIAN_POINT('Ctrl Pts',(5.25168381839431,1.35380222443046,5.23694272258867));
#143582=CARTESIAN_POINT('Ctrl Pts',(5.19286307008215,1.34069379760127,5.17793086369866));
#143583=CARTESIAN_POINT('Ctrl Pts',(5.1634679179709,1.33397958614789,5.14841081584665));
#143584=CARTESIAN_POINT('Ctrl Pts',(5.13412570249903,1.3271004938692,5.11891133803002));
#143585=CARTESIAN_POINT('Ctrl Pts',(5.13108886245636,1.326318298,5.47081317818938));
#143586=CARTESIAN_POINT('Ctrl Pts',(5.42921642824446,1.391911284,5.19119861552024));
#143587=CARTESIAN_POINT('Ctrl Pts',(5.69519407555067,1.457192641,4.88084359396323));
#143588=CARTESIAN_POINT('Ctrl Pts',(5.70438852798741,1.45944932060455,4.87011508157465));
#143589=CARTESIAN_POINT('Ctrl Pts',(5.71358298042421,1.46170600020911,4.85938656918593));
#143590=CARTESIAN_POINT('Ctrl Pts',(5.13079814199999,1.326318298,5.122246619));
#143591=CARTESIAN_POINT('Ctrl Pts',(5.409930853,1.391911284,4.8426479));
#143592=CARTESIAN_POINT('Ctrl Pts',(5.657027848,1.457192641,4.534372715));
#143593=CARTESIAN_POINT('Ctrl Pts',(5.66556962431392,1.45944932060455,4.52371609947377));
#143594=CARTESIAN_POINT('Ctrl Pts',(5.67411140062787,1.46170600020911,4.51305948394751));
#143595=CARTESIAN_POINT('Origin',(-0.142426822481519,1.33928760589289,-0.139172707724181));
#143596=CARTESIAN_POINT('Ctrl Pts',(6.002784315,1.457192641,4.496285186));
#143597=CARTESIAN_POINT('Ctrl Pts',(6.24825432699999,1.391489877,4.16856942));
#143598=CARTESIAN_POINT('Ctrl Pts',(6.456589172,1.326325889,3.816078651));
#143599=CARTESIAN_POINT('Ctrl Pts',(5.657027848,1.457192641,4.534372715));
#143600=CARTESIAN_POINT('Ctrl Pts',(5.90457721,1.391489877,4.225533165));
#143601=CARTESIAN_POINT('Ctrl Pts',(6.117033975,1.326325889,3.891580058));
#143602=CARTESIAN_POINT('',(6.114507322733,1.32710049408698,3.89554876943617));
#143603=CARTESIAN_POINT('Origin',(-0.151876474541786,1.48213096602352,-0.12708765510772));
#143604=CARTESIAN_POINT('Ctrl Pts',(6.3249329372562,1.36645689998677,4.03053635825672));
#143605=CARTESIAN_POINT('Ctrl Pts',(6.28980677379601,1.36020372535361,4.00805082670748));
#143606=CARTESIAN_POINT('Ctrl Pts',(6.25469025164565,1.35380222441028,3.98554912980152));
#143607=CARTESIAN_POINT('Ctrl Pts',(6.18455889429005,1.34069379758154,3.94056165765489));
#143608=CARTESIAN_POINT('Ctrl Pts',(6.14950504670855,1.33397958613157,3.91805086095089));
#143609=CARTESIAN_POINT('Ctrl Pts',(6.11450732013077,1.32710049387763,3.89554877354745));
#143610=CARTESIAN_POINT('Ctrl Pts',(6.18718997383337,1.326318298,4.23987617474291));
#143611=CARTESIAN_POINT('Ctrl Pts',(6.41823861689965,1.391911284,3.90271023113778));
#143612=CARTESIAN_POINT('Ctrl Pts',(6.61128069909955,1.457192641,3.54243380476249));
#143613=CARTESIAN_POINT('Ctrl Pts',(6.61795387734748,1.45944932061391,3.52997958346355));
#143614=CARTESIAN_POINT('Ctrl Pts',(6.62462705559532,1.46170600022782,3.51752536216457));
#143615=CARTESIAN_POINT('Ctrl Pts',(6.111974543,1.326318298,3.899521405));
#143616=CARTESIAN_POINT('Ctrl Pts',(6.324475827,1.391911284,3.566454266));
#143617=CARTESIAN_POINT('Ctrl Pts',(6.49952578000001,1.457192641,3.212267834));
#143618=CARTESIAN_POINT('Ctrl Pts',(6.50557699704731,1.45944932061391,3.20002413476719));
#143619=CARTESIAN_POINT('Ctrl Pts',(6.51162821409463,1.46170600022782,3.1877804355344));
#143620=CARTESIAN_POINT('Origin',(-0.169015122135372,1.33928762967766,-0.105301451691872));
#143621=CARTESIAN_POINT('Ctrl Pts',(6.829010959,1.457192641,3.10074335));
#143622=CARTESIAN_POINT('Ctrl Pts',(6.998292817,1.391489877,2.7279206));
#143623=CARTESIAN_POINT('Ctrl Pts',(7.125981812,1.326325889,2.338885036));
#143624=CARTESIAN_POINT('Ctrl Pts',(6.49952578,1.457192641,3.212267834));
#143625=CARTESIAN_POINT('Ctrl Pts',(6.674896201,1.391489877,2.857432985));
#143626=CARTESIAN_POINT('Ctrl Pts',(6.81059579800001,1.326325889,2.485615592));
#143627=CARTESIAN_POINT('',(6.80898137381432,1.3271004938241,2.49003467323014));
#143628=CARTESIAN_POINT('Origin',(-0.1756460283872,1.48213098434334,-0.0914675728584302));
#143629=CARTESIAN_POINT('Ctrl Pts',(7.04350569533385,1.3664569000354,2.57663104013053));
#143630=CARTESIAN_POINT('Ctrl Pts',(7.00436703759397,1.36020372542726,2.56222229464034));
#143631=CARTESIAN_POINT('Ctrl Pts',(6.96523432048731,1.35380222447523,2.54779568903774));
#143632=CARTESIAN_POINT('Ctrl Pts',(6.88707161862786,1.34069379763287,2.51893616756175));
#143633=CARTESIAN_POINT('Ctrl Pts',(6.84799815522327,1.33397958626634,2.50448720190976));
#143634=CARTESIAN_POINT('Ctrl Pts',(6.80898137228227,1.32710049396137,2.4900346773008));
#143635=CARTESIAN_POINT('Ctrl Pts',(6.95398495829248,1.326318298,2.8106872738861));
#143636=CARTESIAN_POINT('Ctrl Pts',(7.10715110139082,1.391911284,2.43173545452953));
#143637=CARTESIAN_POINT('Ctrl Pts',(7.21823118476806,1.457192641,2.03838374950821));
#143638=CARTESIAN_POINT('Ctrl Pts',(7.22207105844789,1.45944932065765,2.02478616465678));
#143639=CARTESIAN_POINT('Ctrl Pts',(7.22591093212768,1.4617060003153,2.01118857980531));
#143640=CARTESIAN_POINT('Ctrl Pts',(6.807361808,1.326318298,2.494458903));
#143641=CARTESIAN_POINT('Ctrl Pts',(6.94329534,1.391911284,2.123497195));
#143642=CARTESIAN_POINT('Ctrl Pts',(7.038113109,1.457192641,1.739960879));
#143643=CARTESIAN_POINT('Ctrl Pts',(7.04139081859919,1.45944932065765,1.72670259758457));
#143644=CARTESIAN_POINT('Ctrl Pts',(7.04466852819825,1.4617060003153,1.71344431616913));
#143645=CARTESIAN_POINT('Origin',(-0.187700324234343,1.33928758702522,-0.0665063034962282));
#143646=CARTESIAN_POINT('Ctrl Pts',(7.335920641,1.457192641,1.560214201));
#143647=CARTESIAN_POINT('Ctrl Pts',(7.421098912,1.391489877,1.159717245));
#143648=CARTESIAN_POINT('Ctrl Pts',(7.462171463,1.326325889,0.752327757));
#143649=CARTESIAN_POINT('Ctrl Pts',(7.038113109,1.457192641,1.739960879));
#143650=CARTESIAN_POINT('Ctrl Pts',(7.133104463,1.391489877,1.355722415));
#143651=CARTESIAN_POINT('Ctrl Pts',(7.18570173100001,1.326325889,0.963426504000001));
#143652=CARTESIAN_POINT('',(7.18507502296379,1.3271004938514,0.968089323470228));
#143653=CARTESIAN_POINT('Origin',(-0.19120240727187,1.48213096794108,-0.0515704215217526));
#143654=CARTESIAN_POINT('Ctrl Pts',(7.43273195510903,1.36645690001734,1.00224531859331));
#143655=CARTESIAN_POINT('Ctrl Pts',(7.39141088307187,1.36020372540559,0.996587095984889));
#143656=CARTESIAN_POINT('Ctrl Pts',(7.35009177350989,1.35380222447435,0.990910153806536));
#143657=CARTESIAN_POINT('Ctrl Pts',(7.26755252815035,1.34069379764965,0.979528022357111));
#143658=CARTESIAN_POINT('Ctrl Pts',(7.22628648016009,1.33397958630851,0.973816505192048));
#143659=CARTESIAN_POINT('Ctrl Pts',(7.18507502234315,1.32710049402831,0.968089327723748));
#143660=CARTESIAN_POINT('Ctrl Pts',(7.39561933502153,1.326318298,1.25007375973625));
#143661=CARTESIAN_POINT('Ctrl Pts',(7.46374109865892,1.391911284,0.847055430001511));
#143662=CARTESIAN_POINT('Ctrl Pts',(7.48766520227525,1.457192641,0.439021134686234));
#143663=CARTESIAN_POINT('Ctrl Pts',(7.48849222302968,1.45944932062251,0.424915994691601));
#143664=CARTESIAN_POINT('Ctrl Pts',(7.48931924378424,1.46170600024503,0.410810854696974));
#143665=CARTESIAN_POINT('Ctrl Pts',(7.1844444,1.326318298,0.972758276));
#143666=CARTESIAN_POINT('Ctrl Pts',(7.23745408,1.391911284,0.581247754));
#143667=CARTESIAN_POINT('Ctrl Pts',(7.247606092,1.457192641,0.186295287));
#143668=CARTESIAN_POINT('Ctrl Pts',(7.24795703198746,1.45944932062251,0.172642366394501));
#143669=CARTESIAN_POINT('Ctrl Pts',(7.24830797197507,1.46170600024503,0.158989445789));
#143670=CARTESIAN_POINT('Origin',(-0.197608983519719,1.33928764106773,-0.0246014040886011));
#143671=CARTESIAN_POINT('Ctrl Pts',(7.49981082600001,1.457192641,-0.053268829));
#143672=CARTESIAN_POINT('Ctrl Pts',(7.49690267000001,1.391489877,-0.462713199));
#143673=CARTESIAN_POINT('Ctrl Pts',(7.44943827,1.326325889,-0.869407533));
#143674=CARTESIAN_POINT('Ctrl Pts',(7.247606092,1.457192641,0.186295287));
#143675=CARTESIAN_POINT('Ctrl Pts',(7.25777669,1.391489877,-0.209380228));
#143676=CARTESIAN_POINT('Ctrl Pts',(7.224812238,1.326325889,-0.603811336));
#143677=CARTESIAN_POINT('',(7.22520254927648,1.32710049375089,-0.599122808396091));
#143678=CARTESIAN_POINT('Origin',(-0.197818010397776,1.48213094674485,-0.00926186906210269));
#143679=CARTESIAN_POINT('Ctrl Pts',(7.47441192954955,1.3664568999685,-0.619004280640579));
#143680=CARTESIAN_POINT('Ctrl Pts',(7.43284057059421,1.36020372535515,-0.615647407941441));
#143681=CARTESIAN_POINT('Ctrl Pts',(7.39126710412496,1.35380222442509,-0.612309239020518));
#143682=CARTESIAN_POINT('Ctrl Pts',(7.3082107589293,1.340693797625,-0.605681764288891));
#143683=CARTESIAN_POINT('Ctrl Pts',(7.26668168012318,1.33397958614964,-0.60238876858733));
#143684=CARTESIAN_POINT('Ctrl Pts',(7.22520254972496,1.32710049389312,-0.599122802400566));
#143685=CARTESIAN_POINT('Ctrl Pts',(7.49144277026383,1.326318298,-0.36899181485995));
#143686=CARTESIAN_POINT('Ctrl Pts',(7.47133485840931,1.391911284,-0.77723196544628));
#143687=CARTESIAN_POINT('Ctrl Pts',(7.40698431742458,1.457192641,-1.18086962076664));
#143688=CARTESIAN_POINT('Ctrl Pts',(7.4047598146672,1.45944932068645,-1.19482277583736));
#143689=CARTESIAN_POINT('Ctrl Pts',(7.4025353119098,1.4617060003729,-1.20877593090805));
#143690=CARTESIAN_POINT('Ctrl Pts',(7.225590357,1.326318298,-0.594427447));
#143691=CARTESIAN_POINT('Ctrl Pts',(7.193197511,1.391911284,-0.988180185000001));
#143692=CARTESIAN_POINT('Ctrl Pts',(7.118209069,1.457192641,-1.376081265));
#143693=CARTESIAN_POINT('Ctrl Pts',(7.11561682978261,1.45944932068645,-1.38949043000231));
#143694=CARTESIAN_POINT('Ctrl Pts',(7.11302459056518,1.4617060003729,-1.40289959500463));
#143695=CARTESIAN_POINT('Origin',(-0.198277551705002,1.33928765473254,0.0184538507370688));
#143696=CARTESIAN_POINT('Ctrl Pts',(7.313018193,1.457192641,-1.664261068));
#143697=CARTESIAN_POINT('Ctrl Pts',(7.222159592,1.391489877,-2.063507689));
#143698=CARTESIAN_POINT('Ctrl Pts',(7.088377623,1.326325889,-2.450490292));
#143699=CARTESIAN_POINT('Ctrl Pts',(7.118209069,1.457192641,-1.376081265));
#143700=CARTESIAN_POINT('Ctrl Pts',(7.043083344,1.391489877,-1.764692484));
#143701=CARTESIAN_POINT('Ctrl Pts',(6.926098554,1.326325889,-2.14281563));
#143702=CARTESIAN_POINT('',(6.92748763502108,1.32710049371206,-2.13832062223762));
#143703=CARTESIAN_POINT('Origin',(-0.195184343043897,1.48213097566634,0.0334797327397524));
#143704=CARTESIAN_POINT('Ctrl Pts',(7.16659670980258,1.36645689998385,-2.21130992726238));
#143705=CARTESIAN_POINT('Ctrl Pts',(7.12671889445975,1.36020372536164,-2.19909492311465));
#143706=CARTESIAN_POINT('Ctrl Pts',(7.08683500011182,1.35380222442229,-2.18689773242826));
#143707=CARTESIAN_POINT('Ctrl Pts',(7.00714461066936,1.34069370442274,-2.16257037256327));
#143708=CARTESIAN_POINT('Ctrl Pts',(6.96729465666842,1.33397954030356,-2.15042693333813));
#143709=CARTESIAN_POINT('Ctrl Pts',(6.92748763645859,1.32710049384016,-2.13832061743811));
#143710=CARTESIAN_POINT('Ctrl Pts',(7.23697466922751,1.326318298,-1.97080374093117));
#143711=CARTESIAN_POINT('Ctrl Pts',(7.12957730341818,1.391911284,-2.36517685756174));
#143712=CARTESIAN_POINT('Ctrl Pts',(6.97996107817798,1.457192641,-2.74554422463716));
#143713=CARTESIAN_POINT('Ctrl Pts',(6.97478906730758,1.45944932063149,-2.75869296003741));
#143714=CARTESIAN_POINT('Ctrl Pts',(6.96961705643702,1.46170600026299,-2.77184169543771));
#143715=CARTESIAN_POINT('Ctrl Pts',(6.92887574,1.326318298,-2.133818404));
#143716=CARTESIAN_POINT('Ctrl Pts',(6.812595022,1.391911284,-2.511401917));
#143717=CARTESIAN_POINT('Ctrl Pts',(6.655972501,1.457192641,-2.874113787));
#143718=CARTESIAN_POINT('Ctrl Pts',(6.65055829288275,1.45944932063149,-2.88665219806779));
#143719=CARTESIAN_POINT('Ctrl Pts',(6.64514408476563,1.46170600026299,-2.89919060913559));
#143720=CARTESIAN_POINT('Origin',(-0.189674642281049,1.33928762627356,0.060646127450637));
#143721=CARTESIAN_POINT('Ctrl Pts',(6.784276957,1.457192641,-3.19743431));
#143722=CARTESIAN_POINT('Ctrl Pts',(6.609716357,1.391489877,-3.567814853));
#143723=CARTESIAN_POINT('Ctrl Pts',(6.395872317,1.326325889,-3.916990849));
#143724=CARTESIAN_POINT('Ctrl Pts',(6.655972501,1.457192641,-2.874113787));
#143725=CARTESIAN_POINT('Ctrl Pts',(6.499063249,1.391489877,-3.237489682));
#143726=CARTESIAN_POINT('Ctrl Pts',(6.303528199,1.326325889,-3.581624247));
#143727=CARTESIAN_POINT('',(6.30585109648612,1.32710049348248,-3.57753294181973));
#143728=CARTESIAN_POINT('Origin',(-0.183423798973755,1.48213096027346,0.0746558163728089));
#143729=CARTESIAN_POINT('Ctrl Pts',(6.5236793927374,1.36645690002517,-3.7002171795176));
#143730=CARTESIAN_POINT('Ctrl Pts',(6.48735976337419,1.36020372540054,-3.67971520379541));
#143731=CARTESIAN_POINT('Ctrl Pts',(6.45103036781519,1.35380222447272,-3.65922931830479));
#143732=CARTESIAN_POINT('Ctrl Pts',(6.37843277317963,1.34069370711926,-3.61833964867325));
#143733=CARTESIAN_POINT('Ctrl Pts',(6.34212496075972,1.33397954151097,-3.59791354930418));
#143734=CARTESIAN_POINT('Ctrl Pts',(6.30585109973058,1.32710049377457,-3.57753293594657));
#143735=CARTESIAN_POINT('Ctrl Pts',(6.64411367475974,1.326318298,-3.48046307510353));
#143736=CARTESIAN_POINT('Ctrl Pts',(6.45444863851167,1.391911284,-3.8425287080016));
#143737=CARTESIAN_POINT('Ctrl Pts',(6.22656261649628,1.457192641,-4.18184023157355));
#143738=CARTESIAN_POINT('Ctrl Pts',(6.21868493465476,1.45944932070366,-4.19356972776744));
#143739=CARTESIAN_POINT('Ctrl Pts',(6.21080725281313,1.46170600040732,-4.20529922396129));
#143740=CARTESIAN_POINT('Ctrl Pts',(6.30817459400001,1.326318298,-3.573434383));
#143741=CARTESIAN_POINT('Ctrl Pts',(6.11344316000001,1.391911284,-3.917193286));
#143742=CARTESIAN_POINT('Ctrl Pts',(5.882510057,1.457192641,-4.237755942));
#143743=CARTESIAN_POINT('Ctrl Pts',(5.87452704208746,1.45944932070366,-4.24883731764522));
#143744=CARTESIAN_POINT('Ctrl Pts',(5.86654402717481,1.46170600040732,-4.25991869329037));
#143745=CARTESIAN_POINT('Origin',(-0.172203235305617,1.33928763528297,0.100002826680549));
#143746=CARTESIAN_POINT('Ctrl Pts',(5.938310471,1.457192641,-4.581099076));
#143747=CARTESIAN_POINT('Ctrl Pts',(5.688210133,1.391489877,-4.905294959));
#143748=CARTESIAN_POINT('Ctrl Pts',(5.404303129,1.326325889,-5.200337267));
#143749=CARTESIAN_POINT('Ctrl Pts',(5.882510057,1.457192641,-4.237755942));
#143750=CARTESIAN_POINT('Ctrl Pts',(5.65115418,1.391489877,-4.55890546));
#143751=CARTESIAN_POINT('Ctrl Pts',(5.386211872,1.326325889,-4.852960094));
#143752=CARTESIAN_POINT('',(5.38935997065952,1.32710049350691,-4.84946379609861));
#143753=CARTESIAN_POINT('Origin',(-0.163086630338602,1.48213094494524,0.112341076983529));
#143754=CARTESIAN_POINT('Ctrl Pts',(5.57572207796247,1.36645689999479,-5.01610638889124));
#143755=CARTESIAN_POINT('Ctrl Pts',(5.54465890009331,1.36020372537892,-4.98827609134551));
#143756=CARTESIAN_POINT('Ctrl Pts',(5.51358272538254,1.35380222444491,-4.96045940835782));
#143757=CARTESIAN_POINT('Ctrl Pts',(5.45147292145161,1.34069379762287,-4.90491976336936));
#143758=CARTESIAN_POINT('Ctrl Pts',(5.42040474501485,1.33397958598093,-4.87716590416787));
#143759=CARTESIAN_POINT('Ctrl Pts',(5.38935997523652,1.32710049369691,-4.84946379111753));
#143760=CARTESIAN_POINT('Ctrl Pts',(5.74058131055227,1.326318298,-4.82737982414743));
#143761=CARTESIAN_POINT('Ctrl Pts',(5.47751712737932,1.391911284,-5.14020818726269));
#143762=CARTESIAN_POINT('Ctrl Pts',(5.18201700780785,1.457192641,-5.42259803764836));
#143763=CARTESIAN_POINT('Ctrl Pts',(5.17180200742665,1.4594493205831,-5.43235983548967));
#143764=CARTESIAN_POINT('Ctrl Pts',(5.16158700704535,1.46170600016621,-5.442121633331));
#143765=CARTESIAN_POINT('Ctrl Pts',(5.392510215,1.326318298,-4.845960543));
#143766=CARTESIAN_POINT('Ctrl Pts',(5.12843349100001,1.391911284,-5.139821051));
#143767=CARTESIAN_POINT('Ctrl Pts',(4.833987981,1.457192641,-5.40324534));
#143768=CARTESIAN_POINT('Ctrl Pts',(4.82380943690582,1.4594493205831,-5.41235152654387));
#143769=CARTESIAN_POINT('Ctrl Pts',(4.81363089281152,1.46170600016621,-5.42145771308775));
#143770=CARTESIAN_POINT('Origin',(-0.146679738616158,1.33928761876399,0.134683584452131));
#143771=CARTESIAN_POINT('Ctrl Pts',(4.814675187,1.457192641,-5.750556742));
#143772=CARTESIAN_POINT('Ctrl Pts',(4.500729524,1.391489877,-6.013408925));
#143773=CARTESIAN_POINT('Ctrl Pts',(4.160034734,1.326325889,-6.240521694));
#143774=CARTESIAN_POINT('Ctrl Pts',(4.833987981,1.457192641,-5.40324534));
#143775=CARTESIAN_POINT('Ctrl Pts',(4.539003422,1.391489877,-5.667151885));
#143776=CARTESIAN_POINT('Ctrl Pts',(4.217042264,1.326325889,-5.897376921));
#143777=CARTESIAN_POINT('',(4.22086836503791,1.32710049374625,-5.89463911253408));
#143778=CARTESIAN_POINT('Origin',(-0.135123900040557,1.48213095657849,0.144773612127819));
#143779=CARTESIAN_POINT('Ctrl Pts',(4.36705019565857,1.36645689997344,-6.09744803840908));
#143780=CARTESIAN_POINT('Ctrl Pts',(4.34269594892901,1.3602037253429,-6.06359073269705));
#143781=CARTESIAN_POINT('Ctrl Pts',(4.31832608257802,1.35380222442097,-6.02974392943819));
#143782=CARTESIAN_POINT('Ctrl Pts',(4.2696074112792,1.34069370556785,-5.96215052401912));
#143783=CARTESIAN_POINT('Ctrl Pts',(4.24523203343021,1.33397954092168,-5.92836704876963));
#143784=CARTESIAN_POINT('Ctrl Pts',(4.22086836888483,1.32710049390968,-5.89463910972189));
#143785=CARTESIAN_POINT('Ctrl Pts',(4.56862574298837,1.326318298,-5.94857365764973));
#143786=CARTESIAN_POINT('Ctrl Pts',(4.24446300427209,1.391911284,-6.19753724418813));
#143787=CARTESIAN_POINT('Ctrl Pts',(3.89516604182185,1.457192641,-6.40980118682283));
#143788=CARTESIAN_POINT('Ctrl Pts',(3.88309136437659,1.45944932059846,-6.41713883620456));
#143789=CARTESIAN_POINT('Ctrl Pts',(3.87101668693131,1.46170600019692,-6.42447648558641));
#143790=CARTESIAN_POINT('Ctrl Pts',(4.224698052,1.326318298,-5.891894973));
#143791=CARTESIAN_POINT('Ctrl Pts',(3.903623972,1.391911284,-6.122116497));
#143792=CARTESIAN_POINT('Ctrl Pts',(3.559433999,1.457192641,-6.316084991));
#143793=CARTESIAN_POINT('Ctrl Pts',(3.54753586259849,1.45944932059845,-6.32279019388286));
#143794=CARTESIAN_POINT('Ctrl Pts',(3.53563772619695,1.46170600019692,-6.32949539676568));
#143795=CARTESIAN_POINT('Origin',(-0.114297347719498,1.33928765193469,0.163066399485854));
#143796=CARTESIAN_POINT('Ctrl Pts',(3.465911043,1.457192641,-6.651124765));
#143797=CARTESIAN_POINT('Ctrl Pts',(3.102799805,1.391489877,-6.840342573));
#143798=CARTESIAN_POINT('Ctrl Pts',(2.721247738,1.326325889,-6.988906263));
#143799=CARTESIAN_POINT('Ctrl Pts',(3.559433999,1.457192641,-6.316084991));
#143800=CARTESIAN_POINT('Ctrl Pts',(3.214613909,1.391489877,-6.510408587));
#143801=CARTESIAN_POINT('Ctrl Pts',(2.850688446,1.326325889,-6.66603895700001));
#143802=CARTESIAN_POINT('',(2.85501364068508,1.32710049349123,-6.66418765582323));
#143803=CARTESIAN_POINT('Origin',(-0.100842727121628,1.48213099008862,0.170436515317088));
#143804=CARTESIAN_POINT('Ctrl Pts',(2.95417989991179,1.36645689997307,-6.89367979481652));
#143805=CARTESIAN_POINT('Ctrl Pts',(2.93767336182599,1.36020372535119,-6.85537861096055));
#143806=CARTESIAN_POINT('Ctrl Pts',(2.92114931151543,1.35380222442209,-6.81708432616746));
#143807=CARTESIAN_POINT('Ctrl Pts',(2.88810047152572,1.34069379757943,-6.74059867960663));
#143808=CARTESIAN_POINT('Ctrl Pts',(2.87155730126059,1.3339795860005,-6.70236477081003));
#143809=CARTESIAN_POINT('Ctrl Pts',(2.85501364640299,1.32710049370827,-6.66418765330632));
#143810=CARTESIAN_POINT('Ctrl Pts',(3.18304631452933,1.326318298,-6.79161879846183));
#143811=CARTESIAN_POINT('Ctrl Pts',(2.81294250805842,1.391911284,-6.96507634840551));
#143812=CARTESIAN_POINT('Ctrl Pts',(2.42618144212585,1.457192641,-7.09728915532328));
#143813=CARTESIAN_POINT('Ctrl Pts',(2.41281168597534,1.45944932064318,-7.10185955587329));
#143814=CARTESIAN_POINT('Ctrl Pts',(2.39944192982491,1.46170600028635,-7.10642995642344));
#143815=CARTESIAN_POINT('Ctrl Pts',(2.859343703,1.326318298,-6.662330943));
#143816=CARTESIAN_POINT('Ctrl Pts',(2.496285335,1.391911284,-6.818148579));
#143817=CARTESIAN_POINT('Ctrl Pts',(2.118444839,1.457192641,-6.933591527));
#143818=CARTESIAN_POINT('Ctrl Pts',(2.10538345371521,1.45944932064317,-6.93758221841136));
#143819=CARTESIAN_POINT('Ctrl Pts',(2.09232206843043,1.46170600028635,-6.94157290982255));
#143820=CARTESIAN_POINT('Origin',(-0.0765706498909213,1.33928761153607,
0.183824456529189));
#143821=CARTESIAN_POINT('Ctrl Pts',(1.95508475,1.457192641,-7.240693587));
#143822=CARTESIAN_POINT('Ctrl Pts',(1.559786616,1.391489877,-7.347429405));
#143823=CARTESIAN_POINT('Ctrl Pts',(1.155218222,1.326325889,-7.41049734200001));
#143824=CARTESIAN_POINT('Ctrl Pts',(2.118444839,1.457192641,-6.933591527));
#143825=CARTESIAN_POINT('Ctrl Pts',(1.739912622,1.391489877,-7.049245819));
#143826=CARTESIAN_POINT('Ctrl Pts',(1.351039605,1.326325889,-7.12300442100001));
#143827=CARTESIAN_POINT('',(1.35566165652867,1.3271004937223,-7.12212619180199));
#143828=CARTESIAN_POINT('Origin',(-0.0618462780225851,1.4821309815227,0.18813004085965));
#143829=CARTESIAN_POINT('Ctrl Pts',(1.40317543510778,1.36645689995796,-7.36757074577874));
#143830=CARTESIAN_POINT('Ctrl Pts',(1.39528843307492,1.36020372535873,-7.32661660460976));
#143831=CARTESIAN_POINT('Ctrl Pts',(1.38738284513841,1.35380222441668,-7.28566543635231));
#143832=CARTESIAN_POINT('Ctrl Pts',(1.37154882199612,1.34069379762891,-7.20386345811269));
#143833=CARTESIAN_POINT('Ctrl Pts',(1.36361158243823,1.33397958625016,-7.16296714532754));
#143834=CARTESIAN_POINT('Ctrl Pts',(1.35566166106545,1.32710049399294,-7.1221261908733));
#143835=CARTESIAN_POINT('Ctrl Pts',(1.64863117716275,1.326318298,-7.31709539294675));
#143836=CARTESIAN_POINT('Ctrl Pts',(1.24989194723245,1.391911284,-7.40693622353499));
#143837=CARTESIAN_POINT('Ctrl Pts',(0.843751293891287,1.457192641,-7.452915771864));
#143838=CARTESIAN_POINT('Ctrl Pts',(0.829711613941566,1.45944932067839,
-7.45450521664739));
#143839=CARTESIAN_POINT('Ctrl Pts',(0.81567193399185,1.46170600035678,-7.45609466143078));
#143840=CARTESIAN_POINT('Ctrl Pts',(1.360289621,1.326318298,-7.121243722));
#143841=CARTESIAN_POINT('Ctrl Pts',(0.972223169,1.391911284,-7.195371611));
#143842=CARTESIAN_POINT('Ctrl Pts',(0.578399553,1.457192641,-7.22689103));
#143843=CARTESIAN_POINT('Ctrl Pts',(0.564785654761062,1.45944932067839,
-7.22798060956149));
#143844=CARTESIAN_POINT('Ctrl Pts',(0.55117175652214,1.46170600035678,-7.22907018912286));
#143845=CARTESIAN_POINT('Origin',(-0.0352636698467937,1.33928765144172,
0.195987353699291));
#143846=CARTESIAN_POINT('Ctrl Pts',(0.352840867,1.457192641,-7.491695624));
#143847=CARTESIAN_POINT('Ctrl Pts',(-0.056160462,1.391489877,-7.510958604));
#143848=CARTESIAN_POINT('Ctrl Pts',(-0.464828014,1.326325889,-7.485581802));
#143849=CARTESIAN_POINT('Ctrl Pts',(0.578399553,1.457192641,-7.22689103));
#143850=CARTESIAN_POINT('Ctrl Pts',(0.183854955,1.391489877,-7.258468152));
#143851=CARTESIAN_POINT('Ctrl Pts',(-0.211782346,1.326325889,-7.246906115));
#143852=CARTESIAN_POINT('',(-0.207079563753079,1.32710049360996,-7.24704202119074));
#143853=CARTESIAN_POINT('Origin',(-0.019957948281468,1.48213098225561,0.197026683410473));
#143854=CARTESIAN_POINT('Ctrl Pts',(-0.213439952651145,1.36645689674192,
-7.49696225529675));
#143855=CARTESIAN_POINT('Ctrl Pts',(-0.212338631177845,1.36020372208674,
-7.45527012694911));
#143856=CARTESIAN_POINT('Ctrl Pts',(-0.211256100755129,1.35380222443176,
-7.41357692822774));
#143857=CARTESIAN_POINT('Ctrl Pts',(-0.209134926056559,1.34069379761266,
-7.33028358799617));
#143858=CARTESIAN_POINT('Ctrl Pts',(-0.208095099061949,1.33397958596669,
-7.28863713496509));
#143859=CARTESIAN_POINT('Ctrl Pts',(-0.207079557909248,1.32710049367483,
-7.24704202132269));
#143860=CARTESIAN_POINT('Ctrl Pts',(0.0371278792293957,1.326318298,-7.5004327383073));
#143861=CARTESIAN_POINT('Ctrl Pts',(-0.371602173148636,1.391911284,-7.50245599257178));
#143862=CARTESIAN_POINT('Ctrl Pts',(-0.778131726340747,1.457192641,-7.46005233013552));
#143863=CARTESIAN_POINT('Ctrl Pts',(-0.792184849719485,1.45944932063632,
-7.4585864984506));
#143864=CARTESIAN_POINT('Ctrl Pts',(-0.806237973098223,1.46170600027265,
-7.45712066676558));
#143865=CARTESIAN_POINT('Ctrl Pts',(-0.202370093,1.326318298,-7.24717506));
#143866=CARTESIAN_POINT('Ctrl Pts',(-0.597299071,1.391911284,-7.236147064));
#143867=CARTESIAN_POINT('Ctrl Pts',(-0.988691053000001,1.457192641,-7.18226914));
#143868=CARTESIAN_POINT('Ctrl Pts',(-1.00222089300623,1.45944932063632,
-7.18040666012023));
#143869=CARTESIAN_POINT('Ctrl Pts',(-1.01575073301247,1.46170600027265,
-7.17854418024035));
#143870=CARTESIAN_POINT('Origin',(0.00769225992611006,1.33928762690979,
0.198985872132881));
#143871=CARTESIAN_POINT('Ctrl Pts',(-1.265901463,1.457192641,-7.3923943));
#143872=CARTESIAN_POINT('Ctrl Pts',(-1.669481539,1.391489877,-7.323283727));
#143873=CARTESIAN_POINT('Ctrl Pts',(-2.063139409,1.326325889,-7.210648777));
#143874=CARTESIAN_POINT('Ctrl Pts',(-0.988691053,1.457192641,-7.18226914));
#143875=CARTESIAN_POINT('Ctrl Pts',(-1.380799566,1.391489877,-7.128292581));
#143876=CARTESIAN_POINT('Ctrl Pts',(-1.76470159,1.326325889,-7.031950533));
#143877=CARTESIAN_POINT('',(-1.76013797088958,1.32710049375817,-7.03309422218891));
#143878=CARTESIAN_POINT('Origin',(0.0228635298486249,1.48213092814597,0.196710412613236));
#143879=CARTESIAN_POINT('Ctrl Pts',(-1.82007512674902,1.36645689996125,
-7.27580418457839));
#143880=CARTESIAN_POINT('Ctrl Pts',(-1.81003697829886,1.36020372534332,
-7.23532354641029));
#143881=CARTESIAN_POINT('Ctrl Pts',(-1.80001694630848,1.35380222441891,
-7.19483780259815));
#143882=CARTESIAN_POINT('Ctrl Pts',(-1.78003962021609,1.34069370770243,
-7.11394724922861));
#143883=CARTESIAN_POINT('Ctrl Pts',(-1.77007142075049,1.33397954195139,
-7.07349829535953));
#143884=CARTESIAN_POINT('Ctrl Pts',(-1.76013796613543,1.32710049389721,
-7.03309422333406));
#143885=CARTESIAN_POINT('Ctrl Pts',(-1.57611147796712,1.326318298,-7.33305818576935));
#143886=CARTESIAN_POINT('Ctrl Pts',(-1.97572058815322,1.391911284,-7.24716925836755));
#143887=CARTESIAN_POINT('Ctrl Pts',(-2.36363017270464,1.457192641,-7.11836513186888));
#143888=CARTESIAN_POINT('Ctrl Pts',(-2.37703963177751,1.45944932070005,
-7.1139125642307));
#143889=CARTESIAN_POINT('Ctrl Pts',(-2.39044909085038,1.46170600040011,
-7.10945999659266));
#143890=CARTESIAN_POINT('Ctrl Pts',(-1.755567205,1.326318298,-7.034236546));
#143891=CARTESIAN_POINT('Ctrl Pts',(-2.13889227,1.391911284,-6.93856832300001));
#143892=CARTESIAN_POINT('Ctrl Pts',(-2.509551565,1.457192641,-6.801812328));
#143893=CARTESIAN_POINT('Ctrl Pts',(-2.52236470714504,1.45944932070005,
-6.7970848760603));
#143894=CARTESIAN_POINT('Ctrl Pts',(-2.53517784929007,1.46170600040011,
-6.79235742412048));
#143895=CARTESIAN_POINT('Origin',(0.050288452313495,1.33928759751438,0.192679977206598));
#143896=CARTESIAN_POINT('Ctrl Pts',(-2.825451647,1.457192641,-6.947432835));
#143897=CARTESIAN_POINT('Ctrl Pts',(-3.204739515,1.391489877,-6.793180241));
#143898=CARTESIAN_POINT('Ctrl Pts',(-3.564980697,1.326325889,-6.598553828));
#143899=CARTESIAN_POINT('Ctrl Pts',(-2.509551565,1.457192641,-6.801812328));
#143900=CARTESIAN_POINT('Ctrl Pts',(-2.880889433,1.391489877,-6.66480597100001));
#143901=CARTESIAN_POINT('Ctrl Pts',(-3.235105349,1.326325889,-6.48818876000001));
#143902=CARTESIAN_POINT('',(-3.23089428594815,1.32710049348572,-6.49028675121906));
#143903=CARTESIAN_POINT('Origin',(0.0646160045864197,1.48213096720064,0.187196666467568));
#143904=CARTESIAN_POINT('Ctrl Pts',(-3.34160561001,1.36645689996097,-6.71443757429174));
#143905=CARTESIAN_POINT('Ctrl Pts',(-3.32310000733223,1.36020372536039,
-6.67706125633319));
#143906=CARTESIAN_POINT('Ctrl Pts',(-3.30461099988384,1.35380222441652,
-6.63967605740425));
#143907=CARTESIAN_POINT('Ctrl Pts',(-3.26771162001808,1.34069369538312,
-6.56497114488844));
#143908=CARTESIAN_POINT('Ctrl Pts',(-3.2492811600615,1.33397953570377,-6.52761076976344));
#143909=CARTESIAN_POINT('Ctrl Pts',(-3.23089427915016,1.3271004937052,-6.49028675464853));
#143910=CARTESIAN_POINT('Ctrl Pts',(-3.11565361346418,1.326318298,-6.82279798221481));
#143911=CARTESIAN_POINT('Ctrl Pts',(-3.48745650442699,1.391911284,-6.65301294327397));
#143912=CARTESIAN_POINT('Ctrl Pts',(-3.83860789814415,1.457192641,-6.44383109203171));
#143913=CARTESIAN_POINT('Ctrl Pts',(-3.85074668095551,1.45944932067843,
-6.43659998571765));
#143914=CARTESIAN_POINT('Ctrl Pts',(-3.8628854637669,1.46170600035686,-6.42936887940343));
#143915=CARTESIAN_POINT('Ctrl Pts',(-3.226675946,1.326318298,-6.49238495));
#143916=CARTESIAN_POINT('Ctrl Pts',(-3.580473244,1.391911284,-6.316549838));
#143917=CARTESIAN_POINT('Ctrl Pts',(-3.913068234,1.457192641,-6.10331033100001));
#143918=CARTESIAN_POINT('Ctrl Pts',(-3.92456554945993,1.45944932067843,
-6.09593895754517));
#143919=CARTESIAN_POINT('Ctrl Pts',(-3.93606286491986,1.46170600035686,
-6.0885675840903));
#143920=CARTESIAN_POINT('Origin',(0.0905333490495397,1.33928762116643,0.177364880444342));
#143921=CARTESIAN_POINT('Ctrl Pts',(-4.252886852,1.457192641,-6.177617131));
#143922=CARTESIAN_POINT('Ctrl Pts',(-4.590147433,1.391489877,-5.945435198));
#143923=CARTESIAN_POINT('Ctrl Pts',(-4.900127451,1.326325889,-5.67791783700001));
#143924=CARTESIAN_POINT('Ctrl Pts',(-3.913068234,1.457192641,-6.103310331));
#143925=CARTESIAN_POINT('Ctrl Pts',(-4.246272112,1.391489877,-5.889680441));
#143926=CARTESIAN_POINT('Ctrl Pts',(-4.554239178,1.326325889,-5.641046491));
#143927=CARTESIAN_POINT('',(-4.55057757322335,1.32710049349811,-5.64400068666468));
#143928=CARTESIAN_POINT('Origin',(0.103347140030356,1.48213096708157,0.168929683164989));
#143929=CARTESIAN_POINT('Ctrl Pts',(-4.70688632880667,1.36645689996756,
-5.83911132632025));
#143930=CARTESIAN_POINT('Ctrl Pts',(-4.68077857330409,1.36020372535252,
-5.80658700333002));
#143931=CARTESIAN_POINT('Ctrl Pts',(-4.65468511606554,1.35380222443658,
-5.77405043970525));
#143932=CARTESIAN_POINT('Ctrl Pts',(-4.60258908000211,1.34069369659121,
-5.70902436814684));
#143933=CARTESIAN_POINT('Ctrl Pts',(-4.57655813520577,1.33397953632925,
-5.67649945876565));
#143934=CARTESIAN_POINT('Ctrl Pts',(-4.55057756715233,1.32710049376822,
-5.64400069147785));
#143935=CARTESIAN_POINT('Ctrl Pts',(-4.50951124921828,1.326318298,-5.99351132775202));
#143936=CARTESIAN_POINT('Ctrl Pts',(-4.83612282993803,1.391911284,-5.74776913795098));
#143937=CARTESIAN_POINT('Ctrl Pts',(-5.13409658570113,1.457192641,-5.4679906727476));
#143938=CARTESIAN_POINT('Ctrl Pts',(-5.14439709605691,1.45944932059279,
-5.45831914657319));
#143939=CARTESIAN_POINT('Ctrl Pts',(-5.15469760641271,1.46170600018559,
-5.44864762039864));
#143940=CARTESIAN_POINT('Ctrl Pts',(-4.546908906,1.326318298,-5.646956649));
#143941=CARTESIAN_POINT('Ctrl Pts',(-4.854635269,1.391911284,-5.399176504));
#143942=CARTESIAN_POINT('Ctrl Pts',(-5.133614182,1.457192641,-5.119424326));
#143943=CARTESIAN_POINT('Ctrl Pts',(-5.14325806884177,1.45944932059279,
-5.10975370853518));
#143944=CARTESIAN_POINT('Ctrl Pts',(-5.15290195568366,1.46170600018559,
-5.10008309107027));
#143945=CARTESIAN_POINT('Origin',(0.126544741838824,1.3392876175325,0.153755982148334));
#143946=CARTESIAN_POINT('Ctrl Pts',(-5.481461795,1.457192641,-5.118942917));
#143947=CARTESIAN_POINT('Ctrl Pts',(-5.760925159,1.391489877,-4.819688212));
#143948=CARTESIAN_POINT('Ctrl Pts',(-6.006149691,1.326325889,-4.491788718));
#143949=CARTESIAN_POINT('Ctrl Pts',(-5.133614182,1.457192641,-5.119424326));
#143950=CARTESIAN_POINT('Ctrl Pts',(-5.413103827,1.391489877,-4.83916));
#143951=CARTESIAN_POINT('Ctrl Pts',(-5.660421844,1.326325889,-4.530135158));
#143952=CARTESIAN_POINT('',(-5.65748091030866,1.32710049348203,-4.53380742346978));
#143953=CARTESIAN_POINT('Origin',(0.137245870428021,1.48213098361316,0.142763663710617));
#143954=CARTESIAN_POINT('Ctrl Pts',(-5.85207827439091,1.36645689999436,
-4.69075472208899));
#143955=CARTESIAN_POINT('Ctrl Pts',(-5.81958913571005,1.36020372537183,
-4.66460319540688));
#143956=CARTESIAN_POINT('Ctrl Pts',(-5.78711132963947,1.35380222444224,
-4.63843664054921));
#143957=CARTESIAN_POINT('Ctrl Pts',(-5.72225508680042,1.34069379760831,
-4.5861303533718));
#143958=CARTESIAN_POINT('Ctrl Pts',(-5.68984057087204,1.33397958597717,
-4.55996152766193));
#143959=CARTESIAN_POINT('Ctrl Pts',(-5.65748090610616,1.32710049369622,
-4.53380742861306));
#143960=CARTESIAN_POINT('Ctrl Pts',(-5.69250915066891,1.326318298,-4.88397474512399));
#143961=CARTESIAN_POINT('Ctrl Pts',(-5.95865742732611,1.391911284,-4.57376603597315));
#143962=CARTESIAN_POINT('Ctrl Pts',(-6.18952062274078,1.457192641,-4.23647308634013));
#143963=CARTESIAN_POINT('Ctrl Pts',(-6.19750122062436,1.4594493205828,-4.22481336987838));
#143964=CARTESIAN_POINT('Ctrl Pts',(-6.20548181850794,1.46170600016559,
-4.21315365341668));
#143965=CARTESIAN_POINT('Ctrl Pts',(-5.65453346,1.326318298,-4.537482931));
#143966=CARTESIAN_POINT('Ctrl Pts',(-5.901799944,1.391911284,-4.229343677));
#143967=CARTESIAN_POINT('Ctrl Pts',(-6.114118036,1.457192641,-3.89615973));
#143968=CARTESIAN_POINT('Ctrl Pts',(-6.12145755719401,1.45944932058279,
-3.88464205565829));
#143969=CARTESIAN_POINT('Ctrl Pts',(-6.12879707838804,1.4617060001656,-3.87312438131663));
#143970=CARTESIAN_POINT('Origin',(0.156639207923298,1.33928759898889,0.12295788907206));
#143971=CARTESIAN_POINT('Ctrl Pts',(-6.453729677,1.457192641,-3.820912621));
#143972=CARTESIAN_POINT('Ctrl Pts',(-6.662328427,1.391489877,-3.468577963));
#143973=CARTESIAN_POINT('Ctrl Pts',(-6.831331047,1.326325889,-3.095628551));
#143974=CARTESIAN_POINT('Ctrl Pts',(-6.11411803600001,1.457192641,-3.89615973));
#143975=CARTESIAN_POINT('Ctrl Pts',(-6.326824824,1.391489877,-3.562365816));
#143976=CARTESIAN_POINT('Ctrl Pts',(-6.501929476,1.326325889,-3.20739974));
#143977=CARTESIAN_POINT('',(-6.4998467281796,1.32710049370012,-3.21161836600255));
#143978=CARTESIAN_POINT('Origin',(0.164726821765547,1.48213093831918,0.109921952271952));
#143979=CARTESIAN_POINT('Ctrl Pts',(-6.723633543987,1.36645689999757,-3.32306364089608));
#143980=CARTESIAN_POINT('Ctrl Pts',(-6.68628217802592,1.3602037253718,-3.30450772682288));
#143981=CARTESIAN_POINT('Ctrl Pts',(-6.64893864914608,1.35380222444506,
-3.28593469975597));
#143982=CARTESIAN_POINT('Ctrl Pts',(-6.57435389535092,1.34069370829399,
-3.24879322648768));
#143983=CARTESIAN_POINT('Ctrl Pts',(-6.53707196030162,1.33397954224069,
-3.23020451101497));
#143984=CARTESIAN_POINT('Ctrl Pts',(-6.49984672601538,1.32710049388369,
-3.21161837026922));
#143985=CARTESIAN_POINT('Ctrl Pts',(-6.60933165067934,1.326318298,-3.54606893236592));
#143986=CARTESIAN_POINT('Ctrl Pts',(-6.80257182677962,1.391911284,-3.18589871739284));
#143987=CARTESIAN_POINT('Ctrl Pts',(-6.95552955380988,1.457192641,-2.80686272650075));
#143988=CARTESIAN_POINT('Ctrl Pts',(-6.9608170736095,1.45944931985099,-2.79376001933108));
#143989=CARTESIAN_POINT('Ctrl Pts',(-6.9661045934092,1.46170599870198,-2.7806573121614));
#143990=CARTESIAN_POINT('Ctrl Pts',(-6.497758313,1.326318298,-3.215841555));
#143991=CARTESIAN_POINT('Ctrl Pts',(-6.67300301300001,1.391911284,-2.86175144));
#143992=CARTESIAN_POINT('Ctrl Pts',(-6.808732526,1.457192641,-2.490715035));
#143993=CARTESIAN_POINT('Ctrl Pts',(-6.81342449221393,1.45944931985099,
-2.47788886154728));
#143994=CARTESIAN_POINT('Ctrl Pts',(-6.8181164584277,1.46170599870198,-2.46506268809461));
#143995=CARTESIAN_POINT('Origin',(0.179409394884619,1.33928762174604,0.0864104006243482));
#143996=CARTESIAN_POINT('Ctrl Pts',(-7.124228332,1.457192641,-2.344220698));
#143997=CARTESIAN_POINT('Ctrl Pts',(-7.252208622,1.391489877,-1.955280863));
#143998=CARTESIAN_POINT('Ctrl Pts',(-7.33708695600001,1.326325889,-1.554720233));
#143999=CARTESIAN_POINT('Ctrl Pts',(-6.808732526,1.457192641,-2.490715035));
#144000=CARTESIAN_POINT('Ctrl Pts',(-6.944710523,1.391489877,-2.118999365));
#144001=CARTESIAN_POINT('Ctrl Pts',(-7.039414112,1.326325889,-1.734689875));
#144002=CARTESIAN_POINT('',(-7.03828693677588,1.3271004934935,-1.73925759858549));
#144003=CARTESIAN_POINT('Origin',(0.184505602804806,1.48213091444911,0.0719406485621665));
#144004=CARTESIAN_POINT('Ctrl Pts',(-7.2807991818215,1.36645690001632,-1.79998979688873));
#144005=CARTESIAN_POINT('Ctrl Pts',(-7.2403320970141,1.36020372537985,-1.78989714928127));
#144006=CARTESIAN_POINT('Ctrl Pts',(-7.19986898733355,1.3538022244547,-1.7797861040923));
#144007=CARTESIAN_POINT('Ctrl Pts',(-7.1190436215013,1.34069370128852,-1.75954648444623));
#144008=CARTESIAN_POINT('Ctrl Pts',(-7.07863731480259,1.3339795386024,-1.74940688235601));
#144009=CARTESIAN_POINT('Ctrl Pts',(-7.03828693507949,1.32710049369933,
-1.73925760555958));
#144010=CARTESIAN_POINT('Ctrl Pts',(-7.21710914931238,1.326318298,-2.04235287662906));
#144011=CARTESIAN_POINT('Ctrl Pts',(-7.32840552681089,1.391911284,-1.64906231605164));
#144012=CARTESIAN_POINT('Ctrl Pts',(-7.39630565439733,1.457192641,-1.24600658618423));
#144013=CARTESIAN_POINT('Ctrl Pts',(-7.39865286098283,1.45944932057495,
-1.23207354810171));
#144014=CARTESIAN_POINT('Ctrl Pts',(-7.40100006756837,1.46170600014991,
-1.21814051001917));
#144015=CARTESIAN_POINT('Ctrl Pts',(-7.037155209,1.326318298,-1.743831002));
#144016=CARTESIAN_POINT('Ctrl Pts',(-7.13218387800001,1.391911284,-1.360346886));
#144017=CARTESIAN_POINT('Ctrl Pts',(-7.18497825100001,1.457192641,-0.968807273));
#144018=CARTESIAN_POINT('Ctrl Pts',(-7.18680327408004,1.45944932057495,
-0.955272329977257));
#144019=CARTESIAN_POINT('Ctrl Pts',(-7.18862829716009,1.46170600014991,
-0.941737386954499));
#144020=CARTESIAN_POINT('Origin',(0.193790514631866,1.33928765482181,0.0458224414306448));
#144021=CARTESIAN_POINT('Ctrl Pts',(-7.461605988,1.457192641,-0.75791562));
#144022=CARTESIAN_POINT('Ctrl Pts',(-7.502983602,1.391489877,-0.350557003));
#144023=CARTESIAN_POINT('Ctrl Pts',(-7.499768833,1.326325889,0.058885075));
#144024=CARTESIAN_POINT('Ctrl Pts',(-7.184978251,1.457192641,-0.968807273));
#144025=CARTESIAN_POINT('Ctrl Pts',(-7.237869276,1.391489877,-0.57655086));
#144026=CARTESIAN_POINT('Ctrl Pts',(-7.247743568,1.326325889,-0.180867839));
#144027=CARTESIAN_POINT('',(-7.24762467142716,1.32710049364435,-0.185571082245031));
#144028=CARTESIAN_POINT('Origin',(0.195657359581503,1.48213100007743,0.0305955037867436));
#144029=CARTESIAN_POINT('Ctrl Pts',(-7.4975227417753,1.36645690002419,-0.192750430437088));
#144030=CARTESIAN_POINT('Ctrl Pts',(-7.45583213413798,1.36020372540562,
-0.191592970424011));
#144031=CARTESIAN_POINT('Ctrl Pts',(-7.4141414537035,1.35380222448827,-0.190416688389667));
#144032=CARTESIAN_POINT('Ctrl Pts',(-7.3308554322295,1.34069379766143,-0.188025341830143));
#144033=CARTESIAN_POINT('Ctrl Pts',(-7.28921376232473,1.33397958603636,
-0.186808950438261));
#144034=CARTESIAN_POINT('Ctrl Pts',(-7.24762467122657,1.32710049376091,
-0.185571088336482));
#144035=CARTESIAN_POINT('Ctrl Pts',(-7.48742264462421,1.326318298,-0.443138670805058));
#144036=CARTESIAN_POINT('Ctrl Pts',(-7.51157113006944,1.391911284,-0.0351175931108654));
#144037=CARTESIAN_POINT('Ctrl Pts',(-7.49123872278317,1.457192641,0.373111438402629));
#144038=CARTESIAN_POINT('Ctrl Pts',(-7.49053586165044,1.45944932058945,
0.387223309931836));
#144039=CARTESIAN_POINT('Ctrl Pts',(-7.48983300051772,1.4617060001789,0.401335181461041));
#144040=CARTESIAN_POINT('Ctrl Pts',(-7.247502549,1.326318298,-0.190280849));
#144041=CARTESIAN_POINT('Ctrl Pts',(-7.257871751,1.391911284,0.204665976));
#144042=CARTESIAN_POINT('Ctrl Pts',(-7.225262378,1.457192641,0.59840084));
#144043=CARTESIAN_POINT('Ctrl Pts',(-7.22413512038993,1.45944932058945,
0.612011669677492));
#144044=CARTESIAN_POINT('Ctrl Pts',(-7.22300786277985,1.4617060001789,0.625622499354983));
#144045=CARTESIAN_POINT('Origin',(0.199110329142863,1.33928764733072,0.00309190139125497));
#144046=CARTESIAN_POINT('Ctrl Pts',(-7.450087241,1.457192641,0.86382875));
#144047=CARTESIAN_POINT('Ctrl Pts',(-7.402927409,1.391489877,1.270558513));
#144048=CARTESIAN_POINT('Ctrl Pts',(-7.311769855,1.326325889,1.669736982));
#144049=CARTESIAN_POINT('Ctrl Pts',(-7.225262378,1.457192641,0.59840084));
#144050=CARTESIAN_POINT('Ctrl Pts',(-7.192593307,1.391489877,0.992856524000001));
#144051=CARTESIAN_POINT('Ctrl Pts',(-7.11717659,1.326325889,1.381411376));
#144052=CARTESIAN_POINT('',(-7.11807153258829,1.32710049373858,1.37679253178578));
#144053=CARTESIAN_POINT('Origin',(0.197659878927633,1.48213093731636,-0.0121803272532719));
#144054=CARTESIAN_POINT('Ctrl Pts',(-7.36367047157635,1.36645689998419,
1.42350173179027));
#144055=CARTESIAN_POINT('Ctrl Pts',(-7.32270574734249,1.36020372535754,
1.41566988274934));
#144056=CARTESIAN_POINT('Ctrl Pts',(-7.28173690607024,1.3538022244682,1.40785640008115));
#144057=CARTESIAN_POINT('Ctrl Pts',(-7.19988399654352,1.34069379764131,
1.39228780563331));
#144058=CARTESIAN_POINT('Ctrl Pts',(-7.15895439847139,1.33397958617594,
1.38452403057887));
#144059=CARTESIAN_POINT('Ctrl Pts',(-7.11807153346691,1.32710049390419,
1.37679252699242));
#144060=CARTESIAN_POINT('Ctrl Pts',(-7.40763257896271,1.326318298,1.17679620739308));
#144061=CARTESIAN_POINT('Ctrl Pts',(-7.34350401581921,1.391911284,1.58046918964569));
#144062=CARTESIAN_POINT('Ctrl Pts',(-7.23588979397156,1.457192641,1.97478318634273));
#144063=CARTESIAN_POINT('Ctrl Pts',(-7.23216973004729,1.45944932061847,
1.98841403595307));
#144064=CARTESIAN_POINT('Ctrl Pts',(-7.22844966612306,1.46170600023695,
2.00204488556346));
#144065=CARTESIAN_POINT('Ctrl Pts',(-7.118964725,1.326318298,1.372166625));
#144066=CARTESIAN_POINT('Ctrl Pts',(-7.044189608,1.391911284,1.760108884));
#144067=CARTESIAN_POINT('Ctrl Pts',(-6.927701267,1.457192641,2.137628395));
#144068=CARTESIAN_POINT('Ctrl Pts',(-6.92367443794796,1.45944932061847,
2.1506786841668));
#144069=CARTESIAN_POINT('Ctrl Pts',(-6.9196476088959,1.46170600023695,2.16372897333358));
#144070=CARTESIAN_POINT('Origin',(0.195119959503641,1.33928761351094,-0.0397832256104988));
#144071=CARTESIAN_POINT('Ctrl Pts',(-7.090210694,1.457192641,2.445181447));
#144072=CARTESIAN_POINT('Ctrl Pts',(-6.956718557,1.391489877,2.832264125));
#144073=CARTESIAN_POINT('Ctrl Pts',(-6.781880645,1.326325889,3.202513844));
#144074=CARTESIAN_POINT('Ctrl Pts',(-6.927701267,1.457192641,2.137628395));
#144075=CARTESIAN_POINT('Ctrl Pts',(-6.810999668,1.391489877,2.515839039));
#144076=CARTESIAN_POINT('Ctrl Pts',(-6.653818345,1.326325889,2.87909733));
#144077=CARTESIAN_POINT('',(-6.65568527723499,1.32710049346833,2.8747788600681));
#144078=CARTESIAN_POINT('Origin',(0.19042055041486,1.48213096031789,-0.0543866830032513));
#144079=CARTESIAN_POINT('Ctrl Pts',(-6.88550115417648,1.36645690001224,
2.9731925354682));
#144080=CARTESIAN_POINT('Ctrl Pts',(-6.84717777853504,1.36020372538709,
2.95673758590746));
#144081=CARTESIAN_POINT('Ctrl Pts',(-6.80884643362966,1.35380222445678,
2.9402996881705));
#144082=CARTESIAN_POINT('Ctrl Pts',(-6.73225398731902,1.34069379761851,
2.90749912276099));
#144083=CARTESIAN_POINT('Ctrl Pts',(-6.6939502817044,1.33397958597253,2.89111820627741));
#144084=CARTESIAN_POINT('Ctrl Pts',(-6.65568528011168,1.32710049368268,
2.87477885338197));
#144085=CARTESIAN_POINT('Ctrl Pts',(-6.9814698473063,1.326318298,2.74170540229439));
#144086=CARTESIAN_POINT('Ctrl Pts',(-6.83206281608202,1.391911284,3.12215498942192));
#144087=CARTESIAN_POINT('Ctrl Pts',(-6.64219870107241,1.457192641,3.48411626705969));
#144088=CARTESIAN_POINT('Ctrl Pts',(-6.63563538022026,1.45944932068712,
3.49662873157185));
#144089=CARTESIAN_POINT('Ctrl Pts',(-6.62907205936814,1.46170600037424,
3.50914119608405));
#144090=CARTESIAN_POINT('Ctrl Pts',(-6.657552022,1.326318298,2.870453113));
#144091=CARTESIAN_POINT('Ctrl Pts',(-6.501128988,1.391911284,3.233251058));
#144092=CARTESIAN_POINT('Ctrl Pts',(-6.306208544,1.457192641,3.576902822));
#144093=CARTESIAN_POINT('Ctrl Pts',(-6.29947043335412,1.45944932068712,
3.58878235378212));
#144094=CARTESIAN_POINT('Ctrl Pts',(-6.29273232270823,1.46170600037424,
3.60066188556422));
#144095=CARTESIAN_POINT('Origin',(0.182005772061442,1.33928763056823,-0.0807980551483395));
#144096=CARTESIAN_POINT('Ctrl Pts',(-6.398803776,1.457192641,3.912200178));
#144097=CARTESIAN_POINT('Ctrl Pts',(-6.185221277,1.391489877,4.261536214));
#144098=CARTESIAN_POINT('Ctrl Pts',(-5.934878233,1.326325889,4.585544717));
#144099=CARTESIAN_POINT('Ctrl Pts',(-6.306208544,1.457192641,3.576902822));
#144100=CARTESIAN_POINT('Ctrl Pts',(-6.110931255,1.391489877,3.921183718));
#144101=CARTESIAN_POINT('Ctrl Pts',(-5.87933494900001,1.326325889,4.242159893));
#144102=CARTESIAN_POINT('',(-5.88208657716348,1.32710049351043,4.23834372171454));
#144103=CARTESIAN_POINT('Origin',(0.17427700323462,1.48213094100688,-0.0940498837865111));
#144104=CARTESIAN_POINT('Ctrl Pts',(-6.08537345500619,1.36645689999237,
4.38386016046963));
#144105=CARTESIAN_POINT('Ctrl Pts',(-6.05148338649333,1.36020372539536,
4.35955152564049));
#144106=CARTESIAN_POINT('Ctrl Pts',(-6.01758186916682,1.35380222445104,
4.33525783063649));
#144107=CARTESIAN_POINT('Ctrl Pts',(-5.94983126380686,1.34069379764136,
4.28675901230052));
#144108=CARTESIAN_POINT('Ctrl Pts',(-5.91594449053718,1.33397958603012,
4.26252690812683));
#144109=CARTESIAN_POINT('Ctrl Pts',(-5.88208658128532,1.32710049374011,
4.23834371587839));
#144110=CARTESIAN_POINT('Ctrl Pts',(-6.22886134497013,1.326318298,4.1784155004681));
#144111=CARTESIAN_POINT('Ctrl Pts',(-6.00116195121403,1.391911284,4.51785229157823));
#144112=CARTESIAN_POINT('Ctrl Pts',(-5.73792577853377,1.457192641,4.83053594383523));
#144113=CARTESIAN_POINT('Ctrl Pts',(-5.728826094617,1.45944932065123,4.84134495375397));
#144114=CARTESIAN_POINT('Ctrl Pts',(-5.7197264107004,1.46170600030247,4.85215396367269));
#144115=CARTESIAN_POINT('Ctrl Pts',(-5.88483958600001,1.326318298,4.234520403));
#144116=CARTESIAN_POINT('Ctrl Pts',(-5.654082801,1.391911284,4.555210005));
#144117=CARTESIAN_POINT('Ctrl Pts',(-5.389844518,1.457192641,4.848925249));
#144118=CARTESIAN_POINT('Ctrl Pts',(-5.38071019261637,1.45944932065123,
4.85907854918939));
#144119=CARTESIAN_POINT('Ctrl Pts',(-5.37157586723272,1.46170600030247,
4.86923184937878));
#144120=CARTESIAN_POINT('Origin',(0.160381593158633,1.33928762122271,-0.118035070517558));
#144121=CARTESIAN_POINT('Ctrl Pts',(-5.408195905,1.457192641,5.196288777));
#144122=CARTESIAN_POINT('Ctrl Pts',(-5.124509925,1.391489877,5.491543606));
#144123=CARTESIAN_POINT('Ctrl Pts',(-4.810367512,1.326325889,5.754160616));
#144124=CARTESIAN_POINT('Ctrl Pts',(-5.389844518,1.457192641,4.848925249));
#144125=CARTESIAN_POINT('Ctrl Pts',(-5.125122489,1.391489877,5.143178203));
#144126=CARTESIAN_POINT('Ctrl Pts',(-4.829940385,1.326325889,5.406863774));
#144127=CARTESIAN_POINT('',(-4.83344804852087,1.3271004938086,5.40372834108578));
#144128=CARTESIAN_POINT('Origin',(0.14998457613528,1.4821310466166,-0.129315447734775));
#144129=CARTESIAN_POINT('Ctrl Pts',(-5.00070045707493,1.36645689999032,
5.58954335620345));
#144130=CARTESIAN_POINT('Ctrl Pts',(-4.9728283573888,1.36020372537749,5.55851768078015));
#144131=CARTESIAN_POINT('Ctrl Pts',(-4.94494186503069,1.35380222444764,
5.52750413492136));
#144132=CARTESIAN_POINT('Ctrl Pts',(-4.88920104311748,1.34069379760003,
5.46557481462023));
#144133=CARTESIAN_POINT('Ctrl Pts',(-4.86131571074869,1.33397958624442,
5.43462459034137));
#144134=CARTESIAN_POINT('Ctrl Pts',(-4.83344805172475,1.32710049394251,
5.40372833816614));
#144135=CARTESIAN_POINT('Ctrl Pts',(-5.18499820863661,1.326318298,5.41974753300653));
#144136=CARTESIAN_POINT('Ctrl Pts',(-4.8896534235684,1.391911284,5.70229984158403));
#144137=CARTESIAN_POINT('Ctrl Pts',(-4.56535382460105,1.457192641,5.95108512861539));
#144138=CARTESIAN_POINT('Ctrl Pts',(-4.55414326908976,1.45944932056061,
5.95968526651115));
#144139=CARTESIAN_POINT('Ctrl Pts',(-4.54293271357833,1.46170600012122,
5.96828540440697));
#144140=CARTESIAN_POINT('Ctrl Pts',(-4.836958592,1.326318298,5.400586226));
#144141=CARTESIAN_POINT('Ctrl Pts',(-4.54265798800001,1.391911284,5.664172395));
#144142=CARTESIAN_POINT('Ctrl Pts',(-4.221457354,1.457192641,5.89421732));
#144143=CARTESIAN_POINT('Ctrl Pts',(-4.21035392510525,1.45944932056061,
5.90216963141211));
#144144=CARTESIAN_POINT('Ctrl Pts',(-4.1992504962105,1.46170600012122,5.91012194282422));
#144145=CARTESIAN_POINT('Origin',(0.131257950572324,1.3392875952123,-0.149752816308679));
#144146=CARTESIAN_POINT('Ctrl Pts',(-4.164706805,1.457192641,6.237404687));
#144147=CARTESIAN_POINT('Ctrl Pts',(-3.824182184,1.391489877,6.464772523));
#144148=CARTESIAN_POINT('Ctrl Pts',(-3.460929352,1.326325889,6.653718361));
#144149=CARTESIAN_POINT('Ctrl Pts',(-4.221457354,1.457192641,5.89421732));
#144150=CARTESIAN_POINT('Ctrl Pts',(-3.89966869,1.391489877,6.124683393));
#144151=CARTESIAN_POINT('Ctrl Pts',(-3.554703177,1.326325889,6.318748715));
#144152=CARTESIAN_POINT('',(-3.55880285644889,1.32710049347857,6.3164406300595));
#144153=CARTESIAN_POINT('Origin',(0.118678978891426,1.48213094058367,-0.158534356723926));
#144154=CARTESIAN_POINT('Ctrl Pts',(-3.68220026361416,1.36645690003059,
6.53386571770354));
#144155=CARTESIAN_POINT('Ctrl Pts',(-3.66164940112487,1.36020372540053,
6.49757372770157));
#144156=CARTESIAN_POINT('Ctrl Pts',(-3.64108187499581,1.35380222446052,
6.46129048970569));
#144157=CARTESIAN_POINT('Ctrl Pts',(-3.59995721578982,1.34069379762435,
6.38882641346529));
#144158=CARTESIAN_POINT('Ctrl Pts',(-3.57937720959691,1.33397958601979,
6.35260526465788));
#144159=CARTESIAN_POINT('Ctrl Pts',(-3.55880286204966,1.3271004937455,6.31644062682241));
#144160=CARTESIAN_POINT('Ctrl Pts',(-3.89869031899553,1.326318298,6.4076581951046));
#144161=CARTESIAN_POINT('Ctrl Pts',(-3.5495101372942,1.391911284,6.62011418952326));
#144162=CARTESIAN_POINT('Ctrl Pts',(-3.17931099982432,1.457192641,6.79336818647255));
#144163=CARTESIAN_POINT('Ctrl Pts',(-3.16651376501828,1.45944932063382,
6.79935732003778));
#144164=CARTESIAN_POINT('Ctrl Pts',(-3.15371653021228,1.46170600026764,
6.80534645360308));
#144165=CARTESIAN_POINT('Ctrl Pts',(-3.56290679,1.326318298,6.314126639));
#144166=CARTESIAN_POINT('Ctrl Pts',(-3.218823535,1.391911284,6.50828438));
#144167=CARTESIAN_POINT('Ctrl Pts',(-2.855679535,1.457192641,6.66390234));
#144168=CARTESIAN_POINT('Ctrl Pts',(-2.84312618582646,1.45944932063382,
6.66928182193984));
#144169=CARTESIAN_POINT('Ctrl Pts',(-2.83057283665291,1.46170600026764,
6.67466130387953));
#144170=CARTESIAN_POINT('Origin',(0.09599672438588,1.33928764452021,-0.174468164838252));
#144171=CARTESIAN_POINT('Ctrl Pts',(-2.726480643,1.457192641,6.986866487));
#144172=CARTESIAN_POINT('Ctrl Pts',(-2.345039935,1.391489877,7.135715861));
#144173=CARTESIAN_POINT('Ctrl Pts',(-1.949661982,1.326325889,7.242155629));
#144174=CARTESIAN_POINT('Ctrl Pts',(-2.855679535,1.457192641,6.66390234));
#144175=CARTESIAN_POINT('Ctrl Pts',(-2.491870718,1.391489877,6.81980519300001));
#144176=CARTESIAN_POINT('Ctrl Pts',(-2.113252,1.326325889,6.935175988));
#144177=CARTESIAN_POINT('',(-2.11775200048965,1.32710049345207,6.93380317484552));
#144178=CARTESIAN_POINT('Origin',(0.081824182827851,1.48213092866479,-0.180340533094112));
#144179=CARTESIAN_POINT('Ctrl Pts',(-2.19152447788043,1.3664568999714,7.17267177956051));
#144180=CARTESIAN_POINT('Ctrl Pts',(-2.17925578824896,1.36020372535492,
7.13281044820063));
#144181=CARTESIAN_POINT('Ctrl Pts',(-2.16696894311951,1.35380222440394,
7.09295408190761));
#144182=CARTESIAN_POINT('Ctrl Pts',(-2.14238322001099,1.34069370685812,
7.01334303852864));
#144183=CARTESIAN_POINT('Ctrl Pts',(-2.1300709296158,1.33397954135704,6.97354492030573));
#144184=CARTESIAN_POINT('Ctrl Pts',(-2.11775200705747,1.32710049367607,
6.9338031727709));
#144185=CARTESIAN_POINT('Ctrl Pts',(-2.43008400264679,1.326318298,7.09595388132399));
#144186=CARTESIAN_POINT('Ctrl Pts',(-2.04339570073183,1.391911284,7.22837935535174));
#144187=CARTESIAN_POINT('Ctrl Pts',(-1.64460712498484,1.457192641,7.31800089883336));
#144188=CARTESIAN_POINT('Ctrl Pts',(-1.63082159570203,1.45944932063747,
7.32109898259795));
#144189=CARTESIAN_POINT('Ctrl Pts',(-1.61703606641928,1.46170600027495,
7.32419706636265));
#144190=CARTESIAN_POINT('Ctrl Pts',(-2.122257426,1.326318298,6.932425508));
#144191=CARTESIAN_POINT('Ctrl Pts',(-1.744480471,1.391911284,7.04807622));
#144192=CARTESIAN_POINT('Ctrl Pts',(-1.356373314,1.457192641,7.121990693));
#144193=CARTESIAN_POINT('Ctrl Pts',(-1.34295702551262,1.45944932063747,
7.12454580664653));
#144194=CARTESIAN_POINT('Ctrl Pts',(-1.32954073702527,1.46170600027495,
7.1271009202929));
#144195=CARTESIAN_POINT('Origin',(0.0562468783962666,1.33928763488106,-0.191025668185087));
#144196=CARTESIAN_POINT('Ctrl Pts',(-1.160767276,1.457192641,7.409630175));
#144197=CARTESIAN_POINT('Ctrl Pts',(-0.756246224,1.391489877,7.473001057));
#144198=CARTESIAN_POINT('Ctrl Pts',(-0.347230585,1.326325889,7.49195775));
#144199=CARTESIAN_POINT('Ctrl Pts',(-1.356373314,1.457192641,7.121990693));
#144200=CARTESIAN_POINT('Ctrl Pts',(-0.967555641,1.391489877,7.196040483));
#144201=CARTESIAN_POINT('Ctrl Pts',(-0.572987507,1.326325889,7.22732214));
#144202=CARTESIAN_POINT('',(-0.577677415430962,1.32710049363407,7.22694878972836));
#144203=CARTESIAN_POINT('Origin',(0.0411433145576777,1.48213100234167,-0.193714029734774));
#144204=CARTESIAN_POINT('Ctrl Pts',(-0.598375443566073,1.36645689998275,
7.47609168121661));
#144205=CARTESIAN_POINT('Ctrl Pts',(-0.594962597040865,1.36020372536892,
7.43452488005759));
#144206=CARTESIAN_POINT('Ctrl Pts',(-0.591530952127597,1.35380222444649,
7.39295902513781));
#144207=CARTESIAN_POINT('Ctrl Pts',(-0.584634098175082,1.34069379761045,
7.30992461451379));
#144208=CARTESIAN_POINT('Ctrl Pts',(-0.581165056043418,1.33397958602485,
7.26840986999439));
#144209=CARTESIAN_POINT('Ctrl Pts',(-0.577677421155283,1.32710049373197,
7.2269487892306));
#144210=CARTESIAN_POINT('Ctrl Pts',(-0.847849659089698,1.326318298,7.45245065089731));
#144211=CARTESIAN_POINT('Ctrl Pts',(-0.441734353150813,1.391911284,7.49865353618925));
#144212=CARTESIAN_POINT('Ctrl Pts',(-0.0330032499786711,1.457192641,7.50045202179782));
#144213=CARTESIAN_POINT('Ctrl Pts',(-0.0188740223279256,1.45944932062933,
7.50051419277624));
#144214=CARTESIAN_POINT('Ctrl Pts',(-0.00474479467718063,1.46170600025867,
7.50057636375466));
#144215=CARTESIAN_POINT('Ctrl Pts',(-0.582373663,1.326318298,7.22657186500001));
#144216=CARTESIAN_POINT('Ctrl Pts',(-0.18856744,1.391911284,7.25830784900001));
#144217=CARTESIAN_POINT('Ctrl Pts',(0.206355414,1.457192641,7.247062677));
#144218=CARTESIAN_POINT('Ctrl Pts',(0.220007310969285,1.45944932062933,
7.24667394809262));
#144219=CARTESIAN_POINT('Ctrl Pts',(0.233659207938571,1.46170600025867,
7.24628521918508));
#144220=CARTESIAN_POINT('Origin',(0.0138669977767894,1.33928758393614,-0.198651021090203));
#144221=CARTESIAN_POINT('Ctrl Pts',(-1.360746905,4.560731746,7.121156357));
#144222=CARTESIAN_POINT('Ctrl Pts',(-0.969780916,4.495065281,7.195864134));
#144223=CARTESIAN_POINT('Ctrl Pts',(-0.572986203,4.430609079,7.227322244));
#144224=CARTESIAN_POINT('Ctrl Pts',(-1.648506461,4.560731746,7.31658571));
#144225=CARTESIAN_POINT('Ctrl Pts',(-1.246811002,4.495065281,7.407092072));
#144226=CARTESIAN_POINT('Ctrl Pts',(-0.837621771,4.430609079,7.453079214));
#144227=CARTESIAN_POINT('',(-1.35606856648098,4.55994605296445,7.12204874014566));
#144228=CARTESIAN_POINT('Origin',(0.0577273861491251,4.69628092964401,-0.182460475736631));
#144229=CARTESIAN_POINT('Ctrl Pts',(-1.40181135298698,4.5206323408617,7.36783040874985));
#144230=CARTESIAN_POINT('Ctrl Pts',(-1.39421544816574,4.52686607840845,
7.32681968872307));
#144231=CARTESIAN_POINT('Ctrl Pts',(-1.38660265533698,4.53325386659101,
7.28581108465512));
#144232=CARTESIAN_POINT('Ctrl Pts',(-1.37135868269627,4.54634733293425,
7.2038974290939));
#144233=CARTESIAN_POINT('Ctrl Pts',(-1.36371859852423,4.5530606542029,7.16294451736904));
#144234=CARTESIAN_POINT('Ctrl Pts',(-1.35606856762555,4.55994605042158,
7.12204873950343));
#144235=CARTESIAN_POINT('Ctrl Pts',(-2.113250748,4.430609079,6.93517637));
#144236=CARTESIAN_POINT('Ctrl Pts',(-1.73744496,4.495496505,7.04968994800001));
#144237=CARTESIAN_POINT('Ctrl Pts',(-1.351465456,4.560723991,7.122923636));
#144238=CARTESIAN_POINT('Ctrl Pts',(-1.949660675,4.430609079,7.242155981));
#144239=CARTESIAN_POINT('Ctrl Pts',(-1.557220167,4.495496505,7.34780488300001));
#144240=CARTESIAN_POINT('Ctrl Pts',(-1.155661261,4.560723991,7.410428264));
#144241=CARTESIAN_POINT('Origin',(0.0382436804201319,4.55356860646856,-0.195301735550543));
#144242=CARTESIAN_POINT('Ctrl Pts',(-2.859771516,4.560731746,6.662147317));
#144243=CARTESIAN_POINT('Ctrl Pts',(-2.494006057,4.495065281,6.819154599));
#144244=CARTESIAN_POINT('Ctrl Pts',(-2.113250748,4.430609079,6.93517637));
#144245=CARTESIAN_POINT('Ctrl Pts',(-3.182814947,4.560731746,6.79114784200001));
#144246=CARTESIAN_POINT('Ctrl Pts',(-2.809967097,4.495065281,6.965890866));
#144247=CARTESIAN_POINT('Ctrl Pts',(-2.420230359,4.430609079,7.098766443));
#144248=CARTESIAN_POINT('',(-2.85539438941292,4.5599460519018,6.66402454208368));
#144249=CARTESIAN_POINT('Origin',(0.0956012963018976,4.69628105067334,-0.16578473521602));
#144250=CARTESIAN_POINT('Ctrl Pts',(-2.9529035287323,4.52063234088232,6.89422662433444));
#144251=CARTESIAN_POINT('Ctrl Pts',(-2.93666913907048,4.52686607086783,
6.85580765366949));
#144252=CARTESIAN_POINT('Ctrl Pts',(-2.92041868087003,4.53325386292767,
6.81739430829154));
#144253=CARTESIAN_POINT('Ctrl Pts',(-2.88792208022279,4.54634733289054,
6.74067273052007));
#144254=CARTESIAN_POINT('Ctrl Pts',(-2.87165695187537,4.55306065400379,
6.70231966810698));
#144255=CARTESIAN_POINT('Ctrl Pts',(-2.85539439105084,4.55994605023122,
6.66402454108774));
#144256=CARTESIAN_POINT('Ctrl Pts',(-3.554702037,4.430609079,6.318749356));
#144257=CARTESIAN_POINT('Ctrl Pts',(-3.212299413,4.495496505,6.511372807));
#144258=CARTESIAN_POINT('Ctrl Pts',(-2.851086974,4.560723991,6.665868515));
#144259=CARTESIAN_POINT('Ctrl Pts',(-3.460928151,4.430609079,6.653718985));
#144260=CARTESIAN_POINT('Ctrl Pts',(-3.100374075,4.495496505,6.841260983));
#144261=CARTESIAN_POINT('Ctrl Pts',(-2.721665569,4.560723991,6.988743559));
#144262=CARTESIAN_POINT('Origin',(0.0793335642572862,4.55356866085514,-0.182514228437093));
#144263=CARTESIAN_POINT('Ctrl Pts',(-4.225076389,4.560731746,5.891623674));
#144264=CARTESIAN_POINT('Ctrl Pts',(-3.901614248,4.495065281,6.123588974));
#144265=CARTESIAN_POINT('Ctrl Pts',(-3.554702037,4.430609079,6.318749356));
#144266=CARTESIAN_POINT('Ctrl Pts',(-4.568298544,4.560731746,5.948163449));
#144267=CARTESIAN_POINT('Ctrl Pts',(-4.241732254,4.495065281,6.198972345));
#144268=CARTESIAN_POINT('Ctrl Pts',(-3.889671666,4.430609079,6.412523242));
#144269=CARTESIAN_POINT('',(-4.22120514517481,4.55994605119118,5.8943979632248));
#144270=CARTESIAN_POINT('Origin',(0.129005056016454,4.69628090110764,-0.141357475232535));
#144271=CARTESIAN_POINT('Ctrl Pts',(-4.36592121772473,4.52063234083099,
6.09825646575287));
#144272=CARTESIAN_POINT('Ctrl Pts',(-4.34180743928622,4.52686606998888,
6.0642256277437));
#144273=CARTESIAN_POINT('Ctrl Pts',(-4.31767917226126,4.53325386248918,
6.0302037307579));
#144274=CARTESIAN_POINT('Ctrl Pts',(-4.26944945116903,4.54634733287894,
5.96226166741484));
#144275=CARTESIAN_POINT('Ctrl Pts',(-4.24531981791809,4.553060653944,5.92830180049015));
#144276=CARTESIAN_POINT('Ctrl Pts',(-4.22120514626668,4.55994605018937,
5.89439796224474));
#144277=CARTESIAN_POINT('Ctrl Pts',(-4.829939409,4.430609079,5.406864646));
#144278=CARTESIAN_POINT('Ctrl Pts',(-4.536950317,4.495496505,5.66859111));
#144279=CARTESIAN_POINT('Ctrl Pts',(-4.217394834,4.560723991,5.89712479200001));
#144280=CARTESIAN_POINT('Ctrl Pts',(-4.810366473,4.430609079,5.754161485));
#144281=CARTESIAN_POINT('Ctrl Pts',(-4.498557937,4.495496505,6.014827323));
#144282=CARTESIAN_POINT('Ctrl Pts',(-4.16040782,4.560723991,6.240272973));
#144283=CARTESIAN_POINT('Origin',(0.11671398827705,4.55356860863053,-0.161192793785231));
#144284=CARTESIAN_POINT('Ctrl Pts',(-5.392821385,4.560731746,4.845614255));
#144285=CARTESIAN_POINT('Ctrl Pts',(-5.126787292,4.495065281,5.141691134));
#144286=CARTESIAN_POINT('Ctrl Pts',(-4.829939409,4.430609079,5.406864646));
#144287=CARTESIAN_POINT('Ctrl Pts',(-5.74017357700001,4.560731746,4.827049544));
#144288=CARTESIAN_POINT('Ctrl Pts',(-5.475158725,4.495065281,5.142196766));
#144289=CARTESIAN_POINT('Ctrl Pts',(-5.177236248,4.430609079,5.426437582));
#144290=CARTESIAN_POINT('',(-5.38963703994329,4.5599460529448,4.84915588573557));
#144291=CARTESIAN_POINT('Origin',(0.156376705075179,4.69628091630223,-0.110320379162516));
#144292=CARTESIAN_POINT('Ctrl Pts',(-5.57479328282146,4.52063234083508,
5.01713861212511));
#144293=CARTESIAN_POINT('Ctrl Pts',(-5.54392760548432,4.52686607834886,
4.98908710816598));
#144294=CARTESIAN_POINT('Ctrl Pts',(-5.51304976423063,4.53325386650049,
4.96104750887774));
#144295=CARTESIAN_POINT('Ctrl Pts',(-5.45134211096737,4.54634733285367,
4.90506187481746));
#144296=CARTESIAN_POINT('Ctrl Pts',(-5.42047624750108,4.55306065394299,
4.8770831284614));
#144297=CARTESIAN_POINT('Ctrl Pts',(-5.38963704040105,4.55994605021047,
4.84915588455593));
#144298=CARTESIAN_POINT('Ctrl Pts',(-5.879334183,4.430609079,4.242160954));
#144299=CARTESIAN_POINT('Ctrl Pts',(-5.649458466,4.495496505,4.560752393));
#144300=CARTESIAN_POINT('Ctrl Pts',(-5.386501999,4.560723991,4.852638067));
#144301=CARTESIAN_POINT('Ctrl Pts',(-5.934877406,4.430609079,4.585545789));
#144302=CARTESIAN_POINT('Ctrl Pts',(-5.68639423,4.495496505,4.907147023));
#144303=CARTESIAN_POINT('Ctrl Pts',(-5.404614025,4.560723991,5.200014158));
#144304=CARTESIAN_POINT('Origin',(0.148636968836049,4.55356862890809,-0.132334142890484));
#144305=CARTESIAN_POINT('Ctrl Pts',(-6.308404047,4.560731746,3.573029299));
#144306=CARTESIAN_POINT('Ctrl Pts',(-6.112237461,4.495065281,3.919373532));
#144307=CARTESIAN_POINT('Ctrl Pts',(-5.879334183,4.430609079,4.242160954));
#144308=CARTESIAN_POINT('Ctrl Pts',(-6.643644474,4.560731746,3.480228168));
#144309=CARTESIAN_POINT('Ctrl Pts',(-6.452572859,4.495065281,3.844977782));
#144310=CARTESIAN_POINT('Ctrl Pts',(-6.222719017,4.430609079,4.186617732));
#144311=CARTESIAN_POINT('',(-6.30605549550747,4.55994605292005,3.57717266853147));
#144312=CARTESIAN_POINT('Origin',(0.176436100078936,4.69628087970373,-0.0741246307395643));
#144313=CARTESIAN_POINT('Ctrl Pts',(-6.52299420951789,4.5206323408474,3.7014249337822));
#144314=CARTESIAN_POINT('Ctrl Pts',(-6.48681995482906,4.52686607071593,
3.68066449205128));
#144315=CARTESIAN_POINT('Ctrl Pts',(-6.45063631117384,4.53325386286174,
3.65991825214407));
#144316=CARTESIAN_POINT('Ctrl Pts',(-6.37833607187533,4.54634733289592,
3.61850684058568));
#144317=CARTESIAN_POINT('Ctrl Pts',(-6.34217723114368,4.55306065409343,
3.59781746951568));
#144318=CARTESIAN_POINT('Ctrl Pts',(-6.30605549594104,4.55994605029829,
3.57717266689845));
#144319=CARTESIAN_POINT('Ctrl Pts',(-6.653817825,4.430609079,2.879098531));
#144320=CARTESIAN_POINT('Ctrl Pts',(-6.497804216,4.495496505,3.239657963));
#144321=CARTESIAN_POINT('Ctrl Pts',(-6.303742317,4.560723991,3.58124738));
#144322=CARTESIAN_POINT('Ctrl Pts',(-6.781880067,4.430609079,3.202515068));
#144323=CARTESIAN_POINT('Ctrl Pts',(-6.60834104800001,4.495496505,3.570013982));
#144324=CARTESIAN_POINT('Ctrl Pts',(-6.396106485,4.560723991,3.916608461));
#144325=CARTESIAN_POINT('Origin',(0.173609964768517,4.55356862217885,-0.097287761415224));
#144326=CARTESIAN_POINT('Ctrl Pts',(-6.929012748,4.560731746,2.133373465));
#144327=CARTESIAN_POINT('Ctrl Pts',(-6.811886199,4.495065281,2.513790379));
#144328=CARTESIAN_POINT('Ctrl Pts',(-6.653817825,4.430609079,2.879098531));
#144329=CARTESIAN_POINT('Ctrl Pts',(-7.23646594,4.560731746,1.97067519));
#144330=CARTESIAN_POINT('Ctrl Pts',(-7.128271858,4.495065281,2.36797191));
#144331=CARTESIAN_POINT('Ctrl Pts',(-6.977234361,4.430609079,2.751036289));
#144332=CARTESIAN_POINT('',(-6.92760980555269,4.55994605295033,2.13792483369843));
#144333=CARTESIAN_POINT('Origin',(0.188246019437727,4.69628090910426,-0.0344631924695157));
#144334=CARTESIAN_POINT('Ctrl Pts',(-7.16618717754861,4.52063234083719,
2.21263673886221));
#144335=CARTESIAN_POINT('Ctrl Pts',(-7.12639577943664,4.52686607009583,
2.20013806147034));
#144336=CARTESIAN_POINT('Ctrl Pts',(-7.08659825869315,4.53325386258683,
2.18765527027095));
#144337=CARTESIAN_POINT('Ctrl Pts',(-7.00708612763528,4.54634733295565,
2.16275444828854));
#144338=CARTESIAN_POINT('Ctrl Pts',(-6.96732505701765,4.55306065423035,
2.15032186507111));
#144339=CARTESIAN_POINT('Ctrl Pts',(-6.92760980569743,4.5599460504648,2.13792483185427));
#144340=CARTESIAN_POINT('Ctrl Pts',(-7.11717634,4.430609079,1.381412661));
#144341=CARTESIAN_POINT('Ctrl Pts',(-7.04231986300001,4.495496505,1.767080728));
#144342=CARTESIAN_POINT('Ctrl Pts',(-6.926226651,4.560723991,2.142401545));
#144343=CARTESIAN_POINT('Ctrl Pts',(-7.311769554,4.430609079,1.669738302));
#144344=CARTESIAN_POINT('Ctrl Pts',(-7.221289184,4.495496505,2.065951054));
#144345=CARTESIAN_POINT('Ctrl Pts',(-7.08852411500001,4.560723991,2.450066505));
#144346=CARTESIAN_POINT('Origin',(0.190464918460429,4.55356864800771,-0.0576921838180541));
#144347=CARTESIAN_POINT('Ctrl Pts',(-7.22562851299999,4.560731746,0.593963458000001));
#144348=CARTESIAN_POINT('Ctrl Pts',(-7.193018709,4.495065281,0.990665182));
#144349=CARTESIAN_POINT('Ctrl Pts',(-7.11717634,4.430609079,1.381412661));
#144350=CARTESIAN_POINT('Ctrl Pts',(-7.4909183,4.560731746,0.36897563));
#144351=CARTESIAN_POINT('Ctrl Pts',(-7.470660787,4.495065281,0.780242304));
#144352=CARTESIAN_POINT('Ctrl Pts',(-7.405501982,4.430609079,1.186819448));
#144353=CARTESIAN_POINT('',(-7.22523678108189,4.55994605191336,0.598710009952617));
#144354=CARTESIAN_POINT('Origin',(0.191253352314371,4.69628107715055,0.006809920091582));
#144355=CARTESIAN_POINT('Ctrl Pts',(-7.47429719712508,4.52063234086681,
0.620388109190184));
#144356=CARTESIAN_POINT('Ctrl Pts',(-7.43274924743436,4.52686607103456,
0.616735617684281));
#144357=CARTESIAN_POINT('Ctrl Pts',(-7.39119874307093,4.53325386299204,
0.613099958047266));
#144358=CARTESIAN_POINT('Ctrl Pts',(-7.30819262379926,4.54634733285042,
0.605874061569169));
#144359=CARTESIAN_POINT('Ctrl Pts',(-7.26668850755719,4.55306065402255,
0.602279600214153));
#144360=CARTESIAN_POINT('Ctrl Pts',(-7.22523678098004,4.55994605025539,
0.598710007937322));
#144361=CARTESIAN_POINT('Ctrl Pts',(-7.2477436,4.430609079,-0.180866531));
#144362=CARTESIAN_POINT('Ctrl Pts',(-7.25754446000001,4.495496505,0.211876761));
#144363=CARTESIAN_POINT('Ctrl Pts',(-7.22484832400001,4.560723991,0.603379396));
#144364=CARTESIAN_POINT('Ctrl Pts',(-7.499768822,4.430609079,0.0588864280000001));
#144365=CARTESIAN_POINT('Ctrl Pts',(-7.496577864,4.495496505,0.465286552));
#144366=CARTESIAN_POINT('Ctrl Pts',(-7.449490235,4.560723991,0.868962162));
#144367=CARTESIAN_POINT('Origin',(0.198414091241863,4.55356862013888,-0.015399037139459));
#144368=CARTESIAN_POINT('Ctrl Pts',(-7.18438192,4.560731746,-0.97321962));
#144369=CARTESIAN_POINT('Ctrl Pts',(-7.23781366,4.495065281,-0.578782418));
#144370=CARTESIAN_POINT('Ctrl Pts',(-7.2477436,4.430609079,-0.180866531));
#144371=CARTESIAN_POINT('Ctrl Pts',(-7.39510364700001,4.560731746,-1.24997682));
#144372=CARTESIAN_POINT('Ctrl Pts',(-7.463729921,4.495065281,-0.843970566000001));
#144373=CARTESIAN_POINT('Ctrl Pts',(-7.48749656,4.430609079,-0.432891753));
#144374=CARTESIAN_POINT('',(-7.18501971399298,4.55994605292029,-0.968499829450406));
#144375=CARTESIAN_POINT('Origin',(0.185317934164564,4.69628089020531,0.0477644810005477));
#144376=CARTESIAN_POINT('Ctrl Pts',(-7.43291738742458,4.52063234081501,
-1.00086917885161));
#144377=CARTESIAN_POINT('Ctrl Pts',(-7.39155563326788,4.52686607020261,
-0.995504696753631));
#144378=CARTESIAN_POINT('Ctrl Pts',(-7.35019499414071,4.53325386262189,
-0.99012322604503));
#144379=CARTESIAN_POINT('Ctrl Pts',(-7.26757615490632,4.54634733292811,
-0.979336322679522));
#144380=CARTESIAN_POINT('Ctrl Pts',(-7.22626967855141,4.55306065415589,
-0.973924589329539));
#144381=CARTESIAN_POINT('Ctrl Pts',(-7.18501971341777,4.55994605038715,
-0.968499830609143));
#144382=CARTESIAN_POINT('Ctrl Pts',(-7.039414425,4.430609079,-1.734688604));
#144383=CARTESIAN_POINT('Ctrl Pts',(-7.133414344,4.495496505,-1.353234327));
#144384=CARTESIAN_POINT('Ctrl Pts',(-7.185644119,4.560723991,-0.963856104));
#144385=CARTESIAN_POINT('Ctrl Pts',(-7.337087236,4.430609079,-1.554718909));
#144386=CARTESIAN_POINT('Ctrl Pts',(-7.421334894,4.495496505,-1.157134232));
#144387=CARTESIAN_POINT('Ctrl Pts',(-7.462126472,4.560723991,-0.752773886));
#144388=CARTESIAN_POINT('Origin',(0.197085704958381,4.55356864071035,0.0276141514613945));
#144389=CARTESIAN_POINT('Ctrl Pts',(-6.807201613,4.560731746,-2.49489603));
#144390=CARTESIAN_POINT('Ctrl Pts',(-6.94417648700001,4.495065281,-2.121166795));
#144391=CARTESIAN_POINT('Ctrl Pts',(-7.039414425,4.430609079,-1.734688604));
#144392=CARTESIAN_POINT('Ctrl Pts',(-6.953502166,4.560731746,-2.810481743));
#144393=CARTESIAN_POINT('Ctrl Pts',(-7.107803339,4.495065281,-2.428720309));
#144394=CARTESIAN_POINT('Ctrl Pts',(-7.21938412,4.430609079,-2.032361415));
#144395=CARTESIAN_POINT('',(-6.80883911175384,4.5599460529445,-2.49042369268795));
#144396=CARTESIAN_POINT('Origin',(0.170717629805369,4.69628090722908,0.0864857378835263));
#144397=CARTESIAN_POINT('Ctrl Pts',(-7.043982621342,4.52063234084788,-2.57532693620973));
#144398=CARTESIAN_POINT('Ctrl Pts',(-7.00474108494821,4.52686607057047,
-2.56119631750548));
#144399=CARTESIAN_POINT('Ctrl Pts',(-6.9655042930369,4.5332538627838,-2.54704934835764));
#144400=CARTESIAN_POINT('Ctrl Pts',(-6.88713590294052,4.54634733289551,
-2.51875402924257));
#144401=CARTESIAN_POINT('Ctrl Pts',(-6.84795851182919,4.55306065412239,
-2.50458914798822));
#144402=CARTESIAN_POINT('Ctrl Pts',(-6.80883911077304,4.55994605037372,
-2.49042369414695));
#144403=CARTESIAN_POINT('Ctrl Pts',(-6.501930055,4.430609079,-3.207398566));
#144404=CARTESIAN_POINT('Ctrl Pts',(-6.675733702,4.495496505,-2.855069682));
#144405=CARTESIAN_POINT('Ctrl Pts',(-6.81044718200001,4.560723991,-2.486022764));
#144406=CARTESIAN_POINT('Ctrl Pts',(-6.831331606,4.430609079,-3.095627318));
#144407=CARTESIAN_POINT('Ctrl Pts',(-6.999078553,4.495496505,-2.725448706));
#144408=CARTESIAN_POINT('Ctrl Pts',(-7.12584196800001,4.560723991,-2.339311063));
#144409=CARTESIAN_POINT('Origin',(0.186541774057719,4.55356866174391,0.0693361714658935));
#144410=CARTESIAN_POINT('Ctrl Pts',(-6.111724124,4.560731746,-3.899913875));
#144411=CARTESIAN_POINT('Ctrl Pts',(-6.32583734,4.495065281,-3.564367771));
#144412=CARTESIAN_POINT('Ctrl Pts',(-6.501930055,4.430609079,-3.207398566));
#144413=CARTESIAN_POINT('Ctrl Pts',(-6.186762652,4.560731746,-4.239571663));
#144414=CARTESIAN_POINT('Ctrl Pts',(-6.419523772,4.495065281,-3.899905791));
#144415=CARTESIAN_POINT('Ctrl Pts',(-6.61370130300001,4.430609079,-3.536800117));
#144416=CARTESIAN_POINT('',(-6.11428476024427,4.55994605194144,-3.89589811155743));
#144417=CARTESIAN_POINT('Origin',(0.148134494419526,4.69628102985038,0.121163037151322));
#144418=CARTESIAN_POINT('Ctrl Pts',(-6.32567905648816,4.52063234086436,
-4.02936526868397));
#144419=CARTESIAN_POINT('Ctrl Pts',(-6.29039262764739,4.52686607114115,
-4.00712924358968));
#144420=CARTESIAN_POINT('Ctrl Pts',(-6.25511435220891,4.53325386303843,
-3.98487827339725));
#144421=CARTESIAN_POINT('Ctrl Pts',(-6.18466083040304,4.54634733283927,
-3.94039759680153));
#144422=CARTESIAN_POINT('Ctrl Pts',(-6.14944441594127,4.55306065401075,
-3.91814190177734));
#144423=CARTESIAN_POINT('Ctrl Pts',(-6.1142847585915,4.55994605024559,-3.89589811364495));
#144424=CARTESIAN_POINT('Ctrl Pts',(-5.660422662,4.430609079,-4.530134136));
#144425=CARTESIAN_POINT('Ctrl Pts',(-5.905903171,4.495496505,-4.223405152));
#144426=CARTESIAN_POINT('Ctrl Pts',(-6.116801304,4.560723991,-3.891945762));
#144427=CARTESIAN_POINT('Ctrl Pts',(-6.006150502,4.430609079,-4.491787634));
#144428=CARTESIAN_POINT('Ctrl Pts',(-6.249553078,4.495496505,-4.166324228));
#144429=CARTESIAN_POINT('Ctrl Pts',(-6.456361013,4.560723991,-3.816464655));
#144430=CARTESIAN_POINT('Origin',(0.167275480686609,4.55356864254791,0.107816230719945));
#144431=CARTESIAN_POINT('Ctrl Pts',(-5.130469208,4.560731746,-5.12257608100001));
#144432=CARTESIAN_POINT('Ctrl Pts',(-5.41170907,4.495065281,-4.840902871));
#144433=CARTESIAN_POINT('Ctrl Pts',(-5.660422662,4.430609079,-4.530134136));
#144434=CARTESIAN_POINT('Ctrl Pts',(-5.130736993,4.560731746,-5.47042392400001));
#144435=CARTESIAN_POINT('Ctrl Pts',(-5.431074409,4.495065281,-5.188736012));
#144436=CARTESIAN_POINT('Ctrl Pts',(-5.698769164,4.430609079,-4.875861977));
#144437=CARTESIAN_POINT('',(-5.13383324781926,4.55994605191712,-5.11920466472031));
#144438=CARTESIAN_POINT('Origin',(0.11862458411485,4.69628102230035,0.15017473185948));
#144439=CARTESIAN_POINT('Ctrl Pts',(-5.31159377015465,4.52063234085165,
-5.29499495952915));
#144440=CARTESIAN_POINT('Ctrl Pts',(-5.28191237189894,4.52686607840367,
-5.26569322704215));
#144441=CARTESIAN_POINT('Ctrl Pts',(-5.25224220241832,4.53325386656604,
-5.2363787040736));
#144442=CARTESIAN_POINT('Ctrl Pts',(-5.19299789108451,4.54634733290202,
-5.17779255156786));
#144443=CARTESIAN_POINT('Ctrl Pts',(-5.16338913336468,4.55306065406917,
-5.14848669395028));
#144444=CARTESIAN_POINT('Ctrl Pts',(-5.13383324626273,4.55994605026984,
-5.11920466590405));
#144445=CARTESIAN_POINT('Ctrl Pts',(-4.554240196,4.430609079,-5.641045669));
#144446=CARTESIAN_POINT('Ctrl Pts',(-4.859919172,4.495496505,-5.394258892));
#144447=CARTESIAN_POINT('Ctrl Pts',(-5.13714059500001,4.560723991,-5.11588570100001));
#144448=CARTESIAN_POINT('Ctrl Pts',(-4.900128476,4.430609079,-5.677916952));
#144449=CARTESIAN_POINT('Ctrl Pts',(-5.207805447,4.495496505,-5.412387059));
#144450=CARTESIAN_POINT('Ctrl Pts',(-5.48498779400001,4.560723991,-5.115164602));
#144451=CARTESIAN_POINT('Origin',(0.14018715816885,4.55356858826164,0.141254600293736));
#144452=CARTESIAN_POINT('Ctrl Pts',(-3.909319254,4.560731746,-6.105712323));
#144453=CARTESIAN_POINT('Ctrl Pts',(-4.244535298,4.495065281,-5.891082733));
#144454=CARTESIAN_POINT('Ctrl Pts',(-4.554240196,4.430609079,-5.64104566900001));
#144455=CARTESIAN_POINT('Ctrl Pts',(-3.834803774,4.560731746,-6.44548524300001));
#144456=CARTESIAN_POINT('Ctrl Pts',(-4.188674043,4.495065281,-6.234946704));
#144457=CARTESIAN_POINT('Ctrl Pts',(-4.517368912,4.430609079,-5.98693394900001));
#144458=CARTESIAN_POINT('',(-3.9133293995001,4.55994605192187,-6.10314289857883));
#144459=CARTESIAN_POINT('Origin',(0.0835682302581803,4.69628105622506,0.172164714886408));
#144460=CARTESIAN_POINT('Ctrl Pts',(-4.04914426237964,4.52063234081625,
-6.31303657046451));
#144461=CARTESIAN_POINT('Ctrl Pts',(-4.02645583639726,4.52686606975115,
-6.27803932140012));
#144462=CARTESIAN_POINT('Ctrl Pts',(-4.00378107790903,4.5332538623673,-6.24303192029104));
#144463=CARTESIAN_POINT('Ctrl Pts',(-3.95851614221154,4.54634733286745,
-6.17307968194309));
#144464=CARTESIAN_POINT('Ctrl Pts',(-3.93589951412824,4.553060653963,-6.13809397195535));
#144465=CARTESIAN_POINT('Ctrl Pts',(-3.91332939753393,4.55994605021214,
-6.10314289951169));
#144466=CARTESIAN_POINT('Ctrl Pts',(-3.23510652,4.430609079,-6.488188176));
#144467=CARTESIAN_POINT('Ctrl Pts',(-3.586690754,4.495496505,-6.31288308));
#144468=CARTESIAN_POINT('Ctrl Pts',(-3.917272901,4.560723991,-6.100612512));
#144469=CARTESIAN_POINT('Ctrl Pts',(-3.564981888,4.430609079,-6.59855318500001));
#144470=CARTESIAN_POINT('Ctrl Pts',(-3.922546621,4.495496505,-6.405372686));
#144471=CARTESIAN_POINT('Ctrl Pts',(-4.257142641,4.560723991,-6.174685136));
#144472=CARTESIAN_POINT('Origin',(0.106544188479404,4.55356864375883,0.16808840343761));
#144473=CARTESIAN_POINT('Ctrl Pts',(-2.505373877,4.560731746,-6.803352243));
#144474=CARTESIAN_POINT('Ctrl Pts',(-2.878891773,4.495065281,-6.665802114));
#144475=CARTESIAN_POINT('Ctrl Pts',(-3.23510652,4.430609079,-6.488188176));
#144476=CARTESIAN_POINT('Ctrl Pts',(-2.359559393,4.560731746,-7.119162835));
#144477=CARTESIAN_POINT('Ctrl Pts',(-2.750415934,4.495065281,-6.98961821800001));
#144478=CARTESIAN_POINT('Ctrl Pts',(-3.124741511,4.430609079,-6.818063544));
#144479=CARTESIAN_POINT('',(-2.50984261641909,4.5599460529582,-6.80170495217655));
#144480=CARTESIAN_POINT('Origin',(0.0446040535887426,4.69628092221338,0.186104077523651));
#144481=CARTESIAN_POINT('Ctrl Pts',(-2.5973612689532,4.52063234086582,-7.03588760830941));
#144482=CARTESIAN_POINT('Ctrl Pts',(-2.58272665904205,4.52686607014102,
-6.99683123235439));
#144483=CARTESIAN_POINT('Ctrl Pts',(-2.5681075806911,4.53325386260306,-6.95776788295559));
#144484=CARTESIAN_POINT('Ctrl Pts',(-2.53893857804763,4.54634733296754,
-6.87972046655687));
#144485=CARTESIAN_POINT('Ctrl Pts',(-2.52437160761346,4.5530606541495,-6.84069079594136));
#144486=CARTESIAN_POINT('Ctrl Pts',(-2.50984261543137,4.55994605040824,
-6.80170495209429));
#144487=CARTESIAN_POINT('Ctrl Pts',(-1.764702859,4.430609079,-7.03195021400001));
#144488=CARTESIAN_POINT('Ctrl Pts',(-2.145752663,4.495496505,-6.936323872));
#144489=CARTESIAN_POINT('Ctrl Pts',(-2.51423788,4.560723991,-6.800081461));
#144490=CARTESIAN_POINT('Ctrl Pts',(-2.06314071,4.430609079,-7.210648404));
#144491=CARTESIAN_POINT('Ctrl Pts',(-2.453873874,4.495496505,-7.098850206));
#144492=CARTESIAN_POINT('Ctrl Pts',(-2.83023823,4.560723991,-6.94548425700001));
#144493=CARTESIAN_POINT('Origin',(0.067919130555496,4.55356865389157,0.187062182693583));
#144494=CARTESIAN_POINT('Ctrl Pts',(-0.984280001000001,4.560731746,-7.182874973));
#144495=CARTESIAN_POINT('Ctrl Pts',(-1.378634468,4.495065281,-7.128835996));
#144496=CARTESIAN_POINT('Ctrl Pts',(-1.764702859,4.430609079,-7.03195021400001));
#144497=CARTESIAN_POINT('Ctrl Pts',(-0.773984637,4.560731746,-7.45995628600001));
#144498=CARTESIAN_POINT('Ctrl Pts',(-1.183551433,4.495065281,-7.417462952));
#144499=CARTESIAN_POINT('Ctrl Pts',(-1.586004669,4.430609079,-7.330388065));
#144500=CARTESIAN_POINT('',(-0.988998383218425,4.55994605292971,-7.18222684270952));
#144501=CARTESIAN_POINT('Origin',(0.00355437245004808,4.69628093008518,
0.191341631742465));
#144502=CARTESIAN_POINT('Ctrl Pts',(-1.02412854958252,4.52063234085322,
-7.42974836134486));
#144503=CARTESIAN_POINT('Ctrl Pts',(-1.01823205495643,4.52686607013125,
-7.38845909318625));
#144504=CARTESIAN_POINT('Ctrl Pts',(-1.01235222786182,4.53325386256596,
-7.34716635363535));
#144505=CARTESIAN_POINT('Ctrl Pts',(-1.00064306753655,4.54634733286283,
-7.26467316949526));
#144506=CARTESIAN_POINT('Ctrl Pts',(-0.994806890059503,4.55306065407803,
-7.22342452261306));
#144507=CARTESIAN_POINT('Ctrl Pts',(-0.988998381499585,4.55994605029681,
-7.18222684251182));
#144508=CARTESIAN_POINT('Ctrl Pts',(-0.211783654,4.430609079,-7.246906077));
#144509=CARTESIAN_POINT('Ctrl Pts',(-0.604481562,4.495496505,-7.235429869));
#144510=CARTESIAN_POINT('Ctrl Pts',(-0.993639891,4.560723991,-7.18158616));
#144511=CARTESIAN_POINT('Ctrl Pts',(-0.464829365,4.430609079,-7.485581718));
#144512=CARTESIAN_POINT('Ctrl Pts',(-0.870460713,4.495496505,-7.46039338));
#144513=CARTESIAN_POINT('Ctrl Pts',(-1.270995025,4.560723991,-7.391520253));
#144514=CARTESIAN_POINT('Origin',(0.0261184061916772,4.5535686433715,0.197289686172826));
#144515=CARTESIAN_POINT('Ctrl Pts',(0.582837713,4.560731746,-7.226534453));
#144516=CARTESIAN_POINT('Ctrl Pts',(0.186086252,4.495065281,-7.258533431));
#144517=CARTESIAN_POINT('Ctrl Pts',(-0.211783654,4.430609079,-7.246906077));
#144518=CARTESIAN_POINT('Ctrl Pts',(0.847780781,4.560731746,-7.451930471));
#144519=CARTESIAN_POINT('Ctrl Pts',(0.438654618,4.495065281,-7.498475363));
#144520=CARTESIAN_POINT('Ctrl Pts',(0.026891988,4.430609079,-7.499951788));
#144521=CARTESIAN_POINT('',(0.578090315769926,4.55994605294543,-7.22691578804906));
#144522=CARTESIAN_POINT('Origin',(-0.037661533011655,4.6962809452755,0.187632234919998));
#144523=CARTESIAN_POINT('Ctrl Pts',(0.596991283107554,4.52063234082553,
-7.47620233865752));
#144524=CARTESIAN_POINT('Ctrl Pts',(0.593873944611452,4.52686607835563,
-7.43461076353673));
#144525=CARTESIAN_POINT('Ctrl Pts',(0.590739588336727,4.533253866525,-7.39301946604933));
#144526=CARTESIAN_POINT('Ctrl Pts',(0.58444140058795,4.54634733287727,-7.30993782852142));
#144527=CARTESIAN_POINT('Ctrl Pts',(0.581273891583123,4.55306065410427,
-7.26839894647494));
#144528=CARTESIAN_POINT('Ctrl Pts',(0.578090316875135,4.55994605036328,
-7.22691578753565));
#144529=CARTESIAN_POINT('Ctrl Pts',(1.35103832,4.430609079,-7.123004665));
#144530=CARTESIAN_POINT('Ctrl Pts',(0.965054425,4.495496505,-7.196215207));
#144531=CARTESIAN_POINT('Ctrl Pts',(0.573419596,4.560723991,-7.227287871));
#144532=CARTESIAN_POINT('Ctrl Pts',(1.155216884,4.430609079,-7.410497551));
#144533=CARTESIAN_POINT('Ctrl Pts',(0.753654224,4.495496505,-7.473096852));
#144534=CARTESIAN_POINT('Ctrl Pts',(0.347678495,4.560723991,-7.491936977));
#144535=CARTESIAN_POINT('Origin',(-0.0169036609393039,4.55356866514041,
0.198291733154583));
#144536=CARTESIAN_POINT('Ctrl Pts',(2.122702584,4.560731746,-6.932289213));
#144537=CARTESIAN_POINT('Ctrl Pts',(1.742105785,4.495065281,-7.04882990900001));
#144538=CARTESIAN_POINT('Ctrl Pts',(1.35103832,4.430609079,-7.123004665));
#144539=CARTESIAN_POINT('Ctrl Pts',(2.429904911,4.560731746,-7.09546067));
#144540=CARTESIAN_POINT('Ctrl Pts',(2.040349667,4.495065281,-7.2288674));
#144541=CARTESIAN_POINT('Ctrl Pts',(1.638531205,4.430609079,-7.3188261));
#144542=CARTESIAN_POINT('',(2.11814815318168,4.5599460529599,-6.93368218303114));
#144543=CARTESIAN_POINT('Origin',(-0.0771164253400619,4.69628089233295,
0.17514947035037));
#144544=CARTESIAN_POINT('Ctrl Pts',(2.19019646628858,4.5206323408352,-7.1730774035426));
#144545=CARTESIAN_POINT('Ctrl Pts',(2.17821106626066,4.52686607006686,-7.13312840511856));
#144546=CARTESIAN_POINT('Ctrl Pts',(2.16620908142545,4.53325386254879,-7.09318325407002));
#144547=CARTESIAN_POINT('Ctrl Pts',(2.14219803858705,4.54634733288281,-7.0133979188787));
#144548=CARTESIAN_POINT('Ctrl Pts',(2.13017495246057,4.55306065418219,-6.9735111131108));
#144549=CARTESIAN_POINT('Ctrl Pts',(2.11814815529179,4.55994605040166,-6.93368218195171));
#144550=CARTESIAN_POINT('Ctrl Pts',(2.850687243,4.430609079,-6.666039472));
#144551=CARTESIAN_POINT('Ctrl Pts',(2.48946554,4.495496505,-6.82051352));
#144552=CARTESIAN_POINT('Ctrl Pts',(2.11366662,4.560723991,-6.935049634));
#144553=CARTESIAN_POINT('Ctrl Pts',(2.721246476,4.430609079,-6.988906754));
#144554=CARTESIAN_POINT('Ctrl Pts',(2.342529127,4.495496505,-7.13636662));
#144555=CARTESIAN_POINT('Ctrl Pts',(1.950094955,4.560723991,-7.242039054));
#144556=CARTESIAN_POINT('Origin',(-0.059135311493016,4.55356865186134,0.190021965440517));
#144557=CARTESIAN_POINT('Ctrl Pts',(3.563312241,4.560731746,-6.313897835));
#144558=CARTESIAN_POINT('Ctrl Pts',(3.216666389,4.495065281,-6.509530936));
#144559=CARTESIAN_POINT('Ctrl Pts',(2.850687243,4.430609079,-6.666039472));
#144560=CARTESIAN_POINT('Ctrl Pts',(3.898409388,4.560731746,-6.407215015));
#144561=CARTESIAN_POINT('Ctrl Pts',(3.546640232,4.495065281,-6.621245631));
#144562=CARTESIAN_POINT('Ctrl Pts',(3.173554525,4.430609079,-6.79548023900001));
#144563=CARTESIAN_POINT('',(3.55916373788445,4.55994605292436,-6.31623730607955));
#144564=CARTESIAN_POINT('Origin',(-0.112965338102915,4.69628090859361,0.154476604965065));
#144565=CARTESIAN_POINT('Ctrl Pts',(3.68099049666106,4.52063234085873,-6.53454734171104));
#144566=CARTESIAN_POINT('Ctrl Pts',(3.66069745650017,4.52686606958346,-6.49810883839098));
#144567=CARTESIAN_POINT('Ctrl Pts',(3.64038904380658,4.53325386231883,-6.46167765320372));
#144568=CARTESIAN_POINT('Ctrl Pts',(3.59978787616399,4.54634733292843,-6.38891931766763));
#144569=CARTESIAN_POINT('Ctrl Pts',(3.57947139933409,4.55306065404519,-6.35254965228119));
#144570=CARTESIAN_POINT('Ctrl Pts',(3.559163738865,4.55994605028106,-6.31623730502997));
#144571=CARTESIAN_POINT('Ctrl Pts',(4.217041199,4.430609079,-5.897377682));
#144572=CARTESIAN_POINT('Ctrl Pts',(3.897472013,4.495496505,-6.125892201));
#144573=CARTESIAN_POINT('Ctrl Pts',(3.555080941,4.560723991,-6.31853618300001));
#144574=CARTESIAN_POINT('Ctrl Pts',(4.160033607,4.430609079,-6.240522445));
#144575=CARTESIAN_POINT('Ctrl Pts',(3.821869971,4.495496505,-6.465947816));
#144576=CARTESIAN_POINT('Ctrl Pts',(3.461327142,4.560723991,-6.65351143500001));
#144577=CARTESIAN_POINT('Origin',(-0.0986017871400374,4.55356862974844,
0.172866876305883));
#144578=CARTESIAN_POINT('Ctrl Pts',(4.837305378,4.560731746,-5.400275611));
#144579=CARTESIAN_POINT('Ctrl Pts',(4.540819247,4.495065281,-5.66585353));
#144580=CARTESIAN_POINT('Ctrl Pts',(4.217041199,4.430609079,-5.897377682));
#144581=CARTESIAN_POINT('Ctrl Pts',(5.184628575,4.560731746,-5.419375106));
#144582=CARTESIAN_POINT('Ctrl Pts',(4.88709384300001,4.495065281,-5.704021776));
#144583=CARTESIAN_POINT('Ctrl Pts',(4.56018596200001,4.430609079,-5.954385274));
#144584=CARTESIAN_POINT('',(4.83375678100281,4.55994605293975,-5.40345219171606));
#144585=CARTESIAN_POINT('Origin',(-0.143532263022277,4.69628092208878,0.126580913645621));
#144586=CARTESIAN_POINT('Ctrl Pts',(4.99966550307942,4.52063234090427,-5.5904691084804));
#144587=CARTESIAN_POINT('Ctrl Pts',(4.97201370358798,4.52686606921442,-5.55924492289589));
#144588=CARTESIAN_POINT('Ctrl Pts',(4.94434846128484,4.53325386217182,-5.52803118575706));
#144589=CARTESIAN_POINT('Ctrl Pts',(4.88905563426124,4.54634733293204,-5.46570194974545));
#144590=CARTESIAN_POINT('Ctrl Pts',(4.86139574168964,4.55306065422027,-5.43455002807531));
#144591=CARTESIAN_POINT('Ctrl Pts',(4.83375678201757,4.55994605041382,-5.40345219025491));
#144592=CARTESIAN_POINT('Ctrl Pts',(5.386210996,4.430609079,-4.852961066));
#144593=CARTESIAN_POINT('Ctrl Pts',(5.123237026,4.495496505,-5.144830971));
#144594=CARTESIAN_POINT('Ctrl Pts',(4.830263629,4.560723991,-5.406575004));
#144595=CARTESIAN_POINT('Ctrl Pts',(5.40430219,4.430609079,-5.200338242));
#144596=CARTESIAN_POINT('Ctrl Pts',(5.122504424,4.495496505,-5.493188479));
#144597=CARTESIAN_POINT('Ctrl Pts',(4.810711519,4.560723991,-5.75387301500001));
#144598=CARTESIAN_POINT('Origin',(-0.133457977518899,4.55356864071217,0.147629070275643));
#144599=CARTESIAN_POINT('Ctrl Pts',(5.885111492,4.560731746,-4.234142502));
#144600=CARTESIAN_POINT('Ctrl Pts',(5.652648444,4.495065281,-4.557247111));
#144601=CARTESIAN_POINT('Ctrl Pts',(5.38621099600001,4.430609079,-4.852961066));
#144602=CARTESIAN_POINT('Ctrl Pts',(6.22842029200001,4.560731746,-4.17813124));
#144603=CARTESIAN_POINT('Ctrl Pts',(5.999032377,4.495065281,-4.520084201));
#144604=CARTESIAN_POINT('Ctrl Pts',(5.733588172,4.430609079,-4.83486987100001));
#144605=CARTESIAN_POINT('',(5.88232873095195,4.55994605189024,-4.23800766024314));
#144606=CARTESIAN_POINT('Origin',(-0.167387900492737,4.69628105601737,0.0927664531746669));
#144607=CARTESIAN_POINT('Ctrl Pts',(6.0845617075043,4.52063234085544,-4.38498675280473));
#144608=CARTESIAN_POINT('Ctrl Pts',(6.0508441043927,4.52686607108181,-4.36043688347114));
#144609=CARTESIAN_POINT('Ctrl Pts',(6.01711563512917,4.53325386299334,-4.33590011996221));
#144610=CARTESIAN_POINT('Ctrl Pts',(5.94971658496535,4.54634733284697,-4.28691443395888));
#144611=CARTESIAN_POINT('Ctrl Pts',(5.91600662413241,4.55306065390205,-4.26243688720519));
#144612=CARTESIAN_POINT('Ctrl Pts',(5.88232873168168,4.55994605017244,-4.23800765875298));
#144613=CARTESIAN_POINT('Ctrl Pts',(6.303527553,4.430609079,-3.581625384));
#144614=CARTESIAN_POINT('Ctrl Pts',(6.10944517,4.495496505,-3.923203163));
#144615=CARTESIAN_POINT('Ctrl Pts',(5.879588558,4.560723991,-4.241808386));
#144616=CARTESIAN_POINT('Ctrl Pts',(6.39587161000001,4.430609079,-3.916992003));
#144617=CARTESIAN_POINT('Ctrl Pts',(6.183616263,4.495496505,-4.263573754));
#144618=CARTESIAN_POINT('Ctrl Pts',(5.935152372,4.560723991,-4.585189889));
#144619=CARTESIAN_POINT('Origin',(-0.162073690401712,4.5535686417356,0.115488049281015));
#144620=CARTESIAN_POINT('Ctrl Pts',(6.657736333,4.560731746,-2.870025595));
#144621=CARTESIAN_POINT('Ctrl Pts',(6.500166082,4.495065281,-3.235548881));
#144622=CARTESIAN_POINT('Ctrl Pts',(6.303527553,4.430609079,-3.581625384));
#144623=CARTESIAN_POINT('Ctrl Pts',(6.980977999,4.560731746,-2.741522602));
#144624=CARTESIAN_POINT('Ctrl Pts',(6.830462824,4.495065281,-3.124792514));
#144625=CARTESIAN_POINT('Ctrl Pts',(6.638894171,4.430609079,-3.489281327));
#144626=CARTESIAN_POINT('',(6.65584952602707,4.55994605292527,-2.87439859900565));
#144627=CARTESIAN_POINT('Origin',(-0.183416398184002,4.6962809273909,0.0546141480217011));
#144628=CARTESIAN_POINT('Ctrl Pts',(6.88495056874341,4.52063234090296,-2.97446729084825));
#144629=CARTESIAN_POINT('Ctrl Pts',(6.84674376983872,4.52686607085981,-2.95773967239492));
#144630=CARTESIAN_POINT('Ctrl Pts',(6.80852917359772,4.5332538629194,-2.94102718811593));
#144631=CARTESIAN_POINT('Ctrl Pts',(6.73217540049566,4.54634733289709,-2.90767556313908));
#144632=CARTESIAN_POINT('Ctrl Pts',(6.69399161031044,4.5530606540368,-2.89101693261405));
#144633=CARTESIAN_POINT('Ctrl Pts',(6.65584952632393,4.5599460502987,-2.87439859723605));
#144634=CARTESIAN_POINT('Ctrl Pts',(6.926098167,4.430609079,-2.14281688));
#144635=CARTESIAN_POINT('Ctrl Pts',(6.809982448,4.495496505,-2.518130736));
#144636=CARTESIAN_POINT('Ctrl Pts',(6.653990461,4.560723991,-2.878699522));
#144637=CARTESIAN_POINT('Ctrl Pts',(7.08837718100001,4.430609079,-2.450491571));
#144638=CARTESIAN_POINT('Ctrl Pts',(6.95558907800001,4.495496505,-2.834599059));
#144639=CARTESIAN_POINT('Ctrl Pts',(6.782072097,4.560723991,-3.202108379));
#144640=CARTESIAN_POINT('Origin',(-0.183110903817996,4.55356867528369,0.0779469181040598));
#144641=CARTESIAN_POINT('Ctrl Pts',(7.119052823,4.560731746,-1.371709481));
#144642=CARTESIAN_POINT('Ctrl Pts',(7.043743179,4.495065281,-1.762559983));
#144643=CARTESIAN_POINT('Ctrl Pts',(6.926098167,4.430609079,-2.14281688));
#144644=CARTESIAN_POINT('Ctrl Pts',(7.407112933,4.560731746,-1.176723413));
#144645=CARTESIAN_POINT('Ctrl Pts',(7.342508421,4.495065281,-1.583389001));
#144646=CARTESIAN_POINT('Ctrl Pts',(7.233772858,4.430609079,-1.980537866));
#144647=CARTESIAN_POINT('',(7.11815019522467,4.55994605291902,-1.37638585417308));
#144648=CARTESIAN_POINT('Origin',(-0.190868400650031,4.69628087112419,0.0139081448837788));
#144649=CARTESIAN_POINT('Ctrl Pts',(7.3634067933585,4.52063234083335,-1.4248650437653));
#144650=CARTESIAN_POINT('Ctrl Pts',(7.32249725512444,4.52686607836689,-1.41674183026557));
#144651=CARTESIAN_POINT('Ctrl Pts',(7.28158343164322,4.53325386654012,-1.40863508849938));
#144652=CARTESIAN_POINT('Ctrl Pts',(7.1998451768763,4.54634733286553,-1.39247701472649));
#144653=CARTESIAN_POINT('Ctrl Pts',(7.15897298894386,4.55306065408668,-1.38441623981203));
#144654=CARTESIAN_POINT('Ctrl Pts',(7.11815019511434,4.55994605030007,-1.3763858524884));
#144655=CARTESIAN_POINT('Ctrl Pts',(7.224812129,4.430609079,-0.603812641));
#144656=CARTESIAN_POINT('Ctrl Pts',(7.192092516,4.495496505,-0.995313314));
#144657=CARTESIAN_POINT('Ctrl Pts',(7.117259166,4.560723991,-1.380985869));
#144658=CARTESIAN_POINT('Ctrl Pts',(7.449438113,4.430609079,-0.869408877));
#144659=CARTESIAN_POINT('Ctrl Pts',(7.402326278,4.495496505,-1.273081663));
#144660=CARTESIAN_POINT('Ctrl Pts',(7.311869668,4.560723991,-1.66929984));
#144661=CARTESIAN_POINT('Origin',(-0.195586225750846,4.55356863539642,0.0367611360508951));
#144662=CARTESIAN_POINT('Ctrl Pts',(7.247490315,4.560731746,0.190746244));
#144663=CARTESIAN_POINT('Ctrl Pts',(7.257962673,4.495065281,-0.207155738));
#144664=CARTESIAN_POINT('Ctrl Pts',(7.224812129,4.430609079,-0.603812641));
#144665=CARTESIAN_POINT('Ctrl Pts',(7.48689949900001,4.560731746,0.443098054));
#144666=CARTESIAN_POINT('Ctrl Pts',(7.511226485,4.495065281,0.032052021));
#144667=CARTESIAN_POINT('Ctrl Pts',(7.49040836500001,4.430609079,-0.379186656));
#144668=CARTESIAN_POINT('',(7.2476140724582,4.55994605190755,0.185985162743353));
#144669=CARTESIAN_POINT('Origin',(-0.189396225307772,4.69628103500228,-0.0274481071492781));
#144670=CARTESIAN_POINT('Ctrl Pts',(7.49755829989574,4.52063234091446,0.191362308830983));
#144671=CARTESIAN_POINT('Ctrl Pts',(7.45585900341303,4.52686607092702,0.19050126575676));
#144672=CARTESIAN_POINT('Ctrl Pts',(7.41415898547614,4.53325386295828,0.189623213282634));
#144673=CARTESIAN_POINT('Ctrl Pts',(7.3308581944994,4.5463473328595,0.187832211268426));
#144674=CARTESIAN_POINT('Ctrl Pts',(7.28920874762302,4.5530606540035,0.18691821756087));
#144675=CARTESIAN_POINT('Ctrl Pts',(7.24761407212469,4.55994605018931,0.185985164931052));
#144676=CARTESIAN_POINT('Ctrl Pts',(7.185701905,4.430609079,0.963425207));
#144677=CARTESIAN_POINT('Ctrl Pts',(7.237908331,4.495496505,0.574043853));
#144678=CARTESIAN_POINT('Ctrl Pts',(7.247732742,4.560723991,0.181301149));
#144679=CARTESIAN_POINT('Ctrl Pts',(7.462171599,4.430609079,0.75232641));
#144680=CARTESIAN_POINT('Ctrl Pts',(7.502938928,4.495496505,0.347963618));
#144681=CARTESIAN_POINT('Ctrl Pts',(7.49977234,4.560723991,-0.058436696));
#144682=CARTESIAN_POINT('Origin',(-0.198915958463134,4.5535685999915,-0.00614357805637192));
#144683=CARTESIAN_POINT('Ctrl Pts',(7.037043215,4.560731746,1.744282886));
#144684=CARTESIAN_POINT('Ctrl Pts',(7.13280789900001,4.495065281,1.357934879));
#144685=CARTESIAN_POINT('Ctrl Pts',(7.18570190500001,4.430609079,0.963425207));
#144686=CARTESIAN_POINT('Ctrl Pts',(7.21660696600001,4.560731746,2.042200749));
#144687=CARTESIAN_POINT('Ctrl Pts',(7.328727947,4.495065281,1.645994327));
#144688=CARTESIAN_POINT('Ctrl Pts',(7.396800703,4.430609079,1.239894901));
#144689=CARTESIAN_POINT('',(7.03818757051289,4.55994605127143,1.73965971993725));
#144690=CARTESIAN_POINT('Origin',(-0.179067437115114,4.69628090431665,-0.0675208998185697));
#144691=CARTESIAN_POINT('Ctrl Pts',(7.28113231396762,4.52063234088911,1.79864177274421));
#144692=CARTESIAN_POINT('Ctrl Pts',(7.24059302189612,4.52686607101429,1.78883674406937));
#144693=CARTESIAN_POINT('Ctrl Pts',(7.20005668260348,4.53325386303259,1.77901494874863));
#144694=CARTESIAN_POINT('Ctrl Pts',(7.11908843034963,4.54634733292347,1.75935861156909));
#144695=CARTESIAN_POINT('Ctrl Pts',(7.07860920609677,4.55306065405402,1.7495125865457));
#144696=CARTESIAN_POINT('Ctrl Pts',(7.03818756973783,4.55994605023828,1.73965972239497));
#144697=CARTESIAN_POINT('Ctrl Pts',(6.810596247,4.430609079,2.485614363));
#144698=CARTESIAN_POINT('Ctrl Pts',(6.945287596,4.495496505,2.116559367));
#144699=CARTESIAN_POINT('Ctrl Pts',(7.03931039,4.560723991,1.735110727));
#144700=CARTESIAN_POINT('Ctrl Pts',(7.125982234,4.430609079,2.33888375));
#144701=CARTESIAN_POINT('Ctrl Pts',(7.252722494,4.495496505,1.952738506));
#144702=CARTESIAN_POINT('Ctrl Pts',(7.33699399300001,4.560723991,1.555158883));
#144703=CARTESIAN_POINT('Origin',(-0.192944911290353,4.5535685917447,-0.0487610407490913));
#144704=CARTESIAN_POINT('Ctrl Pts',(6.49755179600001,4.560731746,3.216258799));
#144705=CARTESIAN_POINT('Ctrl Pts',(6.674130955,4.495065281,2.85952997));
#144706=CARTESIAN_POINT('Ctrl Pts',(6.810596247,4.430609079,2.485614363));
#144707=CARTESIAN_POINT('Ctrl Pts',(6.608873911,4.560731746,3.545812407));
#144708=CARTESIAN_POINT('Ctrl Pts',(6.803546235,4.495065281,3.182971767));
#144709=CARTESIAN_POINT('Ctrl Pts',(6.95732686000001,4.430609079,2.80100035));
#144710=CARTESIAN_POINT('',(6.49966323932526,4.55994605292362,3.21198972307321));
#144711=CARTESIAN_POINT('Origin',(-0.160366188328788,4.69628093058526,-0.1044366202835));
#144712=CARTESIAN_POINT('Ctrl Pts',(6.72424867288717,4.52063234084894,3.32181874645752));
#144713=CARTESIAN_POINT('Ctrl Pts',(6.68676491361815,4.5268660784116,3.30352818266225));
#144714=CARTESIAN_POINT('Ctrl Pts',(6.64928771115034,4.53325386662127,3.2852219124572));
#144715=CARTESIAN_POINT('Ctrl Pts',(6.57443800366556,4.54634733297343,3.24861935859961));
#144716=CARTESIAN_POINT('Ctrl Pts',(6.53702176458202,4.55306065431381,3.2303016909336));
#144717=CARTESIAN_POINT('Ctrl Pts',(6.49966323833264,4.55994605052893,3.21198972419786));
#144718=CARTESIAN_POINT('Ctrl Pts',(6.117034678,4.430609079,3.891578954));
#144719=CARTESIAN_POINT('Ctrl Pts',(6.327912933,4.495496505,3.560106917));
#144720=CARTESIAN_POINT('Ctrl Pts',(6.501737708,4.560723991,3.207788456));
#144721=CARTESIAN_POINT('Ctrl Pts',(6.45658986,4.430609079,3.816077485));
#144722=CARTESIAN_POINT('Ctrl Pts',(6.663376816,4.495496505,3.466205512));
#144723=CARTESIAN_POINT('Ctrl Pts',(6.831145961,4.560723991,3.096036961));
#144724=CARTESIAN_POINT('Origin',(-0.177951791260036,4.55356861253526,-0.0890984797097816));
#144725=CARTESIAN_POINT('Ctrl Pts',(5.654242076,4.560731746,4.537846025));
#144726=CARTESIAN_POINT('Ctrl Pts',(5.903379066,4.495065281,4.227416618));
#144727=CARTESIAN_POINT('Ctrl Pts',(6.117034678,4.430609079,3.891578954));
#144728=CARTESIAN_POINT('Ctrl Pts',(5.69211725800001,4.560731746,4.883625817));
#144729=CARTESIAN_POINT('Ctrl Pts',(5.960238263,4.495065281,4.571116985));
#144730=CARTESIAN_POINT('Ctrl Pts',(6.19253614600001,4.430609079,4.231134137));
#144731=CARTESIAN_POINT('',(5.65722188060532,4.55994605195593,4.53413065603272));
#144732=CARTESIAN_POINT('Origin',(-0.134165992850245,4.69628104438188,-0.136468870569518));
#144733=CARTESIAN_POINT('Ctrl Pts',(5.85294663755566,4.52063234086994,4.68967116711042));
#144734=CARTESIAN_POINT('Ctrl Pts',(5.82027120162022,4.52686607017123,4.66375036059968));
#144735=CARTESIAN_POINT('Ctrl Pts',(5.7876054789363,4.53325386263838,4.63781557160427));
#144736=CARTESIAN_POINT('Ctrl Pts',(5.72237416328767,4.54634733296961,4.58597827493659));
#144737=CARTESIAN_POINT('Ctrl Pts',(5.68977045243914,4.55306065424697,4.56004547916216));
#144738=CARTESIAN_POINT('Ctrl Pts',(5.6572218792048,4.55994605047594,4.53413065739853));
#144739=CARTESIAN_POINT('Ctrl Pts',(5.137447365,4.430609079,5.115577638));
#144740=CARTESIAN_POINT('Ctrl Pts',(5.41465209400001,4.495496505,4.837187824));
#144741=CARTESIAN_POINT('Ctrl Pts',(5.66015099700001,4.560723991,4.530473562));
#144742=CARTESIAN_POINT('Ctrl Pts',(5.48529452,4.430609079,5.114835679));
#144743=CARTESIAN_POINT('Ctrl Pts',(5.762459044,4.495496505,4.81759660100001));
#144744=CARTESIAN_POINT('Ctrl Pts',(6.005881136,4.560723991,4.492147791));
#144745=CARTESIAN_POINT('Origin',(-0.15463786334905,4.55356865057608,-0.125269808524199));
#144746=CARTESIAN_POINT('Ctrl Pts',(4.54654628,4.560731746,5.647248615));
#144747=CARTESIAN_POINT('Ctrl Pts',(4.856591733,4.495065281,5.397633963));
#144748=CARTESIAN_POINT('Ctrl Pts',(5.13744736500001,4.430609079,5.115577638));
#144749=CARTESIAN_POINT('Ctrl Pts',(4.509203528,4.560731746,5.993086312));
#144750=CARTESIAN_POINT('Ctrl Pts',(4.838236174,4.495065281,5.745521853));
#144751=CARTESIAN_POINT('Ctrl Pts',(5.138189324,4.430609079,5.463424793));
#144752=CARTESIAN_POINT('',(4.55025511321812,4.55994605292947,5.64426067931357));
#144753=CARTESIAN_POINT('Origin',(-0.101692449553174,4.69628087469097,-0.162119920184228));
#144754=CARTESIAN_POINT('Ctrl Pts',(4.70796732248972,4.52063234085653,5.83823977670622));
#144755=CARTESIAN_POINT('Ctrl Pts',(4.68162799240327,4.52686607840256,5.80590068860456));
#144756=CARTESIAN_POINT('Ctrl Pts',(4.65530120807513,4.53325386657975,5.77355009899121));
#144757=CARTESIAN_POINT('Ctrl Pts',(4.60273846663404,4.5463473329181,5.70890194445263));
#144758=CARTESIAN_POINT('Ctrl Pts',(4.57647179682458,4.55306065418861,5.67656660889885));
#144759=CARTESIAN_POINT('Ctrl Pts',(4.5502551116134,4.55994605040326,5.64426068007741));
#144760=CARTESIAN_POINT('Ctrl Pts',(3.917638724,4.430609079,6.100377597));
#144761=CARTESIAN_POINT('Ctrl Pts',(4.248208141,4.495496505,5.888087205));
#144762=CARTESIAN_POINT('Ctrl Pts',(4.553901916,4.560723991,5.64131875900001));
#144763=CARTESIAN_POINT('Ctrl Pts',(4.257512905,4.430609079,6.174429841));
#144764=CARTESIAN_POINT('Ctrl Pts',(4.592095092,4.495496505,5.94372222700001));
#144765=CARTESIAN_POINT('Ctrl Pts',(4.899787985,4.560723991,5.67821078400001));
#144766=CARTESIAN_POINT('Origin',(-0.124093184553192,4.55356863304782,-0.155583612145826));
#144767=CARTESIAN_POINT('Ctrl Pts',(3.226259034,4.560731746,6.492592136));
#144768=CARTESIAN_POINT('Ctrl Pts',(3.582715568,4.495065281,6.315463943));
#144769=CARTESIAN_POINT('Ctrl Pts',(3.917638724,4.430609079,6.100377597));
#144770=CARTESIAN_POINT('Ctrl Pts',(3.115444452,4.560731746,6.822316752));
#144771=CARTESIAN_POINT('Ctrl Pts',(3.490003539,4.495065281,6.651272505));
#144772=CARTESIAN_POINT('Ctrl Pts',(3.84358648,4.430609079,6.440251778));
#144773=CARTESIAN_POINT('',(3.2305234747432,4.55994605294443,6.4904713464554));
#144774=CARTESIAN_POINT('Origin',(-0.0644639989327161,4.69628088593423,
-0.180190601896851));
#144775=CARTESIAN_POINT('Ctrl Pts',(3.34284868775708,4.52063234083049,6.71381878287937));
#144776=CARTESIAN_POINT('Ctrl Pts',(3.32407710461589,4.52686607836884,6.6765735873874));
#144777=CARTESIAN_POINT('Ctrl Pts',(3.30532024644795,4.53325386652875,6.63931985630375));
#144778=CARTESIAN_POINT('Ctrl Pts',(3.2678838350263,4.54634733287855,6.56488370404862));
#144779=CARTESIAN_POINT('Ctrl Pts',(3.24918240690815,4.55306065410071,6.52765779341605));
#144780=CARTESIAN_POINT('Ctrl Pts',(3.23052347304825,4.55994605034044,6.49047134682372));
#144781=CARTESIAN_POINT('Ctrl Pts',(2.51464565,4.430609079,6.79993068));
#144782=CARTESIAN_POINT('Ctrl Pts',(2.883122697,4.495496505,6.663666173));
#144783=CARTESIAN_POINT('Ctrl Pts',(3.234717443,4.560723991,6.488382161));
#144784=CARTESIAN_POINT('Ctrl Pts',(2.830654719,4.430609079,6.945314526));
#144785=CARTESIAN_POINT('Ctrl Pts',(3.207009877,4.495496505,6.791926008));
#144786=CARTESIAN_POINT('Ctrl Pts',(3.564586193,4.560723991,6.598766951));
#144787=CARTESIAN_POINT('Origin',(-0.0877460033528399,4.55356862172701,
-0.178622367928359));
#144788=CARTESIAN_POINT('Ctrl Pts',(1.755115501,4.560731746,7.034349265));
#144789=CARTESIAN_POINT('Ctrl Pts',(2.141315605,4.495065281,6.937989849));
#144790=CARTESIAN_POINT('Ctrl Pts',(2.51464565,4.430609079,6.79993068000001));
#144791=CARTESIAN_POINT('Ctrl Pts',(1.576010657,4.560731746,7.332543243));
#144792=CARTESIAN_POINT('Ctrl Pts',(1.978582217,4.495065281,7.246017048));
#144793=CARTESIAN_POINT('Ctrl Pts',(2.369261804,4.430609079,7.115939748));
#144794=CARTESIAN_POINT('',(1.75973614927375,4.55994605189544,7.03319478739374));
#144795=CARTESIAN_POINT('Origin',(-0.0242212355240337,4.69628106280526,
-0.189835864139755));
#144796=CARTESIAN_POINT('Ctrl Pts',(1.82142216389954,4.52063234086191,7.27546708476632));
#144797=CARTESIAN_POINT('Ctrl Pts',(1.8110960794124,4.52686607033607,7.23505737799141));
#144798=CARTESIAN_POINT('Ctrl Pts',(1.80078618995318,4.5332538626486,7.19464242018641));
#144799=CARTESIAN_POINT('Ctrl Pts',(1.78022658737578,4.54634733288435,7.11389879786007));
#144800=CARTESIAN_POINT('Ctrl Pts',(1.76996485896719,4.55306065389986,7.07352295524677));
#144801=CARTESIAN_POINT('Ctrl Pts',(1.75973614734532,4.55994605016872,7.03319478758805));
#144802=CARTESIAN_POINT('Ctrl Pts',(0.994070541,4.430609079,7.181526562));
#144803=CARTESIAN_POINT('Ctrl Pts',(1.38322564,4.495496505,7.127659516));
#144804=CARTESIAN_POINT('Ctrl Pts',(1.764281177,4.560723991,7.03205602400001));
#144805=CARTESIAN_POINT('Ctrl Pts',(1.271438263,4.430609079,7.391444023));
#144806=CARTESIAN_POINT('Ctrl Pts',(1.671968444,4.495496505,7.32254687700001));
#144807=CARTESIAN_POINT('Ctrl Pts',(2.062708312,4.560723991,7.21077211));
#144808=CARTESIAN_POINT('Origin',(-0.0472960242996028,4.55356862061657,
-0.193309116276226));
#144809=CARTESIAN_POINT('Ctrl Pts',(0.201904718,4.560731746,7.24718804));
#144810=CARTESIAN_POINT('Ctrl Pts',(0.599790104,4.495065281,7.23610306));
#144811=CARTESIAN_POINT('Ctrl Pts',(0.994070541000001,4.430609079,7.18152656200001));
#144812=CARTESIAN_POINT('Ctrl Pts',(-0.037115645,4.560731746,7.499908161));
#144813=CARTESIAN_POINT('Ctrl Pts',(0.37464459,4.495065281,7.501945886));
#144814=CARTESIAN_POINT('Ctrl Pts',(0.78415308,4.430609079,7.458894285));
#144815=CARTESIAN_POINT('',(0.206665516131424,4.55994605293665,7.24705385453353));
#144816=CARTESIAN_POINT('Origin',(0.0171541522854927,4.69628090700534,-0.190604205424212));
#144817=CARTESIAN_POINT('Ctrl Pts',(0.21482796402738,4.52063234085271,7.49692263175493));
#144818=CARTESIAN_POINT('Ctrl Pts',(0.213430188247251,4.52686607841023,
7.45523782448));
#144819=CARTESIAN_POINT('Ctrl Pts',(0.212049360526979,4.53325386660713,
7.41355145322911));
#144820=CARTESIAN_POINT('Ctrl Pts',(0.209327922975149,4.54634733296248,
7.33027588971406));
#144821=CARTESIAN_POINT('Ctrl Pts',(0.207985720792377,4.55306065421451,
7.28863804207581));
#144822=CARTESIAN_POINT('Ctrl Pts',(0.206665514894415,4.55994605043467,
7.24705385415854));
#144823=CARTESIAN_POINT('Ctrl Pts',(-0.572986203,4.430609079,7.22732224400001));
#144824=CARTESIAN_POINT('Ctrl Pts',(-0.181349511,4.495496505,7.25837142200001));
#144825=CARTESIAN_POINT('Ctrl Pts',(0.211349085,4.560723991,7.246918763));
#144826=CARTESIAN_POINT('Ctrl Pts',(-0.347229232,4.430609079,7.491957812));
#144827=CARTESIAN_POINT('Ctrl Pts',(0.0587476260000001,4.495496505,7.510773593));
#144828=CARTESIAN_POINT('Ctrl Pts',(0.464380483,4.560723991,7.485609579));
#144829=CARTESIAN_POINT('Origin',(-0.00463454090715021,4.55356860745719,
-0.198957013389406));
#144830=CARTESIAN_POINT('Ctrl Pts',(0.201633249,1.457976823,7.247195598));
#144831=CARTESIAN_POINT('Ctrl Pts',(0.597296021,1.39227158,7.236187371));
#144832=CARTESIAN_POINT('Ctrl Pts',(0.989408718,1.327100493,7.18217031200001));
#144833=CARTESIAN_POINT('Ctrl Pts',(-0.03739658,1.457976823,7.499906766));
#144834=CARTESIAN_POINT('Ctrl Pts',(0.372063032,1.39227158,7.50194844300001));
#144835=CARTESIAN_POINT('Ctrl Pts',(0.779311259,1.327100493,7.459401716));
#144836=CARTESIAN_POINT('',(0.213145095072078,1.41778968871295,7.49697066565625));
#144837=CARTESIAN_POINT('',(0.77931126906081,1.32710049399577,7.45940171643651));
#144838=CARTESIAN_POINT('Origin',(0.00491638811184272,1.48212079817506,
-0.190660326973322));
#144839=CARTESIAN_POINT('',(0.884360005917485,1.32710049586377,7.32078601189595));
#144840=CARTESIAN_POINT('Ctrl Pts',(0.213145094523798,1.41778968832183,
7.49697066561295));
#144841=CARTESIAN_POINT('Ctrl Pts',(0.211973474313471,1.42404710663119,
7.45528012261522));
#144842=CARTESIAN_POINT('Ctrl Pts',(0.210820057394797,1.43045449292311,
7.41358844026421));
#144843=CARTESIAN_POINT('Ctrl Pts',(0.208555899831965,1.44357823944106,
7.33029933574109));
#144844=CARTESIAN_POINT('Ctrl Pts',(0.207443881005112,1.45030198445001,
7.28865500680507));
#144845=CARTESIAN_POINT('Ctrl Pts',(0.206355413393753,1.45719264070242,
7.24706267711513));
#144846=CARTESIAN_POINT('Ctrl Pts',(0.989408718000001,1.327100493,7.18217031200001));
#144847=CARTESIAN_POINT('Ctrl Pts',(1.380789714,1.392692987,7.128254051));
#144848=CARTESIAN_POINT('Ctrl Pts',(1.76399439,1.45796923,7.03212797));
#144849=CARTESIAN_POINT('Ctrl Pts',(1.266640122,1.327100493,7.392267771));
#144850=CARTESIAN_POINT('Ctrl Pts',(1.669470046,1.392692987,7.323244224));
#144851=CARTESIAN_POINT('Ctrl Pts',(2.062414236,1.45796923,7.210856227));
#144852=CARTESIAN_POINT('',(1.26664012713773,1.32710049307754,7.39226777165038));
#144853=CARTESIAN_POINT('',(1.81978896516141,1.41778968870968,7.27587576303884));
#144854=CARTESIAN_POINT('Origin',(-0.03450053467242,1.33928592015067,-0.18979919100365));
#144855=CARTESIAN_POINT('Ctrl Pts',(1.75943519295771,1.45719264068656,7.03327006476683));
#144856=CARTESIAN_POINT('Ctrl Pts',(1.76943932796608,1.45030198862715,7.07365597612469));
#144857=CARTESIAN_POINT('Ctrl Pts',(1.77947764044795,1.44357824830594,7.1140876026183));
#144858=CARTESIAN_POINT('Ctrl Pts',(1.79959357204886,1.43045449290407,7.19494278218988));
#144859=CARTESIAN_POINT('Ctrl Pts',(1.80968250183055,1.4240471066513,7.23541178548329));
#144860=CARTESIAN_POINT('Ctrl Pts',(1.81978896448098,1.41778968833587,7.27587576315098));
#144861=CARTESIAN_POINT('',(1.12802441867849,1.32710049321647,7.28721904170456));
#144862=CARTESIAN_POINT('Origin',(-6.83047368665868E-14,1.41887506699983,
9.2374025095765E-14));
#144863=CARTESIAN_POINT('',(1.82437897668122,1.23689319339462,7.27472620408252));
#144864=CARTESIAN_POINT('Origin',(-0.00664832877748628,1.48200505002726,
-0.185042883132719));
#144865=CARTESIAN_POINT('',(2.36464227492396,1.32710049399578,7.1174761632605));
#144866=CARTESIAN_POINT('Origin',(-0.0625461989580287,1.33928289225507,
-0.182027286444451));
#144867=CARTESIAN_POINT('Origin',(-0.0361848819786822,1.4821207899034,-0.187259632689556));
#144868=CARTESIAN_POINT('Ctrl Pts',(1.754852004,1.457976823,7.034415004));
#144869=CARTESIAN_POINT('Ctrl Pts',(2.138897957,1.39227158,6.938608343));
#144870=CARTESIAN_POINT('Ctrl Pts',(2.510231206,1.327100493,6.801561533));
#144871=CARTESIAN_POINT('Ctrl Pts',(1.57573599,1.457976823,7.332602273));
#144872=CARTESIAN_POINT('Ctrl Pts',(1.976061564,1.39227158,7.24657450400001));
#144873=CARTESIAN_POINT('Ctrl Pts',(2.364642265,1.327100493,7.11747616499999));
#144874=CARTESIAN_POINT('',(2.43743675205783,1.32710049586375,6.95951884320094));
#144875=CARTESIAN_POINT('Ctrl Pts',(2.510231206,1.327100493,6.801561533));
#144876=CARTESIAN_POINT('Ctrl Pts',(2.880871529,1.392692987,6.66477046000001));
#144877=CARTESIAN_POINT('Ctrl Pts',(3.234452827,1.45796923,6.488514076));
#144878=CARTESIAN_POINT('Ctrl Pts',(2.826145837,1.327100493,6.947150474));
#144879=CARTESIAN_POINT('Ctrl Pts',(3.204719799,1.392692987,6.793144133));
#144880=CARTESIAN_POINT('Ctrl Pts',(3.564317074,1.45796923,6.598912319));
#144881=CARTESIAN_POINT('',(2.82614584214365,1.32710049307753,6.94715047353126));
#144882=CARTESIAN_POINT('',(3.34134152620834,1.41778968874369,6.71456899583714));
#144883=CARTESIAN_POINT('Origin',(-0.0744950944575939,1.33928594525405,
-0.177945054765195));
#144884=CARTESIAN_POINT('Ctrl Pts',(3.23024573729235,1.45719264064239,6.49060956175589));
#144885=CARTESIAN_POINT('Ctrl Pts',(3.24869776185374,1.45030198734322,6.52790068625596));
#144886=CARTESIAN_POINT('Ctrl Pts',(3.26719299295515,1.44357824563603,6.56522911148062));
#144887=CARTESIAN_POINT('Ctrl Pts',(3.30422009154465,1.43045449289261,6.63986959596905));
#144888=CARTESIAN_POINT('Ctrl Pts',(3.32277278724771,1.42404710665793,6.67722363462803));
#144889=CARTESIAN_POINT('Ctrl Pts',(3.34134152552766,1.41778968836386,6.71456899611195));
#144890=CARTESIAN_POINT('',(2.66818852025337,1.32710049321647,6.87435600398386));
#144891=CARTESIAN_POINT('Origin',(-1.45283091113058E-14,1.41887506699983,
-7.37257477290143E-14));
#144892=CARTESIAN_POINT('',(3.34557710444283,1.23689319339271,6.71245959639036));
#144893=CARTESIAN_POINT('Origin',(-0.0462715736869412,1.48200502695773,
-0.179287315894316));
#144894=CARTESIAN_POINT('',(3.83940523733456,1.32710049399579,6.44274533515092));
#144895=CARTESIAN_POINT('Origin',(-0.100214493544963,1.33928284390673,-0.164326226279317));
#144896=CARTESIAN_POINT('Origin',(-0.0755943261787495,1.48212079376037,
-0.175103206174972));
#144897=CARTESIAN_POINT('Ctrl Pts',(3.226015829,1.457976823,6.492712982));
#144898=CARTESIAN_POINT('Ctrl Pts',(3.580487401,1.39227158,6.316587701));
#144899=CARTESIAN_POINT('Ctrl Pts',(3.913678072,1.327100493,6.102919297));
#144900=CARTESIAN_POINT('Ctrl Pts',(3.115188897,1.457976823,6.822433447));
#144901=CARTESIAN_POINT('Ctrl Pts',(3.487661654,1.39227158,6.652358794));
#144902=CARTESIAN_POINT('Ctrl Pts',(3.839405228,1.327100493,6.442745339));
#144903=CARTESIAN_POINT('',(3.87654166492425,1.32710049586378,6.27283230877697));
#144904=CARTESIAN_POINT('Ctrl Pts',(3.913678072,1.327100493,6.102919297));
#144905=CARTESIAN_POINT('Ctrl Pts',(4.246246993,1.392692987,5.889649609));
#144906=CARTESIAN_POINT('Ctrl Pts',(4.553671844,1.45796923,5.641504474));
#144907=CARTESIAN_POINT('Ctrl Pts',(4.253504114,1.327100493,6.177192142));
#144908=CARTESIAN_POINT('Ctrl Pts',(4.590120416,1.392692987,5.945404172));
#144909=CARTESIAN_POINT('Ctrl Pts',(4.899556408,1.45796923,5.678410606));
#144910=CARTESIAN_POINT('',(4.2535041188979,1.32710049307752,6.17719214044297));
#144911=CARTESIAN_POINT('',(4.70665667110046,1.41778968872295,5.83929644531604));
#144912=CARTESIAN_POINT('Origin',(-0.111006437282785,1.33928596431819,-0.157770636694248));
#144913=CARTESIAN_POINT('Ctrl Pts',(4.55001358209102,1.4571926406954,5.64445536825662));
#144914=CARTESIAN_POINT('Ctrl Pts',(4.57605069415297,1.45030198837447,5.67690800266822));
#144915=CARTESIAN_POINT('Ctrl Pts',(4.60213802035174,1.44357824776257,5.70938777653085));
#144916=CARTESIAN_POINT('Ctrl Pts',(4.65434495195885,1.43045449290745,5.77432348688941));
#144917=CARTESIAN_POINT('Ctrl Pts',(4.68049391001257,1.4240471066716,5.80681592778155));
#144918=CARTESIAN_POINT('Ctrl Pts',(4.70665667037991,1.41778968834624,5.83929644582386));
#144919=CARTESIAN_POINT('',(4.08359109188649,1.32710049321648,6.14005572024056));
#144920=CARTESIAN_POINT('Origin',(-8.70397504071363E-13,1.41887506700022,
-1.21430643318376E-12));
#144921=CARTESIAN_POINT('',(4.71033976529093,1.23689319339203,5.83632583826807));
#144922=CARTESIAN_POINT('Origin',(-0.0837313962564479,1.4820050646192,-0.165148862441861));
#144923=CARTESIAN_POINT('',(5.13464187728295,1.32710049399578,5.46675889524378));
#144924=CARTESIAN_POINT('Origin',(-0.133196764415154,1.3392828345734,-0.138941155274088));
#144925=CARTESIAN_POINT('Origin',(-0.111469039437913,1.4821207822942,-0.154758896047827));
#144926=CARTESIAN_POINT('Ctrl Pts',(4.54633474,1.457976823,5.647418918));
#144927=CARTESIAN_POINT('Ctrl Pts',(4.854657234,1.39227158,5.399210438));
#144928=CARTESIAN_POINT('Ctrl Pts',(5.134125702,1.327100493,5.118911337));
#144929=CARTESIAN_POINT('Ctrl Pts',(4.508979033,1.457976823,5.993255216));
#144930=CARTESIAN_POINT('Ctrl Pts',(4.836182561,1.39227158,5.747086181));
#144931=CARTESIAN_POINT('Ctrl Pts',(5.134641869,1.327100493,5.466758901));
#144932=CARTESIAN_POINT('',(5.13438379809266,1.32710049586378,5.29283510678433));
#144933=CARTESIAN_POINT('Ctrl Pts',(5.134125702,1.327100493,5.118911337));
#144934=CARTESIAN_POINT('Ctrl Pts',(5.413072667,1.392692987,4.839135289));
#144935=CARTESIAN_POINT('Ctrl Pts',(5.659966227,1.45796923,4.530704394));
#144936=CARTESIAN_POINT('Ctrl Pts',(5.481973265,1.327100493,5.11839517));
#144937=CARTESIAN_POINT('Ctrl Pts',(5.760892103,1.392692987,4.81966372));
#144938=CARTESIAN_POINT('Ctrl Pts',(6.005697929,1.45796923,4.492392723));
#144939=CARTESIAN_POINT('',(5.48197326949186,1.32710049307754,5.1183951674044));
#144940=CARTESIAN_POINT('',(5.85189378093044,1.41778968872863,4.69098488279759));
#144941=CARTESIAN_POINT('Origin',(-0.142327169791678,1.33928591042193,-0.130218947999294));
#144942=CARTESIAN_POINT('Ctrl Pts',(5.65702784793378,1.45719264077919,4.53437271583438));
#144943=CARTESIAN_POINT('Ctrl Pts',(5.68943258944673,1.45030198726807,4.56046942052694));
#144944=CARTESIAN_POINT('Ctrl Pts',(5.72189220655393,1.4435782453354,4.58658183662514));
#144945=CARTESIAN_POINT('Ctrl Pts',(5.78683781530013,1.43045449292487,4.63877642909337));
#144946=CARTESIAN_POINT('Ctrl Pts',(5.81936033988894,1.4240471066349,4.66488796186657));
#144947=CARTESIAN_POINT('Ctrl Pts',(5.85189378060671,1.41778968834312,4.69098488310873));
#144948=CARTESIAN_POINT('',(5.30804948257172,1.32710049321648,5.11865325446263));
#144949=CARTESIAN_POINT('Origin',(-8.16187395447088E-13,1.41887506700028,
-7.04731412115578E-13));
#144950=CARTESIAN_POINT('',(5.85485217362667,1.23689319338142,4.68729197077231));
#144951=CARTESIAN_POINT('Origin',(-0.117275698567805,1.48200509272981,-0.143287821712398));
#144952=CARTESIAN_POINT('',(6.18978836985319,1.32710049399578,4.23515288559396));
#144953=CARTESIAN_POINT('Origin',(-0.159950765827412,1.33928281164314,-0.107059299319675));
#144954=CARTESIAN_POINT('Origin',(-0.142131268964576,1.48212079248997,-0.127177973873037));
#144955=CARTESIAN_POINT('Ctrl Pts',(5.654072091,1.457976823,4.538057821));
#144956=CARTESIAN_POINT('Ctrl Pts',(5.90182869,1.39227158,4.229372095));
#144957=CARTESIAN_POINT('Ctrl Pts',(6.11450731900001,1.327100493,3.895548773));
#144958=CARTESIAN_POINT('Ctrl Pts',(5.691934321,1.457976823,4.883839032));
#144959=CARTESIAN_POINT('Ctrl Pts',(5.95856894700001,1.39227158,4.573086206));
#144960=CARTESIAN_POINT('Ctrl Pts',(6.189788363,1.327100493,4.235152893));
#144961=CARTESIAN_POINT('',(6.15214785067216,1.32710049586375,4.06535081836299));
#144962=CARTESIAN_POINT('Ctrl Pts',(6.114507319,1.327100493,3.895548773));
#144963=CARTESIAN_POINT('Ctrl Pts',(6.32678908000001,1.392692987,3.562348381));
#144964=CARTESIAN_POINT('Ctrl Pts',(6.50160688,1.45796923,3.208053611));
#144965=CARTESIAN_POINT('Ctrl Pts',(6.45411144,1.327100493,3.82026773));
#144966=CARTESIAN_POINT('Ctrl Pts',(6.662290879,1.392692987,3.468561149));
#144967=CARTESIAN_POINT('Ctrl Pts',(6.83101969100001,1.45796923,3.09631555));
#144968=CARTESIAN_POINT('',(6.45411144382818,1.32710049307764,3.82026772649141));
#144969=CARTESIAN_POINT('',(6.72350284172602,1.41778968869915,3.32332808088867));
#144970=CARTESIAN_POINT('Origin',(-0.166992936340966,1.33928594576275,-0.0965783880493759));
#144971=CARTESIAN_POINT('Ctrl Pts',(6.49952577937695,1.45719264070939,3.21226783447012));
#144972=CARTESIAN_POINT('Ctrl Pts',(6.53678293030639,1.45030198828831,3.2307883484457));
#144973=CARTESIAN_POINT('Ctrl Pts',(6.57409705006756,1.44357824756423,3.2493124091844));
#144974=CARTESIAN_POINT('Ctrl Pts',(6.64874457410277,1.43045449287878,3.28632534162432));
#144975=CARTESIAN_POINT('Ctrl Pts',(6.68611994757602,1.42404710663606,3.30483501978555));
#144976=CARTESIAN_POINT('Ctrl Pts',(6.72350284131941,1.41778968831898,3.323328081582));
#144977=CARTESIAN_POINT('',(6.28430937880036,1.32710049321648,3.85790825263968));
#144978=CARTESIAN_POINT('Origin',(-9.2070448487469E-13,1.41887506700011,
-4.28043017697277E-13));
#144979=CARTESIAN_POINT('',(6.72559820178556,1.23689319341789,3.31908553997918));
#144980=CARTESIAN_POINT('Origin',(-0.145336716879659,1.48200507781202,-0.114727120736509));
#144981=CARTESIAN_POINT('',(6.95550723709846,1.32710049399577,2.80551583431356));
#144982=CARTESIAN_POINT('Origin',(-0.179225865589576,1.33928283772879,-0.070171649672468));
#144983=CARTESIAN_POINT('Origin',(-0.166147914169609,1.48212074243726,-0.093650624888299));
#144984=CARTESIAN_POINT('Ctrl Pts',(6.497431315,1.457976823,3.216502185));
#144985=CARTESIAN_POINT('Ctrl Pts',(6.673037196,1.39227158,2.861773014));
#144986=CARTESIAN_POINT('Ctrl Pts',(6.808981371,1.327100493,2.490034677));
#144987=CARTESIAN_POINT('Ctrl Pts',(6.608741086,1.457976823,3.546059963));
#144988=CARTESIAN_POINT('Ctrl Pts',(6.802339271,1.39227158,3.185253802));
#144989=CARTESIAN_POINT('Ctrl Pts',(6.955507232,1.327100493,2.805515843));
#144990=CARTESIAN_POINT('',(6.88224430779951,1.32710049586375,2.64777524362598));
#144991=CARTESIAN_POINT('Ctrl Pts',(6.80898137100001,1.327100493,2.490034677));
#144992=CARTESIAN_POINT('Ctrl Pts',(6.94467186700001,1.392692987,2.118990022));
#144993=CARTESIAN_POINT('Ctrl Pts',(7.039239622,1.45796923,1.735397808));
#144994=CARTESIAN_POINT('Ctrl Pts',(7.124462536,1.327100493,2.343508816));
#144995=CARTESIAN_POINT('Ctrl Pts',(7.252168337,1.392692987,1.955272514));
#144996=CARTESIAN_POINT('Ctrl Pts',(7.336930563,1.45796923,1.555458103));
#144997=CARTESIAN_POINT('',(7.12446253897948,1.32710049307754,2.34350881176759));
#144998=CARTESIAN_POINT('',(7.28072838188157,1.41778968870772,1.80027615161597));
#144999=CARTESIAN_POINT('Origin',(-0.183850292341285,1.33928591987418,-0.0584219215698881));
#145000=CARTESIAN_POINT('Ctrl Pts',(7.03811310959639,1.45719264069764,1.7399608805707));
#145001=CARTESIAN_POINT('Ctrl Pts',(7.07848058142795,1.45030198665873,1.75003921115543));
#145002=CARTESIAN_POINT('Ctrl Pts',(7.11890445475644,1.44357824413122,1.76010875955486));
#145003=CARTESIAN_POINT('Ctrl Pts',(7.19976342611434,1.43045449288012,1.78020933350881));
#145004=CARTESIAN_POINT('Ctrl Pts',(7.24024401785159,1.42404710660719,1.79025166512369));
#145005=CARTESIAN_POINT('Ctrl Pts',(7.28072838168565,1.41778968831362,1.8002761521612));
#145006=CARTESIAN_POINT('',(6.96672195306172,1.32710049321648,2.41677174776343));
#145007=CARTESIAN_POINT('Origin',(1.22471477403963E-12,1.41887506700044,
2.97830336781768E-13));
#145008=CARTESIAN_POINT('',(7.2818627332403,1.23689319338706,1.79568235838578));
#145009=CARTESIAN_POINT('Origin',(-0.166601486859206,1.48200500153013,-0.0808016886821614));
#145010=CARTESIAN_POINT('',(7.3959943171118,1.32710049399578,1.24469598041886));
#145011=CARTESIAN_POINT('Origin',(-0.19012037374844,1.33928284375318,-0.0300027825352343));
#145012=CARTESIAN_POINT('Origin',(-0.182395433175825,1.48212077510888,-0.0557442137474637));
#145013=CARTESIAN_POINT('Ctrl Pts',(7.036977872,1.457976823,1.744546481));
#145014=CARTESIAN_POINT('Ctrl Pts',(7.1322219,1.39227158,1.360360608));
#145015=CARTESIAN_POINT('Ctrl Pts',(7.185075021,1.327100493,0.968089328));
#145016=CARTESIAN_POINT('Ctrl Pts',(7.216530463,1.457976823,2.042471071));
#145017=CARTESIAN_POINT('Ctrl Pts',(7.328039771,1.39227158,1.648482471));
#145018=CARTESIAN_POINT('Ctrl Pts',(7.395994314,1.327100493,1.24469599));
#145019=CARTESIAN_POINT('',(7.29053467013232,1.32710049586378,1.10639264165444));
#145020=CARTESIAN_POINT('Ctrl Pts',(7.185075021,1.327100493,0.968089328));
#145021=CARTESIAN_POINT('Ctrl Pts',(7.237829515,1.392692987,0.576550044));
#145022=CARTESIAN_POINT('Ctrl Pts',(7.247725342,1.45796923,0.181596731));
#145023=CARTESIAN_POINT('Ctrl Pts',(7.461681683,1.327100493,0.757170034));
#145024=CARTESIAN_POINT('Ctrl Pts',(7.502942465,1.392692987,0.350557509));
#145025=CARTESIAN_POINT('Ctrl Pts',(7.499774717,1.45796923,-0.058130836));
#145026=CARTESIAN_POINT('Ctrl Pts',(7.24760609256058,1.45719264067756,0.186295288436271));
#145027=CARTESIAN_POINT('Ctrl Pts',(7.28919633564811,1.45030198710193,0.187460180071232));
#145028=CARTESIAN_POINT('Ctrl Pts',(7.33083977304701,1.44357824510147,0.188604370185033));
#145029=CARTESIAN_POINT('Ctrl Pts',(7.41412934238839,1.43045449282631,0.190852715567777));
#145030=CARTESIAN_POINT('Ctrl Pts',(7.45582232469342,1.42404710658477,0.191958132493221));
#145031=CARTESIAN_POINT('Ctrl Pts',(7.49751515510443,1.41778968828417,0.193045311129516));
#145032=CARTESIAN_POINT('',(7.32337835184357,1.32710049321648,0.862629682328108));
#145033=CARTESIAN_POINT('Ctrl Pts',(7.247483165,1.457976823,0.191017723));
#145034=CARTESIAN_POINT('Ctrl Pts',(7.25791183400001,1.39227158,-0.204660748));
#145035=CARTESIAN_POINT('Ctrl Pts',(7.22520254800001,1.327100493,-0.599122803));
#145036=CARTESIAN_POINT('Ctrl Pts',(7.486882896,1.457976823,0.443378502));
#145037=CARTESIAN_POINT('Ctrl Pts',(7.511089276,1.39227158,0.034629932));
#145038=CARTESIAN_POINT('Ctrl Pts',(7.490652922,1.327100493,-0.374324464));
#145039=CARTESIAN_POINT('',(7.357927733842,1.32710049586375,-0.486723651005759));
#145040=CARTESIAN_POINT('Ctrl Pts',(7.225202548,1.327100493,-0.599122803));
#145041=CARTESIAN_POINT('Ctrl Pts',(7.1925543,1.392692987,-0.992848772000001));
#145042=CARTESIAN_POINT('Ctrl Pts',(7.11731548,1.45796923,-1.380695607));
#145043=CARTESIAN_POINT('Ctrl Pts',(7.450000887,1.327100493,-0.864573176000001));
#145044=CARTESIAN_POINT('Ctrl Pts',(7.402887342,1.392692987,-1.270549175));
#145045=CARTESIAN_POINT('Ctrl Pts',(7.311937741,1.45796923,-1.669001641));
#145046=CARTESIAN_POINT('',(7.45000088793103,1.32710049307756,-0.864573181109506));
#145047=CARTESIAN_POINT('',(7.3637264526154,1.41778968836978,-1.4232121145184));
#145048=CARTESIAN_POINT('Origin',(-0.191388337446107,1.33928597468727,0.0241743755201032));
#145049=CARTESIAN_POINT('Ctrl Pts',(7.11820906946345,1.45719264072522,-1.37608126440437));
#145050=CARTESIAN_POINT('Ctrl Pts',(7.15907737221457,1.45030198732391,-1.38388427974216));
#145051=CARTESIAN_POINT('Ctrl Pts',(7.19999317518224,1.44357824550689,-1.39171894784093));
#145052=CARTESIAN_POINT('Ctrl Pts',(7.28181881080215,1.4304544928872,-1.40742796307507));
#145053=CARTESIAN_POINT('Ctrl Pts',(7.32277466610963,1.42404710668474,-1.41531114880329));
#145054=CARTESIAN_POINT('Ctrl Pts',(7.36372645274274,1.41778968836392,-1.42321211385375));
#145055=CARTESIAN_POINT('',(7.33760171763273,1.32710049321648,-0.731847988169313));
#145056=CARTESIAN_POINT('Origin',(-1.76941794549634E-13,1.41887506699994,
1.32814766129474E-14));
#145057=CARTESIAN_POINT('',(7.36282707778784,1.23689319393736,-1.42785763063424));
#145058=CARTESIAN_POINT('Origin',(-0.185131207741326,1.48200499910506,-0.00337946924173715));
#145059=CARTESIAN_POINT('',(7.235056922811,1.32710049399576,-1.97584193198526));
#145060=CARTESIAN_POINT('Origin',(-0.185146488048183,1.33928285163288,0.0525997022622385));
#145061=CARTESIAN_POINT('Origin',(-0.18894410901323,1.48212075846602,0.025993811794856));
#145062=CARTESIAN_POINT('Ctrl Pts',(7.1191042,1.457976823,-1.371442812));
#145063=CARTESIAN_POINT('Ctrl Pts',(7.044229877,1.39227158,-1.760112396));
#145064=CARTESIAN_POINT('Ctrl Pts',(6.927487635,1.327100493,-2.138320617));
#145065=CARTESIAN_POINT('Ctrl Pts',(7.407157006,1.457976823,-1.176445953));
#145066=CARTESIAN_POINT('Ctrl Pts',(7.342928594,1.39227158,-1.580841865));
#145067=CARTESIAN_POINT('Ctrl Pts',(7.235056924,1.327100493,-1.975841922));
#145068=CARTESIAN_POINT('',(7.08127227460586,1.32710049586375,-2.05708128634755));
#145069=CARTESIAN_POINT('Ctrl Pts',(6.927487635,1.327100493,-2.138320617));
#145070=CARTESIAN_POINT('Ctrl Pts',(6.81096324000001,1.392692987,-2.515823084));
#145071=CARTESIAN_POINT('Ctrl Pts',(6.654107857,1.45796923,-2.878428153));
#145072=CARTESIAN_POINT('Ctrl Pts',(7.08996633,1.327100493,-2.445889906));
#145073=CARTESIAN_POINT('Ctrl Pts',(6.95668143399999,1.392692987,-2.832246392));
#145074=CARTESIAN_POINT('Ctrl Pts',(6.782202682,1.45796923,-3.201831785));
#145075=CARTESIAN_POINT('',(7.08996632981088,1.32710049307755,-2.44588991119078));
#145076=CARTESIAN_POINT('',(6.88561808541865,1.41778968873307,-2.97292172375148));
#145077=CARTESIAN_POINT('Origin',(-0.181717156461203,1.33928595031602,0.0647520808744406));
#145078=CARTESIAN_POINT('Ctrl Pts',(6.65597250213184,1.45719264070752,-2.87411378637646));
#145079=CARTESIAN_POINT('Ctrl Pts',(6.69420791070999,1.4503019869917,-2.89051984943257));
#145080=CARTESIAN_POINT('Ctrl Pts',(6.73248290497789,1.44357824482253,-2.90696703651909));
#145081=CARTESIAN_POINT('Ctrl Pts',(6.80901852462497,1.43045449289926,-2.93989887497759));
#145082=CARTESIAN_POINT('Ctrl Pts',(6.84732220312894,1.42404710664931,-2.95640205460633));
#145083=CARTESIAN_POINT('Ctrl Pts',(6.88561808565608,1.41778968834761,-2.97292172305506));
#145084=CARTESIAN_POINT('',(7.00872698291568,1.32710049321648,-2.29210526022896));
#145085=CARTESIAN_POINT('Origin',(-2.77555756156289E-14,1.41887506699994,
8.43509290193722E-14));
#145086=CARTESIAN_POINT('',(6.8837410893577,1.23689319389077,-2.97726529079312));
#145087=CARTESIAN_POINT('Origin',(-0.181529237000969,1.4820050380168,0.0364971907420908));
#145088=CARTESIAN_POINT('',(6.6411577026872,1.32710049399577,-3.48497121750172));
#145089=CARTESIAN_POINT('Origin',(-0.169510333087188,1.33928284453501,0.0911709027947322));
#145090=CARTESIAN_POINT('Origin',(-0.178938564863871,1.48212079557788,0.0660033679166011));
#145091=CARTESIAN_POINT('Ctrl Pts',(6.657843835,1.457976823,-2.869776205));
#145092=CARTESIAN_POINT('Ctrl Pts',(6.501167561,1.39227158,-3.233263144));
#145093=CARTESIAN_POINT('Ctrl Pts',(6.30585110000001,1.327100493,-3.577532936));
#145094=CARTESIAN_POINT('Ctrl Pts',(6.98108068700001,1.457976823,-2.741261103));
#145095=CARTESIAN_POINT('Ctrl Pts',(6.831420733,1.39227158,-3.122395253));
#145096=CARTESIAN_POINT('Ctrl Pts',(6.641157706,1.327100493,-3.484971208));
#145097=CARTESIAN_POINT('',(6.47350439459855,1.32710049586375,-3.53125208740157));
#145098=CARTESIAN_POINT('Ctrl Pts',(6.30585110000001,1.327100493,-3.577532936));
#145099=CARTESIAN_POINT('Ctrl Pts',(6.110899109,1.392692987,-3.921160304));
#145100=CARTESIAN_POINT('Ctrl Pts',(5.879761546,1.45796923,-4.241568597));
#145101=CARTESIAN_POINT('Ctrl Pts',(6.39841282800001,1.327100493,-3.912839543));
#145102=CARTESIAN_POINT('Ctrl Pts',(6.18518883400001,1.392692987,-4.261510916));
#145103=CARTESIAN_POINT('Ctrl Pts',(5.935339364,1.45796923,-4.584947834));
#145104=CARTESIAN_POINT('',(6.39841282671024,1.32710049307753,-3.91283954797586));
#145105=CARTESIAN_POINT('',(6.08554586929491,1.41778968832474,-4.38362081670148));
#145106=CARTESIAN_POINT('Origin',(-0.163549035479708,1.33928597081891,0.102302120919976));
#145107=CARTESIAN_POINT('Ctrl Pts',(5.88251005789048,1.4571926407563,-4.23775594170644));
#145108=CARTESIAN_POINT('Ctrl Pts',(5.91632472464706,1.45030198716551,-4.26199792231317));
#145109=CARTESIAN_POINT('Ctrl Pts',(5.95016921096982,1.44357824513485,-4.2862885751256));
#145110=CARTESIAN_POINT('Ctrl Pts',(6.01783610014625,1.43045449287505,-4.33490338257605));
#145111=CARTESIAN_POINT('Ctrl Pts',(6.05169656390113,1.42404710665394,-4.35925488554331));
#145112=CARTESIAN_POINT('Ctrl Pts',(6.08554586967107,1.41778968831878,-4.38362081617738));
#145113=CARTESIAN_POINT('',(6.3521319646792,1.32710049321648,-3.74518623834803));
#145114=CARTESIAN_POINT('Origin',(-1.2490009027033E-13,1.41887506700011,
1.69569219776733E-13));
#145115=CARTESIAN_POINT('',(6.08277901767368,1.23689319337626,-4.38745933493388));
#145116=CARTESIAN_POINT('Origin',(-0.169439546157523,1.4820050469827,0.07466746421667));
#145117=CARTESIAN_POINT('',(5.73672532969594,1.32710049399578,-4.8311471225857));
#145118=CARTESIAN_POINT('Origin',(-0.145948341934135,1.33928281056974,0.125479154956001));
#145119=CARTESIAN_POINT('Origin',(-0.160566641850736,1.48212079340995,0.102926998199179));
#145120=CARTESIAN_POINT('Ctrl Pts',(5.88527009200001,1.457976823,-4.233922052));
#145121=CARTESIAN_POINT('Ctrl Pts',(5.654117875,1.39227158,-4.555230101));
#145122=CARTESIAN_POINT('Ctrl Pts',(5.389359975,1.327100493,-4.849463791));
#145123=CARTESIAN_POINT('Ctrl Pts',(6.228576794,1.457976823,-4.17789793));
#145124=CARTESIAN_POINT('Ctrl Pts',(6.00048323,1.39227158,-4.517948909));
#145125=CARTESIAN_POINT('Ctrl Pts',(5.736725335,1.327100493,-4.831147114));
#145126=CARTESIAN_POINT('',(5.5630426434841,1.32710049586375,-4.84030546573543));
#145127=CARTESIAN_POINT('Ctrl Pts',(5.389359975,1.327100493,-4.84946379100001));
#145128=CARTESIAN_POINT('Ctrl Pts',(5.12509612700001,1.392692987,-5.143148427));
#145129=CARTESIAN_POINT('Ctrl Pts',(4.83048412,1.45796923,-5.406378008));
#145130=CARTESIAN_POINT('Ctrl Pts',(5.407676652,1.327100493,-5.19682915100001));
#145131=CARTESIAN_POINT('Ctrl Pts',(5.124483679,1.392692987,-5.491511925));
#145132=CARTESIAN_POINT('Ctrl Pts',(4.810946174,1.45796923,-5.753676817));
#145133=CARTESIAN_POINT('',(5.40767664965581,1.32710049307754,-5.19682915561586));
#145134=CARTESIAN_POINT('',(5.00092029201621,1.41778968872508,-5.58934667278783));
#145135=CARTESIAN_POINT('Origin',(-0.137733409524872,1.3392859291023,0.13506852863573));
#145136=CARTESIAN_POINT('Ctrl Pts',(4.83398798137623,1.4571926407555,-5.40324533971124));
#145137=CARTESIAN_POINT('Ctrl Pts',(4.86180076686648,1.45030198814266,-5.43418970569204));
#145138=CARTESIAN_POINT('Ctrl Pts',(4.88963221080027,1.44357824720297,-5.4651880153085));
#145139=CARTESIAN_POINT('Ctrl Pts',(4.94526634773805,1.43045449293385,-5.52721262607228));
#145140=CARTESIAN_POINT('Ctrl Pts',(4.97310031956659,1.4240471066704,-5.55827380345815));
#145141=CARTESIAN_POINT('Ctrl Pts',(5.00092029250508,1.41778968834774,-5.58934667227415));
#145142=CARTESIAN_POINT('',(5.39851831441096,1.32710049321648,-5.02314647002097));
#145143=CARTESIAN_POINT('Origin',(-2.20309881449055E-13,1.418875067,1.64365049348802E-13));
#145144=CARTESIAN_POINT('',(4.99739295983039,1.23689319338241,-5.592500657182));
#145145=CARTESIAN_POINT('Origin',(-0.149426903870843,1.48200504998636,0.109346318495925));
#145146=CARTESIAN_POINT('',(4.56405005599846,1.32710049399577,-5.95142395623471));
#145147=CARTESIAN_POINT('Origin',(-0.115561916453181,1.33928286887368,0.153920220597338));
#145148=CARTESIAN_POINT('Origin',(-0.134686256036152,1.48212078565201,0.135037521671934));
#145149=CARTESIAN_POINT('Ctrl Pts',(4.837507661,1.457976823,-5.40009441));
#145150=CARTESIAN_POINT('Ctrl Pts',(4.542687921,1.39227158,-5.66419956100001));
#145151=CARTESIAN_POINT('Ctrl Pts',(4.220868368,1.327100493,-5.894639109));
#145152=CARTESIAN_POINT('Ctrl Pts',(5.184831573,1.457976823,-5.419180894));
#145153=CARTESIAN_POINT('Ctrl Pts',(4.88896980099999,1.39227158,-5.702248296));
#145154=CARTESIAN_POINT('Ctrl Pts',(4.564050063,1.327100493,-5.95142394900001));
#145155=CARTESIAN_POINT('',(4.3924592014081,1.32710049586375,-5.92303153945041));
#145156=CARTESIAN_POINT('Ctrl Pts',(4.220868368,1.327100493,-5.894639109));
#145157=CARTESIAN_POINT('Ctrl Pts',(3.899649346,1.392692987,-6.12464864500001));
#145158=CARTESIAN_POINT('Ctrl Pts',(3.555338625,1.45796923,-6.318391192));
#145159=CARTESIAN_POINT('Ctrl Pts',(4.164083527,1.327100493,-6.23782080400001));
#145160=CARTESIAN_POINT('Ctrl Pts',(3.824163362,1.392692987,-6.46473594));
#145161=CARTESIAN_POINT('Ctrl Pts',(3.461598487,1.45796923,-6.653370267));
#145162=CARTESIAN_POINT('',(4.16408352373067,1.32710049307753,-6.23782080798727));
#145163=CARTESIAN_POINT('',(3.68245723961584,1.41778968871537,-6.53372089029738));
#145164=CARTESIAN_POINT('Origin',(-0.105477626068154,1.33928591507701,0.16151946653965));
#145165=CARTESIAN_POINT('Ctrl Pts',(3.55943399894129,1.45719264078608,-6.31608499055301));
#145166=CARTESIAN_POINT('Ctrl Pts',(3.57994441222619,1.45030198841067,-6.35228481987964));
#145167=CARTESIAN_POINT('Ctrl Pts',(3.60046145127134,1.44357824774572,-6.38854134236741));
#145168=CARTESIAN_POINT('Ctrl Pts',(3.64146143676512,1.4304544929359,-6.46107555007232));
#145169=CARTESIAN_POINT('Ctrl Pts',(3.66196743092277,1.4240471066378,-6.4973940157844));
#145170=CARTESIAN_POINT('Ctrl Pts',(3.68245724002035,1.41778968832776,-6.53372089000245));
#145171=CARTESIAN_POINT('',(4.19247594860012,1.32710049321648,-6.06622995573969));
#145172=CARTESIAN_POINT('Origin',(3.16587034365767E-14,1.41887506700044,
3.59955121265187E-14));
#145173=CARTESIAN_POINT('',(3.67833436110066,1.23689319337654,-6.53604286387826));
#145174=CARTESIAN_POINT('Origin',(-0.122427019057876,1.48200506328858,0.138912014578856));
#145175=CARTESIAN_POINT('',(3.17796487359877,1.32710049399579,-6.79341882156193));
#145176=CARTESIAN_POINT('Origin',(-0.0797718656725155,1.3392828592108,0.175164068385654));
#145177=CARTESIAN_POINT('Origin',(-0.102508324529246,1.48212078864541,0.160834037739207));
#145178=CARTESIAN_POINT('Ctrl Pts',(3.563548747,1.457976823,-6.313764355));
#145179=CARTESIAN_POINT('Ctrl Pts',(3.218846929,1.39227158,-6.508317345));
#145180=CARTESIAN_POINT('Ctrl Pts',(2.855013647,1.327100493,-6.664187653));
#145181=CARTESIAN_POINT('Ctrl Pts',(3.89864939,1.457976823,-6.407068982));
#145182=CARTESIAN_POINT('Ctrl Pts',(3.548853577,1.39227158,-6.61991689));
#145183=CARTESIAN_POINT('Ctrl Pts',(3.177964882,1.327100493,-6.793418816));
#145184=CARTESIAN_POINT('',(3.01648924849091,1.32710049586378,-6.7288032416768));
#145185=CARTESIAN_POINT('Ctrl Pts',(2.855013647,1.327100493,-6.664187653));
#145186=CARTESIAN_POINT('Ctrl Pts',(2.491859296,1.392692987,-6.8197671));
#145187=CARTESIAN_POINT('Ctrl Pts',(2.113949448,1.45796923,-6.934963427));
#145188=CARTESIAN_POINT('Ctrl Pts',(2.725782484,1.327100493,-6.987138889));
#145189=CARTESIAN_POINT('Ctrl Pts',(2.345029417,1.392692987,-7.135676088));
#145190=CARTESIAN_POINT('Ctrl Pts',(1.950390303,1.45796923,-7.241959518));
#145191=CARTESIAN_POINT('',(2.72578247995464,1.32710049307753,-6.98713889218714));
#145192=CARTESIAN_POINT('',(2.19180657984862,1.41778968871566,-7.17258558065227));
#145193=CARTESIAN_POINT('Origin',(-0.0682896582737541,1.3392859226996,0.180417665261952));
#145194=CARTESIAN_POINT('Ctrl Pts',(2.11844483962399,1.45719264080791,-6.93359152718499));
#145195=CARTESIAN_POINT('Ctrl Pts',(2.13069383942566,1.45030198735574,-6.97335416332043));
#145196=CARTESIAN_POINT('Ctrl Pts',(2.14293712316127,1.44357824549033,-7.01317359293416));
#145197=CARTESIAN_POINT('Ctrl Pts',(2.16738583696781,1.4304544929153,-7.09282576249553));
#145198=CARTESIAN_POINT('Ctrl Pts',(2.17960501575865,1.42404710663496,-7.13270330513909));
#145199=CARTESIAN_POINT('Ctrl Pts',(2.19180658033942,1.41778968833467,-7.17258558044234));
#145200=CARTESIAN_POINT('',(2.79039806673785,1.32710049321648,-6.82566327049396));
#145201=CARTESIAN_POINT('Origin',(3.71881345162528E-14,1.41887506700011,
-1.01047642475649E-13));
#145202=CARTESIAN_POINT('',(2.18728093607641,1.23689319391963,-7.17396697093756));
#145203=CARTESIAN_POINT('Origin',(-0.089702922527658,1.48200508663554,0.161982950661606));
#145204=CARTESIAN_POINT('',(1.64328158659184,1.32710049399579,-7.31776097262557));
#145205=CARTESIAN_POINT('Origin',(-0.0402517051760135,1.33928286958148,
0.188217277654796));
#145206=CARTESIAN_POINT('Origin',(-0.0655371205933414,1.48212079741191,
0.179109882251318));
#145207=CARTESIAN_POINT('Ctrl Pts',(2.122962255,1.457976823,-6.932209696));
#145208=CARTESIAN_POINT('Ctrl Pts',(1.744496231,1.39227158,-7.048113443));
#145209=CARTESIAN_POINT('Ctrl Pts',(1.355661661,1.327100493,-7.12212619));
#145210=CARTESIAN_POINT('Ctrl Pts',(2.430170694,1.457976823,-7.09536964500001));
#145211=CARTESIAN_POINT('Ctrl Pts',(2.042796905,1.39227158,-7.228045528));
#145212=CARTESIAN_POINT('Ctrl Pts',(1.643281596,1.327100493,-7.317760969));
#145213=CARTESIAN_POINT('',(1.49947161132239,1.32710049586378,-7.21994358306752));
#145214=CARTESIAN_POINT('Ctrl Pts',(1.355661661,1.327100493,-7.12212619));
#145215=CARTESIAN_POINT('Ctrl Pts',(0.967552675,1.392692987,-7.196000825));
#145216=CARTESIAN_POINT('Ctrl Pts',(0.573714344,1.45796923,-7.227264479));
#145217=CARTESIAN_POINT('Ctrl Pts',(1.160026882,1.327100493,-7.409746125));
#145218=CARTESIAN_POINT('Ctrl Pts',(0.756244503,1.392692987,-7.472959952));
#145219=CARTESIAN_POINT('Ctrl Pts',(0.347984036,1.45796923,-7.49192279100001));
#145220=CARTESIAN_POINT('',(1.16002687736292,1.32710049307753,-7.40974612724363));
#145221=CARTESIAN_POINT('',(0.598669480427782,1.41778968873146,-7.47606814079839));
#145222=CARTESIAN_POINT('Origin',(-0.0279086337482035,1.33928591269015,
0.190879995901798));
#145223=CARTESIAN_POINT('Ctrl Pts',(0.57839955397464,1.4571926407453,-7.22689102994081));
#145224=CARTESIAN_POINT('Ctrl Pts',(0.58181438724212,1.45030198803244,-7.26835720625018));
#145225=CARTESIAN_POINT('Ctrl Pts',(0.585211429058528,1.44357824698866,
-7.3098776184735));
#145226=CARTESIAN_POINT('Ctrl Pts',(0.591965684310373,1.43045449291614,
-7.39292332494198));
#145227=CARTESIAN_POINT('Ctrl Pts',(0.595326692564369,1.42404710663884,
-7.43449531507666));
#145228=CARTESIAN_POINT('Ctrl Pts',(0.598669481038226,1.41778968834016,
-7.4760681406904));
#145229=CARTESIAN_POINT('',(1.25784427281769,1.32710049321648,-7.26593615727189));
#145230=CARTESIAN_POINT('Origin',(-3.11030498231779E-14,1.41887506699989,
9.69710423071035E-13));
#145231=CARTESIAN_POINT('',(0.593952685545576,1.23689319338997,-7.47644435575005));
#145232=CARTESIAN_POINT('Origin',(-0.0527841180949516,1.48200502603679,
0.177478958827875));
#145233=CARTESIAN_POINT('',(0.0317602790409959,1.32710049399578,-7.49993275352055));
#145234=CARTESIAN_POINT('Origin',(0.00115051940608922,1.33928289169456,
0.192469725776021));
#145235=CARTESIAN_POINT('Origin',(-0.0255015599625236,1.48212074045013,
0.189010913845458));
#145236=CARTESIAN_POINT('Ctrl Pts',(0.583108408,1.457976823,-7.22651261599999));
#145237=CARTESIAN_POINT('Ctrl Pts',(0.188574829,1.39227158,-7.25834759));
#145238=CARTESIAN_POINT('Ctrl Pts',(-0.207079558,1.327100493,-7.247042021));
#145239=CARTESIAN_POINT('Ctrl Pts',(0.848059918,1.457976823,-7.451898709));
#145240=CARTESIAN_POINT('Ctrl Pts',(0.441221319,1.39227158,-7.49819879));
#145241=CARTESIAN_POINT('Ctrl Pts',(0.031760289,1.327100493,-7.499932752));
#145242=CARTESIAN_POINT('',(-0.0876596520427781,1.32710049586375,-7.37348738629144));
#145243=CARTESIAN_POINT('Ctrl Pts',(-0.207079558,1.327100493,-7.247042021));
#145244=CARTESIAN_POINT('Ctrl Pts',(-0.601995634,1.392692987,-7.235757549));
#145245=CARTESIAN_POINT('Ctrl Pts',(-0.993347006,1.45796923,-7.181626677));
#145246=CARTESIAN_POINT('Ctrl Pts',(-0.459970288,1.327100493,-7.485881867));
#145247=CARTESIAN_POINT('Ctrl Pts',(-0.867901564,1.392692987,-7.460816515));
#145248=CARTESIAN_POINT('Ctrl Pts',(-1.270693578,1.45796923,-7.391572081));
#145249=CARTESIAN_POINT('',(-0.459970293053227,1.32710049307755,-7.48588186820677));
#145250=CARTESIAN_POINT('',(-1.02246073861237,1.41778968870741,-7.42997806403628));
#145251=CARTESIAN_POINT('Origin',(0.0137773865831164,1.33928592088847,0.192416720129659));
#145252=CARTESIAN_POINT('Ctrl Pts',(-0.988691052623812,1.45719264069763,
-7.1822691405059));
#145253=CARTESIAN_POINT('Ctrl Pts',(-0.994270058772122,1.45030198759079,
-7.22349995135523));
#145254=CARTESIAN_POINT('Ctrl Pts',(-0.999878099571577,1.44357824609767,
-7.26477990600654));
#145255=CARTESIAN_POINT('Ctrl Pts',(-1.01113412627181,1.43045449289424,
-7.34733600981738));
#145256=CARTESIAN_POINT('Ctrl Pts',(-1.01678844545818,1.42404710661956,
-7.38865858731562));
#145257=CARTESIAN_POINT('Ctrl Pts',(-1.02246073805733,1.41778968831938,
-7.42997806405372));
#145258=CARTESIAN_POINT('',(-0.333524921664078,1.32710049321648,-7.36646194406049));
#145259=CARTESIAN_POINT('Origin',(1.71493678632895E-13,1.41887506700022,
1.13537651502682E-12));
#145260=CARTESIAN_POINT('',(-1.02714813242582,1.2368931933649,-7.42933151171882));
#145261=CARTESIAN_POINT('Origin',(-0.0133973341289943,1.48200503132719,
0.184676639741399));
#145262=CARTESIAN_POINT('',(-1.58124610403663,1.32710049399577,-7.33141601435253));
#145263=CARTESIAN_POINT('Origin',(0.0424989283865376,1.33928286297151,0.187722593615965));
#145264=CARTESIAN_POINT('Origin',(0.0157264465032626,1.48212080514855,0.190074241480158));
#145265=CARTESIAN_POINT('Ctrl Pts',(-0.984010941,1.457976823,-7.18291183800001));
#145266=CARTESIAN_POINT('Ctrl Pts',(-1.376164122,1.39227158,-7.129189471));
#145267=CARTESIAN_POINT('Ctrl Pts',(-1.760137966,1.327100493,-7.033094222));
#145268=CARTESIAN_POINT('Ctrl Pts',(-0.773705198,1.457976823,-7.459985273));
#145269=CARTESIAN_POINT('Ctrl Pts',(-1.180985284,1.39227158,-7.41774461));
#145270=CARTESIAN_POINT('Ctrl Pts',(-1.581246094,1.327100493,-7.331416015));
#145271=CARTESIAN_POINT('',(-1.67069204708794,1.32710049586378,-7.1822551145251));
#145272=CARTESIAN_POINT('Ctrl Pts',(-1.760137966,1.327100493,-7.033094222));
#145273=CARTESIAN_POINT('Ctrl Pts',(-2.143395296,1.392692987,-6.937178292));
#145274=CARTESIAN_POINT('Ctrl Pts',(-2.513960553,1.45796923,-6.800183993));
#145275=CARTESIAN_POINT('Ctrl Pts',(-2.058459759,1.327100493,-7.211986094));
#145276=CARTESIAN_POINT('Ctrl Pts',(-2.451465519,1.392692987,-7.09981359));
#145277=CARTESIAN_POINT('Ctrl Pts',(-2.829954972,1.45796923,-6.945599676));
#145278=CARTESIAN_POINT('',(-2.05845976416771,1.32710049307754,-7.21198609409039));
#145279=CARTESIAN_POINT('',(-2.59578182999002,1.41778968871659,-7.03647047077191));
#145280=CARTESIAN_POINT('Origin',(0.0548191445060356,1.33928597923113,0.184956220145635));
#145281=CARTESIAN_POINT('Ctrl Pts',(-2.50955156393115,1.45719264070531,
-6.80181232839606));
#145282=CARTESIAN_POINT('Ctrl Pts',(-2.52386354155141,1.45030198756959,
-6.84087986462242));
#145283=CARTESIAN_POINT('Ctrl Pts',(-2.53821443953213,1.44357824604334,
-6.87998915413039));
#145284=CARTESIAN_POINT('Ctrl Pts',(-2.56695442844666,1.43045449288437,
-6.95819542891081));
#145285=CARTESIAN_POINT('Ctrl Pts',(-2.58135968539634,1.42404710665183,
-6.99733639579766));
#145286=CARTESIAN_POINT('Ctrl Pts',(-2.59578182913589,1.41778968833431,
-7.03647047102556));
#145287=CARTESIAN_POINT('',(-1.90929886120832,1.32710049321648,-7.12254015834626));
#145288=CARTESIAN_POINT('Origin',(1.91036422791946E-13,1.41887506700006,
4.19369400317393E-13));
#145289=CARTESIAN_POINT('',(-2.6002206454442,1.23689319337841,-7.03483138298698));
#145290=CARTESIAN_POINT('Origin',(0.0266158908061881,1.4820050282617,0.183238948990568));
#145291=CARTESIAN_POINT('',(-3.1203151776828,1.32710049399577,-6.82009041119354));
#145292=CARTESIAN_POINT('Origin',(0.0818601302556743,1.33928285452991,0.174197751694014));
#145293=CARTESIAN_POINT('Origin',(0.0562190792265915,1.48212077788429,0.182249609777169));
#145294=CARTESIAN_POINT('Ctrl Pts',(-2.505119032,1.457976823,-6.803446085));
#145295=CARTESIAN_POINT('Ctrl Pts',(-2.876555169,1.39227158,-6.666678376));
#145296=CARTESIAN_POINT('Ctrl Pts',(-3.23089428,1.327100493,-6.490286754));
#145297=CARTESIAN_POINT('Ctrl Pts',(-2.359292718,1.457976823,-7.119251215));
#145298=CARTESIAN_POINT('Ctrl Pts',(-2.747970329,1.39227158,-6.990444937));
#145299=CARTESIAN_POINT('Ctrl Pts',(-3.120315168,1.327100493,-6.820090414));
#145300=CARTESIAN_POINT('',(-3.17560473983382,1.32710049586375,-6.6551885764447));
#145301=CARTESIAN_POINT('Ctrl Pts',(-3.23089428,1.327100493,-6.49028675400001));
#145302=CARTESIAN_POINT('Ctrl Pts',(-3.584572177,1.392692987,-6.314224288));
#145303=CARTESIAN_POINT('Ctrl Pts',(-3.917024099,1.45796923,-6.100772263));
#145304=CARTESIAN_POINT('Ctrl Pts',(-3.560697939,1.327100493,-6.600865866));
#145305=CARTESIAN_POINT('Ctrl Pts',(-3.92040167,1.392692987,-6.406831272));
#145306=CARTESIAN_POINT('Ctrl Pts',(-4.256890817,1.45796923,-6.174858749));
#145307=CARTESIAN_POINT('',(-3.5606979440883,1.32710049307754,-6.60086586497412));
#145308=CARTESIAN_POINT('',(-4.04772704802492,1.41778968875794,-6.31394533862323));
#145309=CARTESIAN_POINT('Origin',(0.0932976026754845,1.33928595488629,0.168847532117771));
#145310=CARTESIAN_POINT('Ctrl Pts',(-3.91306823383847,1.45719264065931,
-6.10331033138983));
#145311=CARTESIAN_POINT('Ctrl Pts',(-3.93544396831024,1.45030198834128,
-6.13838783413044));
#145312=CARTESIAN_POINT('Ctrl Pts',(-3.95786668826544,1.4435782477238,-6.17349774635459));
#145313=CARTESIAN_POINT('Ctrl Pts',(-4.00274679509976,1.43045449293981,
-6.24369736267065));
#145314=CARTESIAN_POINT('Ctrl Pts',(-4.02522941605326,1.42404710668986,
-6.27882653124007));
#145315=CARTESIAN_POINT('Ctrl Pts',(-4.0477270473829,1.41778968837934,-6.31394533896706));
#145316=CARTESIAN_POINT('',(-3.39579610831295,1.32710049321648,-6.54557631061584));
#145317=CARTESIAN_POINT('Origin',(-1.22948526359856E-13,1.41887506699989,
-2.29417179697933E-13));
#145318=CARTESIAN_POINT('',(-4.05170973089699,1.23689319338796,-6.31139035807528));
#145319=CARTESIAN_POINT('Origin',(0.065384597887963,1.4820050181001,0.173233331749791));
#145320=CARTESIAN_POINT('',(-4.5134817808578,1.32710049399579,-5.98986496017169));
#145321=CARTESIAN_POINT('Origin',(0.117393698840258,1.33928287631653,0.152527654543123));
#145322=CARTESIAN_POINT('Origin',(0.0940831752252352,1.48212079763046,0.165903555497967));
#145323=CARTESIAN_POINT('Ctrl Pts',(-3.909090541,1.457976823,-6.105858756));
#145324=CARTESIAN_POINT('Ctrl Pts',(-4.242441693,1.39227158,-5.89244081));
#145325=CARTESIAN_POINT('Ctrl Pts',(-4.550577568,1.327100493,-5.644000691));
#145326=CARTESIAN_POINT('Ctrl Pts',(-3.834562334,1.457976823,-6.445628884));
#145327=CARTESIAN_POINT('Ctrl Pts',(-4.186463335,1.39227158,-6.236279827));
#145328=CARTESIAN_POINT('Ctrl Pts',(-4.513481772,1.327100493,-5.989864965));
#145329=CARTESIAN_POINT('',(-4.53202968383947,1.32710049586375,-5.81693281721754));
#145330=CARTESIAN_POINT('Ctrl Pts',(-4.550577568,1.327100493,-5.64400069100001));
#145331=CARTESIAN_POINT('Ctrl Pts',(-4.85813844599999,1.392692987,-5.396024174));
#145332=CARTESIAN_POINT('Ctrl Pts',(-5.136931951,1.45796923,-5.116095203));
#145333=CARTESIAN_POINT('Ctrl Pts',(-4.896441841,1.327100493,-5.681096487));
#145334=CARTESIAN_POINT('Ctrl Pts',(-5.206024196,1.392692987,-5.414272644));
#145335=CARTESIAN_POINT('Ctrl Pts',(-5.484779179,1.45796923,-5.11538829));
#145336=CARTESIAN_POINT('',(-4.89644184573733,1.32710049307754,-5.68109648490863));
#145337=CARTESIAN_POINT('',(-5.31040504790184,1.41778968873636,-5.29618714009526));
#145338=CARTESIAN_POINT('Origin',(0.127413838397398,1.33928592785563,0.144844021089803));
#145339=CARTESIAN_POINT('Ctrl Pts',(-5.13361418158607,1.45719264066822,
-5.11942432679471));
#145340=CARTESIAN_POINT('Ctrl Pts',(-5.16300740979459,1.45030198839048,
-5.14887161529756));
#145341=CARTESIAN_POINT('Ctrl Pts',(-5.19245349208817,1.44357824782183,
-5.17834045502075));
#145342=CARTESIAN_POINT('Ctrl Pts',(-5.25137516994794,1.43045449293496,
-5.23725094736362));
#145343=CARTESIAN_POINT('Ctrl Pts',(-5.28088389277246,1.42404710665468,
-5.26672571666975));
#145344=CARTESIAN_POINT('Ctrl Pts',(-5.31040504754952,1.41778968836063,
-5.29618714036849));
#145345=CARTESIAN_POINT('',(-4.72350970347309,1.32710049321648,-5.66254858985662));
#145346=CARTESIAN_POINT('Origin',(1.14188172806173E-12,1.41887506700039,
1.19348975147204E-12));
#145347=CARTESIAN_POINT('',(-5.31374537261227,1.23689319338848,-5.29283573454965));
#145348=CARTESIAN_POINT('Origin',(0.101096017214738,1.48200506766614,0.155127518954754));
#145349=CARTESIAN_POINT('',(-5.69560299159707,1.32710049399576,-4.87956008041305));
#145350=CARTESIAN_POINT('Origin',(0.147437970801125,1.33928284907969,0.123725396097225));
#145351=CARTESIAN_POINT('Origin',(0.12754751488669,1.4821207950477,0.141799326758713));
#145352=CARTESIAN_POINT('Ctrl Pts',(-5.130277321,1.457976823,-5.122768257));
#145353=CARTESIAN_POINT('Ctrl Pts',(-5.409956358,1.39227158,-4.84267926));
#145354=CARTESIAN_POINT('Ctrl Pts',(-5.657480906,1.327100493,-4.533807429));
#145355=CARTESIAN_POINT('Ctrl Pts',(-5.130532076,1.457976823,-5.47061610999999));
#145356=CARTESIAN_POINT('Ctrl Pts',(-5.429201969,1.39227158,-5.190513205));
#145357=CARTESIAN_POINT('Ctrl Pts',(-5.695602984,1.327100493,-4.879560087));
#145358=CARTESIAN_POINT('',(-5.676541956198,1.32710049586375,-4.70668374449455));
#145359=CARTESIAN_POINT('Ctrl Pts',(-5.657480906,1.327100493,-4.533807429));
#145360=CARTESIAN_POINT('Ctrl Pts',(-5.904543561,1.392692987,-4.225511967));
#145361=CARTESIAN_POINT('Ctrl Pts',(-6.116642575,1.45796923,-3.892195218));
#145362=CARTESIAN_POINT('Ctrl Pts',(-6.00323356500001,1.327100493,-4.49568535));
#145363=CARTESIAN_POINT('Ctrl Pts',(-6.248218817,1.392692987,-4.168548645));
#145364=CARTESIAN_POINT('Ctrl Pts',(-6.456205362,1.45796923,-3.81672796));
#145365=CARTESIAN_POINT('',(-6.00323356916003,1.32710049307753,-4.49568534695027));
#145366=CARTESIAN_POINT('',(-6.32477440834189,1.41778968840243,-4.0307851183038));
#145367=CARTESIAN_POINT('Origin',(0.155571997664578,1.33928597345127,0.114067300424577));
#145368=CARTESIAN_POINT('Ctrl Pts',(-6.11411803582837,1.45719264067073,
-3.8961597311879));
#145369=CARTESIAN_POINT('Ctrl Pts',(-6.14915437013618,1.45030198703788,
-3.91859988746354));
#145370=CARTESIAN_POINT('Ctrl Pts',(-6.18424695723015,1.44357824495913,
-3.94104973005705));
#145371=CARTESIAN_POINT('Ctrl Pts',(-6.25445507822899,1.43045449290793,
-3.98591649887835));
#145372=CARTESIAN_POINT('Ctrl Pts',(-6.2896101072235,1.42404710669724,-4.00835866099077));
#145373=CARTESIAN_POINT('Ctrl Pts',(-6.32477440900803,1.41778968840232,
-4.03078511725927));
#145374=CARTESIAN_POINT('',(-5.83035723468124,1.32710049321648,-4.51474639055735));
#145375=CARTESIAN_POINT('Ctrl Pts',(-6.111578035,1.457976823,-3.900142807));
#145376=CARTESIAN_POINT('Ctrl Pts',(-6.324507477,1.39227158,-3.56647941));
#145377=CARTESIAN_POINT('Ctrl Pts',(-6.499846725,1.327100493,-3.21161837));
#145378=CARTESIAN_POINT('Ctrl Pts',(-6.18660384,1.457976823,-4.239803406));
#145379=CARTESIAN_POINT('Ctrl Pts',(-6.418077152,1.39227158,-3.902043953));
#145380=CARTESIAN_POINT('Ctrl Pts',(-6.611404132,1.327100493,-3.541092403));
#145381=CARTESIAN_POINT('',(-6.61140413777676,1.32710049397328,-3.54109239737487));
#145382=CARTESIAN_POINT('Origin',(0.155048589728213,1.48212078598296,0.111065447385177));
#145383=CARTESIAN_POINT('',(-6.55562543653298,1.32710049586378,-3.37635537090293));
#145384=CARTESIAN_POINT('Origin',(1.2190769227427E-12,1.41887506700017,
7.255480938273E-13));
#145385=CARTESIAN_POINT('',(-6.32731618627607,1.23689319339346,-4.0267939941612));
#145386=CARTESIAN_POINT('Origin',(0.132080172192659,1.4820050475739,0.129767978857629));
#145387=CARTESIAN_POINT('Origin',(0.170588507694899,1.33928286359429,0.0891381241734063));
#145388=CARTESIAN_POINT('Ctrl Pts',(-6.499846725,1.327100493,-3.21161837));
#145389=CARTESIAN_POINT('Ctrl Pts',(-6.67485878100001,1.392692987,-2.857419517));
#145390=CARTESIAN_POINT('Ctrl Pts',(-6.81034579,1.45796923,-2.48630051));
#145391=CARTESIAN_POINT('Ctrl Pts',(-6.829320759,1.327100493,-3.100060963));
#145392=CARTESIAN_POINT('Ctrl Pts',(-6.998253671,1.392692987,-2.727907945));
#145393=CARTESIAN_POINT('Ctrl Pts',(-7.125746559,1.45796923,-2.339601672));
#145394=CARTESIAN_POINT('',(-6.82932076240318,1.32710049307753,-3.10006095913137));
#145395=CARTESIAN_POINT('',(-6.66458374142768,1.32710049321648,-3.15583966770864));
#145396=CARTESIAN_POINT('',(-7.04340434993579,1.41778968871992,-2.57690806175739));
#145397=CARTESIAN_POINT('Origin',(0.176455929188738,1.33928593254331,0.0779571161467857));
#145398=CARTESIAN_POINT('Ctrl Pts',(-6.80873252634029,1.45719264069918,
-2.49071503621278));
#145399=CARTESIAN_POINT('Ctrl Pts',(-6.84777370210102,1.45030198685207,
-2.50509877827222));
#145400=CARTESIAN_POINT('Ctrl Pts',(-6.88687189798469,1.44357824454109,
-2.5194798876386));
#145401=CARTESIAN_POINT('Ctrl Pts',(-6.96508361886916,1.43045449287376,
-2.54820502485674));
#145402=CARTESIAN_POINT('Ctrl Pts',(-7.00424114436195,1.42404710665038,
-2.56256520971215));
#145403=CARTESIAN_POINT('Ctrl Pts',(-7.04340434957966,1.41778968834056,
-2.5769080625643));
#145404=CARTESIAN_POINT('Origin',(1.00050176476962E-12,1.41887506700017,
2.88180937446647E-13));
#145405=CARTESIAN_POINT('',(-7.21806337412951,1.32710049399578,-2.03704716480427));
#145406=CARTESIAN_POINT('Origin',(0.175299450457352,1.48212077473128,0.0751379289430554));
#145407=CARTESIAN_POINT('',(-7.04502872775174,1.23689319337173,-2.57246384258005));
#145408=CARTESIAN_POINT('Origin',(0.156888684396083,1.48200503551944,0.0983408221406673));
#145409=CARTESIAN_POINT('Origin',(0.18576194971784,1.33928286595704,0.0503825141191694));
#145410=CARTESIAN_POINT('Ctrl Pts',(-6.807108153,1.457976823,-2.495151015));
#145411=CARTESIAN_POINT('Ctrl Pts',(-6.94333165600001,1.39227158,-2.123514947));
#145412=CARTESIAN_POINT('Ctrl Pts',(-7.038286935,1.327100493,-1.739257605));
#145413=CARTESIAN_POINT('Ctrl Pts',(-6.953396885,1.457976823,-2.810742208));
#145414=CARTESIAN_POINT('Ctrl Pts',(-7.106850181,1.39227158,-2.431119463));
#145415=CARTESIAN_POINT('Ctrl Pts',(-7.21806337,1.327100493,-2.037047174));
#145416=CARTESIAN_POINT('',(-7.12817515699226,1.32710049586377,-1.88815237254077));
#145417=CARTESIAN_POINT('Ctrl Pts',(-7.03828693500001,1.327100493,-1.739257605));
#145418=CARTESIAN_POINT('Ctrl Pts',(-7.133065024,1.392692987,-1.355717306));
#145419=CARTESIAN_POINT('Ctrl Pts',(-7.185604805,1.45796923,-0.964149153));
#145420=CARTESIAN_POINT('Ctrl Pts',(-7.336076504,1.327100493,-1.55948117));
#145421=CARTESIAN_POINT('Ctrl Pts',(-7.421057961,1.392692987,-1.159713301));
#145422=CARTESIAN_POINT('Ctrl Pts',(-7.462095765,1.45796923,-0.753078211));
#145423=CARTESIAN_POINT('',(-7.33607650651547,1.32710049307755,-1.55948116545248));
#145424=CARTESIAN_POINT('',(-7.43269253076441,1.41778968874203,-1.00253764978341));
#145425=CARTESIAN_POINT('Origin',(0.189088830370302,1.33928591181856,0.0382017050499422));
#145426=CARTESIAN_POINT('Ctrl Pts',(-7.18497825126012,1.45719264073011,
-0.968807273831989));
#145427=CARTESIAN_POINT('Ctrl Pts',(-7.22619874120902,1.45030198757908,
-0.974462032848068));
#145428=CARTESIAN_POINT('Ctrl Pts',(-7.26747435133052,1.44357824604435,
-0.980101962887697));
#145429=CARTESIAN_POINT('Ctrl Pts',(-7.35003259024956,1.43045449292146,
-0.991342315629223));
#145430=CARTESIAN_POINT('Ctrl Pts',(-7.39136165010221,1.42404710665964,
-0.996949056884781));
#145431=CARTESIAN_POINT('Ctrl Pts',(-7.4326925306375,1.41778968836924,-1.00253765030459));
#145432=CARTESIAN_POINT('',(-7.18718171920089,1.32710049321647,-1.64936938880337));
#145433=CARTESIAN_POINT('Origin',(-4.55798593312906E-13,1.418875067,-1.81712284108571E-13));
#145434=CARTESIAN_POINT('',(-7.4333235556527,1.23689319336187,-0.997848140297996));
#145435=CARTESIAN_POINT('Origin',(0.174360937114771,1.48200502583182,0.0623152203927678));
#145436=CARTESIAN_POINT('',(-7.48721398905891,1.32710049399578,-0.437751873145054));
#145437=CARTESIAN_POINT('Origin',(0.192249680126575,1.33928287077358,0.00927126713742912));
#145438=CARTESIAN_POINT('Origin',(0.187353116954269,1.48212077437295,0.035697005883375));
#145439=CARTESIAN_POINT('Ctrl Pts',(-7.18434546000001,1.457976823,-0.973488735));
#145440=CARTESIAN_POINT('Ctrl Pts',(-7.237493363,1.39227158,-0.581257285));
#145441=CARTESIAN_POINT('Ctrl Pts',(-7.247624671,1.327100493,-0.185571088));
#145442=CARTESIAN_POINT('Ctrl Pts',(-7.39505682,1.457976823,-1.250253828));
#145443=CARTESIAN_POINT('Ctrl Pts',(-7.463314795,1.39227158,-0.846518529));
#145444=CARTESIAN_POINT('Ctrl Pts',(-7.487213987,1.327100493,-0.437751883));
#145445=CARTESIAN_POINT('',(-7.3674193297415,1.32710049586377,-0.311661467971566));
#145446=CARTESIAN_POINT('Ctrl Pts',(-7.247624671,1.327100493,-0.185571088));
#145447=CARTESIAN_POINT('Ctrl Pts',(-7.257737073,1.392692987,0.209376739));
#145448=CARTESIAN_POINT('Ctrl Pts',(-7.224872925,1.45796923,0.603084746));
#145449=CARTESIAN_POINT('Ctrl Pts',(-7.49980546600001,1.327100493,0.054018228));
#145450=CARTESIAN_POINT('Ctrl Pts',(-7.496861828,1.392692987,0.462708249000001));
#145451=CARTESIAN_POINT('Ctrl Pts',(-7.449525667,1.45796923,0.868658351));
#145452=CARTESIAN_POINT('',(-7.49980546747305,1.32710049307754,0.0540182329649172));
#145453=CARTESIAN_POINT('',(-7.47443626940087,1.41778968869693,0.618710308786432));
#145454=CARTESIAN_POINT('Origin',(0.192880487321588,1.33928596308834,-0.00333996688423702));
#145455=CARTESIAN_POINT('Ctrl Pts',(-7.22526237813834,1.45719264078058,
0.598400839381944));
#145456=CARTESIAN_POINT('Ctrl Pts',(-7.2667347605517,1.4503019878546,0.601739472284441));
#145457=CARTESIAN_POINT('Ctrl Pts',(-7.30825778632754,1.44357824657058,
0.605104436637895));
#145458=CARTESIAN_POINT('Ctrl Pts',(-7.39130220627353,1.43045449290774,
0.611874458356217));
#145459=CARTESIAN_POINT('Ctrl Pts',(-7.43287029941618,1.42404710661155,
0.615283325799165));
#145460=CARTESIAN_POINT('Ctrl Pts',(-7.47443626939145,1.41778968829495,
0.618710308166733));
#145461=CARTESIAN_POINT('',(-7.37371506848807,1.32710049321647,-0.0657764313371904));
#145462=CARTESIAN_POINT('Origin',(9.80118763926896E-13,1.41887506699967,
-1.8033670260223E-13));
#145463=CARTESIAN_POINT('',(-7.47404443556084,1.23689319340572,0.62342583135813));
#145464=CARTESIAN_POINT('Origin',(0.183680684593376,1.4820050856247,0.0233758683937176));
#145465=CARTESIAN_POINT('',(-7.40627079988776,1.32710049399577,1.182012209077));
#145466=CARTESIAN_POINT('Origin',(0.189748364559003,1.33928286084184,-0.0322735212225897));
#145467=CARTESIAN_POINT('Origin',(0.190646781264282,1.48212080209065,-0.00541294759872427));
#145468=CARTESIAN_POINT('Ctrl Pts',(-7.225650757,1.457976823,0.593692797));
#145469=CARTESIAN_POINT('Ctrl Pts',(-7.193237924,1.39227158,0.988179322000001));
#145470=CARTESIAN_POINT('Ctrl Pts',(-7.118071532,1.327100493,1.376792527));
#145471=CARTESIAN_POINT('Ctrl Pts',(-7.490932116,1.457976823,0.368695032));
#145472=CARTESIAN_POINT('Ctrl Pts',(-7.470803103,1.39227158,0.77766467));
#145473=CARTESIAN_POINT('Ctrl Pts',(-7.4062708,1.327100493,1.182012199));
#145474=CARTESIAN_POINT('',(-7.26217116295609,1.32710049586375,1.27940238027789));
#145475=CARTESIAN_POINT('Ctrl Pts',(-7.118071532,1.327100493,1.376792527));
#145476=CARTESIAN_POINT('Ctrl Pts',(-7.043045404,1.392692987,1.764680561));
#145477=CARTESIAN_POINT('Ctrl Pts',(-6.926314018,1.45796923,2.142119073));
#145478=CARTESIAN_POINT('Ctrl Pts',(-7.31285186,1.327100493,1.664991795));
#145479=CARTESIAN_POINT('Ctrl Pts',(-7.222120769,1.392692987,2.063494074));
#145480=CARTESIAN_POINT('Ctrl Pts',(-7.088624029,1.45796923,2.449777414));
#145481=CARTESIAN_POINT('',(-7.312851860368,1.32710049307753,1.66499180013895));
#145482=CARTESIAN_POINT('',(-7.1666836756946,1.41778968871963,2.21102806086381));
#145483=CARTESIAN_POINT('Origin',(0.187653049799481,1.33928591086236,-0.0447254774391825));
#145484=CARTESIAN_POINT('Ctrl Pts',(-6.9277012673583,1.45719264075247,2.13762839408098));
#145485=CARTESIAN_POINT('Ctrl Pts',(-6.9674863419721,1.45030198768196,2.14980430826909));
#145486=CARTESIAN_POINT('Ctrl Pts',(-7.00731521566478,1.44357824623667,
2.16201682514904));
#145487=CARTESIAN_POINT('Ctrl Pts',(-7.08696274679494,1.43045449289663,
2.18648066253496));
#145488=CARTESIAN_POINT('Ctrl Pts',(-7.12682619505161,1.4240471066461,2.19874574376936));
#145489=CARTESIAN_POINT('Ctrl Pts',(-7.16668367588273,1.41778968833019,
2.21102806005493));
#145490=CARTESIAN_POINT('',(-7.21546169627581,1.32710049321647,1.52089215969151));
#145491=CARTESIAN_POINT('Origin',(8.56953397132543E-13,1.41887506700022,
-3.25585912397397E-13));
#145492=CARTESIAN_POINT('',(-7.16528730475997,1.23689319336947,2.21554910444165));
#145493=CARTESIAN_POINT('Origin',(0.184411325039866,1.48200508223814,-0.0166565348855671));
#145494=CARTESIAN_POINT('',(-6.97901861873992,1.32710049399577,2.74650671479504));
#145495=CARTESIAN_POINT('Origin',(0.178374116318473,1.33928284139354,-0.0723092163023792));
#145496=CARTESIAN_POINT('Origin',(0.185026189465232,1.48212080143722,-0.0462699162185873));
#145497=CARTESIAN_POINT('Ctrl Pts',(-6.929092656,1.457976823,2.133113913));
#145498=CARTESIAN_POINT('Ctrl Pts',(-6.812634675,1.39227158,2.511409761));
#145499=CARTESIAN_POINT('Ctrl Pts',(-6.65568528,1.327100493,2.874778854));
#145500=CARTESIAN_POINT('Ctrl Pts',(-7.236539753,1.457976823,1.970404122));
#145501=CARTESIAN_POINT('Ctrl Pts',(-7.128964961,1.39227158,2.365485134));
#145502=CARTESIAN_POINT('Ctrl Pts',(-6.979018621,1.327100493,2.746506705));
#145503=CARTESIAN_POINT('',(-6.81735194381297,1.32710049586377,2.81064279571972));
#145504=CARTESIAN_POINT('Ctrl Pts',(-6.65568528000001,1.327100493,2.874778854));
#145505=CARTESIAN_POINT('Ctrl Pts',(-6.499028759,1.392692987,3.237469881));
#145506=CARTESIAN_POINT('Ctrl Pts',(-6.303888365,1.45796923,3.580990293));
#145507=CARTESIAN_POINT('Ctrl Pts',(-6.783957428,1.327100493,3.198112195));
#145508=CARTESIAN_POINT('Ctrl Pts',(-6.609681369,1.392692987,3.567793211));
#145509=CARTESIAN_POINT('Ctrl Pts',(-6.396266209,1.45796923,3.916347607));
#145510=CARTESIAN_POINT('',(-6.78395742725216,1.32710049307754,3.19811220012484));
#145511=CARTESIAN_POINT('',(-6.52382491847514,1.41778968868913,3.6999605981568));
#145512=CARTESIAN_POINT('Origin',(0.173651152695408,1.33928595551319,-0.0840196691405803));
#145513=CARTESIAN_POINT('Ctrl Pts',(-6.30620854436299,1.45719264078498,
3.57690282142813));
#145514=CARTESIAN_POINT('Ctrl Pts',(-6.34244600492938,1.45030198761464,
3.59734668484766));
#145515=CARTESIAN_POINT('Ctrl Pts',(-6.37871837217705,1.44357824605803,
3.61783571074209));
#145516=CARTESIAN_POINT('Ctrl Pts',(-6.45124478528863,1.43045449290822,
3.65884946141489));
#145517=CARTESIAN_POINT('Ctrl Pts',(-6.487539618582,1.42404710661262,3.67939725500589));
#145518=CARTESIAN_POINT('Ctrl Pts',(-6.52382491865153,1.41778968830209,
3.69996059772776));
#145519=CARTESIAN_POINT('',(-6.71982135455065,1.32710049321647,3.03644552328139));
#145520=CARTESIAN_POINT('Origin',(-4.71844785465692E-13,1.41887506699989,
3.31765864780564E-13));
#145521=CARTESIAN_POINT('',(-6.52148930308131,1.23689319340118,3.70407576405903));
#145522=CARTESIAN_POINT('Origin',(0.176518965345178,1.48200502730424,-0.0559099623388354));
#145523=CARTESIAN_POINT('',(-6.22543528466758,1.32710049399579,4.18257761909792));
#145524=CARTESIAN_POINT('Origin',(0.158659732073103,1.33928284933523,-0.108963977220405));
#145525=CARTESIAN_POINT('Origin',(0.170753578389468,1.48212083418589,-0.0849632151973495));
#145526=CARTESIAN_POINT('Ctrl Pts',(-6.308537883,1.457976823,3.572792994));
#145527=CARTESIAN_POINT('Ctrl Pts',(-6.113480201,1.39227158,3.917209472));
#145528=CARTESIAN_POINT('Ctrl Pts',(-5.882086581,1.327100493,4.238343716));
#145529=CARTESIAN_POINT('Ctrl Pts',(-6.643774834,1.457976823,3.479979305));
#145530=CARTESIAN_POINT('Ctrl Pts',(-6.453784342,1.39227158,3.842698142));
#145531=CARTESIAN_POINT('Ctrl Pts',(-6.225435289,1.327100493,4.18257761));
#145532=CARTESIAN_POINT('',(-6.05376092498255,1.32710049586377,4.210460677403));
#145533=CARTESIAN_POINT('Ctrl Pts',(-5.882086581,1.327100493,4.238343716));
#145534=CARTESIAN_POINT('Ctrl Pts',(-5.651124753,1.392692987,4.558878708));
#145535=CARTESIAN_POINT('Ctrl Pts',(-5.38669989800001,1.45796923,4.852418387));
#145536=CARTESIAN_POINT('Ctrl Pts',(-5.937852687,1.327100493,4.58169242400001));
#145537=CARTESIAN_POINT('Ctrl Pts',(-5.688180615,1.392692987,4.905266302));
#145538=CARTESIAN_POINT('Ctrl Pts',(-5.404826091,1.45796923,5.199793739));
#145539=CARTESIAN_POINT('',(-5.93785268517258,1.32710049307753,4.5816924288298));
#145540=CARTESIAN_POINT('',(-5.5759193587845,1.41778968871294,5.01588708998643));
#145541=CARTESIAN_POINT('Origin',(0.15152941117498,1.33928597138522,-0.11938510053391));
#145542=CARTESIAN_POINT('Ctrl Pts',(-5.38984451854538,1.45719264075697,
4.84892524811201));
#145543=CARTESIAN_POINT('Ctrl Pts',(-5.42083994031133,1.45030198781947,
4.87668112715906));
#145544=CARTESIAN_POINT('Ctrl Pts',(-5.45185974380203,1.44357824651703,
4.90448861659059));
#145545=CARTESIAN_POINT('Ctrl Pts',(-5.51387378814892,1.430454492903,4.96013452544236));
#145546=CARTESIAN_POINT('Ctrl Pts',(-5.54490290006085,1.42404710665486,
4.98800423913264));
#145547=CARTESIAN_POINT('Ctrl Pts',(-5.57591935929175,1.41778968833113,
5.0158870893365));
#145548=CARTESIAN_POINT('',(-5.90996963479974,1.32710049321647,4.41001806892825));
#145549=CARTESIAN_POINT('Origin',(5.01768765426291E-13,1.41887506700006,
-5.17814957579077E-13));
#145550=CARTESIAN_POINT('',(-5.57275370974732,1.23689319394209,5.01940395734413));
#145551=CARTESIAN_POINT('Origin',(0.160373399338236,1.48200502642637,-0.092549463413848));
#145552=CARTESIAN_POINT('',(-5.18075751483762,1.32710049399576,5.42307584194051));
#145553=CARTESIAN_POINT('Origin',(0.131526047477788,1.33928284504139,-0.140523358241085));
#145554=CARTESIAN_POINT('Origin',(0.148496874513592,1.48212079504295,-0.119683813909308));
#145555=CARTESIAN_POINT('Ctrl Pts',(-5.39300289,1.457976823,4.845412245));
#145556=CARTESIAN_POINT('Ctrl Pts',(-5.128466186,1.39227158,5.139844821));
#145557=CARTESIAN_POINT('Ctrl Pts',(-4.833448051,1.327100493,5.40372833700001));
#145558=CARTESIAN_POINT('Ctrl Pts',(-5.74035438700001,1.457976823,4.826834523));
#145559=CARTESIAN_POINT('Ctrl Pts',(-5.476831939,1.39227158,5.140230856));
#145560=CARTESIAN_POINT('Ctrl Pts',(-5.180757521,1.327100493,5.42307583399999));
#145561=CARTESIAN_POINT('',(-5.00710277312064,1.32710049586375,5.41340209741272));
#145562=CARTESIAN_POINT('Ctrl Pts',(-4.83344805100001,1.327100493,5.403728337));
#145563=CARTESIAN_POINT('Ctrl Pts',(-4.538980434,1.392692987,5.667119433));
#145564=CARTESIAN_POINT('Ctrl Pts',(-4.217635331,1.45796923,5.89695279));
#145565=CARTESIAN_POINT('Ctrl Pts',(-4.814100554,1.327100493,5.751037807));
#145566=CARTESIAN_POINT('Ctrl Pts',(-4.500706857,1.392692987,6.01337459200001));
#145567=CARTESIAN_POINT('Ctrl Pts',(-4.160662311,1.45796923,6.240103295));
#145568=CARTESIAN_POINT('',(-4.81410055117882,1.32710049307753,5.75103781132099));
#145569=CARTESIAN_POINT('',(-4.36729000692376,1.4177896887255,6.09727627632803));
#145570=CARTESIAN_POINT('Origin',(0.122322587513753,1.33928593777335,-0.149168433170697));
#145571=CARTESIAN_POINT('Ctrl Pts',(-4.22145735396846,1.45719264066533,
5.8942173198239));
#145572=CARTESIAN_POINT('Ctrl Pts',(-4.24576142183573,1.45030198902915,
5.92798737492905));
#145573=CARTESIAN_POINT('Ctrl Pts',(-4.27007820568039,1.44357824918164,
5.9618130737019));
#145574=CARTESIAN_POINT('Ctrl Pts',(-4.31868018037653,1.43045449292316,
6.02948921218209));
#145575=CARTESIAN_POINT('Ctrl Pts',(-4.34299268436843,1.42404710665061,
6.06337768943683));
#145576=CARTESIAN_POINT('Ctrl Pts',(-4.36729000739379,1.41778968834208,
6.09727627592036));
#145577=CARTESIAN_POINT('',(-4.82377430351144,1.32710049321647,5.57738307112523));
#145578=CARTESIAN_POINT('Origin',(-1.12475133373646E-12,1.41887506699978,
1.52178616930065E-12));
#145579=CARTESIAN_POINT('',(-4.36344234637142,1.23689319339394,6.10003040005458));
#145580=CARTESIAN_POINT('Origin',(0.136728527353329,1.48200503359054,-0.124861215505688));
#145581=CARTESIAN_POINT('',(-3.89383328225337,1.32710049399577,6.40999706643645));
#145582=CARTESIAN_POINT('Origin',(0.098242796547533,1.33928284083096,-0.165512376615569));
#145583=CARTESIAN_POINT('Origin',(0.119296622147308,1.48212081958442,-0.148808097778507));
#145584=CARTESIAN_POINT('Ctrl Pts',(-4.225297077,1.457976823,5.891465405));
#145585=CARTESIAN_POINT('Ctrl Pts',(-3.903650793,1.39227158,6.122146739));
#145586=CARTESIAN_POINT('Ctrl Pts',(-3.558802862,1.327100493,6.31644062700001));
#145587=CARTESIAN_POINT('Ctrl Pts',(-4.568521349,1.457976823,5.947992324));
#145588=CARTESIAN_POINT('Ctrl Pts',(-4.243788962,1.39227158,6.197412088));
#145589=CARTESIAN_POINT('Ctrl Pts',(-3.89383329,1.327100493,6.40999706));
#145590=CARTESIAN_POINT('',(-3.72631806086074,1.32710049586377,6.36321885236559));
#145591=CARTESIAN_POINT('Ctrl Pts',(-3.558802862,1.327100493,6.316440627));
#145592=CARTESIAN_POINT('Ctrl Pts',(-3.214598434,1.392692987,6.510371952));
#145593=CARTESIAN_POINT('Ctrl Pts',(-2.851358824,1.45796923,6.665752235));
#145594=CARTESIAN_POINT('Ctrl Pts',(-3.465246429,1.327100493,6.651471054));
#145595=CARTESIAN_POINT('Ctrl Pts',(-3.102785048,1.392692987,6.84030417));
#145596=CARTESIAN_POINT('Ctrl Pts',(-2.721950586,1.45796923,6.988632556));
#145597=CARTESIAN_POINT('',(-3.46524642530106,1.32710049307754,6.65147105762962));
#145598=CARTESIAN_POINT('',(-2.95445102820031,1.41778968870866,6.8935636005648));
#145599=CARTESIAN_POINT('Origin',(0.0873959663614748,1.33928595894931,-0.171976734249653));
#145600=CARTESIAN_POINT('Ctrl Pts',(-2.85567953540615,1.45719264073027,
6.66390233981683));
#145601=CARTESIAN_POINT('Ctrl Pts',(-2.87215582771297,1.45030198748113,
6.70210753480414));
#145602=CARTESIAN_POINT('Ctrl Pts',(-2.88863257782738,1.44357824583997,
6.7403698081076));
#145603=CARTESIAN_POINT('Ctrl Pts',(-2.92154988752125,1.43045449288956,
6.81691168460353));
#145604=CARTESIAN_POINT('Ctrl Pts',(-2.93800895772761,1.42404710660756,
6.85523433781912));
#145605=CARTESIAN_POINT('Ctrl Pts',(-2.95445102865523,1.41778968831593,
6.89356360030554));
#145606=CARTESIAN_POINT('',(-3.51202464667584,1.32710049321647,6.48395583986311));
#145607=CARTESIAN_POINT('Origin',(1.34441069388203E-13,1.41887506699994,
-3.36970035208495E-13));
#145608=CARTESIAN_POINT('',(-2.95010126896827,1.23689319338589,6.89542620135343));
#145609=CARTESIAN_POINT('Origin',(0.106690364867912,1.48200498463762,-0.151334503244875));
#145610=CARTESIAN_POINT('',(-2.42483773306109,1.32710049399578,7.09719395161996));
#145611=CARTESIAN_POINT('Origin',(0.0603656246863346,1.33928285255758,-0.182762001417611));
#145612=CARTESIAN_POINT('Origin',(0.0845181387472432,1.48212075608598,-0.170974189347677));
#145613=CARTESIAN_POINT('Ctrl Pts',(-2.860021067,1.457976823,6.66204019));
#145614=CARTESIAN_POINT('Ctrl Pts',(-2.496305027,1.39227158,6.81818388));
#145615=CARTESIAN_POINT('Ctrl Pts',(-2.117752007,1.327100493,6.933803173));
#145616=CARTESIAN_POINT('Ctrl Pts',(-3.183069331,1.457976823,6.791028614));
#145617=CARTESIAN_POINT('Ctrl Pts',(-2.812311129,1.39227158,6.964809219));
#145618=CARTESIAN_POINT('Ctrl Pts',(-2.424837742,1.327100493,7.09719394700001));
#145619=CARTESIAN_POINT('',(-2.27129485780885,1.32710049586377,7.01549856540383));
#145620=CARTESIAN_POINT('Ctrl Pts',(-2.117752007,1.327100493,6.933803173));
#145621=CARTESIAN_POINT('Ctrl Pts',(-1.739905385,1.392692987,7.049206714));
#145622=CARTESIAN_POINT('Ctrl Pts',(-1.351755947,1.45796923,7.122868513));
#145623=CARTESIAN_POINT('Ctrl Pts',(-1.954361232,1.327100493,7.240888908));
#145624=CARTESIAN_POINT('Ctrl Pts',(-1.55978046,1.392692987,7.347388728));
#145625=CARTESIAN_POINT('Ctrl Pts',(-1.155963477,1.45796923,7.410381126));
#145626=CARTESIAN_POINT('',(-1.95436122763021,1.32710049307753,7.24088891073354));
#145627=CARTESIAN_POINT('',(-1.40346520327497,1.41778968873029,7.36751555254718));
#145628=CARTESIAN_POINT('Origin',(0.0483827133056874,1.33928592280152,-0.18674325857323));
#145629=CARTESIAN_POINT('Ctrl Pts',(-1.35637331540349,1.4571926407211,7.12199069258409));
#145630=CARTESIAN_POINT('Ctrl Pts',(-1.3642514132043,1.45030198781702,7.16284458524739));
#145631=CARTESIAN_POINT('Ctrl Pts',(-1.3721176878921,1.4435782465617,7.20375431971896));
#145632=CARTESIAN_POINT('Ctrl Pts',(-1.38781116924433,1.43045449289558,
7.28558294295861));
#145633=CARTESIAN_POINT('Ctrl Pts',(-1.39564719791282,1.42404710664426,
7.32654784733475));
#145634=CARTESIAN_POINT('Ctrl Pts',(-1.40346520396996,1.41778968834456,
7.36751555235564));
#145635=CARTESIAN_POINT('',(-2.03605662078526,1.32710049321647,7.08734604013077));
#145636=CARTESIAN_POINT('Origin',(-3.24176449573166E-13,1.41887506699978,
1.41249859031412E-12));
#145637=CARTESIAN_POINT('',(-1.39881673462794,1.23689319337654,7.36839953684967));
#145638=CARTESIAN_POINT('Origin',(0.0716636014155367,1.48200507732621,-0.170731826487561));
#145639=CARTESIAN_POINT('',(-0.842459466245457,1.32710049399578,7.45253393658554));
#145640=CARTESIAN_POINT('Origin',(0.0196658882621228,1.33928282222093,-0.19146587916326));
#145641=CARTESIAN_POINT('Origin',(0.0457878018278116,1.48212077089942,-0.185146050959324));
#145642=CARTESIAN_POINT('Ctrl Pts',(-1.361013652,1.457976823,7.12110538));
#145643=CARTESIAN_POINT('Ctrl Pts',(-0.972234813,1.39227158,7.19541032));
#145644=CARTESIAN_POINT('Ctrl Pts',(-0.577677421,1.327100493,7.226948789));
#145645=CARTESIAN_POINT('Ctrl Pts',(-1.648780528,1.457976823,7.316523954));
#145646=CARTESIAN_POINT('Ctrl Pts',(-1.249332754,1.39227158,7.406539611));
#145647=CARTESIAN_POINT('Ctrl Pts',(-0.842459476,1.327100493,7.452533934));
#145648=CARTESIAN_POINT('',(-0.710068431037556,1.32710049586375,7.33974136318937));
#145649=CARTESIAN_POINT('Origin',(-3.47486796281604E-14,1.41887506699989,
1.1666015375944E-13));
#145650=CARTESIAN_POINT('',(0.217874905393073,1.23689319448374,7.49683470012955));
#145651=CARTESIAN_POINT('',(-0.352092272117407,1.32710049307754,7.49173084474164));
#145652=CARTESIAN_POINT('Origin',(0.0332858491289362,1.48200502004435,-0.182145603701761));
#145653=CARTESIAN_POINT('Origin',(-0.0219534349632636,1.33928287002982,
-0.191217377589924));
#145654=CARTESIAN_POINT('Origin',(0.00710727857594066,1.33928593431685,
-0.192778422559777));
#145655=CARTESIAN_POINT('Ctrl Pts',(-0.577677421000001,1.327100493,7.226948789));
#145656=CARTESIAN_POINT('Ctrl Pts',(-0.183856294,1.392692987,7.258428405));
#145657=CARTESIAN_POINT('Ctrl Pts',(0.211053536,1.45796923,7.246927377));
#145658=CARTESIAN_POINT('Ctrl Pts',(-0.352092277,1.327100493,7.49173084300001));
#145659=CARTESIAN_POINT('Ctrl Pts',(0.0561577300000001,1.392692987,7.510917554));
#145660=CARTESIAN_POINT('Ctrl Pts',(0.4640752,1.45796923,7.485628511));
#145661=CARTESIAN_POINT('',(-0.464884850334583,1.32710049321647,7.3593398159157));
#145662=CARTESIAN_POINT('Ctrl Pts',(-1.16045022,4.559946053,7.409679837));
#145663=CARTESIAN_POINT('Ctrl Pts',(-0.75366617,4.494288122,7.473387399));
#145664=CARTESIAN_POINT('Ctrl Pts',(-0.342352821,4.429844992,7.49218222900001));
#145665=CARTESIAN_POINT('Ctrl Pts',(-1.356068566,4.559946053,7.122048725));
#145666=CARTESIAN_POINT('Ctrl Pts',(-0.965075178000001,4.494288122,7.19649554));
#145667=CARTESIAN_POINT('Ctrl Pts',(-0.568281989,4.429844992,7.227693656));
#145668=CARTESIAN_POINT('',(-0.594913062081674,4.46959751864088,7.4763679983408));
#145669=CARTESIAN_POINT('Ctrl Pts',(-0.59491306336725,4.46959751863648,
7.47636799821831));
#145670=CARTESIAN_POINT('Ctrl Pts',(-0.591300604527993,4.46339351469901,
7.43481934129684));
#145671=CARTESIAN_POINT('Ctrl Pts',(-0.587666952126791,4.45704680092971,
7.39327085177197));
#145672=CARTESIAN_POINT('Ctrl Pts',(-0.580360792552427,4.44406034774631,
7.31026810206512));
#145673=CARTESIAN_POINT('Ctrl Pts',(-0.576684369626278,4.43741364858974,
7.26876929900358));
#145674=CARTESIAN_POINT('Ctrl Pts',(-0.572986203044206,4.43060907880598,
7.22732224375387));
#145675=CARTESIAN_POINT('',(-1.16045021425437,4.55994605309726,7.40967983744685));
#145676=CARTESIAN_POINT('Origin',(0.0501922216378608,4.6963258830081,-0.179678134303866));
#145677=CARTESIAN_POINT('',(-1.25825939098333,4.5599460533341,7.26586428134924));
#145678=CARTESIAN_POINT('Ctrl Pts',(-2.42543142521891,4.429837254,7.097537917381));
#145679=CARTESIAN_POINT('Ctrl Pts',(-2.04083356846316,4.494719353,7.22896598944729));
#145680=CARTESIAN_POINT('Ctrl Pts',(-1.64428585990226,4.559946053,7.31806573418139));
#145681=CARTESIAN_POINT('Ctrl Pts',(-1.63065611435896,4.56218796060514,
7.32112818246309));
#145682=CARTESIAN_POINT('Ctrl Pts',(-1.61702636881566,4.56442986821038,
7.32419063074491));
#145683=CARTESIAN_POINT('Ctrl Pts',(-2.117720602,4.429837254,6.933812764));
#145684=CARTESIAN_POINT('Ctrl Pts',(-1.741994603,4.494719353,7.048566756));
#145685=CARTESIAN_POINT('Ctrl Pts',(-1.356068566,4.559946053,7.122048725));
#145686=CARTESIAN_POINT('Ctrl Pts',(-1.34280389804382,4.56218796060514,
7.12457437454447));
#145687=CARTESIAN_POINT('Ctrl Pts',(-1.32953923008762,4.56442986821038,
7.12710002408904));
#145688=CARTESIAN_POINT('',(-1.64369966917306,4.55994605198798,7.3176670746967));
#145689=CARTESIAN_POINT('',(-1.49988410426399,4.55994605006201,7.21985790168456));
#145690=CARTESIAN_POINT('',(-2.18820244725389,4.46959751862817,7.17368594600435));
#145691=CARTESIAN_POINT('Origin',(0.0432519951682417,4.55357071574317,-0.187915365400194));
#145692=CARTESIAN_POINT('Ctrl Pts',(-2.11325074753863,4.43060907881227,
6.93517636918274));
#145693=CARTESIAN_POINT('Ctrl Pts',(-2.12577234002776,4.43741364592441,
6.97485940339133));
#145694=CARTESIAN_POINT('Ctrl Pts',(-2.13828382085451,4.44406034235223,
7.01459764794111));
#145695=CARTESIAN_POINT('Ctrl Pts',(-2.16326220951458,4.4570467462429,7.0940889297557));
#145696=CARTESIAN_POINT('Ctrl Pts',(-2.17574248873862,4.4633934037901,7.13388453421944));
#145697=CARTESIAN_POINT('Ctrl Pts',(-2.18820244614369,4.46959751862594,
7.17368594635225));
#145698=CARTESIAN_POINT('Ctrl Pts',(-2.726181675,4.559946053,6.986983146));
#145699=CARTESIAN_POINT('Ctrl Pts',(-2.342603253,4.494288122,7.136647807));
#145700=CARTESIAN_POINT('Ctrl Pts',(-1.944946514,4.429844992,7.243423435));
#145701=CARTESIAN_POINT('Ctrl Pts',(-2.855394386,4.559946053,6.664024527));
#145702=CARTESIAN_POINT('Ctrl Pts',(-2.489546071,4.494288122,6.82078283800001));
#145703=CARTESIAN_POINT('Ctrl Pts',(-2.108736358,4.429844992,6.936550365));
#145704=CARTESIAN_POINT('',(-2.72618166947526,4.55994605320497,6.98698314764743));
#145705=CARTESIAN_POINT('Origin',(0.087644175324966,4.69632600826713,-0.164687271233922));
#145706=CARTESIAN_POINT('',(-2.79078802860555,4.5599460533341,6.8255038372746));
#145707=CARTESIAN_POINT('Origin',(-4.74880551548651E-13,4.65175593299822,
1.38040620600854E-12));
#145708=CARTESIAN_POINT('',(-2.19171665066047,4.65066950022866,7.17261306109147));
#145709=CARTESIAN_POINT('Origin',(0.0629454791939865,4.69641603009044,-0.180826038642827));
#145710=CARTESIAN_POINT('Origin',(0.0709662625895141,4.55357344854477,-0.17904150220209));
#145711=CARTESIAN_POINT('Ctrl Pts',(-3.89448703711139,4.429837254,6.41020536374285));
#145712=CARTESIAN_POINT('Ctrl Pts',(-3.54713401530404,4.494719353,6.62123789183932));
#145713=CARTESIAN_POINT('Ctrl Pts',(-3.17901118206042,4.559946053,6.79350056986478));
#145714=CARTESIAN_POINT('Ctrl Pts',(-3.16635842794052,4.56218796065315,
6.79942141234521));
#145715=CARTESIAN_POINT('Ctrl Pts',(-3.15370567382063,4.56442986830639,
6.80534225482578));
#145716=CARTESIAN_POINT('Ctrl Pts',(-3.558774254,4.429837254,6.316456745));
#145717=CARTESIAN_POINT('Ctrl Pts',(-3.216501235,4.494719353,6.509297835));
#145718=CARTESIAN_POINT('Ctrl Pts',(-2.855394386,4.559946053,6.664024527));
#145719=CARTESIAN_POINT('Ctrl Pts',(-2.84298277835493,4.56218796065315,
6.66934263990384));
#145720=CARTESIAN_POINT('Ctrl Pts',(-2.83057117070987,4.56442986830639,
6.67466075280755));
#145721=CARTESIAN_POINT('',(-3.17835299299463,4.5599460519893,6.79323724515001));
#145722=CARTESIAN_POINT('',(-3.01687367847068,4.559946050062,6.72863089041115));
#145723=CARTESIAN_POINT('',(-3.67917391567943,4.46959751860266,6.53557031160943));
#145724=CARTESIAN_POINT('Origin',(0.0826369678524574,4.55357068133953,-0.174223947254913));
#145725=CARTESIAN_POINT('Ctrl Pts',(-3.55470203692773,4.43060907877665,
6.31874935623179));
#145726=CARTESIAN_POINT('Ctrl Pts',(-3.57546156005755,4.43741364568478,
6.3548128496631));
#145727=CARTESIAN_POINT('Ctrl Pts',(-3.59622307647419,4.44406034190139,
6.39093243628689));
#145728=CARTESIAN_POINT('Ctrl Pts',(-3.63770575509226,4.45704674429609,
6.46319563253993));
#145729=CARTESIAN_POINT('Ctrl Pts',(-3.65844912392703,4.46339339986109,
6.49937793472558));
#145730=CARTESIAN_POINT('Ctrl Pts',(-3.67917391449682,4.46959751860046,
6.535570312287));
#145731=CARTESIAN_POINT('Ctrl Pts',(-4.164439905,4.559946053,6.237582888));
#145732=CARTESIAN_POINT('Ctrl Pts',(-3.822002811,4.494288122,6.466206494));
#145733=CARTESIAN_POINT('Ctrl Pts',(-3.45659667,4.429844992,6.655970212));
#145734=CARTESIAN_POINT('Ctrl Pts',(-4.221205138,4.559946053,5.894397949));
#145735=CARTESIAN_POINT('Ctrl Pts',(-3.897608556,4.494288122,6.12613791));
#145736=CARTESIAN_POINT('Ctrl Pts',(-3.55058856,4.429844992,6.321061689));
#145737=CARTESIAN_POINT('',(-4.16443989995725,4.55994605320497,6.23758289079854));
#145738=CARTESIAN_POINT('Origin',(0.120998139083789,4.69632601466772,-0.141996301290852));
#145739=CARTESIAN_POINT('',(-4.19282251981636,4.5599460533341,6.06599041966374));
#145740=CARTESIAN_POINT('Origin',(-8.21825246744012E-13,4.65175593300022,
1.48665801891212E-12));
#145741=CARTESIAN_POINT('',(-3.68237532060303,4.65066950023331,6.53376706031242));
#145742=CARTESIAN_POINT('Origin',(0.100346144501832,4.69641608322633,-0.16306706225985));
#145743=CARTESIAN_POINT('Origin',(0.107795750829115,4.55357342128508,-0.159599980214508));
#145744=CARTESIAN_POINT('Ctrl Pts',(-5.18144076307036,4.429837254,5.42313873171298));
#145745=CARTESIAN_POINT('Ctrl Pts',(-4.88757441730978,4.494719353,5.70390806884768));
#145746=CARTESIAN_POINT('Ctrl Pts',(-4.56508947560136,4.559946053,5.95127886750963));
#145747=CARTESIAN_POINT('Ctrl Pts',(-4.55400534158494,4.56218796073192,
5.9597812523639));
#145748=CARTESIAN_POINT('Ctrl Pts',(-4.54292120756855,4.56442986846394,
5.96828363721818));
#145749=CARTESIAN_POINT('Ctrl Pts',(-4.833423576,4.429837254,5.403750228));
#145750=CARTESIAN_POINT('Ctrl Pts',(-4.540607845,4.494719353,5.665661383));
#145751=CARTESIAN_POINT('Ctrl Pts',(-4.221205138,4.559946053,5.894397949));
#145752=CARTESIAN_POINT('Ctrl Pts',(-4.21022694351181,4.56218796073192,
5.90225985640743));
#145753=CARTESIAN_POINT('Ctrl Pts',(-4.19924874902359,4.56442986846394,
5.91012176381473));
#145754=CARTESIAN_POINT('',(-4.56439006760927,4.55994605198929,5.95116319036086));
#145755=CARTESIAN_POINT('',(-4.39279759295034,4.55994605006201,5.92278057629117));
#145756=CARTESIAN_POINT('',(-4.99811130094148,4.46959751858828,5.59185867318702));
#145757=CARTESIAN_POINT('Origin',(0.118157854640977,4.55357071768602,-0.152386075058663));
#145758=CARTESIAN_POINT('Ctrl Pts',(-4.8299394093612,4.43060907886738,5.40686464598623));
#145759=CARTESIAN_POINT('Ctrl Pts',(-4.85796618330899,4.43741364862199,
5.43762232418592));
#145760=CARTESIAN_POINT('Ctrl Pts',(-4.88600696371074,4.44406034775626,
5.46843435724498));
#145761=CARTESIAN_POINT('Ctrl Pts',(-4.94205422368869,4.45704674368818,
5.53009049988148));
#145762=CARTESIAN_POINT('Ctrl Pts',(-4.97009074661369,4.46339339863389,
5.56096766560843));
#145763=CARTESIAN_POINT('Ctrl Pts',(-4.99811129988664,4.46959751858598,
5.5918586741443));
#145764=CARTESIAN_POINT('Ctrl Pts',(-5.407973553,4.559946053,5.196520186));
#145765=CARTESIAN_POINT('Ctrl Pts',(-5.122689766,4.494288122,5.493412553));
#145766=CARTESIAN_POINT('Ctrl Pts',(-4.806620207,4.429844992,5.75729121900001));
#145767=CARTESIAN_POINT('Ctrl Pts',(-5.38963702999999,4.559946053,4.849155874));
#145768=CARTESIAN_POINT('Ctrl Pts',(-5.123423198,4.494288122,5.145041583));
#145769=CARTESIAN_POINT('Ctrl Pts',(-4.826419186,4.429844992,5.410007194));
#145770=CARTESIAN_POINT('',(-5.40797354865546,4.55994605320499,5.19652018986508));
#145771=CARTESIAN_POINT('Origin',(0.148694027502743,4.6963259891713,-0.112665215829012));
#145772=CARTESIAN_POINT('',(-5.39880529010589,4.5599460533341,5.02283803149846));
#145773=CARTESIAN_POINT('Origin',(-1.28803218091278E-12,4.651755933,1.4510961876546E-12));
#145774=CARTESIAN_POINT('',(-5.00085021307748,4.65066950024506,5.58940937371014));
#145775=CARTESIAN_POINT('Origin',(0.133054720112198,4.69641603606148,-0.137683229129221));
#145776=CARTESIAN_POINT('Origin',(0.139584834903529,4.55357340357966,-0.132695705850141));
#145777=CARTESIAN_POINT('Ctrl Pts',(-6.22611607791649,4.429837254,4.1824921598369));
#145778=CARTESIAN_POINT('Ctrl Pts',(-5.99947727212079,4.494719353,4.51986984361682));
#145779=CARTESIAN_POINT('Ctrl Pts',(-5.73770925906248,4.559946053,4.83078198081904));
#145780=CARTESIAN_POINT('Ctrl Pts',(-5.72871202741551,4.56218796072055,
4.84146834577086));
#145781=CARTESIAN_POINT('Ctrl Pts',(-5.71971479576868,4.56442986844111,
4.85215471072267));
#145782=CARTESIAN_POINT('Ctrl Pts',(-5.882067385,4.429837254,4.238370357));
#145783=CARTESIAN_POINT('Ctrl Pts',(-5.65240067800001,4.494719353,4.557104901));
#145784=CARTESIAN_POINT('Ctrl Pts',(-5.38963703,4.559946053,4.849155874));
#145785=CARTESIAN_POINT('Ctrl Pts',(-5.38060557737204,4.56218796072055,
4.85919396164141));
#145786=CARTESIAN_POINT('Ctrl Pts',(-5.37157412474406,4.56442986844111,
4.86923204928272));
#145787=CARTESIAN_POINT('',(-5.73700133724454,4.55994605198842,4.83081935903903));
#145788=CARTESIAN_POINT('',(-5.56331917461028,4.55994605006201,4.83998762566662));
#145789=CARTESIAN_POINT('',(-6.08334255721317,4.46959751861104,4.38667793822612));
#145790=CARTESIAN_POINT('Origin',(0.148154028825501,4.55357072817546,-0.123423031031687));
#145791=CARTESIAN_POINT('Ctrl Pts',(-5.87933418335156,4.43060907880993,
4.2421609543172));
#145792=CARTESIAN_POINT('Ctrl Pts',(-5.9133176837977,4.43741364562489,4.2661745966159));
#145793=CARTESIAN_POINT('Ctrl Pts',(-5.94732654614253,4.44406034175098,
4.29023831074314));
#145794=CARTESIAN_POINT('Ctrl Pts',(-6.01531773827986,4.45704674491822,
4.3384044895316));
#145795=CARTESIAN_POINT('Ctrl Pts',(-6.04933646796366,4.46339340112161,
4.3625327456653));
#145796=CARTESIAN_POINT('Ctrl Pts',(-6.08334255646149,4.46959751860884,
4.38667793928535));
#145797=CARTESIAN_POINT('Ctrl Pts',(-6.398636369,4.559946053,3.912473977));
#145798=CARTESIAN_POINT('Ctrl Pts',(-6.183845441,4.494288122,4.263752746));
#145799=CARTESIAN_POINT('Ctrl Pts',(-5.93189152599999,4.429844992,4.589407688));
#145800=CARTESIAN_POINT('Ctrl Pts',(-6.306055484,4.559946053,3.577172659));
#145801=CARTESIAN_POINT('Ctrl Pts',(-6.109672265,4.494288122,3.92336883));
#145802=CARTESIAN_POINT('Ctrl Pts',(-5.876571816,4.429844992,4.245986775));
#145803=CARTESIAN_POINT('',(-6.39863636559543,4.55994605320497,3.91247398167052));
#145804=CARTESIAN_POINT('Origin',(0.16943747854313,4.69632601282118,-0.0780664411189724));
#145805=CARTESIAN_POINT('',(-6.35234592546061,4.5599460533341,3.74482331976313));
#145806=CARTESIAN_POINT('Origin',(-1.21864324187371E-13,4.65175593299933,
1.00613961606655E-13));
#145807=CARTESIAN_POINT('',(-6.08549090775826,4.65066949967397,4.38369711683319));
#145808=CARTESIAN_POINT('Origin',(0.159541818170423,4.69641603271111,-0.105861446073009));
#145809=CARTESIAN_POINT('Origin',(0.164847346774489,4.55357340755019,-0.0995869337445715));
#145810=CARTESIAN_POINT('Ctrl Pts',(-6.97966512498879,4.429837254,2.74627690292657));
#145811=CARTESIAN_POINT('Ctrl Pts',(-6.83085123720195,4.494719353,3.12448752840191));
#145812=CARTESIAN_POINT('Ctrl Pts',(-6.64204013411244,4.559946053,3.48440309746244));
#145813=CARTESIAN_POINT('Ctrl Pts',(-6.63555050530195,4.56218796073003,
3.49677376003527));
#145814=CARTESIAN_POINT('Ctrl Pts',(-6.62906087649148,4.56442986846015,
3.50914442260804));
#145815=CARTESIAN_POINT('Ctrl Pts',(-6.655672259,4.429837254,2.874808998));
#145816=CARTESIAN_POINT('Ctrl Pts',(-6.49989353800001,4.494719353,3.235463259));
#145817=CARTESIAN_POINT('Ctrl Pts',(-6.30605548400001,4.559946053,3.577172659));
#145818=CARTESIAN_POINT('Ctrl Pts',(-6.29939307379623,4.56218796073003,
3.58891755710594));
#145819=CARTESIAN_POINT('Ctrl Pts',(-6.29273066359246,4.56442986846015,
3.60066245521194));
#145820=CARTESIAN_POINT('',(-6.64135679832003,4.55994605198842,3.48459178406735));
#145821=CARTESIAN_POINT('',(-6.47370613432616,4.559946050062,3.53088223240309));
#145822=CARTESIAN_POINT('',(-6.88412347607716,4.46959751862992,2.97638101838741));
#145823=CARTESIAN_POINT('Origin',(0.171222655052026,4.55357076022744,-0.0886887757941202));
#145824=CARTESIAN_POINT('Ctrl Pts',(-6.65381782566217,4.43060907892645,
2.87909853088944));
#145825=CARTESIAN_POINT('Ctrl Pts',(-6.69216903292966,4.43741364556175,
2.89524529925262));
#145826=CARTESIAN_POINT('Ctrl Pts',(-6.7305557728328,4.44406034147083,2.91143551654796));
#145827=CARTESIAN_POINT('Ctrl Pts',(-6.80731167828225,4.45704674547839,
2.94385950258702));
#145828=CARTESIAN_POINT('Ctrl Pts',(-6.84572193411808,4.46339340219066,
2.96011063365308));
#145829=CARTESIAN_POINT('Ctrl Pts',(-6.8841234755912,4.46959751862791,2.97638101953514));
#145830=CARTESIAN_POINT('Ctrl Pts',(-7.090106059,4.559946053,2.445484832));
#145831=CARTESIAN_POINT('Ctrl Pts',(-6.955851376,4.494288122,2.8347246));
#145832=CARTESIAN_POINT('Ctrl Pts',(-6.779794189,4.429844992,3.206928554));
#145833=CARTESIAN_POINT('Ctrl Pts',(-6.927609792,4.559946053,2.137924827));
#145834=CARTESIAN_POINT('Ctrl Pts',(-6.81023984700001,4.494288122,2.518243711));
#145835=CARTESIAN_POINT('Ctrl Pts',(-6.65194247900001,4.429844992,2.883428734));
#145836=CARTESIAN_POINT('',(-7.09010605667977,4.55994605320498,2.44548483733953));
#145837=CARTESIAN_POINT('Origin',(0.182257792442442,4.69632597364402,-0.0398171190939184));
#145838=CARTESIAN_POINT('',(-7.00885792486393,4.5599460533341,2.29170483144534));
#145839=CARTESIAN_POINT('Origin',(-1.40946282423116E-13,4.65175593299845,
2.21177243187043E-14));
#145840=CARTESIAN_POINT('',(-6.8855808109066,4.65066950021868,2.97300805498941));
#145841=CARTESIAN_POINT('Origin',(0.178568934787088,4.69641602588422,-0.0690897061486873));
#145842=CARTESIAN_POINT('Origin',(0.182401267354205,4.55357341209628,-0.0618212237820231));
#145843=CARTESIAN_POINT('Ctrl Pts',(-7.40685278759499,4.429837254,1.18164879132162));
#145844=CARTESIAN_POINT('Ctrl Pts',(-7.34282219046977,4.494719353,1.58300764889506));
#145845=CARTESIAN_POINT('Ctrl Pts',(-7.23579659428889,4.559946053,1.97509739842135));
#145846=CARTESIAN_POINT('Ctrl Pts',(-7.23211801628928,4.56218796065734,
1.98857391972049));
#145847=CARTESIAN_POINT('Ctrl Pts',(-7.22843943828966,4.56442986831468,
2.00205044101955));
#145848=CARTESIAN_POINT('Ctrl Pts',(-7.118065296,4.429837254,1.376824766));
#145849=CARTESIAN_POINT('Ctrl Pts',(-7.0434586,4.494719353,1.762534951));
#145850=CARTESIAN_POINT('Ctrl Pts',(-6.927609792,4.559946053,2.137924827));
#145851=CARTESIAN_POINT('Ctrl Pts',(-6.92362795128529,4.56218796065734,
2.15082735675371));
#145852=CARTESIAN_POINT('Ctrl Pts',(-6.91964611057047,4.56442986831468,
2.16372988650748));
#145853=CARTESIAN_POINT('',(-7.23516979657245,4.55994605198842,1.97542857061927));
#145854=CARTESIAN_POINT('',(-7.08138978994764,4.559946050062,2.0566767108959));
#145855=CARTESIAN_POINT('',(-7.36301043261897,4.46959751860092,1.42691183008964));
#145856=CARTESIAN_POINT('Origin',(0.186285024016406,4.55357072321,-0.0498074645394533));
#145857=CARTESIAN_POINT('Ctrl Pts',(-7.11717634030228,4.43060907880928,
1.38141266024738));
#145858=CARTESIAN_POINT('Ctrl Pts',(-7.15810199827393,4.43741364586804,
1.38893755061707));
#145859=CARTESIAN_POINT('Ctrl Pts',(-7.19907169877002,4.44406034223659,
1.39649723577526));
#145860=CARTESIAN_POINT('Ctrl Pts',(-7.28100328301253,4.45704674475147,
1.41166291447601));
#145861=CARTESIAN_POINT('Ctrl Pts',(-7.32200903658237,4.46339340079517,
1.41927703266189));
#145862=CARTESIAN_POINT('Ctrl Pts',(-7.36301043237867,4.46959751859857,
1.42691183138207));
#145863=CARTESIAN_POINT('Ctrl Pts',(-7.450050271,4.559946053,0.864147535));
#145864=CARTESIAN_POINT('Ctrl Pts',(-7.402609431,4.494288122,1.273147882));
#145865=CARTESIAN_POINT('Ctrl Pts',(-7.310681212,4.429844992,1.674497005));
#145866=CARTESIAN_POINT('Ctrl Pts',(-7.225236766,4.559946053,0.598710006));
#145867=CARTESIAN_POINT('Ctrl Pts',(-7.192368183,4.494288122,0.995368314));
#145868=CARTESIAN_POINT('Ctrl Pts',(-7.116275704,4.429844992,1.386044769));
#145869=CARTESIAN_POINT('',(-7.45005026987186,4.55994605320497,0.86414754067111));
#145870=CARTESIAN_POINT('Origin',(0.186556548936415,4.69632596822184,0.000293759629906298));
#145871=CARTESIAN_POINT('',(-7.33764351829699,4.5599460533341,0.731428772536595));
#145872=CARTESIAN_POINT('Origin',(6.76542155630955E-13,4.65175593299956,
-1.68105546843877E-13));
#145873=CARTESIAN_POINT('',(-7.36370860840548,4.65066949966057,1.42330444080266));
#145874=CARTESIAN_POINT('Origin',(0.189246192904705,4.69641605414231,-0.0290873467067651));
#145875=CARTESIAN_POINT('Origin',(0.191426669989561,4.55357342761404,-0.0211650195628771));
#145876=CARTESIAN_POINT('Ctrl Pts',(-7.48770424678088,4.429837254,-0.438231905223869));
#145877=CARTESIAN_POINT('Ctrl Pts',(-7.51145093953738,4.494719353,-0.0324919097257988));
#145878=CARTESIAN_POINT('Ctrl Pts',(-7.49121524818656,4.559946053,0.373438339122528));
#145879=CARTESIAN_POINT('Ctrl Pts',(-7.4905197270101,4.56218796064393,0.387390572299871));
#145880=CARTESIAN_POINT('Ctrl Pts',(-7.48982420583371,4.56442986828785,
0.401342805477214));
#145881=CARTESIAN_POINT('Ctrl Pts',(-7.24762551100001,4.429837254,-0.185538262));
#145882=CARTESIAN_POINT('Ctrl Pts',(-7.257679367,4.494719353,0.207192467));
#145883=CARTESIAN_POINT('Ctrl Pts',(-7.225236766,4.559946053,0.598710006));
#145884=CARTESIAN_POINT('Ctrl Pts',(-7.22412168099383,4.56218796064393,
0.612166859764027));
#145885=CARTESIAN_POINT('Ctrl Pts',(-7.2230065959878,4.56442986828785,0.625623713528053));
#145886=CARTESIAN_POINT('',(-7.49067429688774,4.55994605198842,0.373896511680142));
#145887=CARTESIAN_POINT('',(-7.35795552980536,4.559946050062,0.486303271575305));
#145888=CARTESIAN_POINT('',(-7.49761120473734,4.4695975186588,-0.189278169159026));
#145889=CARTESIAN_POINT('Origin',(0.19263692254358,4.5535706981198,-0.00859721874756657));
#145890=CARTESIAN_POINT('Ctrl Pts',(-7.24774360047122,4.43060907884376,
-0.18086653100126));
#145891=CARTESIAN_POINT('Ctrl Pts',(-7.28933008475596,4.4374136486107,-0.18231537550547));
#145892=CARTESIAN_POINT('Ctrl Pts',(-7.33096706380868,4.44406034775353,
-0.183739706672199));
#145893=CARTESIAN_POINT('Ctrl Pts',(-7.41424328253091,4.45704674665977,
-0.186541461035159));
#145894=CARTESIAN_POINT('Ctrl Pts',(-7.45592716814081,4.463393404623,-0.187920382063682));
#145895=CARTESIAN_POINT('Ctrl Pts',(-7.49761120477416,4.46959751865698,
-0.189278168036705));
#145896=CARTESIAN_POINT('Ctrl Pts',(-7.461638412,4.559946053,-0.75759634));
#145897=CARTESIAN_POINT('Ctrl Pts',(-7.503229697,4.494288122,-0.347959816));
#145898=CARTESIAN_POINT('Ctrl Pts',(-7.499728906,4.429844992,0.063767838));
#145899=CARTESIAN_POINT('Ctrl Pts',(-7.185019699,4.559946053,-0.96849983));
#145900=CARTESIAN_POINT('Ctrl Pts',(-7.238189376,4.494288122,-0.574049398));
#145901=CARTESIAN_POINT('Ctrl Pts',(-7.247859787,4.429844992,-0.176149108));
#145902=CARTESIAN_POINT('',(-7.46163841211182,4.55994605320497,-0.757596334230097));
#145903=CARTESIAN_POINT('Origin',(0.182131760323845,4.69632599733105,0.0403910335739126));
#145904=CARTESIAN_POINT('',(-7.32332905573954,4.5599460533341,-0.863048082967379));
#145905=CARTESIAN_POINT('Origin',(-2.32886626649886E-13,4.65175593299889,
2.85958322993052E-14));
#145906=CARTESIAN_POINT('',(-7.49751757547009,4.65066949966848,-0.192951307338631));
#145907=CARTESIAN_POINT('Origin',(0.191074840713347,4.69641604436513,0.012275030549841));
#145908=CARTESIAN_POINT('Origin',(0.191501065218327,4.55357338433389,0.0204808851773172));
#145909=CARTESIAN_POINT('Ctrl Pts',(-7.21843897666819,4.429837254,-2.03762136479284));
#145910=CARTESIAN_POINT('Ctrl Pts',(-7.32885259013124,4.494719353,-1.6464721815396));
#145911=CARTESIAN_POINT('Ctrl Pts',(-7.39635300274173,4.559946053,-1.24568228100516));
#145912=CARTESIAN_POINT('Ctrl Pts',(-7.39867306023058,4.56218796068555,
-1.23190672654212));
#145913=CARTESIAN_POINT('Ctrl Pts',(-7.40099311771942,4.5644298683711,-1.21813117207905));
#145914=CARTESIAN_POINT('Ctrl Pts',(-7.038294813,4.429837254,-1.739225727));
#145915=CARTESIAN_POINT('Ctrl Pts',(-7.13253911200001,4.494719353,-1.357838106));
#145916=CARTESIAN_POINT('Ctrl Pts',(-7.18501969900001,4.559946053,-0.96849983));
#145917=CARTESIAN_POINT('Ctrl Pts',(-7.18682350988321,4.56218796068555,
-0.955117879460748));
#145918=CARTESIAN_POINT('Ctrl Pts',(-7.18862732076655,4.5644298683711,-0.941735928921482));
#145919=CARTESIAN_POINT('',(-7.39592319198274,4.5599460519893,-1.24511852975822));
#145920=CARTESIAN_POINT('',(-7.29047144671895,4.559946050062,-1.10680916809047));
#145921=CARTESIAN_POINT('',(-7.28163200963444,4.46959751863828,-1.79661773201414));
#145922=CARTESIAN_POINT('Origin',(0.189981499374506,4.55357071573259,0.0330150592422844));
#145923=CARTESIAN_POINT('Ctrl Pts',(-7.03941442542484,4.43060907878943,
-1.73468860428));
#145924=CARTESIAN_POINT('Ctrl Pts',(-7.07971718183903,4.43741364855799,
-1.74504344049464));
#145925=CARTESIAN_POINT('Ctrl Pts',(-7.12007452219301,4.44406034770598,
-1.75538519133325));
#145926=CARTESIAN_POINT('Ctrl Pts',(-7.20080148942712,4.45704674579273,
-1.77602336632061));
#145927=CARTESIAN_POINT('Ctrl Pts',(-7.24121439563693,4.46339340288238,
-1.78633085064295));
#145928=CARTESIAN_POINT('Ctrl Pts',(-7.28163200993332,4.46959751863633,
-1.79661773084098));
#145929=CARTESIAN_POINT('Ctrl Pts',(-7.124328633,4.559946053,-2.343915853));
#145930=CARTESIAN_POINT('Ctrl Pts',(-7.253007281,4.494288122,-1.9527973));
#145931=CARTESIAN_POINT('Ctrl Pts',(-7.33809761200001,4.429844992,-1.549943043));
#145932=CARTESIAN_POINT('Ctrl Pts',(-6.808839097,4.559946053,-2.49042369));
#145933=CARTESIAN_POINT('Ctrl Pts',(-6.945560879,4.494288122,-2.116625199));
#145934=CARTESIAN_POINT('Ctrl Pts',(-7.040542002,4.429844992,-1.730106449));
#145935=CARTESIAN_POINT('',(-7.12432863437108,4.55994605320498,-2.34391584736187));
#145936=CARTESIAN_POINT('Origin',(0.169190777109376,4.69632600021766,0.0785996732235539));
#145937=CARTESIAN_POINT('',(-6.9665838656709,4.5599460533341,-2.41716976956639));
#145938=CARTESIAN_POINT('Origin',(-2.4156024402977E-13,4.65175593299956,
-9.37834879199961E-14));
#145939=CARTESIAN_POINT('',(-7.2807509534696,4.65066950026038,-1.80018486640627));
#145940=CARTESIAN_POINT('Origin',(0.183968884340725,4.69641606226494,0.0530635059363921));
#145941=CARTESIAN_POINT('Origin',(0.182620780952183,4.55357342913923,0.0611690349759017));
#145942=CARTESIAN_POINT('Ctrl Pts',(-6.61164752302496,4.429837254,-3.54173391420354));
#145943=CARTESIAN_POINT('Ctrl Pts',(-6.80356523950422,4.494719353,-3.18346524451117));
#145944=CARTESIAN_POINT('Ctrl Pts',(-6.95564551170398,4.559946053,-2.80655618233065));
#145945=CARTESIAN_POINT('Ctrl Pts',(-6.96087266440988,4.56218796062203,
-2.79360143681524));
#145946=CARTESIAN_POINT('Ctrl Pts',(-6.96609981711593,4.56442986824406,
-2.78064669129977));
#145947=CARTESIAN_POINT('Ctrl Pts',(-6.499861271,4.429837254,-3.211588931));
#145948=CARTESIAN_POINT('Ctrl Pts',(-6.673889256,4.494719353,-2.859377679));
#145949=CARTESIAN_POINT('Ctrl Pts',(-6.808839097,4.559946053,-2.49042369));
#145950=CARTESIAN_POINT('Ctrl Pts',(-6.81347745946702,4.56218796062203,
-2.47774236839224));
#145951=CARTESIAN_POINT('Ctrl Pts',(-6.81811582193404,4.56442986824406,
-2.46506104678444));
#145952=CARTESIAN_POINT('',(-6.9553469395449,4.5599460519893,-2.80591321467404));
#145953=CARTESIAN_POINT('',(-6.8820930220054,4.559946050062,-2.64816844109368));
#145954=CARTESIAN_POINT('',(-6.72517179477355,4.46959751860838,-3.31994944661299));
#145955=CARTESIAN_POINT('Origin',(0.178442605709245,4.55357069923117,0.0730836126927792));
#145956=CARTESIAN_POINT('Ctrl Pts',(-6.50193005456292,4.43060907880055,
-3.2073985664642));
#145957=CARTESIAN_POINT('Ctrl Pts',(-6.53906455731207,4.43741364599209,
-3.2261752065072));
#145958=CARTESIAN_POINT('Ctrl Pts',(-6.57625517906146,4.44406034250236,
-3.24495080026111));
#145959=CARTESIAN_POINT('Ctrl Pts',(-6.65065821995069,4.45704674453893,
-3.28246038940059));
#145960=CARTESIAN_POINT('Ctrl Pts',(-6.68791048246892,4.46339340034464,
-3.3012144667574));
#145961=CARTESIAN_POINT('Ctrl Pts',(-6.72517179537509,4.46959751860623,
-3.31994944541732));
#145962=CARTESIAN_POINT('Ctrl Pts',(-6.453893166,4.559946053,-3.820636465));
#145963=CARTESIAN_POINT('Ctrl Pts',(-6.663642306,4.494288122,-3.466324153));
#145964=CARTESIAN_POINT('Ctrl Pts',(-6.833345029,4.429844992,-3.09118031));
#145965=CARTESIAN_POINT('Ctrl Pts',(-6.114284746,4.559946053,-3.895898106));
#145966=CARTESIAN_POINT('Ctrl Pts',(-6.328165675,4.494288122,-3.560229957));
#145967=CARTESIAN_POINT('Ctrl Pts',(-6.504016297,4.429844992,-3.203165935));
#145968=CARTESIAN_POINT('',(-6.45389316855401,4.55994605320497,-3.82063645978579));
#145969=CARTESIAN_POINT('Origin',(0.14833844391806,4.69632602799791,0.113133000893504));
#145970=CARTESIAN_POINT('',(-6.28408895707088,4.5599460533341,-3.85826728375583));
#145971=CARTESIAN_POINT('Origin',(-6.44883452194378E-13,4.65175593299956,
-3.41523684332934E-13));
#145972=CARTESIAN_POINT('',(-6.72354450891252,4.65066950025556,-3.32324378227745));
#145973=CARTESIAN_POINT('Origin',(0.168260763809682,4.69641606952771,0.0913708077746189));
#145974=CARTESIAN_POINT('Origin',(0.165201840700276,4.55357343561515,0.0989970932106476));
#145975=CARTESIAN_POINT('Ctrl Pts',(-5.69570277961821,4.429837254,-4.88023892213889));
#145976=CARTESIAN_POINT('Ctrl Pts',(-5.96015074082042,4.494719353,-4.57160301106179));
#145977=CARTESIAN_POINT('Ctrl Pts',(-6.18969976651714,4.559946053,-4.23619863575322));
#145978=CARTESIAN_POINT('Ctrl Pts',(-6.19758959864021,4.56218796063338,
-4.22467044822775));
#145979=CARTESIAN_POINT('Ctrl Pts',(-6.20547943076325,4.56442986826676,
-4.21314226070228));
#145980=CARTESIAN_POINT('Ctrl Pts',(-5.65750144,4.429837254,-4.533781805));
#145981=CARTESIAN_POINT('Ctrl Pts',(-5.903175755,4.494719353,-4.227215929));
#145982=CARTESIAN_POINT('Ctrl Pts',(-6.114284746,4.559946053,-3.895898106));
#145983=CARTESIAN_POINT('Ctrl Pts',(-6.12154077548477,4.56218796063338,
-3.88451037740953));
#145984=CARTESIAN_POINT('Ctrl Pts',(-6.12879680496953,4.56442986826676,
-3.87312264881898));
#145985=CARTESIAN_POINT('',(-6.18954639384237,4.55994605198929,-4.23550651616055));
#145986=CARTESIAN_POINT('',(-6.15191557598764,4.55994605006201,-4.06570230088745));
#145987=CARTESIAN_POINT('',(-5.85425002175765,4.46959751860776,-4.68804401444961));
#145988=CARTESIAN_POINT('Origin',(0.1585595244886,4.55357068783892,0.109734557183265));
#145989=CARTESIAN_POINT('Ctrl Pts',(-5.66042266109747,4.43060907880261,
-4.53013413644781));
#145990=CARTESIAN_POINT('Ctrl Pts',(-5.69265255780897,4.43741364610902,
-4.55645460991157));
#145991=CARTESIAN_POINT('Ctrl Pts',(-5.72493748651506,4.44406034273362,
-4.58278612547743));
#145992=CARTESIAN_POINT('Ctrl Pts',(-5.78953757171177,4.45704674451748,
-4.63541321458658));
#145993=CARTESIAN_POINT('Ctrl Pts',(-5.82188732474689,4.46339340029751,
-4.66173696713832));
#145994=CARTESIAN_POINT('Ctrl Pts',(-5.85425002260382,4.4695975186056,-4.68804401340916));
#145995=CARTESIAN_POINT('Ctrl Pts',(-5.481680828,4.559946053,-5.11870836300001));
#145996=CARTESIAN_POINT('Ctrl Pts',(-5.762692823,4.494288122,-4.81776954));
#145997=CARTESIAN_POINT('Ctrl Pts',(-6.00907282800001,4.429844992,-4.487877421));
#145998=CARTESIAN_POINT('Ctrl Pts',(-5.133833235,4.559946053,-5.119204656));
#145999=CARTESIAN_POINT('Ctrl Pts',(-5.414872477,4.494288122,-4.83736232));
#146000=CARTESIAN_POINT('Ctrl Pts',(-5.663370019,4.429844992,-4.526448942));
#146001=CARTESIAN_POINT('',(-5.48168083158206,4.55994605320496,-5.11870835847377));
#146002=CARTESIAN_POINT('Origin',(0.120550304306342,4.69632602559465,0.142376541637629));
#146003=CARTESIAN_POINT('',(-5.30775703292076,4.55994605333409,-5.11895650802684));
#146004=CARTESIAN_POINT('Origin',(5.39065320159793E-13,4.65175593300022,
3.36970035208495E-13));
#146005=CARTESIAN_POINT('',(-5.85195259583039,4.65066950024768,-4.69091151220871));
#146006=CARTESIAN_POINT('Origin',(0.144684649761533,4.69641602837144,0.125405500661173));
#146007=CARTESIAN_POINT('Origin',(0.140058261803594,4.55357342842715,0.132196269379788));
#146008=CARTESIAN_POINT('Ctrl Pts',(-4.51343330429278,4.429837254,-5.99054938131607));
#146009=CARTESIAN_POINT('Ctrl Pts',(-4.83804621685821,4.494719353,-5.7459777007136));
#146010=CARTESIAN_POINT('Ctrl Pts',(-5.13433054042936,4.559946053,-5.46776114990866));
#146011=CARTESIAN_POINT('Ctrl Pts',(-5.14451413247666,4.56218796068985,
-5.45819856549634));
#146012=CARTESIAN_POINT('Ctrl Pts',(-5.15469772452387,4.56442986837969,
-5.44863598108387));
#146013=CARTESIAN_POINT('Ctrl Pts',(-4.55060313,4.429837254,-5.643980081));
#146014=CARTESIAN_POINT('Ctrl Pts',(-4.856436318,4.494719353,-5.39739426));
#146015=CARTESIAN_POINT('Ctrl Pts',(-5.133833235,4.559946053,-5.119204656));
#146016=CARTESIAN_POINT('Ctrl Pts',(-5.14336764776899,4.56218796068985,
-5.10964299777661));
#146017=CARTESIAN_POINT('Ctrl Pts',(-5.15290206053796,4.56442986837969,
-5.10008133955327));
#146018=CARTESIAN_POINT('',(-5.13432953879072,4.5599460519893,-5.46705224104394));
#146019=CARTESIAN_POINT('',(-5.13408139500295,4.559946050062,-5.29312843988776));
#146020=CARTESIAN_POINT('',(-4.70959002385817,4.46959751859485,-5.83693085503733));
#146021=CARTESIAN_POINT('Origin',(0.131263059169311,4.5535707426612,0.141254927737274));
#146022=CARTESIAN_POINT('Ctrl Pts',(-4.5542401956578,4.43060907883754,-5.64104566896126));
#146023=CARTESIAN_POINT('Ctrl Pts',(-4.58005846073345,4.43741364857084,
-5.67367927117784));
#146024=CARTESIAN_POINT('Ctrl Pts',(-4.60592809864141,4.44406034769415,
-5.70633548909699));
#146025=CARTESIAN_POINT('Ctrl Pts',(-4.65770458035733,4.45704674427068,
-5.77161926884762));
#146026=CARTESIAN_POINT('Ctrl Pts',(-4.68363918425479,4.46339339978764,
-5.80428182597552));
#146027=CARTESIAN_POINT('Ctrl Pts',(-4.70959002492802,4.46959751859253,
-5.83693085418741));
#146028=CARTESIAN_POINT('Ctrl Pts',(-4.253151186,4.559946053,-6.177435146));
#146029=CARTESIAN_POINT('Ctrl Pts',(-4.592286229,4.494288122,-5.943941379));
#146030=CARTESIAN_POINT('Ctrl Pts',(-4.903823059,4.429844992,-5.674726372));
#146031=CARTESIAN_POINT('Ctrl Pts',(-3.913329389,4.559946053,-6.103142887));
#146032=CARTESIAN_POINT('Ctrl Pts',(-4.24838586,4.494288122,-5.888304997));
#146033=CARTESIAN_POINT('Ctrl Pts',(-4.557910854,4.429844992,-5.638080227));
#146034=CARTESIAN_POINT('',(-4.2531511905143,4.55994605320497,-6.17743514233839));
#146035=CARTESIAN_POINT('Origin',(0.0871248502457178,4.6963259767227,0.16496220389796));
#146036=CARTESIAN_POINT('',(-4.08324028920423,4.55994605333409,-6.14028901536671));
#146037=CARTESIAN_POINT('Origin',(-2.28549817959944E-13,4.65175593300044,
-3.36102673470506E-13));
#146038=CARTESIAN_POINT('',(-4.70672988344605,4.65066950023002,-5.83923743366366));
#146039=CARTESIAN_POINT('Origin',(0.114343684782978,4.69641603551555,0.153576699705674));
#146040=CARTESIAN_POINT('Origin',(0.10836526325891,4.55357338805645,0.159213713368659));
#146041=CARTESIAN_POINT('Ctrl Pts',(-3.12012070376652,4.429837254,-6.820748410091));
#146042=CARTESIAN_POINT('Ctrl Pts',(-3.48972002876384,4.494719353,-6.65167686041999));
#146043=CARTESIAN_POINT('Ctrl Pts',(-3.8388857240293,4.559946053,-6.44365722867717));
#146044=CARTESIAN_POINT('Ctrl Pts',(-3.85088690238008,4.56218796069755,
-6.43650738338921));
#146045=CARTESIAN_POINT('Ctrl Pts',(-3.86288808073079,4.5644298683951,-6.42935753810134));
#146046=CARTESIAN_POINT('Ctrl Pts',(-3.230923675,4.429837254,-6.490272121));
#146047=CARTESIAN_POINT('Ctrl Pts',(-3.582615315,4.494719353,-6.315196435));
#146048=CARTESIAN_POINT('Ctrl Pts',(-3.913329389,4.559946053,-6.10314288700001));
#146049=CARTESIAN_POINT('Ctrl Pts',(-3.92469636645225,4.56218796069755,
-6.09585439192739));
#146050=CARTESIAN_POINT('Ctrl Pts',(-3.93606334390451,4.56442986839511,
-6.08856589685482));
#146051=CARTESIAN_POINT('',(-3.83903713795967,4.55994605198798,-6.44296468060183));
#146052=CARTESIAN_POINT('',(-3.87618327441021,4.559946050062,-6.27305377597788));
#146053=CARTESIAN_POINT('',(-3.34471483088038,4.46959751863189,-6.71288929577102));
#146054=CARTESIAN_POINT('Origin',(0.0978285057877903,4.55357072668722,0.166170023237531));
#146055=CARTESIAN_POINT('Ctrl Pts',(-3.23510652003408,4.43060907887121,
-6.48818817562549));
#146056=CARTESIAN_POINT('Ctrl Pts',(-3.25330590093075,4.43741364578292,
-6.52560897073948));
#146057=CARTESIAN_POINT('Ctrl Pts',(-3.27155059093039,4.44406034200068,
-6.56306289439335));
#146058=CARTESIAN_POINT('Ctrl Pts',(-3.30808250473215,4.45704674581605,
-6.63795083042892));
#146059=CARTESIAN_POINT('Ctrl Pts',(-3.32638929257642,4.46339340290249,
-6.67542493817343));
#146060=CARTESIAN_POINT('Ctrl Pts',(-3.34471483196707,4.46959751862983,
-6.71288929523981));
#146061=CARTESIAN_POINT('Ctrl Pts',(-2.825748922,4.559946053,-6.947311928));
#146062=CARTESIAN_POINT('Ctrl Pts',(-3.207149434,4.494288122,-6.792181124));
#146063=CARTESIAN_POINT('Ctrl Pts',(-3.569275975,4.429844992,-6.596231425));
#146064=CARTESIAN_POINT('Ctrl Pts',(-2.509842609,4.559946053,-6.801704939));
#146065=CARTESIAN_POINT('Ctrl Pts',(-2.883249442,4.494288122,-6.663917077));
#146066=CARTESIAN_POINT('Ctrl Pts',(-3.239328843,4.429844992,-6.486081147));
#146067=CARTESIAN_POINT('',(-2.82574892719149,4.55994605320497,-6.94731192539453));
#146068=CARTESIAN_POINT('Origin',(0.0496260836622386,4.69632598118124,0.179835099128474));
#146069=CARTESIAN_POINT('',(-2.66779576740801,4.55994605333409,-6.87450843275956));
#146070=CARTESIAN_POINT('Origin',(-2.26381413614973E-13,4.65175593299933,
-4.36282954208167E-13));
#146071=CARTESIAN_POINT('',(-3.34142571261755,4.65066950023686,-6.71452710230812));
#146072=CARTESIAN_POINT('Origin',(0.0786558871157211,4.6964160462467,0.174566560371842));
#146073=CARTESIAN_POINT('Origin',(0.0716056046167174,4.55357341172417,0.178786917787327));
#146074=CARTESIAN_POINT('Ctrl Pts',(-1.58091472753821,4.429837254,-7.33201682376214));
#146075=CARTESIAN_POINT('Ctrl Pts',(-1.97821841095581,4.494719353,-7.24635100303436));
#146076=CARTESIAN_POINT('Ctrl Pts',(-2.36393887818029,4.559946053,-7.11825505773228));
#146077=CARTESIAN_POINT('Ctrl Pts',(-2.37719648110749,4.56218796070865,
-7.11385227041945));
#146078=CARTESIAN_POINT('Ctrl Pts',(-2.39045408403462,4.56442986841731,
-7.1094494831066));
#146079=CARTESIAN_POINT('Ctrl Pts',(-1.76016982,4.429837254,-7.03308625));
#146080=CARTESIAN_POINT('Ctrl Pts',(-2.141275202,4.494719353,-6.93770704300001));
#146081=CARTESIAN_POINT('Ctrl Pts',(-2.509842609,4.559946053,-6.801704939));
#146082=CARTESIAN_POINT('Ctrl Pts',(-2.52251064388306,4.56218796070865,
-6.79703040900924));
#146083=CARTESIAN_POINT('Ctrl Pts',(-2.53517867876617,4.56442986841731,
-6.79235587901837));
#146084=CARTESIAN_POINT('',(-2.36423563221371,4.55994605198929,-7.11761124890048));
#146085=CARTESIAN_POINT('',(-2.4370391315969,4.559946050062,-6.95965808951324));
#146086=CARTESIAN_POINT('',(-1.82344448969034,4.46959751861481,-7.27496049448271));
#146087=CARTESIAN_POINT('Origin',(0.0598196423639694,4.55357070591541,0.183315160238214));
#146088=CARTESIAN_POINT('Ctrl Pts',(-1.76470285870704,4.43060907887909,
-7.0319502148614));
#146089=CARTESIAN_POINT('Ctrl Pts',(-1.77443238755811,4.43741364865479,
-7.07240847849282));
#146090=CARTESIAN_POINT('Ctrl Pts',(-1.78419904508117,4.44406034779995,
-7.11290883835043));
#146091=CARTESIAN_POINT('Ctrl Pts',(-1.80377816159113,4.45704674566609,
-7.19389918059214));
#146092=CARTESIAN_POINT('Ctrl Pts',(-1.81360112122397,4.46339340257863,
-7.2344325816342));
#146093=CARTESIAN_POINT('Ctrl Pts',(-1.82344449088131,4.46959751861249,
-7.2749604941938));
#146094=CARTESIAN_POINT('Ctrl Pts',(-1.266217779,4.559946053,-7.392340126));
#146095=CARTESIAN_POINT('Ctrl Pts',(-1.672049896,4.494288122,-7.32282603));
#146096=CARTESIAN_POINT('Ctrl Pts',(-2.067833513,4.429844992,-7.209304028));
#146097=CARTESIAN_POINT('Ctrl Pts',(-0.988998379000001,4.559946053,-7.182226828));
#146098=CARTESIAN_POINT('Ctrl Pts',(-1.383295485,4.494288122,-7.127931801));
#146099=CARTESIAN_POINT('Ctrl Pts',(-1.769279415,4.429844992,-7.030800122));
#146100=CARTESIAN_POINT('',(-1.26621778460305,4.55994605320497,-7.39234012456675));
#146101=CARTESIAN_POINT('Origin',(0.00980662171595426,4.69632599299584,
0.186298799465782));
#146102=CARTESIAN_POINT('',(-1.12760808102257,4.55994605333409,-7.28728347668704));
#146103=CARTESIAN_POINT('Origin',(1.57968256531138E-13,4.65175593299933,
9.04224611852911E-13));
#146104=CARTESIAN_POINT('',(-1.81988018947367,4.65066950021795,-7.27585294622769));
#146105=CARTESIAN_POINT('Origin',(0.0392903191542862,4.69641605117287,0.187394070549128));
#146106=CARTESIAN_POINT('Origin',(0.0314976175481438,4.55357338755637,0.19000014053232));
#146107=CARTESIAN_POINT('Ctrl Pts',(0.032213064727789,4.429837254,-7.50044828046727));
#146108=CARTESIAN_POINT('Ctrl Pts',(-0.374217498669831,4.494719353,-7.50219382594903));
#146109=CARTESIAN_POINT('Ctrl Pts',(-0.778456877615826,4.559946053,-7.46001119121922));
#146110=CARTESIAN_POINT('Ctrl Pts',(-0.792350993964793,4.56218796065686,
-7.45856133139514));
#146111=CARTESIAN_POINT('Ctrl Pts',(-0.806245110313756,4.56442986831374,
-7.45711147157109));
#146112=CARTESIAN_POINT('Ctrl Pts',(-0.207112381,4.429837254,-7.247041083));
#146113=CARTESIAN_POINT('Ctrl Pts',(-0.599811441,4.494719353,-7.23581818000001));
#146114=CARTESIAN_POINT('Ctrl Pts',(-0.988998379000001,4.559946053,-7.182226828));
#146115=CARTESIAN_POINT('Ctrl Pts',(-1.00237512772787,4.56218796065686,
-7.18038483902323));
#146116=CARTESIAN_POINT('Ctrl Pts',(-1.01575187645574,4.56442986831373,
-7.1785428500466));
#146117=CARTESIAN_POINT('',(-0.883941747984119,4.559946050062,-7.32083652582854));
#146118=CARTESIAN_POINT('Ctrl Pts',(-0.211783653451348,4.43060907881915,
-7.246906076998));
#146119=CARTESIAN_POINT('Ctrl Pts',(-0.212588380606481,4.43741364861059,
-7.28851000997835));
#146120=CARTESIAN_POINT('Ctrl Pts',(-0.213420318918682,4.44406034776933,
-7.33016303659061));
#146121=CARTESIAN_POINT('Ctrl Pts',(-0.215131156787447,4.45704674389096,
-7.41346878958388));
#146122=CARTESIAN_POINT('Ctrl Pts',(-0.216010977713216,4.46339339902968,
-7.45516617567207));
#146123=CARTESIAN_POINT('Ctrl Pts',(-0.216911912140415,4.46959751859056,
-7.49686262530735));
#146124=CARTESIAN_POINT('Ctrl Pts',(0.3525203,4.559946053,-7.49171071500001));
#146125=CARTESIAN_POINT('Ctrl Pts',(-0.058767163,4.494288122,-7.51106372900001));
#146126=CARTESIAN_POINT('Ctrl Pts',(-0.469701454,4.429844992,-7.485277586));
#146127=CARTESIAN_POINT('Ctrl Pts',(0.578090317,4.559946053,-7.226915773));
#146128=CARTESIAN_POINT('Ctrl Pts',(0.181339832,4.494288122,-7.258652356));
#146129=CARTESIAN_POINT('Ctrl Pts',(-0.216500448,4.429844992,-7.246766697));
#146130=CARTESIAN_POINT('',(0.465305306457437,4.55994605333409,-7.35931324412915));
#146131=CARTESIAN_POINT('Ctrl Pts',(1.64383461034797,4.429837254,-7.31816711034348));
#146132=CARTESIAN_POINT('Ctrl Pts',(1.2472814078235,4.494719353,-7.4072424037483));
#146133=CARTESIAN_POINT('Ctrl Pts',(0.843424901631317,4.559946053,-7.45294549263354));
#146134=CARTESIAN_POINT('Ctrl Pts',(0.829543944671895,4.56218796071086,
-7.45451635406576));
#146135=CARTESIAN_POINT('Ctrl Pts',(0.81566298771247,4.56442986842169,-7.45608721549797));
#146136=CARTESIAN_POINT('Ctrl Pts',(1.355629403,4.429837254,-7.12213233));
#146137=CARTESIAN_POINT('Ctrl Pts',(0.969698837,4.494719353,-7.195590502));
#146138=CARTESIAN_POINT('Ctrl Pts',(0.578090316999999,4.559946053,-7.226915773));
#146139=CARTESIAN_POINT('Ctrl Pts',(0.564630335725178,4.56218796071085,
-7.22799245427621));
#146140=CARTESIAN_POINT('Ctrl Pts',(0.551170354450339,4.56442986842171,
-7.22906913555243));
#146141=CARTESIAN_POINT('',(0.842885249818538,4.55994605198798,-7.45248579171881));
#146142=CARTESIAN_POINT('',(0.71048776996954,4.559946050062,-7.33970078274536));
#146143=CARTESIAN_POINT('',(1.39976322824942,4.46959751862171,-7.36821979213623));
#146144=CARTESIAN_POINT('Origin',(-0.0226811960224843,4.55357073441964,
0.191489976544781));
#146145=CARTESIAN_POINT('Ctrl Pts',(1.35103831954934,4.43060907872896,-7.12300466507705));
#146146=CARTESIAN_POINT('Ctrl Pts',(1.35919602247054,4.43741364847978,-7.1638089133596));
#146147=CARTESIAN_POINT('Ctrl Pts',(1.36733770405226,4.44406034762445,-7.204666957255));
#146148=CARTESIAN_POINT('Ctrl Pts',(1.38357514172299,4.4570467456653,-7.28639285949099));
#146149=CARTESIAN_POINT('Ctrl Pts',(1.39167959854772,4.46339340262745,-7.3273045318516));
#146150=CARTESIAN_POINT('Ctrl Pts',(1.39976322704982,4.4695975186195,-7.36821979237357));
#146151=CARTESIAN_POINT('Ctrl Pts',(1.954774922,4.559946053,-7.240777238));
#146152=CARTESIAN_POINT('Ctrl Pts',(1.557263457,4.494288122,-7.348092436));
#146153=CARTESIAN_POINT('Ctrl Pts',(1.150393323,4.429844992,-7.411247884));
#146154=CARTESIAN_POINT('Ctrl Pts',(2.118148151,4.559946053,-6.933682168));
#146155=CARTESIAN_POINT('Ctrl Pts',(1.7374959,4.494288122,-7.049966394));
#146156=CARTESIAN_POINT('Ctrl Pts',(1.346401839,4.429844992,-7.123882515));
#146157=CARTESIAN_POINT('',(1.95477491632479,4.55994605320496,-7.2407772390435));
#146158=CARTESIAN_POINT('Origin',(-0.0693245532869646,4.69632599728337,
0.173197784951975));
#146159=CARTESIAN_POINT('',(2.03646153453295,4.55994605333409,-7.08722970356522));
#146160=CARTESIAN_POINT('Origin',(1.8550699171227E-13,4.65175593299889,
-4.97431956736349E-13));
#146161=CARTESIAN_POINT('',(1.4033728301242,4.65066950020261,-7.36753314876966));
#146162=CARTESIAN_POINT('Origin',(-0.043025793661835,4.69641605817414,0.186571819988643));
#146163=CARTESIAN_POINT('Origin',(-0.0511925248948061,4.5535734263607,0.185665015335107));
#146164=CARTESIAN_POINT('Ctrl Pts',(3.17859227584221,4.429837254,-6.79369658045487));
#146165=CARTESIAN_POINT('Ctrl Pts',(2.81045882140123,4.494719353,-6.96593655960307));
#146166=CARTESIAN_POINT('Ctrl Pts',(2.42586906973883,4.559946053,-7.09738834678343));
#146167=CARTESIAN_POINT('Ctrl Pts',(2.41265033056979,4.56218796072225,-7.10190647780624));
#146168=CARTESIAN_POINT('Ctrl Pts',(2.39943159140081,4.56442986844461,-7.1064246088291));
#146169=CARTESIAN_POINT('Ctrl Pts',(2.854983464,4.429837254,-6.664200584));
#146170=CARTESIAN_POINT('Ctrl Pts',(2.493867074,4.494719353,-6.818905009));
#146171=CARTESIAN_POINT('Ctrl Pts',(2.118148151,4.559946053,-6.933682168));
#146172=CARTESIAN_POINT('Ctrl Pts',(2.10523431119399,4.56218796072225,-6.93762717516887));
#146173=CARTESIAN_POINT('Ctrl Pts',(2.09232047138791,4.56442986844461,-6.94157218233777));
#146174=CARTESIAN_POINT('',(2.42524320939363,4.55994605198931,-7.09705540292355));
#146175=CARTESIAN_POINT('',(2.27169566876629,4.55994605006201,-7.01536878858058));
#146176=CARTESIAN_POINT('',(2.95098699365994,4.46959751860328,-6.8950471905747));
#146177=CARTESIAN_POINT('Origin',(-0.0633156292957315,4.55357075974186,
0.182137308187349));
#146178=CARTESIAN_POINT('Ctrl Pts',(2.85068724327673,4.43060907887691,-6.66603947209202));
#146179=CARTESIAN_POINT('Ctrl Pts',(2.86742593071851,4.43741364860001,-6.70413607486207));
#146180=CARTESIAN_POINT('Ctrl Pts',(2.88416053584548,4.44406034771747,-6.74228865957532));
#146181=CARTESIAN_POINT('Ctrl Pts',(2.91758700058967,4.45704674433851,-6.81861327845623));
#146182=CARTESIAN_POINT('Ctrl Pts',(2.934296775964,4.46339339992011,-6.85682623120992));
#146183=CARTESIAN_POINT('Ctrl Pts',(2.95098699241346,4.46959751860108,-6.89504719111936));
#146184=CARTESIAN_POINT('Ctrl Pts',(3.465626441,4.559946053,-6.651273064));
#146185=CARTESIAN_POINT('Ctrl Pts',(3.100478168,4.494288122,-6.841532507));
#146186=CARTESIAN_POINT('Ctrl Pts',(2.716696986,4.429844992,-6.99067646800001));
#146187=CARTESIAN_POINT('Ctrl Pts',(3.559163733,4.559946053,-6.316237292));
#146188=CARTESIAN_POINT('Ctrl Pts',(3.212408591,4.494288122,-6.511631839));
#146189=CARTESIAN_POINT('Ctrl Pts',(2.846347872,4.429844992,-6.667893505));
#146190=CARTESIAN_POINT('',(3.4656264356673,4.55994605320497,-6.6512730662547));
#146191=CARTESIAN_POINT('Origin',(-0.104936233793004,4.69632599638227,0.154245883139481));
#146192=CARTESIAN_POINT('',(3.51239508520045,4.55994605333409,-6.48375517897486));
#146193=CARTESIAN_POINT('Origin',(3.42391046070922E-13,4.65175593300022,
-6.35342473076506E-13));
#146194=CARTESIAN_POINT('',(2.95436459746952,4.65066950022452,-6.89360064298541));
#146195=CARTESIAN_POINT('Origin',(-0.0821273224085139,4.696416072966,0.17296062846072));
#146196=CARTESIAN_POINT('Origin',(-0.0899080840477851,4.55357343357433,
0.170319208237301));
#146197=CARTESIAN_POINT('Ctrl Pts',(4.56472249940374,4.429837254,-5.95156034962665));
#146198=CARTESIAN_POINT('Ctrl Pts',(4.24222230535834,4.494719353,-6.19891126290004));
#146199=CARTESIAN_POINT('Ctrl Pts',(3.89488229582998,4.559946053,-6.40996520963038));
#146200=CARTESIAN_POINT('Ctrl Pts',(3.88294386901984,4.56218796053342,-6.41721934686453));
#146201=CARTESIAN_POINT('Ctrl Pts',(3.87100544220972,4.56442986806685,-6.4244734840987));
#146202=CARTESIAN_POINT('Ctrl Pts',(4.22084167,4.429837254,-5.894658226));
#146203=CARTESIAN_POINT('Ctrl Pts',(3.90142486,4.494719353,-6.123375096));
#146204=CARTESIAN_POINT('Ctrl Pts',(3.559163733,4.559946053,-6.316237292));
#146205=CARTESIAN_POINT('Ctrl Pts',(3.54739987251013,4.56218796053342,-6.32286616039471));
#146206=CARTESIAN_POINT('Ctrl Pts',(3.53563601202026,4.56442986806685,-6.32949502878957));
#146207=CARTESIAN_POINT('',(3.89419949472673,4.5599460519893,-6.40977459130288));
#146208=CARTESIAN_POINT('',(3.72668160336882,4.559946050062,-6.36300594715486));
#146209=CARTESIAN_POINT('',(4.36422588747414,4.46959751861275,-6.0994698457803));
#146210=CARTESIAN_POINT('Origin',(-0.100989590094247,4.55357066949384,0.164268187817004));
#146211=CARTESIAN_POINT('Ctrl Pts',(4.21704119950273,4.43060907879527,-5.89737768206882));
#146212=CARTESIAN_POINT('Ctrl Pts',(4.24157817912082,4.43741364575208,-5.9309852706859));
#146213=CARTESIAN_POINT('Ctrl Pts',(4.26612320506791,4.44406034201518,-5.96464840814477));
#146214=CARTESIAN_POINT('Ctrl Pts',(4.31517573742189,4.45704674471917,-6.03200292935783));
#146215=CARTESIAN_POINT('Ctrl Pts',(4.33970950448323,4.46339340071594,-6.06573037899577));
#146216=CARTESIAN_POINT('Ctrl Pts',(4.36422588640664,4.46959751861062,-6.09946984655637));
#146217=CARTESIAN_POINT('Ctrl Pts',(4.814429119,4.559946053,-5.75076275500001));
#146218=CARTESIAN_POINT('Ctrl Pts',(4.498717966,4.494288122,-6.015070122));
#146219=CARTESIAN_POINT('Ctrl Pts',(4.155970918,4.429844992,-6.24322879));
#146220=CARTESIAN_POINT('Ctrl Pts',(4.833756773,4.559946053,-5.403452179));
#146221=CARTESIAN_POINT('Ctrl Pts',(4.537112626,4.494288122,-5.668820616));
#146222=CARTESIAN_POINT('Ctrl Pts',(4.213201843,4.429844992,-5.900121205));
#146223=CARTESIAN_POINT('',(4.81442911428777,4.55994605320496,-5.75076275832939));
#146224=CARTESIAN_POINT('Origin',(-0.135641291056955,4.69632602118281,0.128081646994533));
#146225=CARTESIAN_POINT('',(4.82409294445209,4.55994605333409,-5.57710746833892));
#146226=CARTESIAN_POINT('Origin',(6.16911036144252E-13,4.65175593299889,
-7.42461647718073E-13));
#146227=CARTESIAN_POINT('',(4.36721355993797,4.6506695002325,-6.09733103257101));
#146228=CARTESIAN_POINT('Origin',(-0.117388650771652,4.69641607718384,0.151261954901537));
#146229=CARTESIAN_POINT('Origin',(-0.124419609548201,4.55357341342025,0.147009578589056));
#146230=CARTESIAN_POINT('Ctrl Pts',(5.73741137231444,4.429837254,-4.83113577047493));
#146231=CARTESIAN_POINT('Ctrl Pts',(5.47562418788991,4.494719353,-5.14203176680074));
#146232=CARTESIAN_POINT('Ctrl Pts',(5.18177515549747,4.559946053,-5.4228192230677));
#146233=CARTESIAN_POINT('Ctrl Pts',(5.17167526673081,4.56218796072131,-5.43247017223801));
#146234=CARTESIAN_POINT('Ctrl Pts',(5.16157537796409,4.56442986844264,-5.4421211214084));
#146235=CARTESIAN_POINT('Ctrl Pts',(5.389338011,4.429837254,-4.8494882));
#146236=CARTESIAN_POINT('Ctrl Pts',(5.12655635500001,4.494719353,-5.14152297));
#146237=CARTESIAN_POINT('Ctrl Pts',(4.833756773,4.559946053,-5.403452179));
#146238=CARTESIAN_POINT('Ctrl Pts',(4.8236929549059,4.56218796072131,-5.41245495111771));
#146239=CARTESIAN_POINT('Ctrl Pts',(4.81362913681171,4.56442986844262,-5.42145772323545));
#146240=CARTESIAN_POINT('',(5.18106734053446,4.5599460519893,-5.42277984334128));
#146241=CARTESIAN_POINT('',(5.00741204770229,4.559946050062,-5.41311601880107));
#146242=CARTESIAN_POINT('',(5.57339842935792,4.46959751862925,-5.01868807039529));
#146243=CARTESIAN_POINT('Origin',(-0.133941263718198,4.55357075941831,0.138717887482821));
#146244=CARTESIAN_POINT('Ctrl Pts',(5.38621099636352,4.43060907884818,-4.85296106573666));
#146245=CARTESIAN_POINT('Ctrl Pts',(5.4173989660286,4.43741364861691,-4.88050821382468));
#146246=CARTESIAN_POINT('Ctrl Pts',(5.44860673686744,4.44406034776174,-4.90810788376682));
#146247=CARTESIAN_POINT('Ctrl Pts',(5.51099165518376,4.45704674542827,-4.96334282803468));
#146248=CARTESIAN_POINT('Ctrl Pts',(5.54220224478526,4.46339340212321,-4.99100771729885));
#146249=CARTESIAN_POINT('Ctrl Pts',(5.57339842852905,4.46959751862724,-5.01868807132989));
#146250=CARTESIAN_POINT('Ctrl Pts',(5.938114442,4.559946053,-4.58135317));
#146251=CARTESIAN_POINT('Ctrl Pts',(5.686602712,4.494288122,-4.907349744));
#146252=CARTESIAN_POINT('Ctrl Pts',(5.400916269,4.429844992,-5.203854673));
#146253=CARTESIAN_POINT('Ctrl Pts',(5.88232872,4.559946053,-4.238007649));
#146254=CARTESIAN_POINT('Ctrl Pts',(5.649666317,4.494288122,-4.560941642));
#146255=CARTESIAN_POINT('Ctrl Pts',(5.383051178,4.429844992,-4.856465795));
#146256=CARTESIAN_POINT('',(5.93811443809986,4.55994605320497,-4.58135317430663));
#146257=CARTESIAN_POINT('Origin',(-0.160003744045962,4.69632600536354,0.0959282054421384));
#146258=CARTESIAN_POINT('',(5.91022157977611,4.55994605333409,-4.40968041114037));
#146259=CARTESIAN_POINT('Origin',(4.79217360238593E-13,4.65175593299911,
-4.35849273339173E-13));
#146260=CARTESIAN_POINT('',(5.57585647005731,4.65066950023898,-5.01595699988356));
#146261=CARTESIAN_POINT('Origin',(-0.147161144742348,4.69641605607194,0.122490578288943));
#146262=CARTESIAN_POINT('Origin',(-0.153113438793119,4.55357339955597,0.116826006957307));
#146263=CARTESIAN_POINT('Ctrl Pts',(6.6418252657073,4.429837254,-3.48481265260984));
#146264=CARTESIAN_POINT('Ctrl Pts',(6.45299196933265,4.494719353,-3.84471657929806));
#146265=CARTESIAN_POINT('Ctrl Pts',(6.22637396687215,4.559946053,-4.18210823669494));
#146266=CARTESIAN_POINT('Ctrl Pts',(6.21858487707689,4.5621879606059,-4.19370472897313));
#146267=CARTESIAN_POINT('Ctrl Pts',(6.21079578728161,4.56442986821181,-4.20530122125132));
#146268=CARTESIAN_POINT('Ctrl Pts',(6.305834896,4.429837254,-3.577561496));
#146269=CARTESIAN_POINT('Ctrl Pts',(6.111975772,4.494719353,-3.919258944));
#146270=CARTESIAN_POINT('Ctrl Pts',(5.88232872,4.559946053,-4.238007649));
#146271=CARTESIAN_POINT('Ctrl Pts',(5.87443551871049,4.5621879606059,-4.24896336416124));
#146272=CARTESIAN_POINT('Ctrl Pts',(5.8665423174211,4.56442986821181,-4.25991907932242));
#146273=CARTESIAN_POINT('',(6.22567423713373,4.55994605198798,-4.18222193475396));
#146274=CARTESIAN_POINT('',(6.05400147015755,4.559946050062,-4.21011480237209));
#146275=CARTESIAN_POINT('',(6.52196505506052,4.4695975186242,-3.70323801853134));
#146276=CARTESIAN_POINT('Origin',(-0.160629967077706,4.55357073825245,0.106681286855047));
#146277=CARTESIAN_POINT('Ctrl Pts',(6.30352755236844,4.43060907884243,-3.58162538384939));
#146278=CARTESIAN_POINT('Ctrl Pts',(6.33990818728124,4.43741364858599,-3.60182400328828));
#146279=CARTESIAN_POINT('Ctrl Pts',(6.37631945111121,4.44406034772407,-3.62206966001857));
#146280=CARTESIAN_POINT('Ctrl Pts',(6.44911973644291,4.45704674738329,-3.66260233480473));
#146281=CARTESIAN_POINT('Ctrl Pts',(6.48554778545811,4.46339340605651,-3.68291108688962));
#146282=CARTESIAN_POINT('Ctrl Pts',(6.52196505462289,4.46959751862424,-3.70323801931538));
#146283=CARTESIAN_POINT('Ctrl Pts',(6.784140134,4.559946053,-3.197724603));
#146284=CARTESIAN_POINT('Ctrl Pts',(6.608588236,4.494288122,-3.570167146));
#146285=CARTESIAN_POINT('Ctrl Pts',(6.393320778,4.429844992,-3.921154095));
#146286=CARTESIAN_POINT('Ctrl Pts',(6.655849513,4.559946053,-2.874398591));
#146287=CARTESIAN_POINT('Ctrl Pts',(6.49804789100001,4.494288122,-3.239798106));
#146288=CARTESIAN_POINT('Ctrl Pts',(6.301195022,4.429844992,-3.585727442));
#146289=CARTESIAN_POINT('',(6.78414013111715,4.55994605320497,-3.19772460804592));
#146290=CARTESIAN_POINT('Origin',(-0.176884535946686,4.69632599893794,0.0592893052161192));
#146291=CARTESIAN_POINT('',(6.71999482265735,4.55994605333409,-3.03606159886512));
#146292=CARTESIAN_POINT('Origin',(-9.61036805691151E-13,4.65175593300111,
5.07406616723216E-13));
#146293=CARTESIAN_POINT('',(6.52377852861029,4.65066950021574,-3.70004239307048));
#146294=CARTESIAN_POINT('Origin',(-0.170052142681483,4.69641603453242,0.0879913437510177));
#146295=CARTESIAN_POINT('Origin',(-0.174647839359464,4.55357340829506,0.0811797979911044));
#146296=CARTESIAN_POINT('Ctrl Pts',(7.23567479167722,4.429837254,-1.97554356808722));
#146297=CARTESIAN_POINT('Ctrl Pts',(7.12862501940249,4.494719353,-2.36762671771851));
#146298=CARTESIAN_POINT('Ctrl Pts',(6.97983445281553,4.559946053,-2.74584651831669));
#146299=CARTESIAN_POINT('Ctrl Pts',(6.97472037041059,4.56218796071268,-2.75884631576231));
#146300=CARTESIAN_POINT('Ctrl Pts',(6.96960628800551,4.56442986842537,-2.77184611320786));
#146301=CARTESIAN_POINT('Ctrl Pts',(6.92747795,4.429837254,-2.138351993));
#146302=CARTESIAN_POINT('Ctrl Pts',(6.811605995,4.494719353,-2.513734725));
#146303=CARTESIAN_POINT('Ctrl Pts',(6.655849513,4.559946053,-2.874398591));
#146304=CARTESIAN_POINT('Ctrl Pts',(6.65049600503019,4.56218796071268,-2.88679497320036));
#146305=CARTESIAN_POINT('Ctrl Pts',(6.64514249706051,4.56442986842537,-2.89919135540066));
#146306=CARTESIAN_POINT('',(6.97917552223325,4.5599460519893,-2.74610798203999));
#146307=CARTESIAN_POINT('',(6.81751251259641,4.559946050062,-2.81025329724772));
#146308=CARTESIAN_POINT('',(7.16557184357888,4.46959751864651,-2.21462867260384));
#146309=CARTESIAN_POINT('Origin',(-0.179807800035303,4.55357071148901,0.0696564124873245));
#146310=CARTESIAN_POINT('Ctrl Pts',(6.92609816677978,4.43060907880938,-2.14281687978804));
#146311=CARTESIAN_POINT('Ctrl Pts',(6.96597033268021,4.43741364583551,-2.15472250080301));
#146312=CARTESIAN_POINT('Ctrl Pts',(7.00588252093412,4.44406034215875,-2.16666747446528));
#146313=CARTESIAN_POINT('Ctrl Pts',(7.0856941328782,4.45704674670509,-2.19060261753264));
#146314=CARTESIAN_POINT('Ctrl Pts',(7.12563629114524,4.46339340470248,-2.20260560724937));
#146315=CARTESIAN_POINT('Ctrl Pts',(7.1655718432567,4.46959751864448,-2.21462867367502));
#146316=CARTESIAN_POINT('Ctrl Pts',(7.312946974,4.559946053,-1.664573988));
#146317=CARTESIAN_POINT('Ctrl Pts',(7.221563518,4.494288122,-2.0660475));
#146318=CARTESIAN_POINT('Ctrl Pts',(7.086780713,4.429844992,-2.455104709));
#146319=CARTESIAN_POINT('Ctrl Pts',(7.118150181,4.559946053,-1.376385849));
#146320=CARTESIAN_POINT('Ctrl Pts',(7.042587967,4.494288122,-1.767165211));
#146321=CARTESIAN_POINT('Ctrl Pts',(6.924701991,4.429844992,-2.147324459));
#146322=CARTESIAN_POINT('',(7.31294697226375,4.55994605320496,-1.66457399350293));
#146323=CARTESIAN_POINT('Origin',(-0.185494785591154,4.69632599477243,0.0198782917454832));
#146324=CARTESIAN_POINT('',(7.215548577078,4.55994605333409,-1.52047992050266));
#146325=CARTESIAN_POINT('Origin',(-5.92841747915074E-13,4.65175593300089,
1.16443313324943E-13));
#146326=CARTESIAN_POINT('',(7.16665595397576,4.65066950024027,-2.21111791586517));
#146327=CARTESIAN_POINT('Origin',(-0.184992040221171,4.69641607107543,0.0493779806617184));
#146328=CARTESIAN_POINT('Origin',(-0.188016192785251,4.55357343082071,0.0417378214458519));
#146329=CARTESIAN_POINT('Ctrl Pts',(7.49119220642967,4.429837254,-0.373900262486289));
#146330=CARTESIAN_POINT('Ctrl Pts',(7.47093148527094,4.494719353,-0.779829261862813));
#146331=CARTESIAN_POINT('Ctrl Pts',(7.40692563610591,4.559946053,-1.18119206711108));
#146332=CARTESIAN_POINT('Ctrl Pts',(7.40472569036061,4.56218796062276,-1.19498731250253));
#146333=CARTESIAN_POINT('Ctrl Pts',(7.40252574461543,4.56442986824553,-1.20878255789398));
#146334=CARTESIAN_POINT('Ctrl Pts',(7.225199835,4.429837254,-0.599155527));
#146335=CARTESIAN_POINT('Ctrl Pts',(7.192733093,4.494719353,-0.990671065));
#146336=CARTESIAN_POINT('Ctrl Pts',(7.118150181,4.559946053,-1.376385849));
#146337=CARTESIAN_POINT('Ctrl Pts',(7.11558669091173,4.56218796062276,-1.3896432560811));
#146338=CARTESIAN_POINT('Ctrl Pts',(7.1130232008236,4.56442986824553,-1.40290066316219));
#146339=CARTESIAN_POINT('',(7.40633831916757,4.55994605198798,-1.18158906556642));
#146340=CARTESIAN_POINT('',(7.26224424685807,4.559946050062,-1.27898747034023));
#146341=CARTESIAN_POINT('',(7.47412445643191,4.46959751866284,-0.6224657513944));
#146342=CARTESIAN_POINT('Origin',(-0.190578005963635,4.55357068622208,0.0293745193372734));
#146343=CARTESIAN_POINT('Ctrl Pts',(7.22481212866711,4.43060907879567,-0.603812640051713));
#146344=CARTESIAN_POINT('Ctrl Pts',(7.26631146379532,4.43741364611699,-0.606868577470451));
#146345=CARTESIAN_POINT('Ctrl Pts',(7.30785834553731,4.44406034275429,-0.609954343799243));
#146346=CARTESIAN_POINT('Ctrl Pts',(7.3909493589693,4.45704674800733,-0.616172759455037));
#146347=CARTESIAN_POINT('Ctrl Pts',(7.43253798891272,4.46339340732277,-0.619308743220647));
#146348=CARTESIAN_POINT('Ctrl Pts',(7.4741244563576,4.46959751866076,-0.622465752377321));
#146349=CARTESIAN_POINT('Ctrl Pts',(7.49980854000001,4.559946053,-0.053589743));
#146350=CARTESIAN_POINT('Ctrl Pts',(7.496866517,4.494288122,-0.465321769));
#146351=CARTESIAN_POINT('Ctrl Pts',(7.448870658,4.429844992,-0.874257356));
#146352=CARTESIAN_POINT('Ctrl Pts',(7.24761405700001,4.559946053,0.185985165));
#146353=CARTESIAN_POINT('Ctrl Pts',(7.257824457,4.494288122,-0.211901635));
#146354=CARTESIAN_POINT('Ctrl Pts',(7.224417591,4.429844992,-0.608514971));
#146355=CARTESIAN_POINT('',(7.49980853949836,4.55994605320497,-0.0535897487794385));
#146356=CARTESIAN_POINT('Origin',(-0.185431009943602,4.69632599840029,-0.0204623678710566));
#146357=CARTESIAN_POINT('',(7.37371129851837,4.55994605333409,0.0661977089534413));
#146358=CARTESIAN_POINT('Origin',(-7.19910242530375E-13,4.65175593300133,
5.37188295148677E-14));
#146359=CARTESIAN_POINT('',(7.47442851198713,4.65066950021361,-0.618804022598333));
#146360=CARTESIAN_POINT('Origin',(-0.191281892709029,4.69641607058777,0.00845574572821542));
#146361=CARTESIAN_POINT('Origin',(-0.192592715119703,4.55357341345698,0.000344072612098205));
#146362=CARTESIAN_POINT('Ctrl Pts',(7.39642979952305,4.429837254,1.24522620453003));
#146363=CARTESIAN_POINT('Ctrl Pts',(7.46390549869833,4.494719353,0.844432143113364));
#146364=CARTESIAN_POINT('Ctrl Pts',(7.48767721008715,4.559946053,0.438693611329296));
#146365=CARTESIAN_POINT('Ctrl Pts',(7.48849426784609,4.56218796063773,0.424747967699879));
#146366=CARTESIAN_POINT('Ctrl Pts',(7.48931132560489,4.56442986827546,0.410802324070462));
#146367=CARTESIAN_POINT('Ctrl Pts',(7.185079405,4.429837254,0.968056785));
#146368=CARTESIAN_POINT('Ctrl Pts',(7.23753598500001,4.494719353,0.578715273));
#146369=CARTESIAN_POINT('Ctrl Pts',(7.247614057,4.559946053,0.185985165));
#146370=CARTESIAN_POINT('Ctrl Pts',(7.24796045052581,4.56218796063773,0.172486634050456));
#146371=CARTESIAN_POINT('Ctrl Pts',(7.2483068440517,4.56442986827546,0.158988103100911));
#146372=CARTESIAN_POINT('',(7.48718896703819,4.55994605198842,0.438179637481071));
#146373=CARTESIAN_POINT('',(7.36740151176666,4.559946050062,0.312082388401445));
#146374=CARTESIAN_POINT('',(7.43319531657439,4.4695975186378,0.998802976821275));
#146375=CARTESIAN_POINT('Origin',(-0.192437143755373,4.55357069465802,-0.0122808925480036));
#146376=CARTESIAN_POINT('Ctrl Pts',(7.18570190538655,4.43060907888725,0.963425207556993));
#146377=CARTESIAN_POINT('Ctrl Pts',(7.22688796026147,4.43741364866101,0.96936184889719));
#146378=CARTESIAN_POINT('Ctrl Pts',(7.26812686428265,4.44406034780755,0.975279579985857));
#146379=CARTESIAN_POINT('Ctrl Pts',(7.3506119895181,4.45704674642975,0.987068653242497));
#146380=CARTESIAN_POINT('Ctrl Pts',(7.39190243297708,4.46339340412326,0.992946311536157));
#146381=CARTESIAN_POINT('Ctrl Pts',(7.43319531673589,4.46959751863569,0.998802975684803));
#146382=CARTESIAN_POINT('Ctrl Pts',(7.335987395,4.559946053,1.559900299));
#146383=CARTESIAN_POINT('Ctrl Pts',(7.421624369,4.494288122,1.157161891));
#146384=CARTESIAN_POINT('Ctrl Pts',(7.46265969,4.429844992,0.7474693));
#146385=CARTESIAN_POINT('Ctrl Pts',(7.038187555,4.559946053,1.73965972));
#146386=CARTESIAN_POINT('Ctrl Pts',(7.133693143,4.494288122,1.353270226));
#146387=CARTESIAN_POINT('Ctrl Pts',(7.186327454,4.429844992,0.958748));
#146388=CARTESIAN_POINT('',(7.3359873957426,4.55994605320496,1.55990029326451));
#146389=CARTESIAN_POINT('Origin',(-0.176697108651742,4.69632600886521,-0.0598461802887937));
#146390=CARTESIAN_POINT('',(7.1870874754579,4.55994605333409,1.64978000750524));
#146391=CARTESIAN_POINT('Origin',(1.14665221762067E-12,4.65175593300044,
9.24553402587014E-14));
#146392=CARTESIAN_POINT('',(7.43270510019513,4.65066949966071,1.00244445928465));
#146393=CARTESIAN_POINT('Origin',(-0.188627616882,4.6964160553568,-0.0328619031159097));
#146394=CARTESIAN_POINT('Origin',(-0.188164155281143,4.55357342077206,-0.0410657367178158));
#146395=CARTESIAN_POINT('Ctrl Pts',(6.95581855635293,4.429837254,2.80612727792483));
#146396=CARTESIAN_POINT('Ctrl Pts',(7.10787558655233,4.494719353,2.42920883959616));
#146397=CARTESIAN_POINT('Ctrl Pts',(7.21831331923951,4.559946053,2.03806646436907));
#146398=CARTESIAN_POINT('Ctrl Pts',(7.2221091757923,4.56218796063961,2.0246225053892));
#146399=CARTESIAN_POINT('Ctrl Pts',(7.22590503234511,4.56442986827924,2.01117854640926));
#146400=CARTESIAN_POINT('Ctrl Pts',(6.80899264800001,4.429837254,2.490003838));
#146401=CARTESIAN_POINT('Ctrl Pts',(6.94391973900001,4.494719353,2.121041529));
#146402=CARTESIAN_POINT('Ctrl Pts',(7.038187555,4.559946053,1.73965972));
#146403=CARTESIAN_POINT('Ctrl Pts',(7.04142763516438,4.56218796063961,1.72655124155173));
#146404=CARTESIAN_POINT('Ctrl Pts',(7.04466771532879,4.56442986827924,1.71344276310344));
#146405=CARTESIAN_POINT('',(7.21794698028822,4.55994605198931,2.03745954714603));
#146406=CARTESIAN_POINT('',(7.12806727013933,4.55994605006204,1.88855962198961));
#146407=CARTESIAN_POINT('',(7.04469822507141,4.46959751858764,2.5733687876881));
#146408=CARTESIAN_POINT('Origin',(-0.185298059327718,4.55357068452273,-0.0533620764200804));
#146409=CARTESIAN_POINT('Ctrl Pts',(6.81059624699143,4.43060907888844,2.48561436359437));
#146410=CARTESIAN_POINT('Ctrl Pts',(6.84954319239936,4.43741364864356,2.50026599383168));
#146411=CARTESIAN_POINT('Ctrl Pts',(6.88854581649443,4.44406034777539,2.51491051693363));
#146412=CARTESIAN_POINT('Ctrl Pts',(6.9665681668036,4.4570467436724,2.54415582565878));
#146413=CARTESIAN_POINT('Ctrl Pts',(7.00562972159081,4.46339339858634,2.55877228550805));
#146414=CARTESIAN_POINT('Ctrl Pts',(7.04469822557119,4.46959751858535,2.57336878635138));
#146415=CARTESIAN_POINT('Ctrl Pts',(6.829143632,4.559946053,3.100451136));
#146416=CARTESIAN_POINT('Ctrl Pts',(6.999355314,4.494288122,2.725537947));
#146417=CARTESIAN_POINT('Ctrl Pts',(7.127503049,4.429844992,2.334245122));
#146418=CARTESIAN_POINT('Ctrl Pts',(6.499663225,4.559946053,3.211989719));
#146419=CARTESIAN_POINT('Ctrl Pts',(6.675998265,4.494288122,2.855164676));
#146420=CARTESIAN_POINT('Ctrl Pts',(6.812212632,4.429844992,2.481180981));
#146421=CARTESIAN_POINT('',(6.82914363398258,4.55994605320497,3.10045113053292));
#146422=CARTESIAN_POINT('Origin',(-0.159700845982542,4.69632603422239,-0.0964316664364823));
#146423=CARTESIAN_POINT('',(6.66440342937601,4.55994605333409,3.15622042565031));
#146424=CARTESIAN_POINT('Origin',(1.56038376664114E-12,4.65175593300044,
6.68735899989059E-13));
#146425=CARTESIAN_POINT('',(7.04343665848191,4.6506695002242,2.57681975219685));
#146426=CARTESIAN_POINT('Origin',(-0.177153273387559,4.69641602642132,-0.0726429733137191));
#146427=CARTESIAN_POINT('Origin',(-0.174936767560196,4.55357340111542,-0.0805552607661836));
#146428=CARTESIAN_POINT('Ctrl Pts',(6.18996096719782,4.429837254,4.23581695831155));
#146429=CARTESIAN_POINT('Ctrl Pts',(6.41948931138595,4.494719353,3.90039843069377));
#146430=CARTESIAN_POINT('Ctrl Pts',(6.61142911962848,4.559946053,3.5421415952428));
#146431=CARTESIAN_POINT('Ctrl Pts',(6.61802628507903,4.56218796068781,3.52982794525585));
#146432=CARTESIAN_POINT('Ctrl Pts',(6.62462345052944,4.56442986837561,3.51751429526898));
#146433=CARTESIAN_POINT('Ctrl Pts',(6.114524963,4.429837254,3.895521079));
#146434=CARTESIAN_POINT('Ctrl Pts',(6.32561352300001,4.494719353,3.564190239));
#146435=CARTESIAN_POINT('Ctrl Pts',(6.499663225,4.559946053,3.211989719));
#146436=CARTESIAN_POINT('Ctrl Pts',(6.50564548939436,4.5621879606878,3.19988423070406));
#146437=CARTESIAN_POINT('Ctrl Pts',(6.51162775378881,4.56442986837561,3.18777874240813));
#146438=CARTESIAN_POINT('',(6.61120181473443,4.5599460519893,3.54147011535814));
#146439=CARTESIAN_POINT('',(6.55543252479518,4.559946050062,3.37672990639611));
#146440=CARTESIAN_POINT('',(6.32679887445887,4.4695975186562,4.02760673392859));
#146441=CARTESIAN_POINT('Origin',(-0.169494590604762,4.55357069773733,-0.0919480823373431));
#146442=CARTESIAN_POINT('Ctrl Pts',(6.11703467734612,4.43060907876927,3.89157895395253));
#146443=CARTESIAN_POINT('Ctrl Pts',(6.15192138417053,4.43741364598305,3.91426047067408));
#146444=CARTESIAN_POINT('Ctrl Pts',(6.18686399414782,4.44406034250939,3.93694701468659));
#146445=CARTESIAN_POINT('Ctrl Pts',(6.25677539552244,4.45704674721445,3.98228111406106));
#146446=CARTESIAN_POINT('Ctrl Pts',(6.29178162727773,4.46339340574468,4.00495294261198));
#146447=CARTESIAN_POINT('Ctrl Pts',(6.32679887503795,4.46959751865421,4.02760673303402));
#146448=CARTESIAN_POINT('Ctrl Pts',(6.002976704,4.559946053,4.496028325));
#146449=CARTESIAN_POINT('Ctrl Pts',(6.24980418500001,4.494288122,4.166470877));
#146450=CARTESIAN_POINT('Ctrl Pts',(6.459072287,4.429844992,3.811874236));
#146451=CARTESIAN_POINT('Ctrl Pts',(5.657221867,4.559946053,4.534130649));
#146452=CARTESIAN_POINT('Ctrl Pts',(5.906141128,4.494288122,4.223554798));
#146453=CARTESIAN_POINT('Ctrl Pts',(6.119566318,4.429844992,3.887596697));
#146454=CARTESIAN_POINT('',(6.00297670706392,4.55994605320496,4.49602832011822));
#146455=CARTESIAN_POINT('Origin',(-0.135237164733756,4.69632598481314,-0.12850808202611));
#146456=CARTESIAN_POINT('',(5.83009928675316,4.55994605333409,4.51507948538187));
#146457=CARTESIAN_POINT('Origin',(-8.76469036237282E-13,4.65175593300044,
-4.99166680212326E-13));
#146458=CARTESIAN_POINT('',(6.32482494729382,4.65066950023528,4.03070581740142));
#146459=CARTESIAN_POINT('Origin',(-0.157395227798709,4.69641604213913,-0.109027212761467));
#146460=CARTESIAN_POINT('Origin',(-0.153530278004034,4.5535734277484,-0.11627844380942));
#146461=CARTESIAN_POINT('Ctrl Pts',(5.13466768313966,4.429837254,5.46744454587086));
#146462=CARTESIAN_POINT('Ctrl Pts',(5.43093485171026,4.494719353,5.18920972569578));
#146463=CARTESIAN_POINT('Ctrl Pts',(5.69540184317369,4.559946053,4.88059012097226));
#146464=CARTESIAN_POINT('Ctrl Pts',(5.70449184166015,4.56218796077457,4.86998255242729));
#146465=CARTESIAN_POINT('Ctrl Pts',(5.71358184014662,4.56442986854915,4.85937498388234));
#146466=CARTESIAN_POINT('Ctrl Pts',(5.134148886,4.429837254,5.118888084));
#146467=CARTESIAN_POINT('Ctrl Pts',(5.411528649,4.494719353,4.840681376));
#146468=CARTESIAN_POINT('Ctrl Pts',(5.657221867,4.559946053,4.534130649));
#146469=CARTESIAN_POINT('Ctrl Pts',(5.66566659186864,4.56218796077458,4.52359418987881));
#146470=CARTESIAN_POINT('Ctrl Pts',(5.67411131673747,4.56442986854915,4.51305773075765));
#146471=CARTESIAN_POINT('',(5.69532420086355,4.55994605198929,4.87988547605668));
#146472=CARTESIAN_POINT('',(5.67627304106311,4.559946050062,4.70700805305583));
#146473=CARTESIAN_POINT('',(5.31306543994044,4.46959751861898,5.29351826587812));
#146474=CARTESIAN_POINT('Origin',(-0.145765720939184,4.55357073318668,-0.126234648917299));
#146475=CARTESIAN_POINT('Ctrl Pts',(5.13744736506547,4.43060907879088,5.1155776381838));
#146476=CARTESIAN_POINT('Ctrl Pts',(5.16664258312233,4.43741364571329,5.1452284831325));
#146477=CARTESIAN_POINT('Ctrl Pts',(5.19589131650275,4.44406034193146,5.17489625514891));
#146478=CARTESIAN_POINT('Ctrl Pts',(5.2544227315973,4.45704674544457,5.23419934774933));
#146479=CARTESIAN_POINT('Ctrl Pts',(5.28373675530313,4.4633934021658,5.26386641755855));
#146480=CARTESIAN_POINT('Ctrl Pts',(5.31306544082685,4.46959751861678,5.29351826500183));
#146481=CARTESIAN_POINT('Ctrl Pts',(4.896117256,4.559946053,5.681376225));
#146482=CARTESIAN_POINT('Ctrl Pts',(5.208019157,4.494288122,5.41258426));
#146483=CARTESIAN_POINT('Ctrl Pts',(5.488622484,4.429844992,5.11126434800001));
#146484=CARTESIAN_POINT('Ctrl Pts',(4.550255102,4.559946053,5.644260669));
#146485=CARTESIAN_POINT('Ctrl Pts',(4.860119396,4.494288122,5.394456192));
#146486=CARTESIAN_POINT('Ctrl Pts',(5.14077588500001,4.429844992,5.112232712));
#146487=CARTESIAN_POINT('',(4.89611726008958,4.55994605320499,5.68137622087235));
#146488=CARTESIAN_POINT('Origin',(-0.104450017754835,4.69632601596199,-0.154575716975075));
#146489=CARTESIAN_POINT('',(4.72318618057174,4.5599460533341,5.66281844568906));
#146490=CARTESIAN_POINT('Origin',(5.52509427098613E-13,4.65175593299956,
5.20417042793042E-13));
#146491=CARTESIAN_POINT('',(5.31047145089206,4.65066950022844,5.29612055861478));
#146492=CARTESIAN_POINT('Origin',(-0.130277934192288,4.69641604863111,-0.140313671209675));
#146493=CARTESIAN_POINT('Origin',(-0.124944090093938,4.55357340165287,-0.146564086543545));
#146494=CARTESIAN_POINT('Ctrl Pts',(3.83928304573516,4.429837254,6.44342050301162));
#146495=CARTESIAN_POINT('Ctrl Pts',(4.18843591350799,4.494719353,6.23537934195569));
#146496=CARTESIAN_POINT('Ctrl Pts',(4.51306390582353,4.559946053,5.99082767770735));
#146497=CARTESIAN_POINT('Ctrl Pts',(4.52422169846457,4.56218796069278,5.98242218950456));
#146498=CARTESIAN_POINT('Ctrl Pts',(4.53537949110564,4.56442986838557,5.97401670130179));
#146499=CARTESIAN_POINT('Ctrl Pts',(3.913705713,4.429837254,6.10290157100001));
#146500=CARTESIAN_POINT('Ctrl Pts',(4.24440671,4.494719353,5.890827631));
#146501=CARTESIAN_POINT('Ctrl Pts',(4.550255102,4.559946053,5.644260669));
#146502=CARTESIAN_POINT('Ctrl Pts',(4.56076742077199,4.56218796069278,5.63578591297389));
#146503=CARTESIAN_POINT('Ctrl Pts',(4.57127973954398,4.56442986838555,5.62731115694767));
#146504=CARTESIAN_POINT('',(4.51313955453792,4.55994605198798,5.9901228186567));
#146505=CARTESIAN_POINT('',(4.53169733829032,4.559946050062,5.81719173486759));
#146506=CARTESIAN_POINT('',(4.05089897038185,4.46959751858392,6.31191076693112));
#146507=CARTESIAN_POINT('Origin',(-0.115221112852132,4.55357071772783,-0.154618720067957));
#146508=CARTESIAN_POINT('Ctrl Pts',(3.91763872356155,4.43060907883284,6.10037759741906));
#146509=CARTESIAN_POINT('Ctrl Pts',(3.93977732792986,4.43741364861268,6.13561134577958));
#146510=CARTESIAN_POINT('Ctrl Pts',(3.96196455879317,4.44406034776373,6.17087313154928));
#146511=CARTESIAN_POINT('Ctrl Pts',(4.00637910359353,4.45704674351445,6.24137223282395));
#146512=CARTESIAN_POINT('Ctrl Pts',(4.02863023130927,4.46339339827232,6.27664734001664));
#146513=CARTESIAN_POINT('Ctrl Pts',(4.05089897160215,4.4695975185816,6.31191076616091));
#146514=CARTESIAN_POINT('Ctrl Pts',(3.560320807,4.559946053,6.601069288));
#146515=CARTESIAN_POINT('Ctrl Pts',(3.922712942,4.494288122,6.405611219));
#146516=CARTESIAN_POINT('Ctrl Pts',(4.261530793,4.429844992,6.171657419));
#146517=CARTESIAN_POINT('Ctrl Pts',(3.230523466,4.559946053,6.49047133400001));
#146518=CARTESIAN_POINT('Ctrl Pts',(3.586843883,4.494288122,6.31311881));
#146519=CARTESIAN_POINT('Ctrl Pts',(3.921608485,4.429844992,6.09782640700001));
#146520=CARTESIAN_POINT('',(3.56032081188552,4.55994605320498,6.60106928484802));
#146521=CARTESIAN_POINT('Origin',(-0.0687787297306519,4.69632601369697,
-0.173415322549491));
#146522=CARTESIAN_POINT('',(3.39542213831681,4.5599460533341,6.54577031005758));
#146523=CARTESIAN_POINT('Origin',(1.1145598333151E-12,4.65175593300067,
1.71824360295503E-12));
#146524=CARTESIAN_POINT('',(4.04780621136812,4.65066950020758,6.31389458847702));
#146525=CARTESIAN_POINT('Origin',(-0.0970687103811368,4.69641607733215,
-0.165038982886628));
#146526=CARTESIAN_POINT('Origin',(-0.0905159256706362,4.55357342512397,
-0.169996615526339));
#146527=CARTESIAN_POINT('Ctrl Pts',(2.3643777998641,4.429837254,7.11810927906325));
#146528=CARTESIAN_POINT('Ctrl Pts',(2.75009036708087,4.494719353,6.98998954960996));
#146529=CARTESIAN_POINT('Ctrl Pts',(3.11970011632363,4.559946053,6.82094079018461));
#146530=CARTESIAN_POINT('Ctrl Pts',(3.13240397732229,4.56218796066586,6.81513041330432));
#146531=CARTESIAN_POINT('Ctrl Pts',(3.14510783832095,4.56442986833173,6.80932003642402));
#146532=CARTESIAN_POINT('Ctrl Pts',(2.510262011,4.429837254,6.801550164));
#146533=CARTESIAN_POINT('Ctrl Pts',(2.878821031,4.494719353,6.665525334));
#146534=CARTESIAN_POINT('Ctrl Pts',(3.230523466,4.559946053,6.490471334));
#146535=CARTESIAN_POINT('Ctrl Pts',(3.24261183449213,4.56218796066586,6.48445455092591));
#146536=CARTESIAN_POINT('Ctrl Pts',(3.25470020298429,4.56442986833173,6.47843776785193));
#146537=CARTESIAN_POINT('',(3.11992552026391,4.55994605198798,6.82026867260156));
#146538=CARTESIAN_POINT('',(3.17522450484931,4.55994605006201,6.65536999669987));
#146539=CARTESIAN_POINT('',(2.5993169674646,4.46959751859883,7.0351653357458));
#146540=CARTESIAN_POINT('Origin',(-0.0792889617611636,4.55357072500979,
-0.175773205964725));
#146541=CARTESIAN_POINT('Ctrl Pts',(2.51464564998812,4.43060907880633,6.79993067958229));
#146542=CARTESIAN_POINT('Ctrl Pts',(2.52869244599149,4.43741364583256,6.83909981235757));
#146543=CARTESIAN_POINT('Ctrl Pts',(2.54278070368981,4.44406034218614,6.87830677841121));
#146544=CARTESIAN_POINT('Ctrl Pts',(2.57100165160829,4.4570467441366,6.95670550167926));
#146545=CARTESIAN_POINT('Ctrl Pts',(2.58514945651061,4.46339339956602,6.99593923562996));
#146546=CARTESIAN_POINT('Ctrl Pts',(2.59931696875979,4.46959751859659,7.03516533527836));
#146547=CARTESIAN_POINT('Ctrl Pts',(2.058047714,4.559946053,7.212103688));
#146548=CARTESIAN_POINT('Ctrl Pts',(2.45398503,4.494288122,7.099118916));
#146549=CARTESIAN_POINT('Ctrl Pts',(2.835174659,4.429844992,6.943470649));
#146550=CARTESIAN_POINT('Ctrl Pts',(1.759736143,4.559946053,7.03319477300001));
#146551=CARTESIAN_POINT('Ctrl Pts',(2.145851537,4.494288122,6.936587009));
#146552=CARTESIAN_POINT('Ctrl Pts',(2.519071031,4.429844992,6.798292516));
#146553=CARTESIAN_POINT('',(2.05804771942638,4.55994605320498,7.21210368597038));
#146554=CARTESIAN_POINT('Origin',(-0.0298916218067086,4.69632598925499,
-0.184146545734074));
#146555=CARTESIAN_POINT('',(1.90889193047692,4.5599460533341,7.12264922997018));
#146556=CARTESIAN_POINT('Origin',(4.04190569902596E-13,4.651755933,1.11542719505309E-12));
#146557=CARTESIAN_POINT('',(2.59587005224224,4.65066950021632,7.03643792502342));
#146558=CARTESIAN_POINT('Origin',(-0.0593208284753782,4.69641607253455,
-0.182047421545034));
#146559=CARTESIAN_POINT('Origin',(-0.051855568022259,4.5535734567917,-0.185480708781655));
#146560=CARTESIAN_POINT('Ctrl Pts',(0.778916875458042,4.429837254,7.45996317561411));
#146561=CARTESIAN_POINT('Ctrl Pts',(1.18315365183431,4.494719353,7.4177556149989));
#146562=CARTESIAN_POINT('Ctrl Pts',(1.58046261703443,4.559946053,7.33211429230165));
#146563=CARTESIAN_POINT('Ctrl Pts',(1.59411852788503,4.56218796062931,7.32917071344912));
#146564=CARTESIAN_POINT('Ctrl Pts',(1.60777443873569,4.56442986825872,7.32622713459661));
#146565=CARTESIAN_POINT('Ctrl Pts',(0.989441248,4.429837254,7.182165831));
#146566=CARTESIAN_POINT('Ctrl Pts',(1.37862488,4.494719353,7.12855048));
#146567=CARTESIAN_POINT('Ctrl Pts',(1.759736143,4.559946053,7.033194773));
#146568=CARTESIAN_POINT('Ctrl Pts',(1.77283532244858,4.56218796062931,7.02991730093683));
#146569=CARTESIAN_POINT('Ctrl Pts',(1.78593450189721,4.56442986825872,7.02663982887367));
#146570=CARTESIAN_POINT('',(1.5808272365642,4.55994605198799,7.33150634364818));
#146571=CARTESIAN_POINT('',(1.67028170264388,4.55994605006201,7.18235055439685));
#146572=CARTESIAN_POINT('',(1.02619379194291,4.46959751861026,7.42946339227434));
#146573=CARTESIAN_POINT('Origin',(-0.0396491670115839,4.55357071019899,
-0.188708442845131));
#146574=CARTESIAN_POINT('Ctrl Pts',(0.994070540727967,4.4306090787179,7.18152656204117));
#146575=CARTESIAN_POINT('Ctrl Pts',(0.999368724674737,4.43741364584496,
7.22279958843321));
#146576=CARTESIAN_POINT('Ctrl Pts',(1.00469926796512,4.44406034229402,7.26411847670696));
#146577=CARTESIAN_POINT('Ctrl Pts',(1.0154070183226,4.45704674513233,7.346750956186));
#146578=CARTESIAN_POINT('Ctrl Pts',(1.02078996321937,4.46339340157552,7.38810879397391));
#146579=CARTESIAN_POINT('Ctrl Pts',(1.02619379320752,4.46959751860798,7.42946339210943));
#146580=CARTESIAN_POINT('Ctrl Pts',(0.459542598,4.559946053,7.485908135));
#146581=CARTESIAN_POINT('Ctrl Pts',(0.870511505,4.494288122,7.460679703));
#146582=CARTESIAN_POINT('Ctrl Pts',(1.276248909,4.429844992,7.390614908));
#146583=CARTESIAN_POINT('Ctrl Pts',(0.206665513,4.559946053,7.24705384000001));
#146584=CARTESIAN_POINT('Ctrl Pts',(0.604521557,4.494288122,7.235708109));
#146585=CARTESIAN_POINT('Ctrl Pts',(0.998744615,4.429844992,7.180878024));
#146586=CARTESIAN_POINT('',(0.459542603715409,4.55994605320497,7.48590813417827));
#146587=CARTESIAN_POINT('Origin',(0.0103932901638211,4.6963260159548,-0.186267111405733));
#146588=CARTESIAN_POINT('',(0.333104057544598,4.5599460533341,7.36648098740755));
#146589=CARTESIAN_POINT('Origin',(1.11808349037568E-13,4.65175593299867,
3.36970035208495E-13));
#146590=CARTESIAN_POINT('',(1.02255389523181,4.65066950018923,7.42996524430959));
#146591=CARTESIAN_POINT('Origin',(-0.0187991239028218,4.69641606393237,
-0.190543498803789));
#146592=CARTESIAN_POINT('Origin',(-0.010770327658639,4.55357343712198,-0.192291557691001));
#146593=CARTESIAN_POINT('Origin',(3.1413063881873E-14,4.65175593299889,
-5.35162192338845E-13));
#146594=CARTESIAN_POINT('',(-0.0321887715704092,4.55994605198799,7.49993092670762));
#146595=CARTESIAN_POINT('Origin',(0.00184455323510964,4.55357069936849,
-0.192820044880267));
#146596=CARTESIAN_POINT('',(-0.598575745926012,4.65066950019027,7.4760756466581));
#146597=CARTESIAN_POINT('Origin',(0.0226016159796813,4.69641607088498,-0.190129976565602));
#146598=CARTESIAN_POINT('Origin',(0.0308184870555671,4.55357345041732,-0.190111286116755));
#146599=CARTESIAN_POINT('Ctrl Pts',(-0.842965336257949,4.429837254,7.45299748588614));
#146600=CARTESIAN_POINT('Ctrl Pts',(-0.439106013265463,4.494719353,7.49867567223329));
#146601=CARTESIAN_POINT('Ctrl Pts',(-0.0326755574928418,4.559946053,7.50044627943846));
#146602=CARTESIAN_POINT('Ctrl Pts',(-0.0187061319879682,4.56218796059731,
7.50050713699747));
#146603=CARTESIAN_POINT('Ctrl Pts',(-0.00473670648309503,4.56442986819472,
7.50056799455651));
#146604=CARTESIAN_POINT('Ctrl Pts',(-0.577644689,4.429837254,7.226951405));
#146605=CARTESIAN_POINT('Ctrl Pts',(-0.186034238,4.494719353,7.25825252900001));
#146606=CARTESIAN_POINT('Ctrl Pts',(0.206665513,4.559946053,7.24705384));
#146607=CARTESIAN_POINT('Ctrl Pts',(0.220163000305543,4.56218796059731,
7.24666892974164));
#146608=CARTESIAN_POINT('Ctrl Pts',(0.233660487611081,4.56442986819472,
7.24628401948334));
#146609=CARTESIAN_POINT('',(0.087238384113425,4.55994605006201,7.37349238228569));
#146610=CARTESIAN_POINT('Ctrl Pts',(-0.0311662252067879,1.197203562,7.50045145207052));
#146611=CARTESIAN_POINT('Ctrl Pts',(0.374955034121473,1.261925886,7.50213898586559));
#146612=CARTESIAN_POINT('Ctrl Pts',(0.778884123117372,1.327100493,7.45996533766874));
#146613=CARTESIAN_POINT('Ctrl Pts',(0.792744303612179,1.32933685537475,
7.45851821639903));
#146614=CARTESIAN_POINT('Ctrl Pts',(0.80660448410698,1.33157321774951,7.45707109512947));
#146615=CARTESIAN_POINT('Ctrl Pts',(0.208122714,1.197203562,7.247012139));
#146616=CARTESIAN_POINT('Ctrl Pts',(0.600521186,1.261925886,7.235743076));
#146617=CARTESIAN_POINT('Ctrl Pts',(0.989408718000001,1.327100493,7.18217031200001));
#146618=CARTESIAN_POINT('Ctrl Pts',(1.00275277152954,1.32933685537475,7.18033204830749));
#146619=CARTESIAN_POINT('Ctrl Pts',(1.01609682505909,1.33157321774952,7.17849378461507));
#146620=CARTESIAN_POINT('',(0.212788489828452,1.19797317409522,7.24687664206066));
#146621=CARTESIAN_POINT('Origin',(-0.029119033607513,1.33927933890375,-0.196346974783305));
#146622=CARTESIAN_POINT('Ctrl Pts',(0.212788489729122,1.19797317409288,
7.2468766420302));
#146623=CARTESIAN_POINT('Ctrl Pts',(0.213408818267352,1.20265893835229,
7.27550948625658));
#146624=CARTESIAN_POINT('Ctrl Pts',(0.214002544381766,1.20726223981372,
7.30415652228153));
#146625=CARTESIAN_POINT('Ctrl Pts',(0.214571291475999,1.21178747097482,
7.33281625257192));
#146626=CARTESIAN_POINT('Ctrl Pts',(0.214676296681177,1.21262294394929,
7.33810756902866));
#146627=CARTESIAN_POINT('Ctrl Pts',(0.214780860070305,1.21345569336825,
7.34339933287842));
#146628=CARTESIAN_POINT('Ctrl Pts',(0.214885194021124,1.214285714,7.34869153090483));
#146629=CARTESIAN_POINT('Ctrl Pts',(0.215319481528753,1.21774065444455,
7.37072017354804));
#146630=CARTESIAN_POINT('Ctrl Pts',(0.215750821020856,1.22115495459576,
7.39275528414919));
#146631=CARTESIAN_POINT('Ctrl Pts',(0.216194451260588,1.2245278005957,7.41479644373849));
#146632=CARTESIAN_POINT('Ctrl Pts',(0.216744671851216,1.2287110350823,7.44213339861891));
#146633=CARTESIAN_POINT('Ctrl Pts',(0.217305051301642,1.23283187911727,
7.46947976624647));
#146634=CARTESIAN_POINT('Ctrl Pts',(0.217874905420452,1.23689319502459,
7.4968347000478));
#146635=CARTESIAN_POINT('Ctrl Pts',(1.25849016475008,1.32841655815206,7.39366423866198));
#146636=CARTESIAN_POINT('Ctrl Pts',(1.26256514337504,1.32775852557603,7.39296600483099));
#146637=CARTESIAN_POINT('Ctrl Pts',(1.266640122,1.327100493,7.392267771));
#146638=CARTESIAN_POINT('Ctrl Pts',(1.618926333,1.270212881,7.331904718));
#146639=CARTESIAN_POINT('Ctrl Pts',(1.963875725,1.214285714,7.238314178));
#146640=CARTESIAN_POINT('Ctrl Pts',(2.016468661,1.205758742,7.22404483400001));
#146641=CARTESIAN_POINT('Ctrl Pts',(2.068848696,1.197204389,7.209012767));
#146642=CARTESIAN_POINT('Ctrl Pts',(0.981490392688463,1.32841655815206,
7.18326113271219));
#146643=CARTESIAN_POINT('Ctrl Pts',(0.985449555344232,1.32775852557603,
7.18271572235609));
#146644=CARTESIAN_POINT('Ctrl Pts',(0.989408718,1.327100493,7.18217031200001));
#146645=CARTESIAN_POINT('Ctrl Pts',(1.331682516,1.270212881,7.13501901));
#146646=CARTESIAN_POINT('Ctrl Pts',(1.667921256,1.214285714,7.055532488));
#146647=CARTESIAN_POINT('Ctrl Pts',(1.719186117,1.205758742,7.043413523));
#146648=CARTESIAN_POINT('Ctrl Pts',(1.770269464,1.197204389,7.030550905));
#146649=CARTESIAN_POINT('',(1.76567787415336,1.19797317427034,7.03170545742107));
#146650=CARTESIAN_POINT('Ctrl Pts',(1.76567787426916,1.19797317415285,7.03170545796061));
#146651=CARTESIAN_POINT('Ctrl Pts',(1.73312358395914,1.20342302018589,7.03987991737876));
#146652=CARTESIAN_POINT('Ctrl Pts',(1.70053641067916,1.20886077954585,7.04782229606081));
#146653=CARTESIAN_POINT('Ctrl Pts',(1.66792125607932,1.21428571398681,7.05553248798125));
#146654=CARTESIAN_POINT('Ctrl Pts',(1.52423747091137,1.23818488470188,7.08949919970331));
#146655=CARTESIAN_POINT('Ctrl Pts',(1.37901947255166,1.26233328407548,7.11918993281469));
#146656=CARTESIAN_POINT('Ctrl Pts',(1.2326558542626,1.28666618647768,7.14444256381536));
#146657=CARTESIAN_POINT('Ctrl Pts',(1.15189907534906,1.30009197385974,7.158375815552));
#146658=CARTESIAN_POINT('Ctrl Pts',(1.07079398594151,1.31357385569416,7.17095875770949));
#146659=CARTESIAN_POINT('Ctrl Pts',(0.989408725594587,1.32710049182887,
7.18217031144485));
#146660=CARTESIAN_POINT('Ctrl Pts',(1.82437897686925,1.23689319179771,7.27472620427518));
#146661=CARTESIAN_POINT('Ctrl Pts',(1.81762552129248,1.23263224513668,7.24682614389789));
#146662=CARTESIAN_POINT('Ctrl Pts',(1.81088428609454,1.22830577224837,7.21893304355694));
#146663=CARTESIAN_POINT('Ctrl Pts',(1.80415624475797,1.22391046495537,7.19104769004101));
#146664=CARTESIAN_POINT('Ctrl Pts',(1.79774357016075,1.21972118102936,7.16446942020277));
#146665=CARTESIAN_POINT('Ctrl Pts',(1.79135285131702,1.21547100858144,7.1378953600032));
#146666=CARTESIAN_POINT('Ctrl Pts',(1.78494930497304,1.21115091644535,7.11133583589125));
#146667=CARTESIAN_POINT('Ctrl Pts',(1.77854559786201,1.20683071584928,7.08477564497744));
#146668=CARTESIAN_POINT('Ctrl Pts',(1.77212215308869,1.20243940496519,7.05823165975828));
#146669=CARTESIAN_POINT('Ctrl Pts',(1.76567787233811,1.19797317480699,7.0317054555096));
#146670=CARTESIAN_POINT('Ctrl Pts',(1.58193777457235,1.197203562,7.33179488248356));
#146671=CARTESIAN_POINT('Ctrl Pts',(1.9789269150576,1.261925886,7.24613889640439));
#146672=CARTESIAN_POINT('Ctrl Pts',(2.36434627734697,1.327100493,7.11811843102544));
#146673=CARTESIAN_POINT('Ctrl Pts',(2.37757132469114,1.32933685512278,7.11372561405432));
#146674=CARTESIAN_POINT('Ctrl Pts',(2.39079637203526,1.33157321724558,7.10933279708321));
#146675=CARTESIAN_POINT('Ctrl Pts',(1.76115031,1.197203562,7.032840791));
#146676=CARTESIAN_POINT('Ctrl Pts',(2.141952209,1.261925886,6.93748112));
#146677=CARTESIAN_POINT('Ctrl Pts',(2.510231206,1.327100493,6.801561533));
#146678=CARTESIAN_POINT('Ctrl Pts',(2.52286810919618,1.32933685512278,6.79689767033782));
#146679=CARTESIAN_POINT('Ctrl Pts',(2.53550501239241,1.33157321724559,6.79223380767549));
#146680=CARTESIAN_POINT('Origin',(-0.0706469541574262,1.33927932656119,
-0.185496486810866));
#146681=CARTESIAN_POINT('Ctrl Pts',(2.81848662049146,1.32841655815206,6.95026629291661));
#146682=CARTESIAN_POINT('Ctrl Pts',(2.82231622874573,1.32775852557603,6.9487083834583));
#146683=CARTESIAN_POINT('Ctrl Pts',(2.826145837,1.327100493,6.947150474));
#146684=CARTESIAN_POINT('Ctrl Pts',(3.15721952,1.270212881,6.812467554));
#146685=CARTESIAN_POINT('Ctrl Pts',(3.473984987,1.214285714,6.646911186));
#146686=CARTESIAN_POINT('Ctrl Pts',(3.522280843,1.205758742,6.62166952500001));
#146687=CARTESIAN_POINT('Ctrl Pts',(3.570204811,1.197204389,6.59572874));
#146688=CARTESIAN_POINT('Ctrl Pts',(2.50273250095792,1.32841655815206,6.80432905678979));
#146689=CARTESIAN_POINT('Ctrl Pts',(2.50648185347896,1.32775852557603,6.80294529489489));
#146690=CARTESIAN_POINT('Ctrl Pts',(2.510231206,1.327100493,6.801561533));
#146691=CARTESIAN_POINT('Ctrl Pts',(2.834366696,1.270212881,6.681933854));
#146692=CARTESIAN_POINT('Ctrl Pts',(3.145657109,1.214285714,6.532024292));
#146693=CARTESIAN_POINT('Ctrl Pts',(3.193118207,1.205758742,6.509168232));
#146694=CARTESIAN_POINT('Ctrl Pts',(3.240242171,1.197204389,6.485624925));
#146695=CARTESIAN_POINT('',(3.23600612405357,1.19797317421957,6.48773954035198));
#146696=CARTESIAN_POINT('Ctrl Pts',(3.23600612183536,1.19797317447889,6.48773953829102));
#146697=CARTESIAN_POINT('Ctrl Pts',(3.190985273,1.20614195,6.510195399));
#146698=CARTESIAN_POINT('Ctrl Pts',(3.145657109,1.214285714,6.532024292));
#146699=CARTESIAN_POINT('Ctrl Pts',(2.83436669912389,1.27021288012494,6.68193385275316));
#146700=CARTESIAN_POINT('Ctrl Pts',(2.5102312133073,1.32710049490568,6.80156153026079));
#146701=CARTESIAN_POINT('Ctrl Pts',(3.34557710467326,1.2368931917972,6.71245959653521));
#146702=CARTESIAN_POINT('Ctrl Pts',(3.33298385271176,1.23263224513067,6.6866636173957));
#146703=CARTESIAN_POINT('Ctrl Pts',(3.32040403182692,1.22830577224287,6.66087180846766));
#146704=CARTESIAN_POINT('Ctrl Pts',(3.30783876168844,1.22391046495352,6.63508472895175));
#146705=CARTESIAN_POINT('Ctrl Pts',(3.29586246955396,1.21972118103539,6.61050637972617));
#146706=CARTESIAN_POINT('Ctrl Pts',(3.28390852482557,1.21547100859969,6.58592742187279));
#146707=CARTESIAN_POINT('Ctrl Pts',(3.27194517730308,1.2111509164746,6.56136541780598));
#146708=CARTESIAN_POINT('Ctrl Pts',(3.25998152942953,1.20683071588954,6.53680279708701));
#146709=CARTESIAN_POINT('Ctrl Pts',(3.2480020891073,1.20243940502162,6.51226024618941));
#146710=CARTESIAN_POINT('Ctrl Pts',(3.23600612183536,1.19797317447889,6.48773953829102));
#146711=CARTESIAN_POINT('Ctrl Pts',(3.12107212213229,1.197203562,6.82031173226986));
#146712=CARTESIAN_POINT('Ctrl Pts',(3.49036637109644,1.261925886,6.65131740573583));
#146713=CARTESIAN_POINT('Ctrl Pts',(3.83925422858829,1.327100493,6.44343621778777));
#146714=CARTESIAN_POINT('Ctrl Pts',(3.85122575575511,1.32933685509038,6.43630310829271));
#146715=CARTESIAN_POINT('Ctrl Pts',(3.86319728292196,1.33157321718078,6.42916999879751));
#146716=CARTESIAN_POINT('Ctrl Pts',(3.231828475,1.197203562,6.489821624));
#146717=CARTESIAN_POINT('Ctrl Pts',(3.583227927,1.261925886,6.314830257));
#146718=CARTESIAN_POINT('Ctrl Pts',(3.913678072,1.327100493,6.102919297));
#146719=CARTESIAN_POINT('Ctrl Pts',(3.92501693863925,1.32933685509038,6.09564791234125));
#146720=CARTESIAN_POINT('Ctrl Pts',(3.93635580527844,1.33157321718077,6.08837652768251));
#146721=CARTESIAN_POINT('Origin',(-0.108871366719813,1.33927930073689,-0.165972435109042));
#146722=CARTESIAN_POINT('Ctrl Pts',(4.24669377469677,1.32841655815206,6.18188161995671));
#146723=CARTESIAN_POINT('Ctrl Pts',(4.25009894434838,1.32775852557603,6.17953688097835));
#146724=CARTESIAN_POINT('Ctrl Pts',(4.253504114,1.327100493,6.177192142));
#146725=CARTESIAN_POINT('Ctrl Pts',(4.547884631,1.270212881,5.974486978));
#146726=CARTESIAN_POINT('Ctrl Pts',(4.821654572,1.214285714,5.744706014));
#146727=CARTESIAN_POINT('Ctrl Pts',(4.863395087,1.205758742,5.709672308));
#146728=CARTESIAN_POINT('Ctrl Pts',(4.904622117,1.197204389,5.674035767));
#146729=CARTESIAN_POINT('Ctrl Pts',(3.90694961831175,1.32841655815206,6.10723411756124));
#146730=CARTESIAN_POINT('Ctrl Pts',(3.91031384515587,1.32775852557603,6.10507670728062));
#146731=CARTESIAN_POINT('Ctrl Pts',(3.913678072,1.327100493,6.102919297));
#146732=CARTESIAN_POINT('Ctrl Pts',(4.20451904,1.270212881,5.916408897));
#146733=CARTESIAN_POINT('Ctrl Pts',(4.476305531,1.214285714,5.703085901));
#146734=CARTESIAN_POINT('Ctrl Pts',(4.517743638,1.205758742,5.67056147000001));
#146735=CARTESIAN_POINT('Ctrl Pts',(4.55870475500001,1.197204389,5.637438333));
#146736=CARTESIAN_POINT('',(4.55502232464208,1.19797317423656,5.64041413517156));
#146737=CARTESIAN_POINT('Ctrl Pts',(4.5550223262341,1.19797317450824,5.64041413707271));
#146738=CARTESIAN_POINT('Ctrl Pts',(4.45269302247191,1.21932945754499,5.72305208213578));
#146739=CARTESIAN_POINT('Ctrl Pts',(4.34815191940103,1.24060038382255,5.80287856834028));
#146740=CARTESIAN_POINT('Ctrl Pts',(4.18786400048255,1.2728618071633,5.91850090968448));
#146741=CARTESIAN_POINT('Ctrl Pts',(4.13380351650863,1.28366385405618,5.95638525333352));
#146742=CARTESIAN_POINT('Ctrl Pts',(4.05190608929962,1.29991103400534,6.01212525060261));
#146743=CARTESIAN_POINT('Ctrl Pts',(4.02444922772756,1.30533866131656,6.03053905404981));
#146744=CARTESIAN_POINT('Ctrl Pts',(3.98306679322179,1.31349012124639,6.05788350614987));
#146745=CARTESIAN_POINT('Ctrl Pts',(3.96923445152479,1.31620998869334,6.06695570360523));
#146746=CARTESIAN_POINT('Ctrl Pts',(3.94843724190009,1.32029216629499,6.0804943727962));
#146747=CARTESIAN_POINT('Ctrl Pts',(3.94149544566517,1.32165353797213,6.08499647671232));
#146748=CARTESIAN_POINT('Ctrl Pts',(3.92791385812345,1.32431471601509,6.09377182750367));
#146749=CARTESIAN_POINT('Ctrl Pts',(3.92454773867684,1.32497441947025,6.09594880219572));
#146750=CARTESIAN_POINT('Ctrl Pts',(3.91367807818555,1.32710049214421,6.10291929458987));
#146751=CARTESIAN_POINT('Ctrl Pts',(4.71033976554031,1.23689319179788,5.83632583836518));
#146752=CARTESIAN_POINT('Ctrl Pts',(4.69249556405988,1.23263224512587,5.81384013165564));
#146753=CARTESIAN_POINT('Ctrl Pts',(4.67466537587517,1.22830577223152,5.79135561055883));
#146754=CARTESIAN_POINT('Ctrl Pts',(4.65685041491457,1.22391046493341,5.76887258033722));
#146755=CARTESIAN_POINT('Ctrl Pts',(4.63987050326617,1.21972118100769,5.74744340810409));
#146756=CARTESIAN_POINT('Ctrl Pts',(4.62291228568413,1.21547100855891,5.72600883746783));
#146757=CARTESIAN_POINT('Ctrl Pts',(4.60594852970562,1.21115091642268,5.70459284556852));
#146758=CARTESIAN_POINT('Ctrl Pts',(4.58898434783614,1.2068307158265,5.68317631600067));
#146759=CARTESIAN_POINT('Ctrl Pts',(4.5720090572157,1.20243940496165,5.66178278189173));
#146760=CARTESIAN_POINT('Ctrl Pts',(4.55502232146844,1.19797317447799,5.64041413304004));
#146761=CARTESIAN_POINT('Ctrl Pts',(4.51426860610597,1.197203562,5.98991838655528));
#146762=CARTESIAN_POINT('Ctrl Pts',(4.83860017587706,1.261925886,5.74548770562734));
#146763=CARTESIAN_POINT('Ctrl Pts',(5.13464291838637,1.327100493,5.46746608780804));
#146764=CARTESIAN_POINT('Ctrl Pts',(5.14480114980126,1.32933685500188,5.4579262223541));
#146765=CARTESIAN_POINT('Ctrl Pts',(5.15495938121626,1.33157321700378,5.44838635690018));
#146766=CARTESIAN_POINT('Ctrl Pts',(4.551389933,1.197203562,5.643345611));
#146767=CARTESIAN_POINT('Ctrl Pts',(4.85695589,1.261925886,5.39690495));
#146768=CARTESIAN_POINT('Ctrl Pts',(5.134125702,1.327100493,5.118911337));
#146769=CARTESIAN_POINT('Ctrl Pts',(5.14363633910482,1.32933685500188,5.10937243248646));
#146770=CARTESIAN_POINT('Ctrl Pts',(5.15314697620968,1.33157321700379,5.09983352797292));
#146771=CARTESIAN_POINT('Origin',(-0.14200526905505,1.33927922316676,-0.138688075081163));
#146772=CARTESIAN_POINT('Ctrl Pts',(5.47633024678037,1.32841655815206,5.12443903217739));
#146773=CARTESIAN_POINT('Ctrl Pts',(5.47915175589019,1.32775852557603,5.12141710108869));
#146774=CARTESIAN_POINT('Ctrl Pts',(5.481973265,1.327100493,5.11839517));
#146775=CARTESIAN_POINT('Ctrl Pts',(5.725895711,1.270212881,4.857146032));
#146776=CARTESIAN_POINT('Ctrl Pts',(5.943868948,1.214285714,4.573884774));
#146777=CARTESIAN_POINT('Ctrl Pts',(5.977102382,1.205758742,4.53069716));
#146778=CARTESIAN_POINT('Ctrl Pts',(6.009704745,1.197204389,4.487031188));
#146779=CARTESIAN_POINT('Ctrl Pts',(5.12848211471851,1.32841655815206,5.12457169809598));
#146780=CARTESIAN_POINT('Ctrl Pts',(5.13130390835926,1.32775852557603,5.121741517548));
#146781=CARTESIAN_POINT('Ctrl Pts',(5.134125702,1.327100493,5.118911337));
#146782=CARTESIAN_POINT('Ctrl Pts',(5.378072746,1.270212881,4.874239236));
#146783=CARTESIAN_POINT('Ctrl Pts',(5.597646882,1.214285714,4.607477551));
#146784=CARTESIAN_POINT('Ctrl Pts',(5.631124397,1.205758742,4.566805555));
#146785=CARTESIAN_POINT('Ctrl Pts',(5.664007371,1.197204389,4.52565139));
#146786=CARTESIAN_POINT('',(5.66105074323027,1.19797317421628,4.52934923308381));
#146787=CARTESIAN_POINT('Ctrl Pts',(5.66105074131956,1.19797317480725,4.52934923316803));
#146788=CARTESIAN_POINT('Ctrl Pts',(5.629619895,1.20614195,4.568633382));
#146789=CARTESIAN_POINT('Ctrl Pts',(5.597646882,1.214285714,4.607477551));
#146790=CARTESIAN_POINT('Ctrl Pts',(5.37807274867207,1.27021288013103,4.87423923389415));
#146791=CARTESIAN_POINT('Ctrl Pts',(5.13412570708811,1.32710049454013,5.11891133135881));
#146792=CARTESIAN_POINT('Ctrl Pts',(5.85485217388923,1.23689319179752,4.68729197081351));
#146793=CARTESIAN_POINT('Ctrl Pts',(5.83259139768625,1.23263224512641,4.66916794326474));
#146794=CARTESIAN_POINT('Ctrl Pts',(5.81034456199047,1.22830577224701,4.65104206117558));
#146795=CARTESIAN_POINT('Ctrl Pts',(5.78811291800978,1.22391046496545,4.63291436170114));
#146796=CARTESIAN_POINT('Ctrl Pts',(5.76692334865123,1.21972118105214,4.61563637066915));
#146797=CARTESIAN_POINT('Ctrl Pts',(5.74575380567806,1.2154710086199,4.59834844384771));
#146798=CARTESIAN_POINT('Ctrl Pts',(5.72458284762704,1.21115091649015,4.58107985205215));
#146799=CARTESIAN_POINT('Ctrl Pts',(5.70341135805905,1.20683071590039,4.56381082671223));
#146800=CARTESIAN_POINT('Ctrl Pts',(5.68223396277897,1.20243940503825,4.54656664728988));
#146801=CARTESIAN_POINT('Ctrl Pts',(5.66105074131956,1.19797317480725,4.52934923316803));
#146802=CARTESIAN_POINT('Ctrl Pts',(5.69638290676076,1.197203562,4.87944311363531));
#146803=CARTESIAN_POINT('Ctrl Pts',(5.96058641405332,1.261925886,4.57100538662929));
#146804=CARTESIAN_POINT('Ctrl Pts',(6.18994141211522,1.327100493,4.2358433205941));
#146805=CARTESIAN_POINT('Ctrl Pts',(6.19781136074892,1.32933685503111,4.22434277224787));
#146806=CARTESIAN_POINT('Ctrl Pts',(6.20568130938254,1.33157321706224,4.21284222390164));
#146807=CARTESIAN_POINT('Ctrl Pts',(5.658133455,1.197203562,4.532993029));
#146808=CARTESIAN_POINT('Ctrl Pts',(5.903577993,1.261925886,4.226626366));
#146809=CARTESIAN_POINT('Ctrl Pts',(6.114507319,1.327100493,3.895548773));
#146810=CARTESIAN_POINT('Ctrl Pts',(6.12174502027091,1.32933685503111,3.88418837679022));
#146811=CARTESIAN_POINT('Ctrl Pts',(6.12898272154169,1.33157321706224,3.87282798058039));
#146812=CARTESIAN_POINT('Origin',(-0.168499168376953,1.33927933743112,-0.104918689288322));
#146813=CARTESIAN_POINT('Ctrl Pts',(6.44989960413632,1.32841655815206,3.82738337217394));
#146814=CARTESIAN_POINT('Ctrl Pts',(6.45200552206816,1.32775852557603,3.82382555108697));
#146815=CARTESIAN_POINT('Ctrl Pts',(6.45411144,1.327100493,3.82026773));
#146816=CARTESIAN_POINT('Ctrl Pts',(6.636170272,1.270212881,3.512690335));
#146817=CARTESIAN_POINT('Ctrl Pts',(6.788154619,1.214285714,3.189193765));
#146818=CARTESIAN_POINT('Ctrl Pts',(6.811327012,1.205758742,3.139871648));
#146819=CARTESIAN_POINT('Ctrl Pts',(6.833780257,1.197204389,3.090218018));
#146820=CARTESIAN_POINT('Ctrl Pts',(6.110212485956,1.32841655815206,3.9022900024487));
#146821=CARTESIAN_POINT('Ctrl Pts',(6.112359902478,1.32775852557603,3.89891938772435));
#146822=CARTESIAN_POINT('Ctrl Pts',(6.114507319,1.327100493,3.895548773));
#146823=CARTESIAN_POINT('Ctrl Pts',(6.300153748,1.270212881,3.604155566));
#146824=CARTESIAN_POINT('Ctrl Pts',(6.457248486,1.214285714,3.296428672));
#146825=CARTESIAN_POINT('Ctrl Pts',(6.481200039,1.205758742,3.249510888));
#146826=CARTESIAN_POINT('Ctrl Pts',(6.504467298,1.197204389,3.202250017));
#146827=CARTESIAN_POINT('',(6.50237472112378,1.19797317411054,3.20649699370496));
#146828=CARTESIAN_POINT('Ctrl Pts',(6.50237471819508,1.1979731744789,3.2064969933566));
#146829=CARTESIAN_POINT('Ctrl Pts',(6.48012364,1.20614195,3.251619405));
#146830=CARTESIAN_POINT('Ctrl Pts',(6.457248486,1.214285714,3.296428672));
#146831=CARTESIAN_POINT('Ctrl Pts',(6.30015374986331,1.27021288013871,3.60415556227763));
#146832=CARTESIAN_POINT('Ctrl Pts',(6.11450732322867,1.32710049475556,3.89554876596969));
#146833=CARTESIAN_POINT('Ctrl Pts',(6.72559820205922,1.2368931917972,3.31908553995813));
#146834=CARTESIAN_POINT('Ctrl Pts',(6.69996174009863,1.23263224516912,3.30617065118014));
#146835=CARTESIAN_POINT('Ctrl Pts',(6.67433849417783,1.22830577227737,3.29325095419084));
#146836=CARTESIAN_POINT('Ctrl Pts',(6.6487296941165,1.22391046498266,3.28032621653173));
#146837=CARTESIAN_POINT('Ctrl Pts',(6.6243212678066,1.21972118106638,3.26800730639257));
#146838=CARTESIAN_POINT('Ctrl Pts',(6.59993026376815,1.21547100862723,3.25567438769194));
#146839=CARTESIAN_POINT('Ctrl Pts',(6.57554203423745,1.21115091650354,3.24336065608557));
#146840=CARTESIAN_POINT('Ctrl Pts',(6.55115319241728,1.20683071591987,3.23104661533138));
#146841=CARTESIAN_POINT('Ctrl Pts',(6.52676392411201,1.20243940506709,3.21875810912996));
#146842=CARTESIAN_POINT('Ctrl Pts',(6.50237471819508,1.1979731744789,3.2064969933566));
#146843=CARTESIAN_POINT('Ctrl Pts',(6.61214067371343,1.197203562,3.54081050413872));
#146844=CARTESIAN_POINT('Ctrl Pts',(6.80386225587355,1.261925886,3.18278793553475));
#146845=CARTESIAN_POINT('Ctrl Pts',(6.95580512444779,1.327100493,2.80615722777762));
#146846=CARTESIAN_POINT('Ctrl Pts',(6.96101880035735,1.32933685513807,2.79323374893157));
#146847=CARTESIAN_POINT('Ctrl Pts',(6.96623247626691,1.33157321727617,2.78031027008552));
#146848=CARTESIAN_POINT('Ctrl Pts',(6.500308946,1.197203562,3.210682731));
#146849=CARTESIAN_POINT('Ctrl Pts',(6.67415535,1.261925886,2.85871543));
#146850=CARTESIAN_POINT('Ctrl Pts',(6.80898137100001,1.327100493,2.490034677));
#146851=CARTESIAN_POINT('Ctrl Pts',(6.81360770973021,1.32933685513807,2.47738398810445));
#146852=CARTESIAN_POINT('Ctrl Pts',(6.81823404846052,1.33157321727617,2.46473329920893));
#146853=CARTESIAN_POINT('Origin',(-0.187113963710771,1.33927926563982,-0.0662433586541727));
#146854=CARTESIAN_POINT('Ctrl Pts',(7.12187882321818,1.32841655815206,2.35136351863108));
#146855=CARTESIAN_POINT('Ctrl Pts',(7.12317067960909,1.32775852557603,2.34743616731554));
#146856=CARTESIAN_POINT('Ctrl Pts',(7.124462536,1.327100493,2.343508816));
#146857=CARTESIAN_POINT('Ctrl Pts',(7.236144887,1.270212881,2.003985142));
#146858=CARTESIAN_POINT('Ctrl Pts',(7.315033724,1.214285714,1.655379601));
#146859=CARTESIAN_POINT('Ctrl Pts',(7.327061562,1.205758742,1.602229227));
#146860=CARTESIAN_POINT('Ctrl Pts',(7.3383158,1.197204389,1.548909688));
#146861=CARTESIAN_POINT('Ctrl Pts',(6.80623611384359,1.32841655815206,2.49754156239315));
#146862=CARTESIAN_POINT('Ctrl Pts',(6.8076087424218,1.32775852557603,2.49378811969658));
#146863=CARTESIAN_POINT('Ctrl Pts',(6.808981371,1.327100493,2.490034677));
#146864=CARTESIAN_POINT('Ctrl Pts',(6.927646563,1.270212881,2.165545587));
#146865=CARTESIAN_POINT('Ctrl Pts',(7.014916327,1.214285714,1.831242452));
#146866=CARTESIAN_POINT('Ctrl Pts',(7.02822197,1.205758742,1.780272704));
#146867=CARTESIAN_POINT('Ctrl Pts',(7.040785563,1.197204389,1.729114993));
#146868=CARTESIAN_POINT('',(7.03965488487991,1.1979731743181,1.73371252044924));
#146869=CARTESIAN_POINT('Ctrl Pts',(7.03965488692215,1.19797317452205,1.73371252091809));
#146870=CARTESIAN_POINT('Ctrl Pts',(7.00820159908294,1.21932945201026,1.86142703754406));
#146871=CARTESIAN_POINT('Ctrl Pts',(6.97328608937065,1.24060037606359,1.98824191820624));
#146872=CARTESIAN_POINT('Ctrl Pts',(6.91565362742755,1.27286181119524,2.17729024714639));
#146873=CARTESIAN_POINT('Ctrl Pts',(6.89554307007011,1.28366386197295,2.24016574396921));
#146874=CARTESIAN_POINT('Ctrl Pts',(6.86407752069048,1.29991103403137,2.33410213484067));
#146875=CARTESIAN_POINT('Ctrl Pts',(6.85336286270133,1.30533866133473,2.36537742066021));
#146876=CARTESIAN_POINT('Ctrl Pts',(6.83696675098894,1.31349012125373,2.41218973157219));
#146877=CARTESIAN_POINT('Ctrl Pts',(6.83144517969175,1.31620998869666,2.42778302154494));
#146878=CARTESIAN_POINT('Ctrl Pts',(6.82308191887862,1.32029216629291,2.45114699715551));
#146879=CARTESIAN_POINT('Ctrl Pts',(6.82028016025447,1.32165353796822,2.45893208693062));
#146880=CARTESIAN_POINT('Ctrl Pts',(6.81477856866167,1.32431471600427,2.47413730936304));
#146881=CARTESIAN_POINT('Ctrl Pts',(6.81341627267494,1.32497441974609,2.47790747414497));
#146882=CARTESIAN_POINT('Ctrl Pts',(6.80898137350066,1.32710049247487,2.49003467335198));
#146883=CARTESIAN_POINT('Ctrl Pts',(7.28186273349879,1.2368931917972,1.79568235830491));
#146884=CARTESIAN_POINT('Ctrl Pts',(7.25404931831883,1.23263224510378,1.78858049393525));
#146885=CARTESIAN_POINT('Ctrl Pts',(7.22624777665621,1.22830577220772,1.78147109270522));
#146886=CARTESIAN_POINT('Ctrl Pts',(7.19845925952399,1.22391046491094,1.77435366321102));
#146887=CARTESIAN_POINT('Ctrl Pts',(7.17197328713478,1.21972118100095,1.7675698524676));
#146888=CARTESIAN_POINT('Ctrl Pts',(7.14550131827908,1.21547100857743,1.76076861535022));
#146889=CARTESIAN_POINT('Ctrl Pts',(7.1190361837065,1.21115091645946,1.75398552037589));
#146890=CARTESIAN_POINT('Ctrl Pts',(7.09257038470169,1.20683071588149,1.74720225510554));
#146891=CARTESIAN_POINT('Ctrl Pts',(7.06610965831957,1.20243940500907,1.74044401924816));
#146892=CARTESIAN_POINT('Ctrl Pts',(7.0396548826297,1.19797317480768,1.73371252114897));
#146893=CARTESIAN_POINT('Ctrl Pts',(7.21872209223307,1.197203562,2.03661353051043));
#146894=CARTESIAN_POINT('Ctrl Pts',(7.32899706144694,1.261925886,1.64574685777119));
#146895=CARTESIAN_POINT('Ctrl Pts',(7.39642312066681,1.327100493,1.24525834149977));
#146896=CARTESIAN_POINT('Ctrl Pts',(7.39873673783603,1.32933685519434,1.23151621986247));
#146897=CARTESIAN_POINT('Ctrl Pts',(7.40105035500526,1.3315732173887,1.2177740982252));
#146898=CARTESIAN_POINT('Ctrl Pts',(7.038537216,1.197203562,1.738244478));
#146899=CARTESIAN_POINT('Ctrl Pts',(7.132656622,1.261925886,1.357134138));
#146900=CARTESIAN_POINT('Ctrl Pts',(7.185075021,1.327100493,0.968089328));
#146901=CARTESIAN_POINT('Ctrl Pts',(7.18687367435913,1.32933685519434,0.954739878804423));
#146902=CARTESIAN_POINT('Ctrl Pts',(7.1886723277183,1.3315732173887,0.941390429608839));
#146903=CARTESIAN_POINT('Origin',(-0.196980054139005,1.33927934730507,-0.0244706883502453));
#146904=CARTESIAN_POINT('Ctrl Pts',(7.46084690487036,1.32841655815206,0.765396519891663));
#146905=CARTESIAN_POINT('Ctrl Pts',(7.46126429393518,1.32775852557603,0.761283276945831));
#146906=CARTESIAN_POINT('Ctrl Pts',(7.46168168300001,1.327100493,0.757170034));
#146907=CARTESIAN_POINT('Ctrl Pts',(7.497765409,1.270212881,0.401575832));
#146908=CARTESIAN_POINT('Ctrl Pts',(7.499869982,1.214285714,0.044161726));
#146909=CARTESIAN_POINT('Ctrl Pts',(7.500190857,1.205758742,-0.010331651));
#146910=CARTESIAN_POINT('Ctrl Pts',(7.499719852,1.197204389,-0.064823938));
#146911=CARTESIAN_POINT('Ctrl Pts',(7.18400770487019,1.32841655815206,0.976010855747787));
#146912=CARTESIAN_POINT('Ctrl Pts',(7.18454136293509,1.32775852557603,0.972050091873894));
#146913=CARTESIAN_POINT('Ctrl Pts',(7.185075021,1.327100493,0.968089328));
#146914=CARTESIAN_POINT('Ctrl Pts',(7.23121032499999,1.270212881,0.625677103));
#146915=CARTESIAN_POINT('Ctrl Pts',(7.244574478,1.214285714,0.28042937));
#146916=CARTESIAN_POINT('Ctrl Pts',(7.246612053,1.205758742,0.227790947));
#146917=CARTESIAN_POINT('Ctrl Pts',(7.24788452,1.197204389,0.175128473));
#146918=CARTESIAN_POINT('',(7.24776860911715,1.19797317432174,0.179861575560411));
#146919=CARTESIAN_POINT('Ctrl Pts',(7.24776861100016,1.19797317454899,0.179861575570232));
#146920=CARTESIAN_POINT('Ctrl Pts',(7.24450553215528,1.21932945234802,0.311351727067775));
#146921=CARTESIAN_POINT('Ctrl Pts',(7.23766777176235,1.24060038425565,0.442707597301654));
#146922=CARTESIAN_POINT('Ctrl Pts',(7.2220225334039,1.27286180664125,0.639725279379605));
#146923=CARTESIAN_POINT('Ctrl Pts',(7.21589852742869,1.2836638529123,0.705453929640085));
#146924=CARTESIAN_POINT('Ctrl Pts',(7.20536216651482,1.29991103405708,0.803958358085943));
#146925=CARTESIAN_POINT('Ctrl Pts',(7.20162127323419,1.30533866136434,0.836805779906436));
#146926=CARTESIAN_POINT('Ctrl Pts',(7.19567175659462,1.31349012127948,0.886048324387821));
#146927=CARTESIAN_POINT('Ctrl Pts',(7.193631372977,1.31620998872371,0.902464026545407));
#146928=CARTESIAN_POINT('Ctrl Pts',(7.19048620468116,1.32029216631906,0.927079619271783));
#146929=CARTESIAN_POINT('Ctrl Pts',(7.189423513794,1.32165353799468,0.93528499327062));
#146930=CARTESIAN_POINT('Ctrl Pts',(7.18731921972352,1.32431471602432,0.951317405599425));
#146931=CARTESIAN_POINT('Ctrl Pts',(7.18679924745915,1.32497441974746,0.955292279283956));
#146932=CARTESIAN_POINT('Ctrl Pts',(7.18507502309713,1.32710049250219,0.968089323712349));
#146933=CARTESIAN_POINT('Ctrl Pts',(7.49763545644904,1.2368931917972,0.188315065585089));
#146934=CARTESIAN_POINT('Ctrl Pts',(7.4689456126465,1.23263224513807,0.187358300905372));
#146935=CARTESIAN_POINT('Ctrl Pts',(7.44026574456447,1.22830577226035,0.18639162315998));
#146936=CARTESIAN_POINT('Ctrl Pts',(7.41159687066663,1.22391046498252,0.185414304967323));
#146937=CARTESIAN_POINT('Ctrl Pts',(7.38427180671392,1.21972118106134,0.184482797081394));
#146938=CARTESIAN_POINT('Ctrl Pts',(7.35695667274409,1.21547100862243,0.183531259927491));
#146939=CARTESIAN_POINT('Ctrl Pts',(7.32965211329941,1.21115091648452,0.182595971637373));
#146940=CARTESIAN_POINT('Ctrl Pts',(7.3023468683482,1.20683071588664,0.181660659865967));
#146941=CARTESIAN_POINT('Ctrl Pts',(7.27505195801014,1.20243940502776,0.18074870167642));
#146942=CARTESIAN_POINT('Ctrl Pts',(7.24776860697027,1.19797317480768,0.179861576786875));
#146943=CARTESIAN_POINT('Ctrl Pts',(7.48749265123569,1.197203562,0.436901152368877));
#146944=CARTESIAN_POINT('Ctrl Pts',(7.51114920656008,1.261925886,0.0314815633877653));
#146945=CARTESIAN_POINT('Ctrl Pts',(7.49089190176009,1.327100493,-0.374122082468887));
#146946=CARTESIAN_POINT('Ctrl Pts',(7.4905840950171,1.32809081149028,-0.38028516973106));
#146947=CARTESIAN_POINT('Ctrl Pts',(7.49027628827411,1.32908112998057,-0.38644825699323));
#146948=CARTESIAN_POINT('Ctrl Pts',(7.247651307,1.197203562,0.184527844));
#146949=CARTESIAN_POINT('Ctrl Pts',(7.257642797,1.261925886,-0.207905238));
#146950=CARTESIAN_POINT('Ctrl Pts',(7.225202548,1.327100493,-0.599122803));
#146951=CARTESIAN_POINT('Ctrl Pts',(7.22470962322619,1.32809081149028,-0.605067295896501));
#146952=CARTESIAN_POINT('Ctrl Pts',(7.22421669845237,1.32908112998057,-0.611011788792999));
#146953=CARTESIAN_POINT('Origin',(-0.19763521706426,1.33927931706354,0.0184463046920125));
#146954=CARTESIAN_POINT('Ctrl Pts',(7.45095407682186,1.32841655815206,-0.856359568123177));
#146955=CARTESIAN_POINT('Ctrl Pts',(7.45047748191093,1.32775852557603,-0.860466372061588));
#146956=CARTESIAN_POINT('Ctrl Pts',(7.450000887,1.327100493,-0.864573176));
#146957=CARTESIAN_POINT('Ctrl Pts',(7.408798753,1.270212881,-1.219610719));
#146958=CARTESIAN_POINT('Ctrl Pts',(7.334020655,1.214285714,-1.569121102));
#146959=CARTESIAN_POINT('Ctrl Pts',(7.32261956300001,1.205758742,-1.622409433));
#146960=CARTESIAN_POINT('Ctrl Pts',(7.31044533900001,1.197204389,-1.675526468));
#146961=CARTESIAN_POINT('Ctrl Pts',(7.22586307942343,1.32841655815206,-0.591157034752268));
#146962=CARTESIAN_POINT('Ctrl Pts',(7.22553281371171,1.32775852557603,-0.595139918876134));
#146963=CARTESIAN_POINT('Ctrl Pts',(7.225202548,1.327100493,-0.599122803));
#146964=CARTESIAN_POINT('Ctrl Pts',(7.196650728,1.270212881,-0.943447347));
#146965=CARTESIAN_POINT('Ctrl Pts',(7.135484378,1.214285714,-1.283496277));
#146966=CARTESIAN_POINT('Ctrl Pts',(7.12615861,1.205758742,-1.335342062));
#146967=CARTESIAN_POINT('Ctrl Pts',(7.11608045300001,1.197204389,-1.387046859));
#146968=CARTESIAN_POINT('',(7.11698472862996,1.19797317408571,-1.3823994984479));
#146969=CARTESIAN_POINT('Ctrl Pts',(7.11698472875213,1.19797317391247,-1.382399498443));
#146970=CARTESIAN_POINT('Ctrl Pts',(7.12338474596396,1.2034230201217,-1.34945039439011));
#146971=CARTESIAN_POINT('Ctrl Pts',(7.12955124253131,1.20886077956071,-1.31648102053784));
#146972=CARTESIAN_POINT('Ctrl Pts',(7.13548437798228,1.21428571393588,-1.28349627746525));
#146973=CARTESIAN_POINT('Ctrl Pts',(7.16162230994452,1.23818480996542,-1.13818475088076));
#146974=CARTESIAN_POINT('Ctrl Pts',(7.18340750111566,1.26233313349311,-0.991572763403286));
#146975=CARTESIAN_POINT('Ctrl Pts',(7.20069910446844,1.2866659590878,-0.844057114460819));
#146976=CARTESIAN_POINT('Ctrl Pts',(7.21023990727024,1.3000918216798,-0.762663984626208));
#146977=CARTESIAN_POINT('Ctrl Pts',(7.21841350827149,1.31357377941461,-0.680996155908423));
#146978=CARTESIAN_POINT('Ctrl Pts',(7.22520254822916,1.32710049187612,-0.599122810739174));
#146979=CARTESIAN_POINT('Ctrl Pts',(7.36282707779834,1.23689319343748,-1.42785763095411));
#146980=CARTESIAN_POINT('Ctrl Pts',(7.33460231089359,1.23263224513027,-1.4226245583736));
#146981=CARTESIAN_POINT('Ctrl Pts',(7.30638515505452,1.22830577224184,-1.41740331178869));
#146982=CARTESIAN_POINT('Ctrl Pts',(7.27817644809364,1.2239104648102,-1.41219482011437));
#146983=CARTESIAN_POINT('Ctrl Pts',(7.25781973847191,1.22073860736887,-1.40843613125535));
#146984=CARTESIAN_POINT('Ctrl Pts',(7.23746645327191,1.21753001354952,-1.40468964664207));
#146985=CARTESIAN_POINT('Ctrl Pts',(7.21711934827861,1.214285714,-1.40094067785228));
#146986=CARTESIAN_POINT('Ctrl Pts',(7.21059267427628,1.21324505074959,-1.39973813346226));
#146987=CARTESIAN_POINT('Ctrl Pts',(7.20406674565574,1.21220011142664,-1.39853525699594));
#146988=CARTESIAN_POINT('Ctrl Pts',(7.19754166102725,1.21115091721806,-1.39733156272361));
#146989=CARTESIAN_POINT('Ctrl Pts',(7.17067372867402,1.2068307159293,-1.39237518619758));
#146990=CARTESIAN_POINT('Ctrl Pts',(7.14382091425827,1.20243940509642,-1.38739822438772));
#146991=CARTESIAN_POINT('Ctrl Pts',(7.11698472848221,1.19797317368262,-1.38239949983265));
#146992=CARTESIAN_POINT('Ctrl Pts',(7.40668655768148,1.197203562,-1.1826823537903));
#146993=CARTESIAN_POINT('Ctrl Pts',(7.34264875278482,1.261925886,-1.58372659622297));
#146994=CARTESIAN_POINT('Ctrl Pts',(7.23568222365081,1.327100493,-1.9755115968509));
#146995=CARTESIAN_POINT('Ctrl Pts',(7.23201183866211,1.32933685516968,-1.9889550711484));
#146996=CARTESIAN_POINT('Ctrl Pts',(7.22834145367339,1.33157321733938,-2.00239854544585));
#146997=CARTESIAN_POINT('Ctrl Pts',(7.117873279,1.197203562,-1.377817106));
#146998=CARTESIAN_POINT('Ctrl Pts',(7.043269661,1.261925886,-1.763223196));
#146999=CARTESIAN_POINT('Ctrl Pts',(6.927487635,1.327100493,-2.138320617));
#147000=CARTESIAN_POINT('Ctrl Pts',(6.92351476036686,1.32933685516968,-2.15119148375138));
#147001=CARTESIAN_POINT('Ctrl Pts',(6.91954188573374,1.33157321733938,-2.16406235050276));
#147002=CARTESIAN_POINT('Origin',(-0.189049009225389,1.3392792235055,0.0605006924093482));
#147003=CARTESIAN_POINT('Ctrl Pts',(7.09266291765338,1.32841655815206,-2.43807323536181));
#147004=CARTESIAN_POINT('Ctrl Pts',(7.09131462382669,1.32775852557603,-2.4419815706809));
#147005=CARTESIAN_POINT('Ctrl Pts',(7.08996633,1.327100493,-2.445889906));
#147006=CARTESIAN_POINT('Ctrl Pts',(6.973404903,1.270212881,-2.783769627));
#147007=CARTESIAN_POINT('Ctrl Pts',(6.825240674,1.214285714,-3.109033571));
#147008=CARTESIAN_POINT('Ctrl Pts',(6.802650717,1.205758742,-3.158625153));
#147009=CARTESIAN_POINT('Ctrl Pts',(6.779342527,1.197204389,-3.207883243));
#147010=CARTESIAN_POINT('Ctrl Pts',(6.92984512827001,1.32841655815206,-2.13068307872255));
#147011=CARTESIAN_POINT('Ctrl Pts',(6.928666381635,1.32775852557603,-2.13450184786127));
#147012=CARTESIAN_POINT('Ctrl Pts',(6.92748763500001,1.327100493,-2.138320617));
#147013=CARTESIAN_POINT('Ctrl Pts',(6.825583742,1.270212881,-2.468457247));
#147014=CARTESIAN_POINT('Ctrl Pts',(6.692746959,1.214285714,-2.787407065));
#147015=CARTESIAN_POINT('Ctrl Pts',(6.672493911,1.205758742,-2.83603596));
#147016=CARTESIAN_POINT('Ctrl Pts',(6.651536372,1.197204389,-2.884365422));
#147017=CARTESIAN_POINT('',(6.65341855209195,1.19797317421024,-2.88002110567815));
#147018=CARTESIAN_POINT('Ctrl Pts',(6.65341855208966,1.19797317415461,-2.88002110531445));
#147019=CARTESIAN_POINT('Ctrl Pts',(6.66675202366146,1.20342302010153,-2.84921814883435));
#147020=CARTESIAN_POINT('Ctrl Pts',(6.67986179183559,1.20886077946157,-2.8183451954448));
#147021=CARTESIAN_POINT('Ctrl Pts',(6.69274695873651,1.21428571388907,-2.78740706563265));
#147022=CARTESIAN_POINT('Ctrl Pts',(6.74951147156,1.23818480505845,-2.65111175178807));
#147023=CARTESIAN_POINT('Ctrl Pts',(6.80230457076466,1.26233312370905,-2.51261067121566));
#147024=CARTESIAN_POINT('Ctrl Pts',(6.85090340211003,1.28666594441934,-2.37226106832997));
#147025=CARTESIAN_POINT('Ctrl Pts',(6.87771827383148,1.30009181183023,-2.29482182764554));
#147026=CARTESIAN_POINT('Ctrl Pts',(6.90325695945089,1.31357377444449,-2.21682040196567));
#147027=CARTESIAN_POINT('Ctrl Pts',(6.92748763334545,1.32710049182833,-2.13832062464059));
#147028=CARTESIAN_POINT('Ctrl Pts',(6.88374108930052,1.2368931934011,-2.97726529110107));
#147029=CARTESIAN_POINT('Ctrl Pts',(6.85730115750648,1.23263224506685,-2.96608707433597));
#147030=CARTESIAN_POINT('Ctrl Pts',(6.83086611675,1.22830577218589,-2.95492204319668));
#147031=CARTESIAN_POINT('Ctrl Pts',(6.80443658539514,1.22391046475872,-2.94377128502051));
#147032=CARTESIAN_POINT('Ctrl Pts',(6.78536381140319,1.22073860733689,-2.93572438143839));
#147033=CARTESIAN_POINT('Ctrl Pts',(6.76629175820736,1.21753001353641,-2.92769013290503));
#147034=CARTESIAN_POINT('Ctrl Pts',(6.74722627473991,1.214285714,-2.9196547868689));
#147035=CARTESIAN_POINT('Ctrl Pts',(6.74111070209017,1.21324505072843,-2.9170773152643));
#147036=CARTESIAN_POINT('Ctrl Pts',(6.73499592878081,1.21220011138391,-2.91449967958569));
#147037=CARTESIAN_POINT('Ctrl Pts',(6.72888215553346,1.21115091715362,-2.91192142665918));
#147038=CARTESIAN_POINT('Ctrl Pts',(6.70370785482671,1.20683071586637,-2.90130511626558));
#147039=CARTESIAN_POINT('Ctrl Pts',(6.67855274380652,1.20243940503684,-2.89067195182176));
#147040=CARTESIAN_POINT('Ctrl Pts',(6.65341855208966,1.19797317415461,-2.88002110531445));
#147041=CARTESIAN_POINT('Ctrl Pts',(6.97928059608386,1.197203562,-2.74725056763781));
#147042=CARTESIAN_POINT('Ctrl Pts',(6.8305273023256,1.261925886,-3.12515238362192));
#147043=CARTESIAN_POINT('Ctrl Pts',(6.64183939663927,1.327100493,-3.48478302660899));
#147044=CARTESIAN_POINT('Ctrl Pts',(6.63536487355604,1.32933685518721,-3.49712317576157));
#147045=CARTESIAN_POINT('Ctrl Pts',(6.62889035047272,1.33157321737445,-3.50946332491413));
#147046=CARTESIAN_POINT('Ctrl Pts',(6.655271408,1.197203562,-2.87573686));
#147047=CARTESIAN_POINT('Ctrl Pts',(6.49956106400001,1.261925886,-3.236094797));
#147048=CARTESIAN_POINT('Ctrl Pts',(6.30585110000001,1.327100493,-3.577532936));
#147049=CARTESIAN_POINT('Ctrl Pts',(6.29920425303431,1.32933685518721,-3.58924883853445));
#147050=CARTESIAN_POINT('Ctrl Pts',(6.29255740606874,1.33157321737445,-3.6009647410689));
#147051=CARTESIAN_POINT('Origin',(-0.171623641713373,1.33927930011166,0.0997263771225571));
#147052=CARTESIAN_POINT('Ctrl Pts',(6.40272672408439,1.32841655815206,-3.90578530842664));
#147053=CARTESIAN_POINT('Ctrl Pts',(6.40056977604219,1.32775852557603,-3.90931242571332));
#147054=CARTESIAN_POINT('Ctrl Pts',(6.398412828,1.327100493,-3.912839543));
#147055=CARTESIAN_POINT('Ctrl Pts',(6.211942389,1.270212881,-4.217762562));
#147056=CARTESIAN_POINT('Ctrl Pts',(5.997320024,1.214285714,-4.503571086));
#147057=CARTESIAN_POINT('Ctrl Pts',(5.964597484,1.205758742,-4.547147072));
#147058=CARTESIAN_POINT('Ctrl Pts',(5.931245193,1.197204389,-4.590242963));
#147059=CARTESIAN_POINT('Ctrl Pts',(6.30979532136945,1.32841655815206,-3.57058075049654));
#147060=CARTESIAN_POINT('Ctrl Pts',(6.30782321068472,1.32775852557603,-3.57405684324827));
#147061=CARTESIAN_POINT('Ctrl Pts',(6.3058511,1.327100493,-3.577532936));
#147062=CARTESIAN_POINT('Ctrl Pts',(6.135360046,1.270212881,-3.87804483));
#147063=CARTESIAN_POINT('Ctrl Pts',(5.93706413,1.214285714,-4.160981797));
#147064=CARTESIAN_POINT('Ctrl Pts',(5.906830812,1.205758742,-4.204119968));
#147065=CARTESIAN_POINT('Ctrl Pts',(5.875973844,1.197204389,-4.246814263));
#147066=CARTESIAN_POINT('',(5.87874591871806,1.19797317422931,-4.24297612677607));
#147067=CARTESIAN_POINT('Ctrl Pts',(5.87874592077807,1.19797317443603,-4.24297612830428));
#147068=CARTESIAN_POINT('Ctrl Pts',(5.95572268929811,1.21932946232458,-4.1363229488652));
#147069=CARTESIAN_POINT('Ctrl Pts',(6.02977236921766,1.24060039083117,-4.02761342976386));
#147070=CARTESIAN_POINT('Ctrl Pts',(6.13654727984032,1.27286179973307,-3.86130099382886));
#147071=CARTESIAN_POINT('Ctrl Pts',(6.17144926667873,1.28366383961176,-3.80526881585095));
#147072=CARTESIAN_POINT('Ctrl Pts',(6.22267372412087,1.29991103381881,-3.72047372114034));
#147073=CARTESIAN_POINT('Ctrl Pts',(6.23957403768495,1.30533866114673,-3.69206022407433));
#147074=CARTESIAN_POINT('Ctrl Pts',(6.26463798703239,1.3134901210992,-3.6492580815018));
#147075=CARTESIAN_POINT('Ctrl Pts',(6.27294801147348,1.31620998855437,-3.63495486719273));
#147076=CARTESIAN_POINT('Ctrl Pts',(6.28534088684618,1.32029216616772,-3.61345518960003));
#147077=CARTESIAN_POINT('Ctrl Pts',(6.28946056677987,1.32165353784895,-3.60627983508245));
#147078=CARTESIAN_POINT('Ctrl Pts',(6.29748775538821,1.32431471587585,-3.5922430782577));
#147079=CARTESIAN_POINT('Ctrl Pts',(6.2994792991663,1.32497441927737,-3.58876403675979));
#147080=CARTESIAN_POINT('Ctrl Pts',(6.3058510974985,1.32710049205904,-3.57753294212463));
#147081=CARTESIAN_POINT('Ctrl Pts',(6.08277901777997,1.23689319179776,-4.38745933517958));
#147082=CARTESIAN_POINT('Ctrl Pts',(6.05936022279369,1.23263224511165,-4.37085865528992));
#147083=CARTESIAN_POINT('Ctrl Pts',(6.03594337023099,1.2283057722232,-4.35427190405315));
#147084=CARTESIAN_POINT('Ctrl Pts',(6.01252883073701,1.22391046493218,-4.33770027700123));
#147085=CARTESIAN_POINT('Ctrl Pts',(5.99021181229749,1.21972118100941,-4.32190541985337));
#147086=CARTESIAN_POINT('Ctrl Pts',(5.96789057786927,1.21547100856215,-4.30613251721398));
#147087=CARTESIAN_POINT('Ctrl Pts',(5.94558759502441,1.21115091644438,-4.2903530785531));
#147088=CARTESIAN_POINT('Ctrl Pts',(5.92328405224218,1.20683071586663,-4.27457324373457));
#147089=CARTESIAN_POINT('Ctrl Pts',(5.90100286981086,1.20243940501135,-4.25878107146338));
#147090=CARTESIAN_POINT('Ctrl Pts',(5.87874591645608,1.19797317447863,-4.24297612382197));
#147091=CARTESIAN_POINT('Ctrl Pts',(6.22553122981399,1.197203562,-4.18336039794212));
#147092=CARTESIAN_POINT('Ctrl Pts',(5.99901798618057,1.261925886,-4.52044951809398));
#147093=CARTESIAN_POINT('Ctrl Pts',(5.73743154150362,1.327100493,-4.83110987552457));
#147094=CARTESIAN_POINT('Ctrl Pts',(5.72845562219651,1.32933685510976,-4.84176968744128));
#147095=CARTESIAN_POINT('Ctrl Pts',(5.7194797028895,1.33157321721954,-4.85242949935788));
#147096=CARTESIAN_POINT('Ctrl Pts',(5.881476442,1.197203562,-4.239190355));
#147097=CARTESIAN_POINT('Ctrl Pts',(5.651940215,1.261925886,-4.557650202));
#147098=CARTESIAN_POINT('Ctrl Pts',(5.389359975,1.327100493,-4.84946379100001));
#147099=CARTESIAN_POINT('Ctrl Pts',(5.3803499552003,1.32933685510976,-4.85947690628512));
#147100=CARTESIAN_POINT('Ctrl Pts',(5.37133993540046,1.33157321721954,-4.86949002157024));
#147101=CARTESIAN_POINT('Origin',(-0.146172789174652,1.3392792791228,0.134288671367934));
#147102=CARTESIAN_POINT('Ctrl Pts',(5.41340614349393,1.32841655815206,-5.19086720064895));
#147103=CARTESIAN_POINT('Ctrl Pts',(5.41054139774696,1.32775852557603,-5.19384817582447));
#147104=CARTESIAN_POINT('Ctrl Pts',(5.407676652,1.327100493,-5.196829151));
#147105=CARTESIAN_POINT('Ctrl Pts',(5.160016353,1.270212881,-5.454537607));
#147106=CARTESIAN_POINT('Ctrl Pts',(4.888971356,1.214285714,-5.687526623));
#147107=CARTESIAN_POINT('Ctrl Pts',(4.847646301,1.205758742,-5.723049447));
#147108=CARTESIAN_POINT('Ctrl Pts',(4.805809426,1.197204389,-5.75796802300001));
#147109=CARTESIAN_POINT('Ctrl Pts',(5.3947064970428,1.32841655815206,-4.84352203473393));
#147110=CARTESIAN_POINT('Ctrl Pts',(5.3920332360214,1.32775852557603,-4.84649291286696));
#147111=CARTESIAN_POINT('Ctrl Pts',(5.389359975,1.327100493,-4.849463791));
#147112=CARTESIAN_POINT('Ctrl Pts',(5.158253733,1.270212881,-5.106299347));
#147113=CARTESIAN_POINT('Ctrl Pts',(4.903770781,1.214285714,-5.339993645));
#147114=CARTESIAN_POINT('Ctrl Pts',(4.86497087,1.205758742,-5.37562400000001));
#147115=CARTESIAN_POINT('Ctrl Pts',(4.825657309,1.197204389,-5.41068678999999));
#147116=CARTESIAN_POINT('',(4.82918966005797,1.19797317413119,-5.40753430064078));
#147117=CARTESIAN_POINT('Ctrl Pts',(4.82918965923873,1.1979731744789,-5.40753429774621));
#147118=CARTESIAN_POINT('Ctrl Pts',(4.866714564,1.20614195,-5.374022748));
#147119=CARTESIAN_POINT('Ctrl Pts',(4.903770781,1.214285714,-5.339993645));
#147120=CARTESIAN_POINT('Ctrl Pts',(5.1582537310117,1.2702128801536,-5.10629934886565));
#147121=CARTESIAN_POINT('Ctrl Pts',(5.38935996966452,1.32710049490569,-4.8494637968944));
#147122=CARTESIAN_POINT('Ctrl Pts',(4.99739295987831,1.2368931917972,-5.59250065744889));
#147123=CARTESIAN_POINT('Ctrl Pts',(4.97809033885803,1.23263224511286,-5.57125374342456));
#147124=CARTESIAN_POINT('Ctrl Pts',(4.95878662051537,1.2283057722275,-5.55002085012779));
#147125=CARTESIAN_POINT('Ctrl Pts',(4.93948190990829,1.22391046494225,-5.52880322466368));
#147126=CARTESIAN_POINT('Ctrl Pts',(4.92108207837026,1.21972118102846,-5.50858014325508));
#147127=CARTESIAN_POINT('Ctrl Pts',(4.90267340981734,1.21547100859722,-5.48837759677755));
#147128=CARTESIAN_POINT('Ctrl Pts',(4.88428397121444,1.21115091649139,-5.46817259061412));
#147129=CARTESIAN_POINT('Ctrl Pts',(4.8658940709274,1.20683071592559,-5.44796707718502));
#147130=CARTESIAN_POINT('Ctrl Pts',(4.84752866049305,1.20243940506542,-5.42775432148555));
#147131=CARTESIAN_POINT('Ctrl Pts',(4.82918965923873,1.1979731744789,-5.40753429774621));
#147132=CARTESIAN_POINT('Ctrl Pts',(5.18068294323111,1.197203562,-5.42386094580908));
#147133=CARTESIAN_POINT('Ctrl Pts',(4.88700125593062,1.261925886,-5.70437545777784));
#147134=CARTESIAN_POINT('Ctrl Pts',(4.56474776398113,1.327100493,-5.9515393946638));
#147135=CARTESIAN_POINT('Ctrl Pts',(4.55369015191196,1.32933685517751,-5.96002042900432));
#147136=CARTESIAN_POINT('Ctrl Pts',(4.54263253984269,1.33157321735505,-5.96850146334481));
#147137=CARTESIAN_POINT('Ctrl Pts',(4.832670174,1.197203562,-5.40442402));
#147138=CARTESIAN_POINT('Ctrl Pts',(4.540040923,1.261925886,-5.66609494900001));
#147139=CARTESIAN_POINT('Ctrl Pts',(4.220868368,1.327100493,-5.894639109));
#147140=CARTESIAN_POINT('Ctrl Pts',(4.20991647334412,1.32933685517751,-5.9024812355404));
#147141=CARTESIAN_POINT('Ctrl Pts',(4.1989645786882,1.33157321735505,-5.91032336208092));
#147142=CARTESIAN_POINT('Origin',(-0.113887131184427,1.33927922518391,0.162571745578474));
#147143=CARTESIAN_POINT('Ctrl Pts',(4.17096070925662,1.32841655815206,-6.23322991204394));
#147144=CARTESIAN_POINT('Ctrl Pts',(4.16752211812831,1.32775852557603,-6.23552535802196));
#147145=CARTESIAN_POINT('Ctrl Pts',(4.164083527,1.327100493,-6.237820804));
#147146=CARTESIAN_POINT('Ctrl Pts',(3.866813688,1.270212881,-6.436264536));
#147147=CARTESIAN_POINT('Ctrl Pts',(3.55201982,1.214285714,-6.605539735));
#147148=CARTESIAN_POINT('Ctrl Pts',(3.504024566,1.205758742,-6.63134839));
#147149=CARTESIAN_POINT('Ctrl Pts',(3.455659352,1.197204389,-6.656456899));
#147150=CARTESIAN_POINT('Ctrl Pts',(4.22736719328812,1.32841655815206,-5.88998561188718));
#147151=CARTESIAN_POINT('Ctrl Pts',(4.22411778064406,1.32775852557603,-5.89231236044358));
#147152=CARTESIAN_POINT('Ctrl Pts',(4.220868368,1.327100493,-5.894639109));
#147153=CARTESIAN_POINT('Ctrl Pts',(3.939953209,1.270212881,-6.095788982));
#147154=CARTESIAN_POINT('Ctrl Pts',(3.641182561,1.214285714,-6.269313324));
#147155=CARTESIAN_POINT('Ctrl Pts',(3.595630297,1.205758742,-6.29576982800001));
#147156=CARTESIAN_POINT('Ctrl Pts',(3.549698402,1.197204389,-6.321561615));
#147157=CARTESIAN_POINT('',(3.55382586037817,1.19797317422833,-6.31924218135152));
#147158=CARTESIAN_POINT('Ctrl Pts',(3.55382586159486,1.19797317443837,-6.31924218358456));
#147159=CARTESIAN_POINT('Ctrl Pts',(3.66847053387572,1.21932945129378,-6.25476811985903));
#147160=CARTESIAN_POINT('Ctrl Pts',(3.78132215100889,1.24060038065143,-6.18719868670361));
#147161=CARTESIAN_POINT('Ctrl Pts',(3.94806130701094,1.27286180742993,-6.08109117049854));
#147162=CARTESIAN_POINT('Ctrl Pts',(4.00326482999537,1.28366385468844,-6.04489267913147));
#147163=CARTESIAN_POINT('Ctrl Pts',(4.08535934885952,1.29991103391507,-5.98944337806926));
#147164=CARTESIAN_POINT('Ctrl Pts',(4.11262817573049,1.3053386612337,-5.97075224407891));
#147165=CARTESIAN_POINT('Ctrl Pts',(4.15334775316636,1.31349012116991,-5.94243015083713));
#147166=CARTESIAN_POINT('Ctrl Pts',(4.16689549086053,1.3162099886202,-5.932938193834));
#147167=CARTESIAN_POINT('Ctrl Pts',(4.18717044018716,1.32029216622577,-5.91862924827255));
#147168=CARTESIAN_POINT('Ctrl Pts',(4.19392221357816,1.32165353790458,-5.91384688160607));
#147169=CARTESIAN_POINT('Ctrl Pts',(4.20710137385622,1.32431471593206,-5.90447799516369));
#147170=CARTESIAN_POINT('Ctrl Pts',(4.21036966344095,1.32497441969706,-5.90215672886456));
#147171=CARTESIAN_POINT('Ctrl Pts',(4.22086836507627,1.32710049245079,-5.89463911222129));
#147172=CARTESIAN_POINT('Ctrl Pts',(3.67833436109359,1.2368931917972,-6.53604286414623));
#147173=CARTESIAN_POINT('Ctrl Pts',(3.66405048306732,1.23263224513278,-6.51114319839324));
#147174=CARTESIAN_POINT('Ctrl Pts',(3.64976251940711,1.2283057722557,-6.48625698950042));
#147175=CARTESIAN_POINT('Ctrl Pts',(3.63547030455459,1.22391046497494,-6.46138547817636));
#147176=CARTESIAN_POINT('Ctrl Pts',(3.6218480156065,1.21972118105975,-6.43767978124078));
#147177=CARTESIAN_POINT('Ctrl Pts',(3.60821268185683,1.21547100862238,-6.41399223943781));
#147178=CARTESIAN_POINT('Ctrl Pts',(3.59459665732802,1.21115091648973,-6.39030642927422));
#147179=CARTESIAN_POINT('Ctrl Pts',(3.58098029095612,1.2068307158971,-6.36662002445609));
#147180=CARTESIAN_POINT('Ctrl Pts',(3.56738939858888,1.20243940503687,-6.34293181137135));
#147181=CARTESIAN_POINT('Ctrl Pts',(3.55382585953398,1.1979731744789,-6.31924217758386));
#147182=CARTESIAN_POINT('Ctrl Pts',(3.89359167974831,1.197203562,-6.41074778369874));
#147183=CARTESIAN_POINT('Ctrl Pts',(3.54647377862539,1.261925886,-6.62157114079826));
#147184=CARTESIAN_POINT('Ctrl Pts',(3.17862145369144,1.327100493,-6.79368154768851));
#147185=CARTESIAN_POINT('Ctrl Pts',(3.16599919117411,1.3293368551031,-6.79958724024633));
#147186=CARTESIAN_POINT('Ctrl Pts',(3.15337692865672,1.33157321720621,-6.80549293280415));
#147187=CARTESIAN_POINT('Ctrl Pts',(3.55789362,1.197203562,-6.316952824));
#147188=CARTESIAN_POINT('Ctrl Pts',(3.215854364,1.261925886,-6.509599393));
#147189=CARTESIAN_POINT('Ctrl Pts',(2.855013647,1.327100493,-6.664187653));
#147190=CARTESIAN_POINT('Ctrl Pts',(2.84263197656271,1.3293368551031,-6.66949210119171));
#147191=CARTESIAN_POINT('Ctrl Pts',(2.83025030612543,1.33157321720621,-6.67479654938358));
#147192=CARTESIAN_POINT('Origin',(-0.0762763624267304,1.33927926043528,
0.183253217390437));
#147193=CARTESIAN_POINT('Ctrl Pts',(2.7334857876269,1.32841655815206,-6.98413372045931));
#147194=CARTESIAN_POINT('Ctrl Pts',(2.72963413581345,1.32775852557603,-6.98563630472966));
#147195=CARTESIAN_POINT('Ctrl Pts',(2.725782484,1.327100493,-6.987138889));
#147196=CARTESIAN_POINT('Ctrl Pts',(2.392803112,1.270212881,-7.117038888));
#147197=CARTESIAN_POINT('Ctrl Pts',(2.048979786,1.214285714,-7.214685152));
#147198=CARTESIAN_POINT('Ctrl Pts',(1.996558536,1.205758742,-7.229572853));
#147199=CARTESIAN_POINT('Ctrl Pts',(1.943926487,1.197204389,-7.243697248));
#147200=CARTESIAN_POINT('Ctrl Pts',(2.8623608976771,1.32841655815206,-6.661040007405));
#147201=CARTESIAN_POINT('Ctrl Pts',(2.85868727233855,1.32775852557603,-6.6626138302025));
#147202=CARTESIAN_POINT('Ctrl Pts',(2.855013647,1.327100493,-6.664187653));
#147203=CARTESIAN_POINT('Ctrl Pts',(2.537424852,1.270212881,-6.800246298));
#147204=CARTESIAN_POINT('Ctrl Pts',(2.208336691,1.214285714,-6.905486881));
#147205=CARTESIAN_POINT('Ctrl Pts',(2.158162048,1.205758742,-6.921532455));
#147206=CARTESIAN_POINT('Ctrl Pts',(2.107759543,1.197204389,-6.936847246));
#147207=CARTESIAN_POINT('',(2.11228911222365,1.19797317414004,-6.93546932052256));
#147208=CARTESIAN_POINT('Ctrl Pts',(2.11228911319232,1.1979731744789,-6.9354693168474));
#147209=CARTESIAN_POINT('Ctrl Pts',(2.16041693,1.20614195,-6.920811357));
#147210=CARTESIAN_POINT('Ctrl Pts',(2.208336691,1.214285714,-6.905486881));
#147211=CARTESIAN_POINT('Ctrl Pts',(2.53742484868758,1.27021288015463,-6.80024629937446));
#147212=CARTESIAN_POINT('Ctrl Pts',(2.85501363945865,1.32710049475556,-6.66418765610293));
#147213=CARTESIAN_POINT('Ctrl Pts',(2.1872809358002,1.23689319341796,-7.17396697109652));
#147214=CARTESIAN_POINT('Ctrl Pts',(2.17868369939942,1.23263224510868,-7.1465788341424));
#147215=CARTESIAN_POINT('Ctrl Pts',(2.17007957965209,1.22830577222041,-7.11920296110771));
#147216=CARTESIAN_POINT('Ctrl Pts',(2.16146814827954,1.22391046478458,-7.09184052727123));
#147217=CARTESIAN_POINT('Ctrl Pts',(2.15525374053095,1.22073860735404,-7.07209452762292));
#147218=CARTESIAN_POINT('Ctrl Pts',(2.14903015416926,1.21753001353903,-7.05235727007206));
#147219=CARTESIAN_POINT('Ctrl Pts',(2.14281165749886,1.214285714,-7.03262430918844));
#147220=CARTESIAN_POINT('Ctrl Pts',(2.14081697072266,1.21324505073512,-7.02629463208905));
#147221=CARTESIAN_POINT('Ctrl Pts',(2.13882292648665,1.21220011139562,-7.01996545799531));
#147222=CARTESIAN_POINT('Ctrl Pts',(2.13683000013097,1.21115091716963,-7.01363664650975));
#147223=CARTESIAN_POINT('Ctrl Pts',(2.12862385216706,1.2068307158552,-6.98757689606371));
#147224=CARTESIAN_POINT('Ctrl Pts',(2.12044297297646,1.20243940497546,-6.96152086016398));
#147225=CARTESIAN_POINT('Ctrl Pts',(2.11228911062145,1.19797317360287,-6.9354693220977));
#147226=CARTESIAN_POINT('Ctrl Pts',(2.42444039675648,1.197203562,-7.09787518030664));
#147227=CARTESIAN_POINT('Ctrl Pts',(2.0401171296216,1.261925886,-7.22914951711605));
#147228=CARTESIAN_POINT('Ctrl Pts',(1.64386633789125,1.327100493,-7.31815870169077));
#147229=CARTESIAN_POINT('Ctrl Pts',(1.63026962690392,1.32933685520693,-7.32121290923592));
#147230=CARTESIAN_POINT('Ctrl Pts',(1.61667291591659,1.33157321741388,-7.32426711678122));
#147231=CARTESIAN_POINT('Ctrl Pts',(2.116753915,1.197203562,-6.934107936));
#147232=CARTESIAN_POINT('Ctrl Pts',(1.741298029,1.261925886,-7.04872220500001));
#147233=CARTESIAN_POINT('Ctrl Pts',(1.355661661,1.327100493,-7.12212619));
#147234=CARTESIAN_POINT('Ctrl Pts',(1.342429166955,1.32933685520693,-7.12464493012668));
#147235=CARTESIAN_POINT('Ctrl Pts',(1.32919667290999,1.33157321741388,-7.12716367025349));
#147236=CARTESIAN_POINT('Origin',(-0.0350990746584939,1.3392792370096,0.195366164253897));
#147237=CARTESIAN_POINT('Ctrl Pts',(1.16819610908941,1.32841655815206,-7.40846719817911));
#147238=CARTESIAN_POINT('Ctrl Pts',(1.1641114955447,1.32775852557603,-7.40910666158955));
#147239=CARTESIAN_POINT('Ctrl Pts',(1.160026882,1.327100493,-7.409746125));
#147240=CARTESIAN_POINT('Ctrl Pts',(0.806907722,1.270212881,-7.465028413));
#147241=CARTESIAN_POINT('Ctrl Pts',(0.450131734,1.214285714,-7.486479909));
#147242=CARTESIAN_POINT('Ctrl Pts',(0.395735648,1.205758742,-7.489750525));
#147243=CARTESIAN_POINT('Ctrl Pts',(0.34129778,1.197204389,-7.492230364));
#147244=CARTESIAN_POINT('Ctrl Pts',(1.36351378779214,1.32841655815206,-7.12063157633199));
#147245=CARTESIAN_POINT('Ctrl Pts',(1.35958772439607,1.32775852557603,-7.12137888316599));
#147246=CARTESIAN_POINT('Ctrl Pts',(1.355661661,1.327100493,-7.12212619));
#147247=CARTESIAN_POINT('Ctrl Pts',(1.016249329,1.270212881,-7.186731656));
#147248=CARTESIAN_POINT('Ctrl Pts',(0.672231452,1.214285714,-7.218767545));
#147249=CARTESIAN_POINT('Ctrl Pts',(0.619780539,1.205758742,-7.223651918));
#147250=CARTESIAN_POINT('Ctrl Pts',(0.56726419,1.197204389,-7.227773609));
#147251=CARTESIAN_POINT('',(0.571984074779071,1.19797317419155,-7.22740162212021));
#147252=CARTESIAN_POINT('Ctrl Pts',(0.571984074867032,1.19797317412081,
-7.22740162308611));
#147253=CARTESIAN_POINT('Ctrl Pts',(0.605444369462677,1.2034230203102,-7.22475354015837));
#147254=CARTESIAN_POINT('Ctrl Pts',(0.638861721438653,1.20886077967912,
-7.22187502591681));
#147255=CARTESIAN_POINT('Ctrl Pts',(0.672231451661377,1.21428571395252,
-7.21876754508335));
#147256=CARTESIAN_POINT('Ctrl Pts',(0.819239089143573,1.23818482283999,
-7.20507779056777));
#147257=CARTESIAN_POINT('Ctrl Pts',(0.966335304119417,1.26233315949238,
-7.1868460377057));
#147258=CARTESIAN_POINT('Ctrl Pts',(1.11310007968281,1.28666599845873,-7.16404272835986));
#147259=CARTESIAN_POINT('Ctrl Pts',(1.19407878472327,1.30009184796444,-7.15146080974638));
#147260=CARTESIAN_POINT('Ctrl Pts',(1.27495641085275,1.31357379251701,-7.13748803685432));
#147261=CARTESIAN_POINT('Ctrl Pts',(1.3556616535332,1.32710049174852,-7.12212619142127));
#147262=CARTESIAN_POINT('Ctrl Pts',(0.593952685421233,1.2368931917972,-7.4764443559927));
#147263=CARTESIAN_POINT('Ctrl Pts',(0.59144408727556,1.2326322451142,-7.44784838639651));
#147264=CARTESIAN_POINT('Ctrl Pts',(0.588926130551418,1.22830577222365,
-7.41926291457609));
#147265=CARTESIAN_POINT('Ctrl Pts',(0.586398144197795,1.2239104649318,-7.39068899687834));
#147266=CARTESIAN_POINT('Ctrl Pts',(0.583988653383375,1.21972118102563,
-7.36345443838238));
#147267=CARTESIAN_POINT('Ctrl Pts',(0.581559700274736,1.2154710086013,-7.33623087966888));
#147268=CARTESIAN_POINT('Ctrl Pts',(0.579147544540276,1.21115091650039,
-7.30901700028623));
#147269=CARTESIAN_POINT('Ctrl Pts',(0.576735328246361,1.20683071593948,
-7.28180243767335));
#147270=CARTESIAN_POINT('Ctrl Pts',(0.574346991003699,1.20243940508096,
-7.25459693016565));
#147271=CARTESIAN_POINT('Ctrl Pts',(0.571984075606748,1.1979731744789,-7.22740161874848));
#147272=CARTESIAN_POINT('Ctrl Pts',(0.841924975632513,1.197203562,-7.45311382237692));
#147273=CARTESIAN_POINT('Ctrl Pts',(0.438366870731753,1.261925886,-7.49870089635555));
#147274=CARTESIAN_POINT('Ctrl Pts',(0.0322458591924727,1.327100493,-7.50044688815638));
#147275=CARTESIAN_POINT('Ctrl Pts',(0.0183104670971001,1.32933685526002,
-7.50050679906878));
#147276=CARTESIAN_POINT('Ctrl Pts',(0.00437507500172815,1.33157321752005,
-7.50056670998106));
#147277=CARTESIAN_POINT('Ctrl Pts',(0.57663715,1.197203562,-7.227031866));
#147278=CARTESIAN_POINT('Ctrl Pts',(0.185320533,1.261925886,-7.258254601));
#147279=CARTESIAN_POINT('Ctrl Pts',(-0.207079558,1.327100493,-7.247042021));
#147280=CARTESIAN_POINT('Ctrl Pts',(-0.220544138681554,1.32933685526002,
-7.2466572792746));
#147281=CARTESIAN_POINT('Ctrl Pts',(-0.234008719363109,1.33157321752005,
-7.24627253754923));
#147282=CARTESIAN_POINT('Origin',(0.00771948208620379,1.33927931000909,
0.19834381347634));
#147283=CARTESIAN_POINT('Ctrl Pts',(-0.451717121439883,1.32841655815206,
-7.48638898311077));
#147284=CARTESIAN_POINT('Ctrl Pts',(-0.455843704719942,1.32775852557603,
-7.48613542505538));
#147285=CARTESIAN_POINT('Ctrl Pts',(-0.459970288,1.327100493,-7.48588186700001));
#147286=CARTESIAN_POINT('Ctrl Pts',(-0.816717776000001,1.270212881,-7.46396150500001));
#147287=CARTESIAN_POINT('Ctrl Pts',(-1.169763977,1.214285714,-7.408215186));
#147288=CARTESIAN_POINT('Ctrl Pts',(-1.223591399,1.205758742,-7.399715786));
#147289=CARTESIAN_POINT('Ctrl Pts',(-1.277289632,1.197204389,-7.390435115));
#147290=CARTESIAN_POINT('Ctrl Pts',(-0.199089711805015,1.32841655815206,
-7.24727032571477));
#147291=CARTESIAN_POINT('Ctrl Pts',(-0.203084634902507,1.32775852557603,
-7.24715617335739));
#147292=CARTESIAN_POINT('Ctrl Pts',(-0.207079558,1.327100493,-7.247042021));
#147293=CARTESIAN_POINT('Ctrl Pts',(-0.552444884,1.270212881,-7.237173429));
#147294=CARTESIAN_POINT('Ctrl Pts',(-0.895306583,1.214285714,-7.194506663));
#147295=CARTESIAN_POINT('Ctrl Pts',(-0.947581218,1.205758742,-7.188001446));
#147296=CARTESIAN_POINT('Ctrl Pts',(-0.999755805999999,1.197204389,-7.180737311));
#147297=CARTESIAN_POINT('',(-0.995066303928726,1.19797317409232,-7.18138865723257));
#147298=CARTESIAN_POINT('Ctrl Pts',(-0.995066304282821,1.19797317433401,
-7.18138865950215));
#147299=CARTESIAN_POINT('Ctrl Pts',(-0.864780371989077,1.21932946147407,
-7.19944131181136));
#147300=CARTESIAN_POINT('Ctrl Pts',(-0.734048704424371,1.24060039054742,
-7.2139446398357));
#147301=CARTESIAN_POINT('Ctrl Pts',(-0.537095387670994,1.27286180063188,
-7.23037941102887));
#147302=CARTESIAN_POINT('Ctrl Pts',(-0.471241893446828,1.28366384129796,
-7.23496979160408));
#147303=CARTESIAN_POINT('Ctrl Pts',(-0.372330447545514,1.29991103390507,
-7.2405084779935));
#147304=CARTESIAN_POINT('Ctrl Pts',(-0.339310531179135,1.30533866123095,
-7.24213098669581));
#147305=CARTESIAN_POINT('Ctrl Pts',(-0.28975415731532,1.31349012118079,
-7.24422640291922));
#147306=CARTESIAN_POINT('Ctrl Pts',(-0.273224609628572,1.316209988635,-7.24486866327605));
#147307=CARTESIAN_POINT('Ctrl Pts',(-0.248424458125744,1.32029216624683,
-7.24574728745407));
#147308=CARTESIAN_POINT('Ctrl Pts',(-0.240155253142869,1.32165353792755,
-7.24602607766629));
#147309=CARTESIAN_POINT('Ctrl Pts',(-0.223993606449739,1.32431471596907,
-7.24654326009665));
#147310=CARTESIAN_POINT('Ctrl Pts',(-0.219986974589969,1.32497441951572,
-7.24667320063075));
#147311=CARTESIAN_POINT('Ctrl Pts',(-0.207079563538114,1.32710049222491,
-7.24704202165181));
#147312=CARTESIAN_POINT('Ctrl Pts',(-1.02714813259364,1.2368931917972,-7.42933151192617));
#147313=CARTESIAN_POINT('Ctrl Pts',(-1.02345079312789,1.23263224508648,
-7.40086482581375));
#147314=CARTESIAN_POINT('Ctrl Pts',(-1.01976484996718,1.22830577220348,
-7.37240638023503));
#147315=CARTESIAN_POINT('Ctrl Pts',(-1.01609118573003,1.22391046491851,
-7.34395706257801));
#147316=CARTESIAN_POINT('Ctrl Pts',(-1.01258971894321,1.21972118100939,
-7.31684126362269));
#147317=CARTESIAN_POINT('Ctrl Pts',(-1.00910962403246,1.21547100857855,
-7.28973202346733));
#147318=CARTESIAN_POINT('Ctrl Pts',(-1.00561520528948,1.21115091648241,
-7.26263584727502));
#147319=CARTESIAN_POINT('Ctrl Pts',(-1.00212069881583,1.20683071592629,
-7.2355389908077));
#147320=CARTESIAN_POINT('Ctrl Pts',(-0.998604818142201,1.20243940507305,
-7.20845611103345));
#147321=CARTESIAN_POINT('Ctrl Pts',(-0.995066302196114,1.1979731744789,
-7.1813886540959));
#147322=CARTESIAN_POINT('Ctrl Pts',(-0.779957922291379,1.197203562,-7.45985314609555));
#147323=CARTESIAN_POINT('Ctrl Pts',(-1.18388093561253,1.261925886,-7.41762135550114));
#147324=CARTESIAN_POINT('Ctrl Pts',(-1.58088240026032,1.327100493,-7.3320225141512));
#147325=CARTESIAN_POINT('Ctrl Pts',(-1.59450486913966,1.32933685516649,
-7.32908532712236));
#147326=CARTESIAN_POINT('Ctrl Pts',(-1.60812733801905,1.331573217333,-7.32614814009351));
#147327=CARTESIAN_POINT('Ctrl Pts',(-0.990442528,1.197203562,-7.182027819));
#147328=CARTESIAN_POINT('Ctrl Pts',(-1.379322344,1.261925886,-7.128399079));
#147329=CARTESIAN_POINT('Ctrl Pts',(-1.760137966,1.327100493,-7.033094222));
#147330=CARTESIAN_POINT('Ctrl Pts',(-1.77320504363426,1.32933685516649,
-7.02982398860254));
#147331=CARTESIAN_POINT('Ctrl Pts',(-1.78627212126847,1.33157321733301,
-7.0265537552051));
#147332=CARTESIAN_POINT('Origin',(0.0501770555670825,1.33927929947402,0.192047116197817));
#147333=CARTESIAN_POINT('Ctrl Pts',(-2.05050856186381,1.32841655815206,
-7.2142555408744));
#147334=CARTESIAN_POINT('Ctrl Pts',(-2.0544841604319,1.32775852557603,-7.2131208174372));
#147335=CARTESIAN_POINT('Ctrl Pts',(-2.058459759,1.327100493,-7.211986094));
#147336=CARTESIAN_POINT('Ctrl Pts',(-2.402154459,1.270212881,-7.11388805300001));
#147337=CARTESIAN_POINT('Ctrl Pts',(-2.734962825,1.214285714,-6.983550554));
#147338=CARTESIAN_POINT('Ctrl Pts',(-2.785704672,1.205758742,-6.963678562));
#147339=CARTESIAN_POINT('Ctrl Pts',(-2.836152401,1.197204389,-6.943071335));
#147340=CARTESIAN_POINT('Ctrl Pts',(-1.75238399671172,1.32841655815206,
-7.03503476980878));
#147341=CARTESIAN_POINT('Ctrl Pts',(-1.75626098135586,1.32775852557603,
-7.03406449590439));
#147342=CARTESIAN_POINT('Ctrl Pts',(-1.760137966,1.327100493,-7.033094222));
#147343=CARTESIAN_POINT('Ctrl Pts',(-2.095307388,1.270212881,-6.949213017));
#147344=CARTESIAN_POINT('Ctrl Pts',(-2.420981077,1.214285714,-6.833838645));
#147345=CARTESIAN_POINT('Ctrl Pts',(-2.470635131,1.205758742,-6.816248015));
#147346=CARTESIAN_POINT('Ctrl Pts',(-2.520028332,1.197204389,-6.797937717));
#147347=CARTESIAN_POINT('',(-2.515588486907,1.19797317420338,-6.79958194010459));
#147348=CARTESIAN_POINT('Ctrl Pts',(-2.51558848697322,1.1979731742374,-6.79958194026763));
#147349=CARTESIAN_POINT('Ctrl Pts',(-2.48410884521609,1.20342302033325,
-6.81122821864144));
#147350=CARTESIAN_POINT('Ctrl Pts',(-2.45257142183251,1.20886077966291,
-6.82264733217239));
#147351=CARTESIAN_POINT('Ctrl Pts',(-2.42098107736823,1.21428571399529,
-6.83383864515277));
#147352=CARTESIAN_POINT('Ctrl Pts',(-2.2818123815728,1.23818482264714,-6.88314106461257));
#147353=CARTESIAN_POINT('Ctrl Pts',(-2.1406561597672,1.2623331590456,-6.92835847082164));
#147354=CARTESIAN_POINT('Ctrl Pts',(-1.99788119768136,1.28666599770993,
-6.96928767690998));
#147355=CARTESIAN_POINT('Ctrl Pts',(-1.91910390320488,1.30009184751514,
-6.99187071299422));
#147356=CARTESIAN_POINT('Ctrl Pts',(-1.83983434093763,1.31357379235643,
-7.01314900188966));
#147357=CARTESIAN_POINT('Ctrl Pts',(-1.76013797324525,1.32710049185966,
-7.03309422063433));
#147358=CARTESIAN_POINT('Ctrl Pts',(-2.60022064565276,1.2368931917972,-7.03483138315546));
#147359=CARTESIAN_POINT('Ctrl Pts',(-2.59049025192455,1.23263224512833,
-7.00782505119041));
#147360=CARTESIAN_POINT('Ctrl Pts',(-2.58077275948662,1.22830577224818,
-6.98082431713158));
#147361=CARTESIAN_POINT('Ctrl Pts',(-2.57106922114835,1.22391046496396,
-6.95382985797731));
#147362=CARTESIAN_POINT('Ctrl Pts',(-2.56182052148295,1.21972118105618,
-6.92810072323856));
#147363=CARTESIAN_POINT('Ctrl Pts',(-2.55259410397172,1.21547100862086,
-6.90237339964068));
#147364=CARTESIAN_POINT('Ctrl Pts',(-2.5433565058699,1.2111509165129,-6.87666191378215));
#147365=CARTESIAN_POINT('Ctrl Pts',(-2.53411867584956,1.20683071594498,
-6.85094978241275));
#147366=CARTESIAN_POINT('Ctrl Pts',(-2.52486297614487,1.20243940511241,
-6.8252558957049));
#147367=CARTESIAN_POINT('Ctrl Pts',(-2.51558848481493,1.1979731744789,-6.79958193754073));
#147368=CARTESIAN_POINT('Ctrl Pts',(-2.36537085379973,1.197203562,-7.11777802662513));
#147369=CARTESIAN_POINT('Ctrl Pts',(-2.75077178539882,1.261925886,-6.9897020842389));
#147370=CARTESIAN_POINT('Ctrl Pts',(-3.12009035661124,1.327100493,-6.82076091693207));
#147371=CARTESIAN_POINT('Ctrl Pts',(-3.1327629312016,1.32933685513552,-6.81496397166328));
#147372=CARTESIAN_POINT('Ctrl Pts',(-3.14543550579188,1.33157321727106,
-6.80916702639437));
#147373=CARTESIAN_POINT('Ctrl Pts',(-2.511210214,1.197203562,-6.80120013400001));
#147374=CARTESIAN_POINT('Ctrl Pts',(-2.879469642,1.261925886,-6.665227538));
#147375=CARTESIAN_POINT('Ctrl Pts',(-3.23089428,1.327100493,-6.49028675400001));
#147376=CARTESIAN_POINT('Ctrl Pts',(-3.24295285296404,1.32933685513552,
-6.4842839415044));
#147377=CARTESIAN_POINT('Ctrl Pts',(-3.25501142592809,1.33157321727106,
-6.47828112900879));
#147378=CARTESIAN_POINT('Origin',(0.0902884086503142,1.33927920699605,0.176770638020913));
#147379=CARTESIAN_POINT('Ctrl Pts',(-3.55342050042447,1.32841655815206,
-6.60479152680991));
#147380=CARTESIAN_POINT('Ctrl Pts',(-3.55705921971224,1.32775852557603,
-6.60282869640496));
#147381=CARTESIAN_POINT('Ctrl Pts',(-3.560697939,1.327100493,-6.600865866));
#147382=CARTESIAN_POINT('Ctrl Pts',(-3.875269069,1.270212881,-6.431177102));
#147383=CARTESIAN_POINT('Ctrl Pts',(-4.172277851,1.214285714,-6.232342861));
#147384=CARTESIAN_POINT('Ctrl Pts',(-4.217561491,1.205758742,-6.202027467));
#147385=CARTESIAN_POINT('Ctrl Pts',(-4.262399835,1.197204389,-6.171057255));
#147386=CARTESIAN_POINT('Ctrl Pts',(-3.22373875465858,1.32841655815206,
-6.49384880706528));
#147387=CARTESIAN_POINT('Ctrl Pts',(-3.22731651732929,1.32775852557603,
-6.49206778053264));
#147388=CARTESIAN_POINT('Ctrl Pts',(-3.23089428,1.327100493,-6.490286754));
#147389=CARTESIAN_POINT('Ctrl Pts',(-3.540195646,1.270212881,-6.336315127));
#147390=CARTESIAN_POINT('Ctrl Pts',(-3.833453187,1.214285714,-6.153627927));
#147391=CARTESIAN_POINT('Ctrl Pts',(-3.878164891,1.205758742,-6.125774403));
#147392=CARTESIAN_POINT('Ctrl Pts',(-3.922467133,1.197204389,-6.097274111));
#147393=CARTESIAN_POINT('',(-3.91848454889701,1.19797317421983,-6.09983432791826));
#147394=CARTESIAN_POINT('Ctrl Pts',(-3.91848454655753,1.1979731744789,-6.09983432616152));
#147395=CARTESIAN_POINT('Ctrl Pts',(-3.876155517,1.20614195,-6.127026159));
#147396=CARTESIAN_POINT('Ctrl Pts',(-3.833453187,1.214285714,-6.153627927));
#147397=CARTESIAN_POINT('Ctrl Pts',(-3.54019564989936,1.27021288012461,
-6.3363151241931));
#147398=CARTESIAN_POINT('Ctrl Pts',(-3.23089428679994,1.32710049454013,
-6.49028675033807));
#147399=CARTESIAN_POINT('Ctrl Pts',(-4.05170973114006,1.2368931917972,-6.31139035819461));
#147400=CARTESIAN_POINT('Ctrl Pts',(-4.03640126539842,1.23263224511851,
-6.28710716620259));
#147401=CARTESIAN_POINT('Ctrl Pts',(-4.02110660284373,1.22830577222571,
-6.26282666784149));
#147402=CARTESIAN_POINT('Ctrl Pts',(-4.00582691709565,1.22391046493059,
-6.2385492979449));
#147403=CARTESIAN_POINT('Ctrl Pts',(-3.9912634435281,1.21972118102325,-6.21540989307704));
#147404=CARTESIAN_POINT('Ctrl Pts',(-3.9767221205835,1.21547100859937,-6.19226746695517));
#147405=CARTESIAN_POINT('Ctrl Pts',(-3.96217328298514,1.21115091647881,
-6.16914291186207));
#147406=CARTESIAN_POINT('Ctrl Pts',(-3.94762408012453,1.20683071589829,
-6.14601777620529));
#147407=CARTESIAN_POINT('Ctrl Pts',(-3.93306134734589,1.20243940503364,
-6.12291430016812));
#147408=CARTESIAN_POINT('Ctrl Pts',(-3.91848454655753,1.1979731744789,-6.09983432616152));
#147409=CARTESIAN_POINT('Ctrl Pts',(-3.84018167302787,1.197203562,-6.44288351854414));
#147410=CARTESIAN_POINT('Ctrl Pts',(-4.18903960369843,1.261925886,-6.23495211221092));
#147411=CARTESIAN_POINT('Ctrl Pts',(-4.51340635488509,1.327100493,-5.99056811976438));
#147412=CARTESIAN_POINT('Ctrl Pts',(-4.52453648009277,1.32933685518452,
-5.98218247473529));
#147413=CARTESIAN_POINT('Ctrl Pts',(-4.53566660530047,1.33157321736907,
-5.97379682970635));
#147414=CARTESIAN_POINT('Ctrl Pts',(-3.914556502,1.197203562,-6.102355889));
#147415=CARTESIAN_POINT('Ctrl Pts',(-4.24497614,1.261925886,-5.890397365));
#147416=CARTESIAN_POINT('Ctrl Pts',(-4.550577568,1.327100493,-5.64400069100001));
#147417=CARTESIAN_POINT('Ctrl Pts',(-4.56106379121753,1.32933685518452,
-5.63554598402913));
#147418=CARTESIAN_POINT('Ctrl Pts',(-4.57155001443505,1.33157321736907,
-5.62709127705826));
#147419=CARTESIAN_POINT('Origin',(0.126178134698828,1.33927923045498,0.15322871453506));
#147420=CARTESIAN_POINT('Ctrl Pts',(-4.8901784459381,1.32841655815206,-5.68649480220919));
#147421=CARTESIAN_POINT('Ctrl Pts',(-4.89331014346905,1.32775852557603,
-5.68379564460459));
#147422=CARTESIAN_POINT('Ctrl Pts',(-4.896441841,1.327100493,-5.681096487));
#147423=CARTESIAN_POINT('Ctrl Pts',(-5.167180404,1.270212881,-5.447751458));
#147424=CARTESIAN_POINT('Ctrl Pts',(-5.414501802,1.214285714,-5.189717742));
#147425=CARTESIAN_POINT('Ctrl Pts',(-5.452209822,1.205758742,-5.150376461));
#147426=CARTESIAN_POINT('Ctrl Pts',(-5.48934219,1.197204389,-5.110491397));
#147427=CARTESIAN_POINT('Ctrl Pts',(-4.5443550709688,1.32841655815206,-5.64901769170602));
#147428=CARTESIAN_POINT('Ctrl Pts',(-4.54746631948441,1.32775852557603,
-5.64650919135301));
#147429=CARTESIAN_POINT('Ctrl Pts',(-4.550577568,1.327100493,-5.64400069100001));
#147430=CARTESIAN_POINT('Ctrl Pts',(-4.819548292,1.270212881,-5.42713818300001));
#147431=CARTESIAN_POINT('Ctrl Pts',(-5.066677286,1.214285714,-5.185680407));
#147432=CARTESIAN_POINT('Ctrl Pts',(-5.104355971,1.205758742,-5.148866388));
#147433=CARTESIAN_POINT('Ctrl Pts',(-5.14149573100001,1.197204389,-5.111508744));
#147434=CARTESIAN_POINT('',(-5.138156628083,1.19797317418971,-5.11486524319787));
#147435=CARTESIAN_POINT('Ctrl Pts',(-5.13815662819914,1.1979731742527,-5.11486524329903));
#147436=CARTESIAN_POINT('Ctrl Pts',(-5.11447662531269,1.20342302023506,
-5.13865307776319));
#147437=CARTESIAN_POINT('Ctrl Pts',(-5.09064879615534,1.20886077956019,
-5.16225900494202));
#147438=CARTESIAN_POINT('Ctrl Pts',(-5.06667728625762,1.21428571394757,
-5.18568040677395));
#147439=CARTESIAN_POINT('Ctrl Pts',(-4.96107249736565,1.23818487921893,
-5.2888617335718));
#147440=CARTESIAN_POINT('Ctrl Pts',(-4.85194861090683,1.26233327307656,
-5.38917012841354));
#147441=CARTESIAN_POINT('Ctrl Pts',(-4.7395550123306,1.28666616990491,-5.48626633390387));
#147442=CARTESIAN_POINT('Ctrl Pts',(-4.67754130380628,1.30009196274881,
-5.53983963222664));
#147443=CARTESIAN_POINT('Ctrl Pts',(-4.61453298472437,1.31357385009881,
-5.59243548013358));
#147444=CARTESIAN_POINT('Ctrl Pts',(-4.55057757375112,1.32710049178363,
-5.64400068636306));
#147445=CARTESIAN_POINT('Ctrl Pts',(-5.31374537287477,1.2368931917972,-5.29283573461458));
#147446=CARTESIAN_POINT('Ctrl Pts',(-5.29357464216323,1.2326322451214,-5.27241113771948));
#147447=CARTESIAN_POINT('Ctrl Pts',(-5.27341797098529,1.2283057722396,-5.25198620429075));
#147448=CARTESIAN_POINT('Ctrl Pts',(-5.25327659895755,1.22391046495337,
-5.23156110664842));
#147449=CARTESIAN_POINT('Ctrl Pts',(-5.23407932319174,1.21972118102907,
-5.21209340447582));
#147450=CARTESIAN_POINT('Ctrl Pts',(-5.21490303063396,1.21547100857755,
-5.19261799002205));
#147451=CARTESIAN_POINT('Ctrl Pts',(-5.19572324093141,1.21115091645384,
-5.17316164412882));
#147452=CARTESIAN_POINT('Ctrl Pts',(-5.17654296970241,1.20683071587019,
-5.15370480976593));
#147453=CARTESIAN_POINT('Ctrl Pts',(-5.15735414107387,1.20243940501329,
-5.13427203714468));
#147454=CARTESIAN_POINT('Ctrl Pts',(-5.13815662496132,1.1979731744789,-5.11486524163069));
#147455=CARTESIAN_POINT('Ctrl Pts',(-5.1354298661806,1.197203562,-5.4667269377071));
#147456=CARTESIAN_POINT('Ctrl Pts',(-5.43143258568287,1.261925886,-5.1886627093742));
#147457=CARTESIAN_POINT('Ctrl Pts',(-5.69568048758388,1.327100493,-4.88026301484489));
#147458=CARTESIAN_POINT('Ctrl Pts',(-5.70474773081824,1.32933685518157,
-4.86968077361013));
#147459=CARTESIAN_POINT('Ctrl Pts',(-5.7138149740526,1.33157321736317,-4.85909853237526));
#147460=CARTESIAN_POINT('Ctrl Pts',(-5.134862478,1.197203562,-5.118172265));
#147461=CARTESIAN_POINT('Ctrl Pts',(-5.411992272,1.261925886,-4.840138759));
#147462=CARTESIAN_POINT('Ctrl Pts',(-5.657480906,1.327100493,-4.533807429));
#147463=CARTESIAN_POINT('Ctrl Pts',(-5.66590445502249,1.32933685518157,
-4.523296160379));
#147464=CARTESIAN_POINT('Ctrl Pts',(-5.67432800404486,1.33157321736317,
-4.51278489175806));
#147465=CARTESIAN_POINT('Origin',(0.156167784693459,1.3392793125037,0.122521716615214));
#147466=CARTESIAN_POINT('Ctrl Pts',(-5.99827708283658,1.32841655815206,
-4.502303900394));
#147467=CARTESIAN_POINT('Ctrl Pts',(-6.00075532391828,1.32775852557603,
-4.498994625197));
#147468=CARTESIAN_POINT('Ctrl Pts',(-6.003233565,1.327100493,-4.49568535));
#147469=CARTESIAN_POINT('Ctrl Pts',(-6.217480127,1.270212881,-4.20959501));
#147470=CARTESIAN_POINT('Ctrl Pts',(-6.403549666,1.214285714,-3.904427189));
#147471=CARTESIAN_POINT('Ctrl Pts',(-6.431918881,1.205758742,-3.857899576));
#147472=CARTESIAN_POINT('Ctrl Pts',(-6.459609006,1.197204389,-3.810964641));
#147473=CARTESIAN_POINT('Ctrl Pts',(-5.65248239434487,1.32841655815206,
-4.54004478794311));
#147474=CARTESIAN_POINT('Ctrl Pts',(-5.65498165017243,1.32775852557603,
-4.53692610847156));
#147475=CARTESIAN_POINT('Ctrl Pts',(-5.657480906,1.327100493,-4.533807429));
#147476=CARTESIAN_POINT('Ctrl Pts',(-5.873544215,1.270212881,-4.264194291));
#147477=CARTESIAN_POINT('Ctrl Pts',(-6.062989186,1.214285714,-3.975256234));
#147478=CARTESIAN_POINT('Ctrl Pts',(-6.091873039,1.205758742,-3.931203103));
#147479=CARTESIAN_POINT('Ctrl Pts',(-6.120113703,1.197204389,-3.88673491));
#147480=CARTESIAN_POINT('',(-6.11757421509193,1.19797317422572,-3.89073074390562));
#147481=CARTESIAN_POINT('Ctrl Pts',(-6.11757421698391,1.19797317448009,
-3.89073074505997));
#147482=CARTESIAN_POINT('Ctrl Pts',(-6.04698796875694,1.21932945204533,
-4.00171673013818));
#147483=CARTESIAN_POINT('Ctrl Pts',(-5.97340797643286,1.24060037954165,
-4.11074469498818));
#147484=CARTESIAN_POINT('Ctrl Pts',(-5.85842899190968,1.27286180860714,
-4.27149478000183));
#147485=CARTESIAN_POINT('Ctrl Pts',(-5.81929492630778,1.28366385684478,
-4.32465760012926));
#147486=CARTESIAN_POINT('Ctrl Pts',(-5.7594824465453,1.2999110339762,-4.4036297454828));
#147487=CARTESIAN_POINT('Ctrl Pts',(-5.73934242028341,1.30533866127671,
-4.42984666258494));
#147488=CARTESIAN_POINT('Ctrl Pts',(-5.70885735049756,1.31349012118794,
-4.46897319390663));
#147489=CARTESIAN_POINT('Ctrl Pts',(-5.69864585458784,1.31620998862927,
-4.48198717843723));
#147490=CARTESIAN_POINT('Ctrl Pts',(-5.6832602307808,1.32029216622185,-4.50145772203961));
#147491=CARTESIAN_POINT('Ctrl Pts',(-5.67811934425274,1.32165353789618,
-4.50794068123779));
#147492=CARTESIAN_POINT('Ctrl Pts',(-5.66805069280448,1.32431471591157,
-4.52059329179272));
#147493=CARTESIAN_POINT('Ctrl Pts',(-5.66555589084582,1.32497441924694,
-4.52373111528487));
#147494=CARTESIAN_POINT('Ctrl Pts',(-5.65748091102111,1.32710049205024,
-4.53380742434282));
#147495=CARTESIAN_POINT('Ctrl Pts',(-6.32731618654932,1.2368931917972,-4.02679399416497));
#147496=CARTESIAN_POINT('Ctrl Pts',(-6.30322635167544,1.23263224513509,
-4.01118302401817));
#147497=CARTESIAN_POINT('Ctrl Pts',(-6.279150175269,1.22830577224276,-3.99556870262379));
#147498=CARTESIAN_POINT('Ctrl Pts',(-6.25508890503236,1.22391046494856,
-3.97995093197957));
#147499=CARTESIAN_POINT('Ctrl Pts',(-6.23215547048253,1.21972118104266,
-3.96506522073654));
#147500=CARTESIAN_POINT('Ctrl Pts',(-6.20924087068471,1.2154710086209,-3.95016746669878));
#147501=CARTESIAN_POINT('Ctrl Pts',(-6.18632695457099,1.21115091649654,
-3.93528908736913));
#147502=CARTESIAN_POINT('Ctrl Pts',(-6.16341246318181,1.20683071591219,
-3.92041033450375));
#147503=CARTESIAN_POINT('Ctrl Pts',(-6.14049478700707,1.20243940505261,
-3.90555692044374));
#147504=CARTESIAN_POINT('Ctrl Pts',(-6.11757421157736,1.19797317447888,
-3.89073074300301));
#147505=CARTESIAN_POINT('Ctrl Pts',(-6.19055106550973,1.197203562,-4.2349522806284));
#147506=CARTESIAN_POINT('Ctrl Pts',(-6.41985781637798,1.261925886,-3.89975720421092));
#147507=CARTESIAN_POINT('Ctrl Pts',(-6.61163093231082,1.327100493,-3.54176223582509));
#147508=CARTESIAN_POINT('Ctrl Pts',(-6.61821131918263,1.32933685510004,
-3.52947821270389));
#147509=CARTESIAN_POINT('Ctrl Pts',(-6.62479170605458,1.3315732172001,-3.51719418958263));
#147510=CARTESIAN_POINT('Ctrl Pts',(-6.115067991,1.197203562,-3.894668594));
#147511=CARTESIAN_POINT('Ctrl Pts',(-6.32594966,1.261925886,-3.563560643));
#147512=CARTESIAN_POINT('Ctrl Pts',(-6.499846725,1.327100493,-3.21161837));
#147513=CARTESIAN_POINT('Ctrl Pts',(-6.50581372385702,1.32933685510004,
-3.19954203541252));
#147514=CARTESIAN_POINT('Ctrl Pts',(-6.51178072271392,1.3315732172001,-3.18746570082503));
#147515=CARTESIAN_POINT('Origin',(0.178855070989341,1.33927929116881,0.086085685520943));
#147516=CARTESIAN_POINT('Ctrl Pts',(-6.82590294932948,1.32841655815206,
-3.10759027252605));
#147517=CARTESIAN_POINT('Ctrl Pts',(-6.82761185416474,1.32775852557603,
-3.10382561776302));
#147518=CARTESIAN_POINT('Ctrl Pts',(-6.829320759,1.327100493,-3.100060963));
#147519=CARTESIAN_POINT('Ctrl Pts',(-6.977057389,1.270212881,-2.774602578));
#147520=CARTESIAN_POINT('Ctrl Pts',(-7.093174665,1.214285714,-2.436569961));
#147521=CARTESIAN_POINT('Ctrl Pts',(-7.11087856200001,1.205758742,-2.385031595));
#147522=CARTESIAN_POINT('Ctrl Pts',(-7.127831683,1.197204389,-2.333241414));
#147523=CARTESIAN_POINT('Ctrl Pts',(-6.49630592356605,1.32841655815206,
-3.21878443522406));
#147524=CARTESIAN_POINT('Ctrl Pts',(-6.49807632428302,1.32775852557603,
-3.21520140261203));
#147525=CARTESIAN_POINT('Ctrl Pts',(-6.499846725,1.327100493,-3.21161837));
#147526=CARTESIAN_POINT('Ctrl Pts',(-6.652899739,1.270212881,-2.901861412));
#147527=CARTESIAN_POINT('Ctrl Pts',(-6.775802451,1.214285714,-2.578953498));
#147528=CARTESIAN_POINT('Ctrl Pts',(-6.794540894,1.205758742,-2.52972113));
#147529=CARTESIAN_POINT('Ctrl Pts',(-6.81256196,1.197204389,-2.480221671));
#147530=CARTESIAN_POINT('',(-6.81094082973592,1.19797317417747,-2.48466999862016));
#147531=CARTESIAN_POINT('Ctrl Pts',(-6.81094083026715,1.19797317404191,
-2.48466999883739));
#147532=CARTESIAN_POINT('Ctrl Pts',(-6.7994376935698,1.20342302021377,-2.51620222837882));
#147533=CARTESIAN_POINT('Ctrl Pts',(-6.7877240128223,1.20886077960922,-2.54763143357809));
#147534=CARTESIAN_POINT('Ctrl Pts',(-6.77580245114939,1.21428571398706,
-2.57895349787104));
#147535=CARTESIAN_POINT('Ctrl Pts',(-6.72328286275153,1.23818487596032,
-2.71694061468588));
#147536=CARTESIAN_POINT('Ctrl Pts',(-6.66636311616781,1.26233326641375,
-2.85379796006965));
#147537=CARTESIAN_POINT('Ctrl Pts',(-6.60512709703676,1.28666615973806,
-2.98911291815804));
#147538=CARTESIAN_POINT('Ctrl Pts',(-6.57133981565453,1.30009195594851,
-3.06377362649663));
#147539=CARTESIAN_POINT('Ctrl Pts',(-6.5362394286992,1.313573846679,-3.13796485072405));
#147540=CARTESIAN_POINT('Ctrl Pts',(-6.49984672854157,1.32710049174616,
-3.21161836311582));
#147541=CARTESIAN_POINT('Ctrl Pts',(-7.0450287280152,1.23689319179729,-2.57246384252723));
#147542=CARTESIAN_POINT('Ctrl Pts',(-7.01814620294757,1.23263224510488,
-2.56239645050775));
#147543=CARTESIAN_POINT('Ctrl Pts',(-6.99127629662418,1.22830577222459,
-2.55232284955791));
#147544=CARTESIAN_POINT('Ctrl Pts',(-6.96442020648894,1.22391046493979,
-2.54224267560677));
#147545=CARTESIAN_POINT('Ctrl Pts',(-6.93882295490602,1.21972118102739,
-2.53263499454345));
#147546=CARTESIAN_POINT('Ctrl Pts',(-6.91324150887695,1.21547100859126,
-2.52301150334711));
#147547=CARTESIAN_POINT('Ctrl Pts',(-6.88766489559399,1.21115091647302,
-2.51340678675703));
#147548=CARTESIAN_POINT('Ctrl Pts',(-6.86208764018606,1.20683071589479,
-2.50380182903149));
#147549=CARTESIAN_POINT('Ctrl Pts',(-6.83651272154253,1.20243940503304,
-2.49422230234871));
#147550=CARTESIAN_POINT('Ctrl Pts',(-6.81094082624304,1.19797317447888,
-2.48466999852047));
#147551=CARTESIAN_POINT('Ctrl Pts',(-6.95620897777927,1.197203562,-2.80515596191497));
#147552=CARTESIAN_POINT('Ctrl Pts',(-7.10809763203512,1.261925886,-2.428503387158));
#147553=CARTESIAN_POINT('Ctrl Pts',(-7.2184288620977,1.327100493,-2.03765259113515));
#147554=CARTESIAN_POINT('Ctrl Pts',(-7.22221470149621,1.3293368552233,-2.02424117224969));
#147555=CARTESIAN_POINT('Ctrl Pts',(-7.2260005408947,1.33157321744662,-2.0108297533642));
#147556=CARTESIAN_POINT('Ctrl Pts',(-6.80933972200001,1.197203562,-2.489054549));
#147557=CARTESIAN_POINT('Ctrl Pts',(-6.94411267200001,1.261925886,-2.120354393));
#147558=CARTESIAN_POINT('Ctrl Pts',(-7.03828693500001,1.327100493,-1.739257605));
#147559=CARTESIAN_POINT('Ctrl Pts',(-7.04151837395874,1.3293368552233,-1.72618087927298));
#147560=CARTESIAN_POINT('Ctrl Pts',(-7.04474981291752,1.33157321744662,
-1.71310415354602));
#147561=CARTESIAN_POINT('Origin',(0.19317929026764,1.33927922477741,0.0456244733727038));
#147562=CARTESIAN_POINT('Ctrl Pts',(-7.33435717978959,1.32841655815206,
-1.56756917649812));
#147563=CARTESIAN_POINT('Ctrl Pts',(-7.33521684189479,1.32775852557603,
-1.56352517324906));
#147564=CARTESIAN_POINT('Ctrl Pts',(-7.336076504,1.327100493,-1.55948117));
#147565=CARTESIAN_POINT('Ctrl Pts',(-7.410395202,1.270212881,-1.209872813));
#147566=CARTESIAN_POINT('Ctrl Pts',(-7.4511307,1.214285714,-0.854781429));
#147567=CARTESIAN_POINT('Ctrl Pts',(-7.457341465,1.205758742,-0.800642187));
#147568=CARTESIAN_POINT('Ctrl Pts',(-7.462764873,1.197204389,-0.746418412));
#147569=CARTESIAN_POINT('Ctrl Pts',(-7.03636940770779,1.32841655815206,
-1.7470172992385));
#147570=CARTESIAN_POINT('Ctrl Pts',(-7.0373281713539,1.32775852557603,-1.74313745211925));
#147571=CARTESIAN_POINT('Ctrl Pts',(-7.038286935,1.327100493,-1.739257605));
#147572=CARTESIAN_POINT('Ctrl Pts',(-7.121173066,1.270212881,-1.403840719));
#147573=CARTESIAN_POINT('Ctrl Pts',(-7.171786724,1.214285714,-1.062061763));
#147574=CARTESIAN_POINT('Ctrl Pts',(-7.179503569,1.205758742,-1.009952209));
#147575=CARTESIAN_POINT('Ctrl Pts',(-7.186462392,1.197204389,-0.957736023));
#147576=CARTESIAN_POINT('',(-7.18583542174986,1.19797317417719,-0.962428846770062));
#147577=CARTESIAN_POINT('Ctrl Pts',(-7.18583542231247,1.19797317411523,
-0.962428846855556));
#147578=CARTESIAN_POINT('Ctrl Pts',(-7.18137971988736,1.20342302019982,
-0.995696704436819));
#147579=CARTESIAN_POINT('Ctrl Pts',(-7.17669624851764,1.20886077957267,
-1.02890920738066));
#147580=CARTESIAN_POINT('Ctrl Pts',(-7.17178672423234,1.21428571396036,
-1.06206176261196));
#147581=CARTESIAN_POINT('Ctrl Pts',(-7.15015817611276,1.23818486528209,
-1.20811291074965));
#147582=CARTESIAN_POINT('Ctrl Pts',(-7.12398947874848,1.26233324483327,
-1.35400660537596));
#147583=CARTESIAN_POINT('Ctrl Pts',(-7.09327385727488,1.28666612712761,
-1.49932184448164));
#147584=CARTESIAN_POINT('Ctrl Pts',(-7.0763263374022,1.30009193414236,-1.57950035900928));
#147585=CARTESIAN_POINT('Ctrl Pts',(-7.05799548418409,1.31357383577967,
-1.65950264433222));
#147586=CARTESIAN_POINT('Ctrl Pts',(-7.0382869371124,1.32710049183488,-1.7392575978799));
#147587=CARTESIAN_POINT('Ctrl Pts',(-7.43332355589694,1.23689319179771,
-0.997848140191201));
#147588=CARTESIAN_POINT('Ctrl Pts',(-7.4049053377193,1.23263224508818,-0.993795066420124));
#147589=CARTESIAN_POINT('Ctrl Pts',(-7.37649810848686,1.22830577220118,
-0.989733216274669));
#147590=CARTESIAN_POINT('Ctrl Pts',(-7.34810295942658,1.22391046490981,
-0.985661976730492));
#147591=CARTESIAN_POINT('Ctrl Pts',(-7.3210387899748,1.21972118099116,-0.981781570374163));
#147592=CARTESIAN_POINT('Ctrl Pts',(-7.29398665783928,1.21547100854749,
-0.977882325800221));
#147593=CARTESIAN_POINT('Ctrl Pts',(-7.26694328144624,1.21115091641908,
-0.974000378013044));
#147594=CARTESIAN_POINT('Ctrl Pts',(-7.23989922610388,1.20683071583071,
-0.970118332765928));
#147595=CARTESIAN_POINT('Ctrl Pts',(-7.21286291982689,1.20243940497373,
-0.966260621572256));
#147596=CARTESIAN_POINT('Ctrl Pts',(-7.18583541843957,1.19797317447885,
-0.962428847399313));
#147597=CARTESIAN_POINT('Ctrl Pts',(-7.39660228961004,1.197203562,-1.24419366777322));
#147598=CARTESIAN_POINT('Ctrl Pts',(-7.46397070148977,1.261925886,-0.843695450120498));
#147599=CARTESIAN_POINT('Ctrl Pts',(-7.48770108087841,1.327100493,-0.438264575817652));
#147600=CARTESIAN_POINT('Ctrl Pts',(-7.48851535082179,1.32933685520391,
-0.424352865025269));
#147601=CARTESIAN_POINT('Ctrl Pts',(-7.48932962076503,1.33157321740785,
-0.410441154232886));
#147602=CARTESIAN_POINT('Ctrl Pts',(-7.185214296,1.197203562,-0.967055079));
#147603=CARTESIAN_POINT('Ctrl Pts',(-7.237576694,1.261925886,-0.578002727000001));
#147604=CARTESIAN_POINT('Ctrl Pts',(-7.247624671,1.327100493,-0.185571088));
#147605=CARTESIAN_POINT('Ctrl Pts',(-7.24796945122994,1.32933685520391,
-0.17210542513716));
#147606=CARTESIAN_POINT('Ctrl Pts',(-7.24831423146002,1.33157321740785,
-0.158639762274315));
#147607=CARTESIAN_POINT('Origin',(0.198471074688573,1.33927925974612,0.00302998021384858));
#147608=CARTESIAN_POINT('Ctrl Pts',(-7.4998650209685,1.32841655815206,0.0457497107196035));
#147609=CARTESIAN_POINT('Ctrl Pts',(-7.49983524348425,1.32775852557603,
0.0498839693598018));
#147610=CARTESIAN_POINT('Ctrl Pts',(-7.499805466,1.327100493,0.054018228));
#147611=CARTESIAN_POINT('Ctrl Pts',(-7.497231171,1.270212881,0.411429259));
#147612=CARTESIAN_POINT('Ctrl Pts',(-7.460680145,1.214285714,0.766975733));
#147613=CARTESIAN_POINT('Ctrl Pts',(-7.455107369,1.205758742,0.82118436));
#147614=CARTESIAN_POINT('Ctrl Pts',(-7.448747472,1.197204389,0.875306286));
#147615=CARTESIAN_POINT('Ctrl Pts',(-7.24742007933239,1.32841655815206,
-0.193561576570007));
#147616=CARTESIAN_POINT('Ctrl Pts',(-7.24752237516619,1.32775852557603,
-0.189566332285004));
#147617=CARTESIAN_POINT('Ctrl Pts',(-7.247624671,1.327100493,-0.185571088));
#147618=CARTESIAN_POINT('Ctrl Pts',(-7.256468254,1.270212881,0.159822005));
#147619=CARTESIAN_POINT('Ctrl Pts',(-7.23242622,1.214285714,0.5044908));
#147620=CARTESIAN_POINT('Ctrl Pts',(-7.22876063600001,1.205758742,0.557040955));
#147621=CARTESIAN_POINT('Ctrl Pts',(-7.224331829,1.197204389,0.609532297));
#147622=CARTESIAN_POINT('',(-7.22472833605622,1.19797317423029,0.604814408844145));
#147623=CARTESIAN_POINT('Ctrl Pts',(-7.22472833840409,1.19797317450532,
0.604814409085507));
#147624=CARTESIAN_POINT('Ctrl Pts',(-7.23570097124237,1.21932945016343,
0.473742269969239));
#147625=CARTESIAN_POINT('Ctrl Pts',(-7.24310536311774,1.24060037865077,
0.342417143140362));
#147626=CARTESIAN_POINT('Ctrl Pts',(-7.24885319740134,1.27286180825459,
0.144862795239759));
#147627=CARTESIAN_POINT('Ctrl Pts',(-7.24987160719395,1.28366385610865,
0.0788573177664608));
#147628=CARTESIAN_POINT('Ctrl Pts',(-7.25004721285279,1.29991103404772,
-0.0202088349386995));
#147629=CARTESIAN_POINT('Ctrl Pts',(-7.24987967981377,1.30533866134997,
-0.0532681654429701));
#147630=CARTESIAN_POINT('Ctrl Pts',(-7.24928909500079,1.31349012126183,
-0.102865303901341));
#147631=CARTESIAN_POINT('Ctrl Pts',(-7.24903552177914,1.31620998870393,
-0.119405380772484));
#147632=CARTESIAN_POINT('Ctrl Pts',(-7.24857020427949,1.32029216629707,
-0.144216728339316));
#147633=CARTESIAN_POINT('Ctrl Pts',(-7.24840089990121,1.32165353797173,
-0.15248889917553));
#147634=CARTESIAN_POINT('Ctrl Pts',(-7.24804234995001,1.32431471600077,
-0.168654843025585));
#147635=CARTESIAN_POINT('Ctrl Pts',(-7.24795518524569,1.32497441954237,
-0.172662633619452));
#147636=CARTESIAN_POINT('Ctrl Pts',(-7.24762467222746,1.32710049226711,
-0.185571082492359));
#147637=CARTESIAN_POINT('Ctrl Pts',(-7.47404443578264,1.23689319179786,
0.623425831516707));
#147638=CARTESIAN_POINT('Ctrl Pts',(-7.44541932874534,1.23263224516357,
0.621275069824));
#147639=CARTESIAN_POINT('Ctrl Pts',(-7.4168030670333,1.22830577227991,0.619135241647015));
#147640=CARTESIAN_POINT('Ctrl Pts',(-7.38819658462302,1.22391046499459,
0.61700718021737));
#147641=CARTESIAN_POINT('Ctrl Pts',(-7.36093098775273,1.21972118108181,
0.614978868444404));
#147642=CARTESIAN_POINT('Ctrl Pts',(-7.33367309711137,1.21547100864985,
0.61297154213858));
#147643=CARTESIAN_POINT('Ctrl Pts',(-7.3064274758196,1.21115091651599,0.610949205513832));
#147644=CARTESIAN_POINT('Ctrl Pts',(-7.27918117050091,1.20683071592216,
0.608926818116424));
#147645=CARTESIAN_POINT('Ctrl Pts',(-7.25194766417653,1.20243940507204,
0.606882331437855));
#147646=CARTESIAN_POINT('Ctrl Pts',(-7.22472833267014,1.19797317447885,
0.604814407458392));
#147647=CARTESIAN_POINT('Ctrl Pts',(-7.49113869911298,1.197203562,0.374945738428602));
#147648=CARTESIAN_POINT('Ctrl Pts',(-7.47083679599597,1.261925886,0.780562747110606));
#147649=CARTESIAN_POINT('Ctrl Pts',(-7.40685671966889,1.327100493,1.18161620345816));
#147650=CARTESIAN_POINT('Ctrl Pts',(-7.40466134597188,1.32933685510107,
1.19537770953492));
#147651=CARTESIAN_POINT('Ctrl Pts',(-7.40246597227482,1.33157321720217,
1.20913921561166));
#147652=CARTESIAN_POINT('Ctrl Pts',(-7.225116234,1.197203562,0.600162811));
#147653=CARTESIAN_POINT('Ctrl Pts',(-7.192619674,1.261925886,0.991375703));
#147654=CARTESIAN_POINT('Ctrl Pts',(-7.118071532,1.327100493,1.376792527));
#147655=CARTESIAN_POINT('Ctrl Pts',(-7.11551353208027,1.32933685510107,
1.39001748711844));
#147656=CARTESIAN_POINT('Ctrl Pts',(-7.11295553216052,1.33157321720217,
1.40324244723689));
#147657=CARTESIAN_POINT('Origin',(0.194482044550137,1.33927923986393,-0.0397062397596998));
#147658=CARTESIAN_POINT('Ctrl Pts',(-7.31468750940415,1.32841655815206,
1.65692939362537));
#147659=CARTESIAN_POINT('Ctrl Pts',(-7.31376968470208,1.32775852557603,
1.66096059431268));
#147660=CARTESIAN_POINT('Ctrl Pts',(-7.31285186,1.327100493,1.664991795));
#147661=CARTESIAN_POINT('Ctrl Pts',(-7.233504944,1.270212881,2.013493357));
#147662=CARTESIAN_POINT('Ctrl Pts',(-7.121376478,1.214285714,2.352869961));
#147663=CARTESIAN_POINT('Ctrl Pts',(-7.104280738,1.205758742,2.404613239));
#147664=CARTESIAN_POINT('Ctrl Pts',(-7.08643491800001,1.197204389,2.456102635));
#147665=CARTESIAN_POINT('Ctrl Pts',(-7.11958944241024,1.32841655815206,
1.36894487045972));
#147666=CARTESIAN_POINT('Ctrl Pts',(-7.11883048720513,1.32775852557603,
1.37286869872986));
#147667=CARTESIAN_POINT('Ctrl Pts',(-7.118071532,1.327100493,1.376792527));
#147668=CARTESIAN_POINT('Ctrl Pts',(-7.052459052,1.270212881,1.71601163));
#147669=CARTESIAN_POINT('Ctrl Pts',(-6.954885505,1.214285714,2.047453934));
#147670=CARTESIAN_POINT('Ctrl Pts',(-6.94000889,1.205758742,2.097987503));
#147671=CARTESIAN_POINT('Ctrl Pts',(-6.924399539,1.197204389,2.148299564));
#147672=CARTESIAN_POINT('',(-6.92580098254477,1.19797317427717,2.14377721438708));
#147673=CARTESIAN_POINT('Ctrl Pts',(-6.92580098244253,1.19797317417169,
2.1437772143375));
#147674=CARTESIAN_POINT('Ctrl Pts',(-6.93572590728547,1.20342302016956,
2.11171322408074));
#147675=CARTESIAN_POINT('Ctrl Pts',(-6.94542087193241,1.20886077952329,
2.07960383451994));
#147676=CARTESIAN_POINT('Ctrl Pts',(-6.95488550517671,1.21428571404043,
2.04745393395516));
#147677=CARTESIAN_POINT('Ctrl Pts',(-6.99658133912896,1.23818491548697,
1.90581961217231));
#147678=CARTESIAN_POINT('Ctrl Pts',(-7.03409051482239,1.26233334606286,
1.76242182670478));
#147679=CARTESIAN_POINT('Ctrl Pts',(-7.06723010831685,1.28666628008868,
1.61763982428158));
#147680=CARTESIAN_POINT('Ctrl Pts',(-7.08551496087135,1.30009203653179,
1.53775599688052));
#147681=CARTESIAN_POINT('Ctrl Pts',(-7.10247034740864,1.31357388715097,
1.45745126759499));
#147682=CARTESIAN_POINT('Ctrl Pts',(-7.11807153122654,1.32710049190844,
1.3767925342273));
#147683=CARTESIAN_POINT('Ctrl Pts',(-7.16528730493939,1.2368931917972,2.21554910463667));
#147684=CARTESIAN_POINT('Ctrl Pts',(-7.13779378704583,1.23263224509684,
2.20729507488363));
#147685=CARTESIAN_POINT('Ctrl Pts',(-7.11030655738309,1.22830577220572,
2.19905362431552));
#147686=CARTESIAN_POINT('Ctrl Pts',(-7.08282634888458,1.22391046491265,
2.19082576765584));
#147687=CARTESIAN_POINT('Ctrl Pts',(-7.05663423357138,1.21972118099716,
2.18298357932519));
#147688=CARTESIAN_POINT('Ctrl Pts',(-7.03044513306688,1.21547100856121,
2.17516354243795));
#147689=CARTESIAN_POINT('Ctrl Pts',(-7.00427124181747,1.21115091643179,
2.16733148377018));
#147690=CARTESIAN_POINT('Ctrl Pts',(-6.97809669344801,1.2068307158424,2.15949922847124));
#147691=CARTESIAN_POINT('Ctrl Pts',(-6.95193939554073,1.20243940499078,
2.1516481419384));
#147692=CARTESIAN_POINT('Ctrl Pts',(-6.9258009810858,1.19797317480768,2.14377721262108));
#147693=CARTESIAN_POINT('Ctrl Pts',(-7.23539778916891,1.197203562,1.97655309987448));
#147694=CARTESIAN_POINT('Ctrl Pts',(-7.12837486615898,1.261925886,2.36832269907289));
#147695=CARTESIAN_POINT('Ctrl Pts',(-6.97967596952128,1.327100493,2.74624592302433));
#147696=CARTESIAN_POINT('Ctrl Pts',(-6.97457360543554,1.32933685508188,
2.75921375216535));
#147697=CARTESIAN_POINT('Ctrl Pts',(-6.96947124134975,1.33157321716379,
2.77218158130638));
#147698=CARTESIAN_POINT('Ctrl Pts',(-6.927179768,1.197203562,2.139317756));
#147699=CARTESIAN_POINT('Ctrl Pts',(-6.811343751,1.261925886,2.514398508));
#147700=CARTESIAN_POINT('Ctrl Pts',(-6.65568528000001,1.327100493,2.874778854));
#147701=CARTESIAN_POINT('Ctrl Pts',(-6.65034410928501,1.32933685508188,
2.88714472742753));
#147702=CARTESIAN_POINT('Ctrl Pts',(-6.64500293857002,1.33157321716379,
2.89951060085513));
#147703=CARTESIAN_POINT('Origin',(0.181399943194743,1.3392793125703,-0.0805860116453921));
#147704=CARTESIAN_POINT('Ctrl Pts',(-6.78748333890469,1.32841655815206,
3.1906328984192));
#147705=CARTESIAN_POINT('Ctrl Pts',(-6.78572038345235,1.32775852557603,
3.1943725467096));
#147706=CARTESIAN_POINT('Ctrl Pts',(-6.783957428,1.327100493,3.198112195));
#147707=CARTESIAN_POINT('Ctrl Pts',(-6.631548065,1.270212881,3.521408744));
#147708=CARTESIAN_POINT('Ctrl Pts',(-6.449085162,1.214285714,3.828746606));
#147709=CARTESIAN_POINT('Ctrl Pts',(-6.421265836,1.205758742,3.875605075));
#147710=CARTESIAN_POINT('Ctrl Pts',(-6.392768543,1.197204389,3.922054354));
#147711=CARTESIAN_POINT('Ctrl Pts',(-6.6588547166992,1.32841655815206,2.86744097718164));
#147712=CARTESIAN_POINT('Ctrl Pts',(-6.6572699983496,1.32775852557603,2.87110991559082));
#147713=CARTESIAN_POINT('Ctrl Pts',(-6.65568528,1.327100493,2.874778854));
#147714=CARTESIAN_POINT('Ctrl Pts',(-6.518684703,1.270212881,3.191962459));
#147715=CARTESIAN_POINT('Ctrl Pts',(-6.352142073,1.214285714,3.494680397));
#147716=CARTESIAN_POINT('Ctrl Pts',(-6.326750041,1.205758742,3.540834488));
#147717=CARTESIAN_POINT('Ctrl Pts',(-6.300690023,1.197204389,3.586614732));
#147718=CARTESIAN_POINT('',(-6.30303087216245,1.19797317413244,3.58249938059888));
#147719=CARTESIAN_POINT('Ctrl Pts',(-6.3030308742562,1.19797317443891,3.58249938184616));
#147720=CARTESIAN_POINT('Ctrl Pts',(-6.3680251451983,1.21932945586211,3.46814879049661));
#147721=CARTESIAN_POINT('Ctrl Pts',(-6.42988717670857,1.24060038374378,
3.35207035709678));
#147722=CARTESIAN_POINT('Ctrl Pts',(-6.51805466472989,1.2728618049945,3.17518838572025));
#147723=CARTESIAN_POINT('Ctrl Pts',(-6.54669392265111,1.28366385007748,
3.11571107208527));
#147724=CARTESIAN_POINT('Ctrl Pts',(-6.58845011078457,1.29991103381072,
3.02587476984802));
#147725=CARTESIAN_POINT('Ctrl Pts',(-6.60217931457941,1.30533866114479,
2.99580058862257));
#147726=CARTESIAN_POINT('Ctrl Pts',(-6.62246861232924,1.31349012110038,
2.9505394645095));
#147727=CARTESIAN_POINT('Ctrl Pts',(-6.62918347355876,1.31620998855811,
2.93542162458502));
#147728=CARTESIAN_POINT('Ctrl Pts',(-6.63917917732145,1.32029216617391,
2.91270807353505));
#147729=CARTESIAN_POINT('Ctrl Pts',(-6.64249891522654,1.32165353785643,
2.90512936551094));
#147730=CARTESIAN_POINT('Ctrl Pts',(-6.64896140772192,1.32431471587872,
2.8903070010599));
#147731=CARTESIAN_POINT('Ctrl Pts',(-6.65056512628387,1.32497441921909,
2.8866330304428));
#147732=CARTESIAN_POINT('Ctrl Pts',(-6.65568527803507,1.3271004920459,2.87477886015856));
#147733=CARTESIAN_POINT('Ctrl Pts',(-6.52148930321594,1.23689319179727,
3.70407576429506));
#147734=CARTESIAN_POINT('Ctrl Pts',(-6.49641294089309,1.2326322451282,3.69010441533616));
#147735=CARTESIAN_POINT('Ctrl Pts',(-6.47134001560237,1.22830577222934,
3.67614670344645));
#147736=CARTESIAN_POINT('Ctrl Pts',(-6.4462710250368,1.22391046492801,3.66220377698956));
#147737=CARTESIAN_POINT('Ctrl Pts',(-6.42237710548012,1.21972118100729,
3.64891440411775));
#147738=CARTESIAN_POINT('Ctrl Pts',(-6.39848136835551,1.21547100856151,
3.63564731287302));
#147739=CARTESIAN_POINT('Ctrl Pts',(-6.37460306918195,1.21115091643823,
3.62237175053087));
#147740=CARTESIAN_POINT('Ctrl Pts',(-6.35072417052125,1.20683071585497,
3.60909585489325));
#147741=CARTESIAN_POINT('Ctrl Pts',(-6.32686616717161,1.20243940501151,
3.59580527662948));
#147742=CARTESIAN_POINT('Ctrl Pts',(-6.30303086975239,1.1979731744788,3.58249937757813));
#147743=CARTESIAN_POINT('Ctrl Pts',(-6.64133771968192,1.197203562,3.48573903474642));
#147744=CARTESIAN_POINT('Ctrl Pts',(-6.45259804968267,1.261925886,3.84534251319514));
#147745=CARTESIAN_POINT('Ctrl Pts',(-6.22613332948749,1.327100493,4.18246423546586));
#147746=CARTESIAN_POINT('Ctrl Pts',(-6.21836255600276,1.32933685505903,
4.1940320264149));
#147747=CARTESIAN_POINT('Ctrl Pts',(-6.21059178251804,1.33157321711808,
4.20559981736393));
#147748=CARTESIAN_POINT('Ctrl Pts',(-6.305336075,1.197203562,3.57844058));
#147749=CARTESIAN_POINT('Ctrl Pts',(-6.111576965,1.261925886,3.919850833));
#147750=CARTESIAN_POINT('Ctrl Pts',(-5.882086581,1.327100493,4.238343716));
#147751=CARTESIAN_POINT('Ctrl Pts',(-5.87421198671683,1.32933685505903,
4.2492722882216));
#147752=CARTESIAN_POINT('Ctrl Pts',(-5.86633739243366,1.33157321711808,
4.26020086044316));
#147753=CARTESIAN_POINT('Origin',(0.159834875138244,1.33927926526417,-0.117697270307699));
#147754=CARTESIAN_POINT('Ctrl Pts',(-5.94290399176302,1.32841655815206,
4.57514595584754));
#147755=CARTESIAN_POINT('Ctrl Pts',(-5.94037833938151,1.32775852557603,
4.57841918992377));
#147756=CARTESIAN_POINT('Ctrl Pts',(-5.937852687,1.327100493,4.581692424));
#147757=CARTESIAN_POINT('Ctrl Pts',(-5.71950736800001,1.270212881,4.864666971));
#147758=CARTESIAN_POINT('Ctrl Pts',(-5.475241792,1.214285714,5.125595314));
#147759=CARTESIAN_POINT('Ctrl Pts',(-5.43799968,1.205758742,5.165377926));
#147760=CARTESIAN_POINT('Ctrl Pts',(-5.400183416,1.197204389,5.20461517));
#147761=CARTESIAN_POINT('Ctrl Pts',(-5.88675934464409,1.32841655815206,
4.23185872984856));
#147762=CARTESIAN_POINT('Ctrl Pts',(-5.88442296282204,1.32775852557603,
4.23510122292428));
#147763=CARTESIAN_POINT('Ctrl Pts',(-5.882086581,1.327100493,4.238343716));
#147764=CARTESIAN_POINT('Ctrl Pts',(-5.680103902,1.270212881,4.518660671));
#147765=CARTESIAN_POINT('Ctrl Pts',(-5.452379538,1.214285714,4.77849949));
#147766=CARTESIAN_POINT('Ctrl Pts',(-5.41765939300001,1.205758742,4.818115986));
#147767=CARTESIAN_POINT('Ctrl Pts',(-5.382367244,1.197204389,4.85722378));
#147768=CARTESIAN_POINT('',(-5.38553804369929,1.19797317410539,4.85370785820065));
#147769=CARTESIAN_POINT('Ctrl Pts',(-5.38553804399106,1.19797317394536,
4.85370785842864));
#147770=CARTESIAN_POINT('Ctrl Pts',(-5.40800898235996,1.20342302011357,
4.8287747357346));
#147771=CARTESIAN_POINT('Ctrl Pts',(-5.43029027688968,1.2088607795396,4.80370385279805));
#147772=CARTESIAN_POINT('Ctrl Pts',(-5.45237953797633,1.21428571399169,
4.77849949019284));
#147773=CARTESIAN_POINT('Ctrl Pts',(-5.54969238256278,1.23818492097584,
4.66746326117485));
#147774=CARTESIAN_POINT('Ctrl Pts',(-5.64394597677683,1.26233335717944,
4.55306862269188));
#147775=CARTESIAN_POINT('Ctrl Pts',(-5.73481506164025,1.28666629688152,
4.43558296187854));
#147776=CARTESIAN_POINT('Ctrl Pts',(-5.78495227115069,1.30009204775908,
4.37076000036721));
#147777=CARTESIAN_POINT('Ctrl Pts',(-5.83405962295373,1.31357389275472,
4.30499681124347));
#147778=CARTESIAN_POINT('Ctrl Pts',(-5.8820865770368,1.32710049184556,4.23834372252408));
#147779=CARTESIAN_POINT('Ctrl Pts',(-5.57275370959136,1.23689319345816,
5.01940395762015));
#147780=CARTESIAN_POINT('Ctrl Pts',(-5.55126704606301,1.23263224511414,
5.00036857440288));
#147781=CARTESIAN_POINT('Ctrl Pts',(-5.5297808073759,1.22830577223117,4.98134724825955));
#147782=CARTESIAN_POINT('Ctrl Pts',(-5.50829523230249,1.2239104648033,4.96234120710719));
#147783=CARTESIAN_POINT('Ctrl Pts',(-5.49279024607477,1.22073860736394,
4.94862556741388));
#147784=CARTESIAN_POINT('Ctrl Pts',(-5.47728190210846,1.2175300135409,4.93492215050233));
#147785=CARTESIAN_POINT('Ctrl Pts',(-5.46178013446649,1.214285714,4.92121979118411));
#147786=CARTESIAN_POINT('Ctrl Pts',(-5.45680768340001,1.2132450507382,4.91682453042089));
#147787=CARTESIAN_POINT('Ctrl Pts',(-5.45183604222682,1.21220011140555,
4.91242936939489));
#147788=CARTESIAN_POINT('Ctrl Pts',(-5.44686554586363,1.21115091718982,
4.9080339427415));
#147789=CARTESIAN_POINT('Ctrl Pts',(-5.42639884426299,1.20683071587282,
4.88993516967154));
#147790=CARTESIAN_POINT('Ctrl Pts',(-5.40595570935509,1.20243940501851,
4.87182655211498));
#147791=CARTESIAN_POINT('Ctrl Pts',(-5.38553804287434,1.19797317367453,
4.85370785966772));
#147792=CARTESIAN_POINT('Ctrl Pts',(-5.73673607986545,1.197203562,4.83193568617798));
#147793=CARTESIAN_POINT('Ctrl Pts',(-5.47510492068508,1.261925886,5.1425583858957));
#147794=CARTESIAN_POINT('Ctrl Pts',(-5.18146361388604,1.327100493,5.42311516817074));
#147795=CARTESIAN_POINT('Ctrl Pts',(-5.17138778328492,1.32933685513441,
5.43274202429333));
#147796=CARTESIAN_POINT('Ctrl Pts',(-5.16131195268384,1.33157321726885,
5.44236888041577));
#147797=CARTESIAN_POINT('Ctrl Pts',(-5.388661875,1.197203562,4.850239499));
#147798=CARTESIAN_POINT('Ctrl Pts',(-5.126039633,1.261925886,5.14201528900001));
#147799=CARTESIAN_POINT('Ctrl Pts',(-4.83344805100001,1.327100493,5.403728337));
#147800=CARTESIAN_POINT('Ctrl Pts',(-4.82340824002217,1.32933685513441,
5.41270860059607));
#147801=CARTESIAN_POINT('Ctrl Pts',(-4.81336842904435,1.33157321726885,
5.42168886419204));
#147802=CARTESIAN_POINT('Origin',(0.130796662513575,1.33927930361659,-0.149305428651654));
#147803=CARTESIAN_POINT('Ctrl Pts',(-4.82044105921187,1.32841655815206,
5.74573027284353));
#147804=CARTESIAN_POINT('Ctrl Pts',(-4.81727080660594,1.32775852557603,
5.74838403992177));
#147805=CARTESIAN_POINT('Ctrl Pts',(-4.81410055400001,1.327100493,5.751037807));
#147806=CARTESIAN_POINT('Ctrl Pts',(-4.540028864,1.270212881,5.980458777));
#147807=CARTESIAN_POINT('Ctrl Pts',(-4.2453822,1.214285714,6.182776882));
#147808=CARTESIAN_POINT('Ctrl Pts',(-4.200458702,1.205758742,6.213623445));
#147809=CARTESIAN_POINT('Ctrl Pts',(-4.155091715,1.197204389,6.243813966));
#147810=CARTESIAN_POINT('Ctrl Pts',(-4.83940564834473,1.32841655815206,
5.39839947227737));
#147811=CARTESIAN_POINT('Ctrl Pts',(-4.83642684967236,1.32775852557603,
5.40106390463868));
#147812=CARTESIAN_POINT('Ctrl Pts',(-4.83344805100001,1.327100493,5.403728337));
#147813=CARTESIAN_POINT('Ctrl Pts',(-4.575927756,1.270212881,5.634071332));
#147814=CARTESIAN_POINT('Ctrl Pts',(-4.297669796,1.214285714,5.838881257));
#147815=CARTESIAN_POINT('Ctrl Pts',(-4.255245012,1.205758742,5.870107737));
#147816=CARTESIAN_POINT('Ctrl Pts',(-4.212370955,1.197204389,5.900714443));
#147817=CARTESIAN_POINT('',(-4.21622344285429,1.19797317421792,5.89796234909753));
#147818=CARTESIAN_POINT('Ctrl Pts',(-4.21622344432245,1.19797317438231,
5.89796235119718));
#147819=CARTESIAN_POINT('Ctrl Pts',(-4.32322526032568,1.21932946512229,
5.8214709182476));
#147820=CARTESIAN_POINT('Ctrl Pts',(-4.42810978821949,1.24060039327363,
5.74209617395239));
#147821=CARTESIAN_POINT('Ctrl Pts',(-4.58239917712483,1.27286180032043,
5.61858306591172));
#147822=CARTESIAN_POINT('Ctrl Pts',(-4.63336531931438,1.28366384098551,
5.57662824920296));
#147823=CARTESIAN_POINT('Ctrl Pts',(-4.70898353566001,1.29991103378527,
5.51262796203305));
#147824=CARTESIAN_POINT('Ctrl Pts',(-4.7340716445523,1.30533866113643,5.4910981173484));
#147825=CARTESIAN_POINT('Ctrl Pts',(-4.7714903652932,1.31349012111498,5.45853948853499));
#147826=CARTESIAN_POINT('Ctrl Pts',(-4.78393242454547,1.31620998858104,
5.4476384056337));
#147827=CARTESIAN_POINT('Ctrl Pts',(-4.80254145216897,1.32029216620858,
5.43122123203128));
#147828=CARTESIAN_POINT('Ctrl Pts',(-4.80873658160936,1.32165353789512,
5.42573690466597));
#147829=CARTESIAN_POINT('Ctrl Pts',(-4.82082553029863,1.32431471593174,
5.41499802113977));
#147830=CARTESIAN_POINT('Ctrl Pts',(-4.82382368759139,1.32497441960859,
5.41233699830146));
#147831=CARTESIAN_POINT('Ctrl Pts',(-4.83344804840376,1.32710049244325,
5.40372834061765));
#147832=CARTESIAN_POINT('Ctrl Pts',(-4.36344234639536,1.2368931917972,6.10003040032343));
#147833=CARTESIAN_POINT('Ctrl Pts',(-4.34655007361735,1.23263224514028,
6.07682105633262));
#147834=CARTESIAN_POINT('Ctrl Pts',(-4.32965519414463,1.22830577224801,
6.05362553204983));
#147835=CARTESIAN_POINT('Ctrl Pts',(-4.31275767749973,1.22391046495372,
6.03044507880315));
#147836=CARTESIAN_POINT('Ctrl Pts',(-4.29665220633116,1.21972118102563,
6.00835117416118));
#147837=CARTESIAN_POINT('Ctrl Pts',(-4.28053572977284,1.21547100857371,
5.98627672859718));
#147838=CARTESIAN_POINT('Ctrl Pts',(-4.26443863631162,1.21115091646208,
5.96420191693392));
#147839=CARTESIAN_POINT('Ctrl Pts',(-4.24834113871775,1.20683071589047,
5.94212655106177));
#147840=CARTESIAN_POINT('Ctrl Pts',(-4.23226877044292,1.20243940502681,
5.92004663319214));
#147841=CARTESIAN_POINT('Ctrl Pts',(-4.21622344160552,1.19797317447889,
5.89796234547384));
#147842=CARTESIAN_POINT('Ctrl Pts',(-4.56389103632907,1.197203562,5.95219639508915));
#147843=CARTESIAN_POINT('Ctrl Pts',(-4.24160196994146,1.261925886,6.19931394307092));
#147844=CARTESIAN_POINT('Ctrl Pts',(-3.8945144191289,1.327100493,6.41018726365432));
#147845=CARTESIAN_POINT('Ctrl Pts',(-3.88260466660897,1.32933685508828,
6.41742304337422));
#147846=CARTESIAN_POINT('Ctrl Pts',(-3.87069491408911,1.33157321717659,
6.42465882309414));
#147847=CARTESIAN_POINT('Ctrl Pts',(-4.220019834,1.197203562,5.89524661));
#147848=CARTESIAN_POINT('Ctrl Pts',(-3.900814385,1.261925886,6.123744826));
#147849=CARTESIAN_POINT('Ctrl Pts',(-3.558802862,1.327100493,6.316440627));
#147850=CARTESIAN_POINT('Ctrl Pts',(-3.54706728523169,1.32933685508828,
6.3230526742952));
#147851=CARTESIAN_POINT('Ctrl Pts',(-3.53533170846331,1.33157321717659,
6.32966472159023));
#147852=CARTESIAN_POINT('Origin',(0.0956423502217701,1.33927920723841,-0.173931980984078));
#147853=CARTESIAN_POINT('Ctrl Pts',(-3.47257965967507,1.32841655815206,
6.64765062822451));
#147854=CARTESIAN_POINT('Ctrl Pts',(-3.46891304433754,1.32775852557603,
6.64956084111226));
#147855=CARTESIAN_POINT('Ctrl Pts',(-3.465246429,1.327100493,6.651471054));
#147856=CARTESIAN_POINT('Ctrl Pts',(-3.148263656,1.270212881,6.81661097799999));
#147857=CARTESIAN_POINT('Ctrl Pts',(-2.817013256,1.214285714,6.950858675));
#147858=CARTESIAN_POINT('Ctrl Pts',(-2.766508945,1.205758742,6.971326838));
#147859=CARTESIAN_POINT('Ctrl Pts',(-2.715712542,1.197204389,6.99105896000001));
#147860=CARTESIAN_POINT('Ctrl Pts',(-3.56576672243298,1.32841655815206,
6.31251705551099));
#147861=CARTESIAN_POINT('Ctrl Pts',(-3.56228479221649,1.32775852557603,
6.31447884125549));
#147862=CARTESIAN_POINT('Ctrl Pts',(-3.558802862,1.327100493,6.31644062700001));
#147863=CARTESIAN_POINT('Ctrl Pts',(-3.257786313,1.270212881,6.486039079));
#147864=CARTESIAN_POINT('Ctrl Pts',(-2.94200579,1.214285714,6.626243425));
#147865=CARTESIAN_POINT('Ctrl Pts',(-2.893860104,1.205758742,6.647619773));
#147866=CARTESIAN_POINT('Ctrl Pts',(-2.845408881,1.197204389,6.668294257));
#147867=CARTESIAN_POINT('',(-2.8497629195214,1.19797317420091,6.66643467637103));
#147868=CARTESIAN_POINT('Ctrl Pts',(-2.8497629196775,1.19797317419801,6.66643467673501));
#147869=CARTESIAN_POINT('Ctrl Pts',(-2.88062613759635,1.20342302042728,
6.65324128928377));
#147870=CARTESIAN_POINT('Ctrl Pts',(-2.91137508290018,1.20886077977041,
6.6398432452646));
#147871=CARTESIAN_POINT('Ctrl Pts',(-2.94200579033808,1.21428571409209,
6.62624342524151));
#147872=CARTESIAN_POINT('Ctrl Pts',(-3.07694694590982,1.23818483384919,
6.56633049468183));
#147873=CARTESIAN_POINT('Ctrl Pts',(-3.21052177357322,1.26233318155733,
6.50208503886017));
#147874=CARTESIAN_POINT('Ctrl Pts',(-3.34232280477992,1.28666603166305,
6.43361315836795));
#147875=CARTESIAN_POINT('Ctrl Pts',(-3.41504504490551,1.30009187023295,
6.39583326780551));
#147876=CARTESIAN_POINT('Ctrl Pts',(-3.48722739618415,1.31357380373224,
6.3567676065478));
#147877=CARTESIAN_POINT('Ctrl Pts',(-3.55880285574871,1.3271004918186,6.3164406305221));
#147878=CARTESIAN_POINT('Ctrl Pts',(-2.95010126892948,1.23689319179796,
6.89542620162164));
#147879=CARTESIAN_POINT('Ctrl Pts',(-2.93859325105436,1.23263224511884,
6.86912813973384));
#147880=CARTESIAN_POINT('Ctrl Pts',(-2.92707971648569,1.22830577223091,
6.84284301422456));
#147881=CARTESIAN_POINT('Ctrl Pts',(-2.91556036655635,1.22391046494234,
6.81657204049203));
#147882=CARTESIAN_POINT('Ctrl Pts',(-2.9045809687198,1.21972118103039,6.7915324788907));
#147883=CARTESIAN_POINT('Ctrl Pts',(-2.89358663965225,1.21547100859607,
6.76650955559761));
#147884=CARTESIAN_POINT('Ctrl Pts',(-2.88261131919966,1.2111509165027,6.74149044156448));
#147885=CARTESIAN_POINT('Ctrl Pts',(-2.87163572320136,1.20683071594937,
6.716470699403));
#147886=CARTESIAN_POINT('Ctrl Pts',(-2.86068564753189,1.20243940510623,
6.69145191373865));
#147887=CARTESIAN_POINT('Ctrl Pts',(-2.84976291926544,1.19797317447889,
6.66643467296224));
#147888=CARTESIAN_POINT('Ctrl Pts',(-3.17764352089231,1.197203562,6.79413901620443));
#147889=CARTESIAN_POINT('Ctrl Pts',(-2.80976642584269,1.261925886,6.96619647104677));
#147890=CARTESIAN_POINT('Ctrl Pts',(-2.42546205857299,1.327100493,7.09752612644195));
#147891=CARTESIAN_POINT('Ctrl Pts',(-2.41227527010536,1.32933685518884,
7.10203249309483));
#147892=CARTESIAN_POINT('Ctrl Pts',(-2.39908848163773,1.33157321737771,
7.1065388597478));
#147893=CARTESIAN_POINT('Ctrl Pts',(-2.854054357,1.197203562,6.664598542));
#147894=CARTESIAN_POINT('Ctrl Pts',(-2.493191391,1.261925886,6.81913486));
#147895=CARTESIAN_POINT('Ctrl Pts',(-2.117752007,1.327100493,6.933803173));
#147896=CARTESIAN_POINT('Ctrl Pts',(-2.10486940622604,1.32933685518884,
6.93773783239047));
#147897=CARTESIAN_POINT('Ctrl Pts',(-2.09198680545205,1.33157321737771,
6.94167249178079));
#147898=CARTESIAN_POINT('Origin',(0.0560160757373296,1.33927925412577,-0.190425938296791));
#147899=CARTESIAN_POINT('Ctrl Pts',(-1.96234429440288,1.32841655815206,
7.23873422950782));
#147900=CARTESIAN_POINT('Ctrl Pts',(-1.95835276320144,1.32775852557603,
7.23981156875392));
#147901=CARTESIAN_POINT('Ctrl Pts',(-1.954361232,1.327100493,7.240888908));
#147902=CARTESIAN_POINT('Ctrl Pts',(-1.609289139,1.270212881,7.334026025));
#147903=CARTESIAN_POINT('Ctrl Pts',(-1.256923902,1.214285714,7.393926041));
#147904=CARTESIAN_POINT('Ctrl Pts',(-1.203200304,1.205758742,7.403058737));
#147905=CARTESIAN_POINT('Ctrl Pts',(-1.14934967,1.197204389,7.411409808));
#147906=CARTESIAN_POINT('Ctrl Pts',(-2.1253965081304,1.32841655815206,6.93146835656078));
#147907=CARTESIAN_POINT('Ctrl Pts',(-2.1215742575652,1.32775852557603,6.93263576478039));
#147908=CARTESIAN_POINT('Ctrl Pts',(-2.117752007,1.327100493,6.933803173));
#147909=CARTESIAN_POINT('Ctrl Pts',(-1.787314404,1.270212881,7.034726848));
#147910=CARTESIAN_POINT('Ctrl Pts',(-1.448776863,1.214285714,7.103769816));
#147911=CARTESIAN_POINT('Ctrl Pts',(-1.397161514,1.205758742,7.114296498));
#147912=CARTESIAN_POINT('Ctrl Pts',(-1.345398651,1.197204389,7.124072043));
#147913=CARTESIAN_POINT('',(-1.35005064865986,1.19797317421996,7.12319192784027));
#147914=CARTESIAN_POINT('Ctrl Pts',(-1.35005064910984,1.19797317440035,
7.12319193037176));
#147915=CARTESIAN_POINT('Ctrl Pts',(-1.47928071219414,1.21932945282983,
7.09869909662958));
#147916=CARTESIAN_POINT('Ctrl Pts',(-1.60779992972453,1.24060038228738,
7.07070040217712));
#147917=CARTESIAN_POINT('Ctrl Pts',(-1.7996910921651,1.27286180569472,7.02338735035821));
#147918=CARTESIAN_POINT('Ctrl Pts',(-1.86356310852297,1.2836638510999,7.0067103081862));
#147919=CARTESIAN_POINT('Ctrl Pts',(-1.95906530747638,1.29991103392261,
6.98037650178806));
#147920=CARTESIAN_POINT('Ctrl Pts',(-1.99087480528982,1.30533866122108,
6.97137076754721));
#147921=CARTESIAN_POINT('Ctrl Pts',(-2.03850612946368,1.31349012112496,
6.95753306948214));
#147922=CARTESIAN_POINT('Ctrl Pts',(-2.05437548237295,1.3162099885649,6.95286379971252));
#147923=CARTESIAN_POINT('Ctrl Pts',(-2.07815797049138,1.32029216615428,
6.94577770443496));
#147924=CARTESIAN_POINT('Ctrl Pts',(-2.08608332691097,1.32165353782778,
6.94340153107818));
#147925=CARTESIAN_POINT('Ctrl Pts',(-2.10156409950636,1.32431471582199,
6.93873120222481));
#147926=CARTESIAN_POINT('Ctrl Pts',(-2.10540248571035,1.32497441912895,
6.93757501752879));
#147927=CARTESIAN_POINT('Ctrl Pts',(-2.11775200093844,1.32710049202878,
6.93380317551267));
#147928=CARTESIAN_POINT('Ctrl Pts',(-1.39881673453843,1.23689319179734,
7.3683995371008));
#147929=CARTESIAN_POINT('Ctrl Pts',(-1.39323107349378,1.23263224512494,
7.34024242578046));
#147930=CARTESIAN_POINT('Ctrl Pts',(-1.38763724397553,1.22830577224665,
7.31209676235928));
#147931=CARTESIAN_POINT('Ctrl Pts',(-1.38203469282474,1.22391046496842,
7.28396366972702));
#147932=CARTESIAN_POINT('Ctrl Pts',(-1.37669475276434,1.21972118105452,
7.2571492731554));
#147933=CARTESIAN_POINT('Ctrl Pts',(-1.3713366537356,1.21547100862847,7.23034791613787));
#147934=CARTESIAN_POINT('Ctrl Pts',(-1.36599630035224,1.21115091648819,
7.20355436555754));
#147935=CARTESIAN_POINT('Ctrl Pts',(-1.36065581289424,1.20683071588789,
7.1767601422997));
#147936=CARTESIAN_POINT('Ctrl Pts',(-1.35534004338375,1.20243940501276,
7.14997233931328));
#147937=CARTESIAN_POINT('Ctrl Pts',(-1.35005064905439,1.1979731744787,7.12319192419207));
#147938=CARTESIAN_POINT('Ctrl Pts',(-1.64281292560465,1.197203562,7.31839524783592));
#147939=CARTESIAN_POINT('Ctrl Pts',(-1.24654932631938,1.261925886,7.40734739431066));
#147940=CARTESIAN_POINT('Ctrl Pts',(-0.842997787614654,1.327100493,7.45299255686116));
#147941=CARTESIAN_POINT('Ctrl Pts',(-0.829150563903604,1.3293368550922,
7.45455879739437));
#147942=CARTESIAN_POINT('Ctrl Pts',(-0.81530334019254,1.33157321718442,
7.45612503792762));
#147943=CARTESIAN_POINT('Ctrl Pts',(-1.354636469,1.197203562,7.122321253));
#147944=CARTESIAN_POINT('Ctrl Pts',(-0.968989539,1.261925886,7.195669727));
#147945=CARTESIAN_POINT('Ctrl Pts',(-0.577677421000001,1.327100493,7.226948789));
#147946=CARTESIAN_POINT('Ctrl Pts',(-0.564250173377097,1.3293368550922,
7.22802207983758));
#147947=CARTESIAN_POINT('Ctrl Pts',(-0.550822925754192,1.33157321718442,
7.22909537067527));
#147948=CARTESIAN_POINT('Origin',(0.013770519155653,1.33927931061205,-0.198015818953889));
#147949=CARTESIAN_POINT('Ctrl Pts',(-0.360351892041104,1.32841655815206,
7.49134266211465));
#147950=CARTESIAN_POINT('Ctrl Pts',(-0.356222084520552,1.32775852557603,
7.49153675255733));
#147951=CARTESIAN_POINT('Ctrl Pts',(-0.352092277,1.327100493,7.491730843));
#147952=CARTESIAN_POINT('Ctrl Pts',(0.00493395,1.270212881,7.508510167));
#147953=CARTESIAN_POINT('Ctrl Pts',(0.361937816,1.214285714,7.491261644));
#147954=CARTESIAN_POINT('Ctrl Pts',(0.416368646,1.205758742,7.488631836));
#147955=CARTESIAN_POINT('Ctrl Pts',(0.470755515,1.197204389,7.485211369));
#147956=CARTESIAN_POINT('Ctrl Pts',(-0.585645114452639,1.32841655815206,
7.22631190105834));
#147957=CARTESIAN_POINT('Ctrl Pts',(-0.58166126772632,1.32775852557603,
7.22663034502917));
#147958=CARTESIAN_POINT('Ctrl Pts',(-0.577677420999999,1.327100493,7.226948789));
#147959=CARTESIAN_POINT('Ctrl Pts',(-0.233269659,1.270212881,7.25447860700001));
#147960=CARTESIAN_POINT('Ctrl Pts',(0.112195259,1.214285714,7.249131826));
#147961=CARTESIAN_POINT('Ctrl Pts',(0.164866796,1.205758742,7.24831662500001));
#147962=CARTESIAN_POINT('Ctrl Pts',(0.217520925,1.197204389,7.246736138));
#147963=CARTESIAN_POINT('Ctrl Pts',(0.212788489902239,1.19797317430066,
7.24687664343713));
#147964=CARTESIAN_POINT('Ctrl Pts',(0.0813144678011027,1.21932946130748,
7.25073708450024));
#147965=CARTESIAN_POINT('Ctrl Pts',(-0.0502189469217795,1.24060039265624,
7.25102081258366));
#147966=CARTESIAN_POINT('Ctrl Pts',(-0.24779461253972,1.27286180050114,
7.24606484346783));
#147967=CARTESIAN_POINT('Ctrl Pts',(-0.31375837853524,1.28366384122101,
7.24350829985415));
#147968=CARTESIAN_POINT('Ctrl Pts',(-0.412688838702702,1.29991103383973,
7.23832030978511));
#147969=CARTESIAN_POINT('Ctrl Pts',(-0.445690615054844,1.30533866118305,
7.23636322632265));
#147970=CARTESIAN_POINT('Ctrl Pts',(-0.495183041810729,1.3134901211564,
7.2330883726259));
#147971=CARTESIAN_POINT('Ctrl Pts',(-0.511685133188544,1.31620998861918,
7.23193970955356));
#147972=CARTESIAN_POINT('Ctrl Pts',(-0.536434901191604,1.3202921662431,
7.23013181516178));
#147973=CARTESIAN_POINT('Ctrl Pts',(-0.544685774288287,1.32165353792807,
7.22951491276793));
#147974=CARTESIAN_POINT('Ctrl Pts',(-0.560808598010649,1.32431471597657,
7.22828168207693));
#147975=CARTESIAN_POINT('Ctrl Pts',(-0.564805791744118,1.32497441950331,
7.22797766780088));
#147976=CARTESIAN_POINT('Ctrl Pts',(-0.577677415696369,1.32710049223466,
7.22694879015694));
#147977=CARTESIAN_POINT('Ctrl Pts',(-1.356068566,4.559946053,7.122048725));
#147978=CARTESIAN_POINT('Ctrl Pts',(-0.967605761,4.62560150099999,7.196013706));
#147979=CARTESIAN_POINT('Ctrl Pts',(-0.573402753,4.690829639,7.227289207));
#147980=CARTESIAN_POINT('Ctrl Pts',(-1.16045022,4.559946053,7.409679837));
#147981=CARTESIAN_POINT('Ctrl Pts',(-0.756298953,4.62560150099999,7.472975072));
#147982=CARTESIAN_POINT('Ctrl Pts',(-0.347661035,4.690829639,7.491937787));
#147983=CARTESIAN_POINT('',(-0.578090309697558,4.69005394722626,7.22691577233048));
#147984=CARTESIAN_POINT('Ctrl Pts',(-0.578090316489442,4.69005394650282,
7.22691577311486));
#147985=CARTESIAN_POINT('Ctrl Pts',(-0.581541766825931,4.6831682404923,
7.2683793815881));
#147986=CARTESIAN_POINT('Ctrl Pts',(-0.584975039978215,4.67644844968185,
7.30989694698229));
#147987=CARTESIAN_POINT('Ctrl Pts',(-0.591801078376235,4.66333077530932,
7.39293693911767));
#147988=CARTESIAN_POINT('Ctrl Pts',(-0.595197661045881,4.65692555576185,
7.43450584453084));
#147989=CARTESIAN_POINT('Ctrl Pts',(-0.598575746204779,4.65066950057451,
7.47607564640176));
#147990=CARTESIAN_POINT('Origin',(0.0382219043895207,4.55357680227839,-0.194944154157056));
#147991=CARTESIAN_POINT('Ctrl Pts',(-2.122659554,4.690837228,6.932302389));
#147992=CARTESIAN_POINT('Ctrl Pts',(-1.744538893,4.625180297,7.04808231200001));
#147993=CARTESIAN_POINT('Ctrl Pts',(-1.356068566,4.559946053,7.122048725));
#147994=CARTESIAN_POINT('Ctrl Pts',(-1.34263297146768,4.55768986818721,
7.12460691970628));
#147995=CARTESIAN_POINT('Ctrl Pts',(-1.32919737693536,4.55543368337429,
7.12716511441254));
#147996=CARTESIAN_POINT('Ctrl Pts',(-2.4304970474152,4.690837228,7.09581366670855));
#147997=CARTESIAN_POINT('Ctrl Pts',(-2.04345770499716,4.625180297,7.22838450695184));
#147998=CARTESIAN_POINT('Ctrl Pts',(-1.64429532972506,4.559946053,7.31807217462192));
#147999=CARTESIAN_POINT('Ctrl Pts',(-1.63048994111758,4.55768986818721,
7.32117410301548));
#148000=CARTESIAN_POINT('Ctrl Pts',(-1.6166845525101,4.55543368337429,7.32427603140891));
#148001=CARTESIAN_POINT('',(-2.11814814960832,4.69005394728041,6.93368216963888));
#148002=CARTESIAN_POINT('Origin',(0.0590761079533894,4.69642264267046,-0.189672411948689));
#148003=CARTESIAN_POINT('Ctrl Pts',(-2.19171665082087,4.6506695006115,7.17261306095222));
#148004=CARTESIAN_POINT('Ctrl Pts',(-2.17948126558908,4.65692555540451,
7.13274132882446));
#148005=CARTESIAN_POINT('Ctrl Pts',(-2.16722800709513,4.66333077501547,
7.09287444557865));
#148006=CARTESIAN_POINT('Ctrl Pts',(-2.14271041380535,4.67644844946209,
7.01324327791012));
#148007=CARTESIAN_POINT('Ctrl Pts',(-2.13043235929365,4.6831682402748,6.97343442208798));
#148008=CARTESIAN_POINT('Ctrl Pts',(-2.11814815155723,4.69005394634728,
6.93368216887499));
#148009=CARTESIAN_POINT('Ctrl Pts',(-2.855394386,4.559946053,6.664024527));
#148010=CARTESIAN_POINT('Ctrl Pts',(-2.491913911,4.625601501,6.819768268));
#148011=CARTESIAN_POINT('Ctrl Pts',(-2.113650457,4.690829639,6.93505456));
#148012=CARTESIAN_POINT('Ctrl Pts',(-2.726181675,4.559946053,6.986983146));
#148013=CARTESIAN_POINT('Ctrl Pts',(-2.345085845,4.62560150099999,7.135679149));
#148014=CARTESIAN_POINT('Ctrl Pts',(-1.950078078,4.690829639,7.24204359900001));
#148015=CARTESIAN_POINT('Origin',(0.0792368453391867,4.55357610284578,-0.182173073954132));
#148016=CARTESIAN_POINT('Ctrl Pts',(-3.563273049,4.690837228,6.313919953));
#148017=CARTESIAN_POINT('Ctrl Pts',(-3.2188819,4.625180297,6.508277771));
#148018=CARTESIAN_POINT('Ctrl Pts',(-2.855394386,4.559946053,6.664024527));
#148019=CARTESIAN_POINT('Ctrl Pts',(-2.84282284356996,4.55768986802873,
6.66941116856532));
#148020=CARTESIAN_POINT('Ctrl Pts',(-2.83025130113985,4.55543368305734,
6.67479781013075));
#148021=CARTESIAN_POINT('Ctrl Pts',(-3.89906356435433,4.690837228,6.40743246670585));
#148022=CARTESIAN_POINT('Ctrl Pts',(-3.54957179938072,4.625180297,6.62010589188558));
#148023=CARTESIAN_POINT('Ctrl Pts',(-3.17902181502321,4.559946053,6.7935048240134));
#148024=CARTESIAN_POINT('Ctrl Pts',(-3.16620601070701,4.55768986802873,
6.79950198195862));
#148025=CARTESIAN_POINT('Ctrl Pts',(-3.15339020639086,4.55543368305734,
6.8054991399038));
#148026=CARTESIAN_POINT('',(-3.55916373143488,4.69005394733074,6.31623729381741));
#148027=CARTESIAN_POINT('Origin',(0.0984688797849448,4.69642269253522,-0.172538298857151));
#148028=CARTESIAN_POINT('Ctrl Pts',(-3.68237532007636,4.65066950063932,
6.53376706035625));
#148029=CARTESIAN_POINT('Ctrl Pts',(-3.66185475179114,4.65692555415041,
6.49745776078882));
#148030=CARTESIAN_POINT('Ctrl Pts',(-3.64131776398155,4.66333077444185,
6.46115702742171));
#148031=CARTESIAN_POINT('Ctrl Pts',(-3.60025502954068,4.67644844950924,
6.38865814667701));
#148032=CARTESIAN_POINT('Ctrl Pts',(-3.57970630213485,4.68316824029048,
6.35241941876875));
#148033=CARTESIAN_POINT('Ctrl Pts',(-3.55916373320053,4.69005394637357,
6.31623729263279));
#148034=CARTESIAN_POINT('Ctrl Pts',(-4.221205138,4.559946053,5.894397949));
#148035=CARTESIAN_POINT('Ctrl Pts',(-3.899702935,4.625601501,6.124638046));
#148036=CARTESIAN_POINT('Ctrl Pts',(-3.555066216,4.690829639,6.318544469));
#148037=CARTESIAN_POINT('Ctrl Pts',(-4.164439905,4.559946053,6.237582888));
#148038=CARTESIAN_POINT('Ctrl Pts',(-3.824219129,4.62560150099999,6.464726799));
#148039=CARTESIAN_POINT('Ctrl Pts',(-3.461311636,4.690829639,6.653519501));
#148040=CARTESIAN_POINT('Origin',(0.116546219047508,4.55357609998137,-0.160880490426645));
#148041=CARTESIAN_POINT('Ctrl Pts',(-4.837271857,4.690837228,5.400305637));
#148042=CARTESIAN_POINT('Ctrl Pts',(-4.54271356700001,4.625180297,5.664153394));
#148043=CARTESIAN_POINT('Ctrl Pts',(-4.221205138,4.559946053,5.894397949));
#148044=CARTESIAN_POINT('Ctrl Pts',(-4.21008548002964,4.55768986804247,
5.90236116386531));
#148045=CARTESIAN_POINT('Ctrl Pts',(-4.19896582205929,4.55543368308483,
5.91032437873072));
#148046=CARTESIAN_POINT('Ctrl Pts',(-5.18531420308181,4.690837228,5.41944684537354));
#148047=CARTESIAN_POINT('Ctrl Pts',(-4.8897118604343,4.625180297,5.70227848261148));
#148048=CARTESIAN_POINT('Ctrl Pts',(-4.56510077445871,4.559946053,5.95128073642111));
#148049=CARTESIAN_POINT('Ctrl Pts',(-4.55387380830834,4.55768986804247,
5.95989270315809));
#148050=CARTESIAN_POINT('Ctrl Pts',(-4.54264684215807,4.55543368308483,
5.9685046698951));
#148051=CARTESIAN_POINT('',(-4.83375677188436,4.69005394729794,5.40345218106921));
#148052=CARTESIAN_POINT('Origin',(0.133257365750999,4.6964226808519,-0.147336525368674));
#148053=CARTESIAN_POINT('Ctrl Pts',(-5.00085021302195,4.65066950061665,
5.58940937375438));
#148054=CARTESIAN_POINT('Ctrl Pts',(-4.97300397526571,4.65692555475222,
5.55836027793321));
#148055=CARTESIAN_POINT('Ctrl Pts',(-4.94514354744579,4.66333077475262,
5.52732308234134));
#148056=CARTESIAN_POINT('Ctrl Pts',(-4.8894557215615,4.6764484495377,5.46534646051497));
#148057=CARTESIAN_POINT('Ctrl Pts',(-4.86159715617397,4.68316824040816,
5.43437234245755));
#148058=CARTESIAN_POINT('Ctrl Pts',(-4.83375677343035,4.69005394646861,
5.40345217949458));
#148059=CARTESIAN_POINT('Ctrl Pts',(-5.38963703,4.559946053,4.849155874));
#148060=CARTESIAN_POINT('Ctrl Pts',(-5.125146184,4.625601501,5.143126555));
#148061=CARTESIAN_POINT('Ctrl Pts',(-4.830251029,4.690829639,5.406586261));
#148062=CARTESIAN_POINT('Ctrl Pts',(-5.407973553,4.559946053,5.196520186));
#148063=CARTESIAN_POINT('Ctrl Pts',(-5.124536177,4.62560150099999,5.491491009));
#148064=CARTESIAN_POINT('Ctrl Pts',(-4.81069811,4.690829639,5.753884227));
#148065=CARTESIAN_POINT('Origin',(0.148405940700649,4.55357613816343,-0.132065186293442));
#148066=CARTESIAN_POINT('Ctrl Pts',(-5.88508521,4.690837228,4.234179032));
#148067=CARTESIAN_POINT('Ctrl Pts',(-5.65413299700001,4.625180297,4.5551795));
#148068=CARTESIAN_POINT('Ctrl Pts',(-5.38963702999999,4.559946053,4.849155874));
#148069=CARTESIAN_POINT('Ctrl Pts',(-5.38048919998591,4.55768986821966,
4.85932331030542));
#148070=CARTESIAN_POINT('Ctrl Pts',(-5.37134136997195,4.55543368343922,
4.86949074661071));
#148071=CARTESIAN_POINT('Ctrl Pts',(-6.22910531267341,4.690837228,4.17805391238254));
#148072=CARTESIAN_POINT('Ctrl Pts',(-6.00121443024345,4.625180297,4.51781886922404));
#148073=CARTESIAN_POINT('Ctrl Pts',(-5.73772069546451,4.559946053,4.83078137711897));
#148074=CARTESIAN_POINT('Ctrl Pts',(-5.72860752854982,4.55768986821967,
4.84160546587721));
#148075=CARTESIAN_POINT('Ctrl Pts',(-5.71949436163511,4.55543368343922,
4.85242955463548));
#148076=CARTESIAN_POINT('',(-5.8823287196018,4.69005394733027,4.23800765141649));
#148077=CARTESIAN_POINT('Origin',(0.161815073408853,4.69642264836266,-0.115245659539057));
#148078=CARTESIAN_POINT('Ctrl Pts',(-6.08549090773312,4.6506695005771,4.38369711687511));
#148079=CARTESIAN_POINT('Ctrl Pts',(-6.05162106171909,4.65692555473231,
4.35936004960284));
#148080=CARTESIAN_POINT('Ctrl Pts',(-6.01773991589036,4.663330774701,4.33503765500821));
#148081=CARTESIAN_POINT('Ctrl Pts',(-5.95003089877631,4.67644844951874,
4.2864812486659));
#148082=CARTESIAN_POINT('Ctrl Pts',(-5.91616513215525,4.68316824025294,
4.26222005696167));
#148083=CARTESIAN_POINT('Ctrl Pts',(-5.88232872077917,4.69005394638316,
4.23800764950179));
#148084=CARTESIAN_POINT('Ctrl Pts',(-6.306055484,4.559946053,3.577172659));
#148085=CARTESIAN_POINT('Ctrl Pts',(-6.110943294,4.625601501,3.921128183));
#148086=CARTESIAN_POINT('Ctrl Pts',(-5.879578673,4.690829639,4.241822088));
#148087=CARTESIAN_POINT('Ctrl Pts',(-6.398636369,4.559946053,3.912473977));
#148088=CARTESIAN_POINT('Ctrl Pts',(-6.185235608,4.62560150099999,4.261479203));
#148089=CARTESIAN_POINT('Ctrl Pts',(-5.935141687,4.690829639,4.585203721));
#148090=CARTESIAN_POINT('Origin',(0.173326479962918,4.55357612721855,-0.0970747065674799));
#148091=CARTESIAN_POINT('Ctrl Pts',(-6.657718518,4.690837228,2.870066921));
#148092=CARTESIAN_POINT('Ctrl Pts',(-6.501171452,4.625180297,3.233210475));
#148093=CARTESIAN_POINT('Ctrl Pts',(-6.306055484,4.559946053,3.577172659));
#148094=CARTESIAN_POINT('Ctrl Pts',(-6.29930722346074,4.55768986823408,
3.58906889925688));
#148095=CARTESIAN_POINT('Ctrl Pts',(-6.29255896292154,4.55543368346804,
3.60096513951376));
#148096=CARTESIAN_POINT('Ctrl Pts',(-6.98163038082113,4.690837228,2.7412998228952));
#148097=CARTESIAN_POINT('Ctrl Pts',(-6.83210688278231,4.625180297,3.12211106708368));
#148098=CARTESIAN_POINT('Ctrl Pts',(-6.64205117335276,4.559946053,3.48440004939021));
#148099=CARTESIAN_POINT('Ctrl Pts',(-6.63547792638916,4.55768986823408,
3.49693013838376));
#148100=CARTESIAN_POINT('Ctrl Pts',(-6.62890467942558,4.55543368346802,
3.50946022737734));
#148101=CARTESIAN_POINT('',(-6.65584951362986,4.69005394733147,2.87439859321748));
#148102=CARTESIAN_POINT('Origin',(0.182806036133766,4.69642265498479,-0.0777656857180081));
#148103=CARTESIAN_POINT('Ctrl Pts',(-6.885580810478,4.65066950062011,2.97300805530623));
#148104=CARTESIAN_POINT('Ctrl Pts',(-6.84727107633065,4.65692555415897,
2.95652099241279));
#148105=CARTESIAN_POINT('Ctrl Pts',(-6.8089534551083,4.66333077442245,2.9400506858322));
#148106=CARTESIAN_POINT('Ctrl Pts',(-6.73238924394089,4.6764484494647,2.90718493774101));
#148107=CARTESIAN_POINT('Ctrl Pts',(-6.69409980081816,4.68316824025995,
2.89077109770168));
#148108=CARTESIAN_POINT('Ctrl Pts',(-6.65584951439294,4.69005394636003,
2.87439859102618));
#148109=CARTESIAN_POINT('Ctrl Pts',(-6.927609792,4.559946053,2.137924827));
#148110=CARTESIAN_POINT('Ctrl Pts',(-6.810999487,4.625601501,2.515782215));
#148111=CARTESIAN_POINT('Ctrl Pts',(-6.653983753,4.690829639,2.87871503));
#148112=CARTESIAN_POINT('Ctrl Pts',(-7.090106059,4.559946053,2.445484832));
#148113=CARTESIAN_POINT('Ctrl Pts',(-6.956720297,4.62560150099999,2.832205366));
#148114=CARTESIAN_POINT('Ctrl Pts',(-6.782064634,4.690829639,3.202124185));
#148115=CARTESIAN_POINT('Origin',(0.190142418624709,4.5535761338538,-0.0575450919829879));
#148116=CARTESIAN_POINT('Ctrl Pts',(-7.11904430900001,4.690837228,1.371753671));
#148117=CARTESIAN_POINT('Ctrl Pts',(-7.044222355,4.625180297,1.760060122));
#148118=CARTESIAN_POINT('Ctrl Pts',(-6.927609792,4.559946053,2.137924827));
#148119=CARTESIAN_POINT('Ctrl Pts',(-6.92357664196433,4.55768986818812,
2.15099361658192));
#148120=CARTESIAN_POINT('Ctrl Pts',(-6.91954349192857,4.55543368337614,
2.16406240616389));
#148121=CARTESIAN_POINT('Ctrl Pts',(-7.40770217163727,4.690837228,1.17636559945564));
#148122=CARTESIAN_POINT('Ctrl Pts',(-7.34353761129185,4.625180297,1.58041682072324));
#148123=CARTESIAN_POINT('Ctrl Pts',(-7.23580672022578,4.559946053,1.97509204848342));
#148124=CARTESIAN_POINT('Ctrl Pts',(-7.23208075077643,4.55768986818812,
1.98874224506581));
#148125=CARTESIAN_POINT('Ctrl Pts',(-7.22835478132707,4.55543368337614,
2.00239244164813));
#148126=CARTESIAN_POINT('',(-7.11815018154454,4.69005394731783,1.37638585135298));
#148127=CARTESIAN_POINT('Origin',(0.195249511375112,4.69642264758951,-0.0366496854463455));
#148128=CARTESIAN_POINT('Ctrl Pts',(-7.36370860838712,4.65066950056237,
1.42330444072716));
#148129=CARTESIAN_POINT('Ctrl Pts',(-7.32275029711851,4.6569255550511,1.41543829550915));
#148130=CARTESIAN_POINT('Ctrl Pts',(-7.28178789480078,4.66333077483531,
1.40759021220586));
#148131=CARTESIAN_POINT('Ctrl Pts',(-7.19994855029538,4.67644844951645,
1.39195189002702));
#148132=CARTESIAN_POINT('Ctrl Pts',(-7.15902580303485,4.68316824025603,
1.3841528952024));
#148133=CARTESIAN_POINT('Ctrl Pts',(-7.11815018169184,4.69005394643278,
1.37638584979319));
#148134=CARTESIAN_POINT('Ctrl Pts',(-7.225236766,4.559946053,0.598710006));
#148135=CARTESIAN_POINT('Ctrl Pts',(-7.192580914,4.625601501,0.992801067));
#148136=CARTESIAN_POINT('Ctrl Pts',(-7.11725594700001,4.690829639,1.381002455));
#148137=CARTESIAN_POINT('Ctrl Pts',(-7.450050271,4.559946053,0.864147535));
#148138=CARTESIAN_POINT('Ctrl Pts',(-7.402916477,4.625601501,1.270500754));
#148139=CARTESIAN_POINT('Ctrl Pts',(-7.311865778,4.690829639,1.669316881));
#148140=CARTESIAN_POINT('Origin',(0.198067364172025,4.55357616421649,-0.015324714123944));
#148141=CARTESIAN_POINT('Ctrl Pts',(-7.24749149900001,4.690837228,-0.190701257));
#148142=CARTESIAN_POINT('Ctrl Pts',(-7.25789325,4.625180297,0.204611314));
#148143=CARTESIAN_POINT('Ctrl Pts',(-7.225236766,4.559946053,0.598710006));
#148144=CARTESIAN_POINT('Ctrl Pts',(-7.22410731225297,4.55768986824605,
0.612340262226292));
#148145=CARTESIAN_POINT('Ctrl Pts',(-7.2229778585061,4.55543368349199,0.625970518452585));
#148146=CARTESIAN_POINT('Ctrl Pts',(-7.48739804276081,4.690837228,-0.443574171164436));
#148147=CARTESIAN_POINT('Ctrl Pts',(-7.51159268225325,4.625180297,-0.035175959275478));
#148148=CARTESIAN_POINT('Ctrl Pts',(-7.49122398729528,4.559946053,0.37343093749525));
#148149=CARTESIAN_POINT('Ctrl Pts',(-7.49051951773749,4.55768986824605,
0.387562972977406));
#148150=CARTESIAN_POINT('Ctrl Pts',(-7.48981504817983,4.55543368349199,
0.401695008459564));
#148151=CARTESIAN_POINT('',(-7.24761405802198,4.69005394733152,-0.185985163060938));
#148152=CARTESIAN_POINT('Origin',(0.198563202849756,4.69642265207484,0.00618004660821885));
#148153=CARTESIAN_POINT('Ctrl Pts',(-7.49751757546059,4.65066950057572,
-0.19295130721211));
#148154=CARTESIAN_POINT('Ctrl Pts',(-7.4558258610395,4.65692555461459,-0.191828720249321));
#148155=CARTESIAN_POINT('Ctrl Pts',(-7.41413402924507,4.66333077464523,
-0.190687614096624));
#148156=CARTESIAN_POINT('Ctrl Pts',(-7.33084626478274,4.67644844950723,
-0.188367281286426));
#148157=CARTESIAN_POINT('Ctrl Pts',(-7.28920371489588,4.68316824028114,
-0.187186759113336));
#148158=CARTESIAN_POINT('Ctrl Pts',(-7.24761405780493,4.69005394640255,
-0.185985165250032));
#148159=CARTESIAN_POINT('Ctrl Pts',(-7.18501969900001,4.559946053,-0.96849983));
#148160=CARTESIAN_POINT('Ctrl Pts',(-7.237845252,4.625601501,-0.576602356));
#148161=CARTESIAN_POINT('Ctrl Pts',(-7.247733164,4.690829639,-0.181284259));
#148162=CARTESIAN_POINT('Ctrl Pts',(-7.461638412,4.559946053,-0.75759634));
#148163=CARTESIAN_POINT('Ctrl Pts',(-7.50296051,4.625601501,-0.350611062));
#148164=CARTESIAN_POINT('Ctrl Pts',(-7.499772204,4.690829639,0.058454175));
#148165=CARTESIAN_POINT('Origin',(0.196730823850354,4.55357617794149,0.0276121826918264));
#148166=CARTESIAN_POINT('Ctrl Pts',(-7.037054042,4.690837228,-1.744239205));
#148167=CARTESIAN_POINT('Ctrl Pts',(-7.132193124,4.625180297,-1.360404892));
#148168=CARTESIAN_POINT('Ctrl Pts',(-7.185019699,4.559946053,-0.96849983));
#148169=CARTESIAN_POINT('Ctrl Pts',(-7.18684675352726,4.55768986810005,
-0.954945441554801));
#148170=CARTESIAN_POINT('Ctrl Pts',(-7.1886738080545,4.55543368319999,-0.941391053109596));
#148171=CARTESIAN_POINT('Ctrl Pts',(-7.21699150217716,4.690837228,-2.04277290610587));
#148172=CARTESIAN_POINT('Ctrl Pts',(-7.32841402767017,4.625180297,-1.64912395008705));
#148173=CARTESIAN_POINT('Ctrl Pts',(-7.39635994642545,4.559946053,-1.24569138826482));
#148174=CARTESIAN_POINT('Ctrl Pts',(-7.39870991703153,4.55768986810005,
-1.23173831088819));
#148175=CARTESIAN_POINT('Ctrl Pts',(-7.40105988763752,4.55543368319998,
-1.21778523351154));
#148176=CARTESIAN_POINT('',(-7.03818755607615,4.69005394729387,-1.73965971772344));
#148177=CARTESIAN_POINT('Origin',(0.192592371211763,4.69642264078062,0.0487207763574957));
#148178=CARTESIAN_POINT('Ctrl Pts',(-7.28075095342903,4.65066950062243,
-1.80018486679472));
#148179=CARTESIAN_POINT('Ctrl Pts',(-7.24027528496446,4.65692555561415,
-1.79012603745073));
#148180=CARTESIAN_POINT('Ctrl Pts',(-7.19980349256061,4.66333077513083,
-1.78004909900782));
#148181=CARTESIAN_POINT('Ctrl Pts',(-7.11896175532797,4.67644844955349,
-1.7598786072466));
#148182=CARTESIAN_POINT('Ctrl Pts',(-7.07854656244168,4.683168240323,-1.74977376756505));
#148183=CARTESIAN_POINT('Ctrl Pts',(-7.03818755555002,4.69005394643001,
-1.7396597192348));
#148184=CARTESIAN_POINT('Ctrl Pts',(-6.808839097,4.559946053,-2.49042369));
#148185=CARTESIAN_POINT('Ctrl Pts',(-6.94467599,4.625601501,-2.119044493));
#148186=CARTESIAN_POINT('Ctrl Pts',(-7.039314433,4.690829639,-1.735094322));
#148187=CARTESIAN_POINT('Ctrl Pts',(-7.124328633,4.559946053,-2.343915853));
#148188=CARTESIAN_POINT('Ctrl Pts',(-7.252174449,4.625601501,-1.955328694));
#148189=CARTESIAN_POINT('Ctrl Pts',(-7.336997617,4.690829639,-1.555141784));
#148190=CARTESIAN_POINT('Origin',(0.186195839981054,4.55357613693572,0.0692580166496981));
#148191=CARTESIAN_POINT('Ctrl Pts',(-6.49757176,4.690837228,-3.216218467));
#148192=CARTESIAN_POINT('Ctrl Pts',(-6.672999573,4.625180297,-2.861810077));
#148193=CARTESIAN_POINT('Ctrl Pts',(-6.808839097,4.559946053,-2.49042369));
#148194=CARTESIAN_POINT('Ctrl Pts',(-6.81353722888779,4.55768986810709,
-2.47757895839265));
#148195=CARTESIAN_POINT('Ctrl Pts',(-6.81823536077545,4.55543368321406,
-2.46473422678533));
#148196=CARTESIAN_POINT('Ctrl Pts',(-6.60912646082549,4.690837228,-3.546453851052));
#148197=CARTESIAN_POINT('Ctrl Pts',(-6.80256687881719,4.625180297,-3.18596073831595));
#148198=CARTESIAN_POINT('Ctrl Pts',(-6.95565033526412,4.559946053,-2.80656656937056));
#148199=CARTESIAN_POINT('Ctrl Pts',(-6.96094486403635,4.55768986810709,
-2.79344488143564));
#148200=CARTESIAN_POINT('Ctrl Pts',(-6.96623939280858,4.55543368321407,
-2.78032319350065));
#148201=CARTESIAN_POINT('',(-6.49966322680666,4.69005394729517,-3.21198971733521));
#148202=CARTESIAN_POINT('Origin',(0.177616129444476,4.6964226569031,0.0889833830679743));
#148203=CARTESIAN_POINT('Ctrl Pts',(-6.72354450891878,4.65066950062616,
-3.32324378223984));
#148204=CARTESIAN_POINT('Ctrl Pts',(-6.68617749493491,4.65692555480842,
-3.3047190529955));
#148205=CARTESIAN_POINT('Ctrl Pts',(-6.64881815156918,4.6633307747993,-3.28617746743296));
#148206=CARTESIAN_POINT('Ctrl Pts',(-6.57420250684019,4.67644844959452,
-3.24909996596324));
#148207=CARTESIAN_POINT('Ctrl Pts',(-6.53690444003399,4.68316824048538,
-3.23054329983003));
#148208=CARTESIAN_POINT('Ctrl Pts',(-6.49966322605803,4.69005394657573,
-3.21198971904582));
#148209=CARTESIAN_POINT('Ctrl Pts',(-6.114284746,4.559946053,-3.895898106));
#148210=CARTESIAN_POINT('Ctrl Pts',(-6.326781397,4.625601501,-3.562402465));
#148211=CARTESIAN_POINT('Ctrl Pts',(-6.501745184,4.690829639,-3.207773304));
#148212=CARTESIAN_POINT('Ctrl Pts',(-6.453893166,4.559946053,-3.820636465));
#148213=CARTESIAN_POINT('Ctrl Pts',(-6.66228477,4.625601501,-3.468617329));
#148214=CARTESIAN_POINT('Ctrl Pts',(-6.831153176,4.690829639,-3.096021041));
#148215=CARTESIAN_POINT('Origin',(0.166954016505535,4.55357622549867,0.107665247459791));
#148216=CARTESIAN_POINT('Ctrl Pts',(-5.654270243,4.690837228,-4.537810928));
#148217=CARTESIAN_POINT('Ctrl Pts',(-5.90178398,4.625180297,-4.229400204));
#148218=CARTESIAN_POINT('Ctrl Pts',(-6.114284746,4.559946053,-3.895898106));
#148219=CARTESIAN_POINT('Ctrl Pts',(-6.1216342760813,4.55768986801004,-3.88436363604226));
#148220=CARTESIAN_POINT('Ctrl Pts',(-6.12898380616261,4.55543368301997,
-3.87282916608446));
#148221=CARTESIAN_POINT('Ctrl Pts',(-5.69222601069263,4.690837228,-4.88430655563121));
#148222=CARTESIAN_POINT('Ctrl Pts',(-5.9586392635831,4.625180297,-4.57382554315651));
#148223=CARTESIAN_POINT('Ctrl Pts',(-6.1897022444045,4.559946053,-4.2362098168995));
#148224=CARTESIAN_POINT('Ctrl Pts',(-6.19769376537727,4.55768986801004,
-4.22453307340936));
#148225=CARTESIAN_POINT('Ctrl Pts',(-6.20568528634992,4.55543368301996,
-4.2128563299192));
#148226=CARTESIAN_POINT('',(-5.65722186911748,4.69005394727052,-4.5341306477488));
#148227=CARTESIAN_POINT('Origin',(0.154334891420042,4.69642268872752,0.125085317682646));
#148228=CARTESIAN_POINT('Ctrl Pts',(-5.85195259570583,4.65066950062562,
-4.69091151222382));
#148229=CARTESIAN_POINT('Ctrl Pts',(-5.81944146920557,4.65692555514123,
-4.66478707599278));
#148230=CARTESIAN_POINT('Ctrl Pts',(-5.78694146035984,4.66333077493862,
-4.63864782873607));
#148231=CARTESIAN_POINT('Ctrl Pts',(-5.72204085546351,4.67644844957531,
-4.58639702126181));
#148232=CARTESIAN_POINT('Ctrl Pts',(-5.68960393149243,4.68316824044095,
-4.56025621791814));
#148233=CARTESIAN_POINT('Ctrl Pts',(-5.6572218677117,4.69005394654428,-4.53413064929983));
#148234=CARTESIAN_POINT('Ctrl Pts',(-5.133833235,4.559946053,-5.119204656));
#148235=CARTESIAN_POINT('Ctrl Pts',(-5.413053537,4.62560150099999,-4.839186457));
#148236=CARTESIAN_POINT('Ctrl Pts',(-5.660161555,4.690829639,-4.530460371));
#148237=CARTESIAN_POINT('Ctrl Pts',(-5.481680828,4.559946053,-5.118708363));
#148238=CARTESIAN_POINT('Ctrl Pts',(-5.76087406,4.62560150099999,-4.819717273));
#148239=CARTESIAN_POINT('Ctrl Pts',(-6.00589160500001,4.690829639,-4.492133795));
#148240=CARTESIAN_POINT('Origin',(0.139906077312633,4.55357614863355,0.141038475289471));
#148241=CARTESIAN_POINT('Ctrl Pts',(-4.546581334,4.690837228,-5.647220394));
#148242=CARTESIAN_POINT('Ctrl Pts',(-4.85460752600001,4.625180297,-5.399228277));
#148243=CARTESIAN_POINT('Ctrl Pts',(-5.133833235,4.559946053,-5.119204656));
#148244=CARTESIAN_POINT('Ctrl Pts',(-5.1434905069197,4.55768986808407,-5.1095197875772));
#148245=CARTESIAN_POINT('Ctrl Pts',(-5.15314777883924,4.55543368316826,
-5.09983491915429));
#148246=CARTESIAN_POINT('Ctrl Pts',(-4.50916339980099,4.690837228,-5.99377451448871));
#148247=CARTESIAN_POINT('Ctrl Pts',(-4.83609229828384,4.625180297,-5.74782334933595));
#148248=CARTESIAN_POINT('Ctrl Pts',(-5.13433055676911,4.55994605300001,
-5.46777260227703));
#148249=CARTESIAN_POINT('Ctrl Pts',(-5.14464539478797,4.55768986808407,
-5.45808679567509));
#148250=CARTESIAN_POINT('Ctrl Pts',(-5.15496023280698,4.55543368316826,
-5.44840098907329));
#148251=CARTESIAN_POINT('',(-4.55025510439708,4.6900539473003,-5.64426066861927));
#148252=CARTESIAN_POINT('Origin',(0.123836918956326,4.69642264566216,0.155338239191032));
#148253=CARTESIAN_POINT('Ctrl Pts',(-4.70672988353111,4.65066950059933,
-5.83923743366634));
#148254=CARTESIAN_POINT('Ctrl Pts',(-4.68059483217912,4.65692555473698,
-5.80673484297425));
#148255=CARTESIAN_POINT('Ctrl Pts',(-4.65447382010427,4.66333077472239,
-5.7742201744936));
#148256=CARTESIAN_POINT('Ctrl Pts',(-4.60232293359513,4.67644844953836,
-5.70923924922473));
#148257=CARTESIAN_POINT('Ctrl Pts',(-4.5762638670516,4.68316824035594,-5.67673662366901));
#148258=CARTESIAN_POINT('Ctrl Pts',(-4.55025510284291,4.6900539464758,-5.64426066968913));
#148259=CARTESIAN_POINT('Ctrl Pts',(-3.913329389,4.559946053,-6.10314288700001));
#148260=CARTESIAN_POINT('Ctrl Pts',(-4.246217311,4.62560150099999,-5.889695469));
#148261=CARTESIAN_POINT('Ctrl Pts',(-4.553915063,4.690829639,-5.641308146));
#148262=CARTESIAN_POINT('Ctrl Pts',(-4.253151186,4.559946053,-6.177435146));
#148263=CARTESIAN_POINT('Ctrl Pts',(-4.590091282,4.62560150099999,-5.945452595));
#148264=CARTESIAN_POINT('Ctrl Pts',(-4.899801218,4.690829639,-5.678199365));
#148265=CARTESIAN_POINT('Origin',(0.106316165810689,4.55357608865779,0.167816914275922));
#148266=CARTESIAN_POINT('Ctrl Pts',(-3.226299335,4.690837228,-6.49257211000001));
#148267=CARTESIAN_POINT('Ctrl Pts',(-3.58043502,4.625180297,-6.316594438));
#148268=CARTESIAN_POINT('Ctrl Pts',(-3.913329389,4.559946053,-6.103142887));
#148269=CARTESIAN_POINT('Ctrl Pts',(-3.92484283910021,4.55768986820667,
-6.09576047380798));
#148270=CARTESIAN_POINT('Ctrl Pts',(-3.93635628920047,4.55543368341347,
-6.08837806061598));
#148271=CARTESIAN_POINT('Ctrl Pts',(-3.11525731968891,4.690837228,-6.82298023806261));
#148272=CARTESIAN_POINT('Ctrl Pts',(-3.48741503215406,4.625180297,-6.6530593240067));
#148273=CARTESIAN_POINT('Ctrl Pts',(-3.83888327807568,4.559946053,-6.44366841676536));
#148274=CARTESIAN_POINT('Ctrl Pts',(-3.8510391223556,4.55768986820667,-6.43642644457697));
#148275=CARTESIAN_POINT('Ctrl Pts',(-3.86319496663552,4.55543368341345,
-6.42918447238861));
#148276=CARTESIAN_POINT('',(-3.23052346845693,4.69005394729118,-6.49047133413896));
#148277=CARTESIAN_POINT('Origin',(0.087548756417985,4.69642265196506,0.178328165779703));
#148278=CARTESIAN_POINT('Ctrl Pts',(-3.3414257128972,4.65066950063507,-6.71452710196661));
#148279=CARTESIAN_POINT('Ctrl Pts',(-3.32288878222841,4.65692555427717,
-6.67716614327895));
#148280=CARTESIAN_POINT('Ctrl Pts',(-3.30436815677363,4.66333077449093,
-6.63979640280476));
#148281=CARTESIAN_POINT('Ctrl Pts',(-3.2674055064748,4.67644844951943,-6.56512379521447));
#148282=CARTESIAN_POINT('Ctrl Pts',(-3.24894279044509,4.6831682402169,-6.5277791346204));
#148283=CARTESIAN_POINT('Ctrl Pts',(-3.23052346675912,4.6900539463452,-6.4904713348026));
#148284=CARTESIAN_POINT('Ctrl Pts',(-2.509842609,4.559946053,-6.801704939));
#148285=CARTESIAN_POINT('Ctrl Pts',(-2.880832682,4.62560150099999,-6.66480886600001));
#148286=CARTESIAN_POINT('Ctrl Pts',(-3.234732564,4.690829639,-6.488374622));
#148287=CARTESIAN_POINT('Ctrl Pts',(-2.825748922,4.559946053,-6.947311928));
#148288=CARTESIAN_POINT('Ctrl Pts',(-3.204680937,4.62560150099999,-6.79318516));
#148289=CARTESIAN_POINT('Ctrl Pts',(-3.564601571,4.690829639,-6.598758644));
#148290=CARTESIAN_POINT('Origin',(0.0677547936467743,4.55357613660652,0.186748104515124));
#148291=CARTESIAN_POINT('Ctrl Pts',(-1.755159165,4.690837228,-7.03433837));
#148292=CARTESIAN_POINT('Ctrl Pts',(-2.138845352,4.625180297,-6.938603662));
#148293=CARTESIAN_POINT('Ctrl Pts',(-2.509842609,4.559946053,-6.801704939));
#148294=CARTESIAN_POINT('Ctrl Pts',(-2.5226738823718,4.55768986807635,-6.79697017369941));
#148295=CARTESIAN_POINT('Ctrl Pts',(-2.5355051557436,4.55543368315257,-6.79223540839867));
#148296=CARTESIAN_POINT('Ctrl Pts',(-1.57568526882399,4.690837228,-7.33315098852527));
#148297=CARTESIAN_POINT('Ctrl Pts',(-1.97567011476171,4.625180297,-7.2472056382896));
#148298=CARTESIAN_POINT('Ctrl Pts',(-2.36393408428663,4.559946053,-7.11826545847802));
#148299=CARTESIAN_POINT('Ctrl Pts',(-2.37736254242049,4.55768986807635,
-7.11380594654213));
#148300=CARTESIAN_POINT('Ctrl Pts',(-2.39079100055429,4.55543368315257,
-7.10934643460628));
#148301=CARTESIAN_POINT('',(-1.75973614522046,4.69005394734215,-7.0331947738758));
#148302=CARTESIAN_POINT('Origin',(0.0471665917159619,4.69642264847688,0.192979168038592));
#148303=CARTESIAN_POINT('Ctrl Pts',(-1.81988018914674,4.6506695006064,-7.27585294610869));
#148304=CARTESIAN_POINT('Ctrl Pts',(-1.80980814109728,4.65692555564396,
-7.23538056476313));
#148305=CARTESIAN_POINT('Ctrl Pts',(-1.7997539084123,4.66333077509884,-7.19490312626228));
#148306=CARTESIAN_POINT('Ctrl Pts',(-1.77970782869064,4.67644844946861,
-7.11403044988764));
#148307=CARTESIAN_POINT('Ctrl Pts',(-1.76970475880949,4.68316824019229,
-7.07358994854362));
#148308=CARTESIAN_POINT('Ctrl Pts',(-1.75973614281127,4.69005394634804,
-7.03319477430088));
#148309=CARTESIAN_POINT('Ctrl Pts',(-0.988998379000001,4.559946053,-7.182226828));
#148310=CARTESIAN_POINT('Ctrl Pts',(-1.380743519,4.62560150099999,-7.128283209));
#148311=CARTESIAN_POINT('Ctrl Pts',(-1.764297565,4.690829639,-7.032051913));
#148312=CARTESIAN_POINT('Ctrl Pts',(-1.266217779,4.559946053,-7.392340126));
#148313=CARTESIAN_POINT('Ctrl Pts',(-1.669423273,4.62560150099999,-7.323275938));
#148314=CARTESIAN_POINT('Ctrl Pts',(-2.062725117,4.690829639,-7.210767303));
#148315=CARTESIAN_POINT('Origin',(0.0260254480465574,4.55357606320967,0.196947624641689));
#148316=CARTESIAN_POINT('Ctrl Pts',(-0.201949703,4.690837228,-7.247186786));
#148317=CARTESIAN_POINT('Ctrl Pts',(-0.597245653,4.625180297,-7.236171492));
#148318=CARTESIAN_POINT('Ctrl Pts',(-0.988998379000001,4.559946053,-7.182226828));
#148319=CARTESIAN_POINT('Ctrl Pts',(-1.00254749810723,4.55768986821006,
-7.18036110345178));
#148320=CARTESIAN_POINT('Ctrl Pts',(-1.01609661721445,4.55543368342,-7.17849537890344));
#148321=CARTESIAN_POINT('Ctrl Pts',(0.0375640730718744,4.690837228,-7.50043175005402));
#148322=CARTESIAN_POINT('Ctrl Pts',(-0.371545059360647,4.625180297,-7.50248067266783));
#148323=CARTESIAN_POINT('Ctrl Pts',(-0.778449959965024,4.559946053,-7.46002031823318));
#148324=CARTESIAN_POINT('Ctrl Pts',(-0.792523130609923,4.55768986821006,
-7.45855178882321));
#148325=CARTESIAN_POINT('Ctrl Pts',(-0.80659630125483,4.55543368342001,
-7.45708325941323));
#148326=CARTESIAN_POINT('',(-0.206665515392902,4.69005394729617,-7.24705384059663));
#148327=CARTESIAN_POINT('Origin',(0.00457900162748118,4.69642265313607,
0.198606590580912));
#148328=CARTESIAN_POINT('Ctrl Pts',(-0.213239090823364,4.65066950319989,
-7.49696797599281));
#148329=CARTESIAN_POINT('Ctrl Pts',(-0.212102887474093,4.65692555718157,
-7.45527663113703));
#148330=CARTESIAN_POINT('Ctrl Pts',(-0.210985170253372,4.66333077468,-7.41358418236226));
#148331=CARTESIAN_POINT('Ctrl Pts',(-0.20879299148723,4.67644844957351,
-7.33029294597433));
#148332=CARTESIAN_POINT('Ctrl Pts',(-0.207717300189202,4.68316824044063,
-7.28864755558494));
#148333=CARTESIAN_POINT('Ctrl Pts',(-0.206665513338619,4.69005394649188,
-7.24705384051543));
#148334=CARTESIAN_POINT('Ctrl Pts',(0.578090316999999,4.559946053,-7.226915773));
#148335=CARTESIAN_POINT('Ctrl Pts',(0.183907677,4.62560150099999,-7.258446951));
#148336=CARTESIAN_POINT('Ctrl Pts',(-0.211365974,4.690829639,-7.246918271));
#148337=CARTESIAN_POINT('Ctrl Pts',(0.3525203,4.559946053,-7.491710715));
#148338=CARTESIAN_POINT('Ctrl Pts',(-0.056105233,4.62560150099999,-7.510938472));
#148339=CARTESIAN_POINT('Ctrl Pts',(-0.464397928,4.690829639,-7.485608497));
#148340=CARTESIAN_POINT('Origin',(-0.0169208918346127,4.55357611859478,
0.197937287104135));
#148341=CARTESIAN_POINT('Ctrl Pts',(1.360702703,4.690837228,-7.12116480300001));
#148342=CARTESIAN_POINT('Ctrl Pts',(0.97228059,4.625180297,-7.19538398400001));
#148343=CARTESIAN_POINT('Ctrl Pts',(0.578090317,4.559946053,-7.226915773));
#148344=CARTESIAN_POINT('Ctrl Pts',(0.564456893314398,4.55768986823804,
-7.22800632816698));
#148345=CARTESIAN_POINT('Ctrl Pts',(0.550823469628794,4.55543368347596,
-7.22909688333405));
#148346=CARTESIAN_POINT('Ctrl Pts',(1.64905696119275,4.690837228,-7.31700065792814));
#148347=CARTESIAN_POINT('Ctrl Pts',(1.24995303106491,4.625180297,-7.40694804796946));
#148348=CARTESIAN_POINT('Ctrl Pts',(0.843433619569688,4.559946053,-7.45295291915567));
#148349=CARTESIAN_POINT('Ctrl Pts',(0.829373781585471,4.55768986823804,
-7.45454403883429));
#148350=CARTESIAN_POINT('Ctrl Pts',(0.815313943601237,4.55543368347595,
-7.45613515851278));
#148351=CARTESIAN_POINT('',(1.35606856387976,4.6900539472633,-7.12204872627897));
#148352=CARTESIAN_POINT('Origin',(-0.0382226035133557,4.69642263628286,
0.194947726860468));
#148353=CARTESIAN_POINT('Ctrl Pts',(1.40337283024095,4.65066950057685,-7.36753314860582));
#148354=CARTESIAN_POINT('Ctrl Pts',(1.39552006198328,4.65692555525109,-7.32657226924565));
#148355=CARTESIAN_POINT('Ctrl Pts',(1.3876490007401,4.66333077493922,-7.28561427662822));
#148356=CARTESIAN_POINT('Ctrl Pts',(1.371884774107,4.67644844949167,-7.20379909165715));
#148357=CARTESIAN_POINT('Ctrl Pts',(1.36398278850602,4.68316824027346,-7.16289610614497));
#148358=CARTESIAN_POINT('Ctrl Pts',(1.35606856587716,4.69005394638793,-7.12204872574441));
#148359=CARTESIAN_POINT('Ctrl Pts',(2.118148151,4.559946053,-6.933682168));
#148360=CARTESIAN_POINT('Ctrl Pts',(1.739959553,4.62560150099999,-7.04921378));
#148361=CARTESIAN_POINT('Ctrl Pts',(1.351448856,4.690829639,-7.122926785));
#148362=CARTESIAN_POINT('Ctrl Pts',(1.954774922,4.559946053,-7.24077723800001));
#148363=CARTESIAN_POINT('Ctrl Pts',(1.559836226,4.62560150099999,-7.347397871));
#148364=CARTESIAN_POINT('Ctrl Pts',(1.155643991,4.690829639,-7.410430957));
#148365=CARTESIAN_POINT('Origin',(-0.0590759568647822,4.55357616882721,
0.189672134404391));
#148366=CARTESIAN_POINT('Ctrl Pts',(2.859730162,4.690837228,-6.662165068));
#148367=CARTESIAN_POINT('Ctrl Pts',(2.496344072,4.625180297,-6.818148319));
#148368=CARTESIAN_POINT('Ctrl Pts',(2.118148151,4.559946053,-6.933682168));
#148369=CARTESIAN_POINT('Ctrl Pts',(2.10506790544386,4.55768986808944,-6.93767800991962));
#148370=CARTESIAN_POINT('Ctrl Pts',(2.09198765988772,4.55543368317901,-6.94167385183935));
#148371=CARTESIAN_POINT('Ctrl Pts',(3.18344177798669,4.690837228,-6.7914347477429));
#148372=CARTESIAN_POINT('Ctrl Pts',(2.8130047063723,4.625180297,-6.96507476535647));
#148373=CARTESIAN_POINT('Ctrl Pts',(2.42587918037998,4.559946053,-7.09739372560017));
#148374=CARTESIAN_POINT('Ctrl Pts',(2.41249009641619,4.55768986808944,-7.10197009566556));
#148375=CARTESIAN_POINT('Ctrl Pts',(2.39910101245242,4.55543368317901,-7.10654646573097));
#148376=CARTESIAN_POINT('',(2.85539438454128,4.69005394734903,-6.66402452886225));
#148377=CARTESIAN_POINT('Origin',(-0.0792369470889415,4.69642268535183,
0.18217313625983));
#148378=CARTESIAN_POINT('Ctrl Pts',(2.95436459788649,4.65066950058357,-6.89360064286475));
#148379=CARTESIAN_POINT('Ctrl Pts',(2.93789004392934,4.65692555558273,-6.85528551722975));
#148380=CARTESIAN_POINT('Ctrl Pts',(2.92139824654535,4.66333077509932,-6.81697714636908));
#148381=CARTESIAN_POINT('Ctrl Pts',(2.88841473289329,4.67644844951969,-6.74046359853245));
#148382=CARTESIAN_POINT('Ctrl Pts',(2.871904558448,4.68316824035792,-6.70221559510132));
#148383=CARTESIAN_POINT('Ctrl Pts',(2.8553943867348,4.69005394645179,-6.66402452775221));
#148384=CARTESIAN_POINT('Ctrl Pts',(3.559163733,4.559946053,-6.316237292));
#148385=CARTESIAN_POINT('Ctrl Pts',(3.214652856,4.62560150099999,-6.51036720800001));
#148386=CARTESIAN_POINT('Ctrl Pts',(2.85107144,4.690829639,-6.66587516));
#148387=CARTESIAN_POINT('Ctrl Pts',(3.465626441,4.559946053,-6.651273064));
#148388=CARTESIAN_POINT('Ctrl Pts',(3.102841477,4.62560150099999,-6.840301112));
#148389=CARTESIAN_POINT('Ctrl Pts',(2.721649282,4.690829639,-6.988749902));
#148390=CARTESIAN_POINT('Origin',(-0.0984686841105226,4.55357616529912,
0.172538095315817));
#148391=CARTESIAN_POINT('Ctrl Pts',(4.225039818,4.690837228,-5.891649899));
#148392=CARTESIAN_POINT('Ctrl Pts',(3.903681281,4.625180297,-6.122103616));
#148393=CARTESIAN_POINT('Ctrl Pts',(3.559163733,4.559946053,-6.316237292));
#148394=CARTESIAN_POINT('Ctrl Pts',(3.54724828415092,4.55768986807677,-6.32295157955862));
#148395=CARTESIAN_POINT('Ctrl Pts',(3.53533283530178,4.55543368315343,-6.32966586711737));
#148396=CARTESIAN_POINT('Ctrl Pts',(4.5689723957904,4.690837228,-5.94830889693407));
#148397=CARTESIAN_POINT('Ctrl Pts',(4.2445234080404,4.625180297,-6.19752232790761));
#148398=CARTESIAN_POINT('Ctrl Pts',(3.89489332643794,4.559946053,-6.40996828922153));
#148399=CARTESIAN_POINT('Ctrl Pts',(3.88280105602207,4.55768986807677,-6.41731592361615));
#148400=CARTESIAN_POINT('Ctrl Pts',(3.87070878560611,4.55543368315345,-6.42466355801077));
#148401=CARTESIAN_POINT('',(4.22120513711781,4.69005394729203,-5.89439795128933));
#148402=CARTESIAN_POINT('Origin',(-0.116546242049927,4.69642265312355,0.160880395786349));
#148403=CARTESIAN_POINT('Ctrl Pts',(4.36721356001129,4.65066950061697,-6.09733103232014));
#148404=CARTESIAN_POINT('Ctrl Pts',(4.34288755318521,4.65692555542693,-6.06345323611052));
#148405=CARTESIAN_POINT('Ctrl Pts',(4.31854615715426,4.66333077500663,-6.02958574219209));
#148406=CARTESIAN_POINT('Ctrl Pts',(4.26988562827294,4.67644844947529,-5.96195151866449));
#148407=CARTESIAN_POINT('Ctrl Pts',(4.24553926283835,4.68316824016109,-5.92814693247655));
#148408=CARTESIAN_POINT('Ctrl Pts',(4.22120513897642,4.69005394628535,-5.89439794974382));
#148409=CARTESIAN_POINT('Ctrl Pts',(4.833756773,4.559946053,-5.403452179));
#148410=CARTESIAN_POINT('Ctrl Pts',(4.539032563,4.62560150099999,-5.667103101));
#148411=CARTESIAN_POINT('Ctrl Pts',(4.217381091,4.690829639,-5.89713462));
#148412=CARTESIAN_POINT('Ctrl Pts',(4.814429119,4.559946053,-5.750762755));
#148413=CARTESIAN_POINT('Ctrl Pts',(4.500761309,4.62560150099999,-6.013359475));
#148414=CARTESIAN_POINT('Ctrl Pts',(4.160393277,4.690829639,-6.240282668));
#148415=CARTESIAN_POINT('Origin',(-0.133257209622126,4.55357610187738,0.147336455412355));
#148416=CARTESIAN_POINT('Ctrl Pts',(5.392791307,4.690837228,-4.845647729));
#148417=CARTESIAN_POINT('Ctrl Pts',(5.128486691,4.625180297,-5.139796152));
#148418=CARTESIAN_POINT('Ctrl Pts',(4.833756773,4.559946053,-5.403452179));
#148419=CARTESIAN_POINT('Ctrl Pts',(4.82356327437088,4.55768986814676,-5.41257095923113));
#148420=CARTESIAN_POINT('Ctrl Pts',(4.81336977574183,4.55543368329364,-5.42168973946224));
#148421=CARTESIAN_POINT('Ctrl Pts',(5.74086294257771,4.690837228,-4.82704673403762));
#148422=CARTESIAN_POINT('Ctrl Pts',(5.4775729123286,4.625180297,-5.14018063457471));
#148423=CARTESIAN_POINT('Ctrl Pts',(5.18178659015542,4.559946053,-5.42281985940054));
#148424=CARTESIAN_POINT('Ctrl Pts',(5.17155655484025,4.55768986814676,-5.43259519055912));
#148425=CARTESIAN_POINT('Ctrl Pts',(5.16132651952504,4.55543368329364,-5.44237052171769));
#148426=CARTESIAN_POINT('',(5.38963702945794,4.69005394731139,-4.84915587636755));
#148427=CARTESIAN_POINT('Origin',(-0.14840603322689,4.69642265777085,0.132065168005893));
#148428=CARTESIAN_POINT('Ctrl Pts',(5.57585646967172,4.65066950063289,-5.01595700001295));
#148429=CARTESIAN_POINT('Ctrl Pts',(5.54481647208783,4.65692555434243,-4.98810062512853));
#148430=CARTESIAN_POINT('Ctrl Pts',(5.51376365132302,4.66333077450115,-4.96025761229812));
#148431=CARTESIAN_POINT('Ctrl Pts',(5.45170141738881,4.67644844948845,-4.90466521235817));
#148432=CARTESIAN_POINT('Ctrl Pts',(5.42065726996585,4.68316824012357,-4.87688470765217));
#148433=CARTESIAN_POINT('Ctrl Pts',(5.38963703080559,4.69005394625158,-4.84915587459676));
#148434=CARTESIAN_POINT('Ctrl Pts',(5.88232872,4.559946053,-4.238007649));
#148435=CARTESIAN_POINT('Ctrl Pts',(5.651172152,4.62560150099999,-4.55885155200001));
#148436=CARTESIAN_POINT('Ctrl Pts',(5.38649069,4.690829639,-4.85265062));
#148437=CARTESIAN_POINT('Ctrl Pts',(5.938114442,4.559946053,-4.58135317));
#148438=CARTESIAN_POINT('Ctrl Pts',(5.688230544,4.62560150099999,-4.905239832));
#148439=CARTESIAN_POINT('Ctrl Pts',(5.404601906,4.690829639,-5.200026753));
#148440=CARTESIAN_POINT('Origin',(-0.161814908908519,4.55357611144126,0.115245624276269));
#148441=CARTESIAN_POINT('Ctrl Pts',(6.308381869,4.690837228,-3.573068457));
#148442=CARTESIAN_POINT('Ctrl Pts',(6.113489763,4.625180297,-3.917157533));
#148443=CARTESIAN_POINT('Ctrl Pts',(5.88232872,4.559946053,-4.238007649));
#148444=CARTESIAN_POINT('Ctrl Pts',(5.87433380809871,4.55768986819065,-4.24910453789466));
#148445=CARTESIAN_POINT('Ctrl Pts',(5.86633889619729,4.55543368338141,-4.26020142678927));
#148446=CARTESIAN_POINT('Ctrl Pts',(6.64431711846052,4.690837228,-3.48007722958924));
#148447=CARTESIAN_POINT('Ctrl Pts',(6.45449719567473,4.625180297,-3.84248980808535));
#148448=CARTESIAN_POINT('Ctrl Pts',(6.22638527100694,4.559946053,-4.18210640003392));
#148449=CARTESIAN_POINT('Ctrl Pts',(6.2184958155966,4.55768986819065,-4.19385234432286));
#148450=CARTESIAN_POINT('Ctrl Pts',(6.21060636018626,4.55543368338141,-4.20559828861183));
#148451=CARTESIAN_POINT('',(6.30605548334288,4.69005394732156,-3.57717266141838));
#148452=CARTESIAN_POINT('Origin',(-0.173326514540458,4.6964226515756,0.097074634998458));
#148453=CARTESIAN_POINT('Ctrl Pts',(6.52377852850537,4.65066950058853,-3.70004239318149));
#148454=CARTESIAN_POINT('Ctrl Pts',(6.48747592977033,4.65692555462453,-3.67950996574764));
#148455=CARTESIAN_POINT('Ctrl Pts',(6.45116368268525,4.66333077467253,-3.65899334604125));
#148456=CARTESIAN_POINT('Ctrl Pts',(6.37860170737359,4.67644844952994,-3.61804221178828));
#148457=CARTESIAN_POINT('Ctrl Pts',(6.34231136657993,4.6831682403472,-3.59758477342315));
#148458=CARTESIAN_POINT('Ctrl Pts',(6.30605548408511,4.69005394644704,-3.57717265980503));
#148459=CARTESIAN_POINT('Ctrl Pts',(6.655849513,4.559946053,-2.874398591));
#148460=CARTESIAN_POINT('Ctrl Pts',(6.499069213,4.62560150099999,-3.237433171));
#148461=CARTESIAN_POINT('Ctrl Pts',(6.303733971,4.690829639,-3.581262071));
#148462=CARTESIAN_POINT('Ctrl Pts',(6.784140134,4.559946053,-3.197724603));
#148463=CARTESIAN_POINT('Ctrl Pts',(6.609724441,4.62560150099999,-3.567756627));
#148464=CARTESIAN_POINT('Ctrl Pts',(6.396097357,4.690829639,-3.916623367));
#148465=CARTESIAN_POINT('Origin',(-0.182805944568682,4.55357610379343,0.0777657167856155));
#148466=CARTESIAN_POINT('Ctrl Pts',(6.928999505,4.690837228,-2.133416475));
#148467=CARTESIAN_POINT('Ctrl Pts',(6.81263284900001,4.625180297,-2.511356981));
#148468=CARTESIAN_POINT('Ctrl Pts',(6.655849513,4.559946053,-2.874398591));
#148469=CARTESIAN_POINT('Ctrl Pts',(6.65042702044375,4.55768986805376,-2.88695471129988));
#148470=CARTESIAN_POINT('Ctrl Pts',(6.64500452788751,4.55543368310764,-2.89951083159971));
#148471=CARTESIAN_POINT('Ctrl Pts',(7.23709041011188,4.690837228,-1.97038318210181));
#148472=CARTESIAN_POINT('Ctrl Pts',(7.12961636364939,4.625180297,-2.36512842791059));
#148473=CARTESIAN_POINT('Ctrl Pts',(6.97984509784936,4.559946053,-2.74584229453652));
#148474=CARTESIAN_POINT('Ctrl Pts',(6.97466512404182,4.55768986805376,-2.75900962571157));
#148475=CARTESIAN_POINT('Ctrl Pts',(6.96948515023431,4.55543368310764,-2.77217695688653));
#148476=CARTESIAN_POINT('',(6.92760979279972,4.69005394727773,-2.13792482936519));
#148477=CARTESIAN_POINT('Origin',(-0.190142576289496,4.69642264810554,0.0575450801682964));
#148478=CARTESIAN_POINT('Ctrl Pts',(7.16665595397255,4.65066950061211,-2.21111791583262));
#148479=CARTESIAN_POINT('Ctrl Pts',(7.12678822298077,4.65692555494341,-2.19886951017351));
#148480=CARTESIAN_POINT('Ctrl Pts',(7.08691447053393,4.66333077480341,-2.18663861775419));
#148481=CARTESIAN_POINT('Ctrl Pts',(7.00724567148053,4.67644844950687,-2.16224357833835));
#148482=CARTESIAN_POINT('Ctrl Pts',(6.967406034475,4.68316824027248,-2.15006577416036));
#148483=CARTESIAN_POINT('Ctrl Pts',(6.92760979323705,4.69005394638669,-2.13792482742635));
#148484=CARTESIAN_POINT('Ctrl Pts',(7.118150181,4.559946053,-1.376385849));
#148485=CARTESIAN_POINT('Ctrl Pts',(7.04307702,4.62560150099999,-1.764636013));
#148486=CARTESIAN_POINT('Ctrl Pts',(6.926221658,4.690829639,-2.142417687));
#148487=CARTESIAN_POINT('Ctrl Pts',(7.31294697400001,4.559946053,-1.664573988));
#148488=CARTESIAN_POINT('Ctrl Pts',(7.222154969,4.62560150099999,-2.063449087));
#148489=CARTESIAN_POINT('Ctrl Pts',(7.088518405,4.690829639,-2.450083024));
#148490=CARTESIAN_POINT('Origin',(-0.195249611847796,4.55357612535333,0.0366497801067472));
#148491=CARTESIAN_POINT('Ctrl Pts',(7.225624826,4.690837228,-0.594008309));
#148492=CARTESIAN_POINT('Ctrl Pts',(7.193224795,4.625180297,-0.988128168));
#148493=CARTESIAN_POINT('Ctrl Pts',(7.118150181,4.559946053,-1.376385849));
#148494=CARTESIAN_POINT('Ctrl Pts',(7.11555365822817,4.55768986823893,-1.38981408867173));
#148495=CARTESIAN_POINT('Ctrl Pts',(7.11295713545635,4.55543368347798,-1.40324232834349));
#148496=CARTESIAN_POINT('Ctrl Pts',(7.49146539823089,4.690837228,-0.368556206901194));
#148497=CARTESIAN_POINT('Ctrl Pts',(7.47136259377661,4.625180297,-0.77717627114012));
#148498=CARTESIAN_POINT('Ctrl Pts',(7.40693512424965,4.55994605300001,-1.18118565373131));
#148499=CARTESIAN_POINT('Ctrl Pts',(7.40470684250641,4.55768986823893,-1.19515868011186));
#148500=CARTESIAN_POINT('Ctrl Pts',(7.40247856076304,4.55543368347799,-1.20913170649241));
#148501=CARTESIAN_POINT('',(7.22523676694344,4.69005394732446,-0.598710008128546));
#148502=CARTESIAN_POINT('Origin',(-0.198067624172564,4.69642264164339,0.0153246688116216));
#148503=CARTESIAN_POINT('Ctrl Pts',(7.47442851183213,4.65066950059866,-0.618804022328881));
#148504=CARTESIAN_POINT('Ctrl Pts',(7.43285981682515,4.65692555558568,-0.615412360954817));
#148505=CARTESIAN_POINT('Ctrl Pts',(7.39128901259814,4.66333077511546,-0.612039098318582));
#148506=CARTESIAN_POINT('Ctrl Pts',(7.30823861545105,4.67644844951654,-0.605340838244193));
#148507=CARTESIAN_POINT('Ctrl Pts',(7.26671253877903,4.68316824033724,-0.602012088546937));
#148508=CARTESIAN_POINT('Ctrl Pts',(7.22523676698526,4.69005394643149,-0.598710005741081));
#148509=CARTESIAN_POINT('Ctrl Pts',(7.247614057,4.559946053,0.185985165));
#148510=CARTESIAN_POINT('Ctrl Pts',(7.257758374,4.62560150099999,-0.209326436));
#148511=CARTESIAN_POINT('Ctrl Pts',(7.224846918,4.690829639,-0.603396233));
#148512=CARTESIAN_POINT('Ctrl Pts',(7.49980854,4.559946053,-0.053589743));
#148513=CARTESIAN_POINT('Ctrl Pts',(7.496885558,4.62560150099999,-0.462656961));
#148514=CARTESIAN_POINT('Ctrl Pts',(7.44948821,4.690829639,-0.868979523));
#148515=CARTESIAN_POINT('Origin',(-0.198563393855347,4.55357609619741,-0.00617996657845194));
#148516=CARTESIAN_POINT('Ctrl Pts',(7.184387961,4.690837228,0.973175025));
#148517=CARTESIAN_POINT('Ctrl Pts',(7.237469544,4.625180297,0.581304421));
#148518=CARTESIAN_POINT('Ctrl Pts',(7.24761405700001,4.559946053,0.185985165));
#148519=CARTESIAN_POINT('Ctrl Pts',(7.24796491406655,4.55768986825367,0.172312694520973));
#148520=CARTESIAN_POINT('Ctrl Pts',(7.24831577113324,4.55543368350747,0.158640224041953));
#148521=CARTESIAN_POINT('Ctrl Pts',(7.39554779057242,4.690837228,1.2505040473491));
#148522=CARTESIAN_POINT('Ctrl Pts',(7.46375621382002,4.625180297,0.84711578386299));
#148523=CARTESIAN_POINT('Ctrl Pts',(7.48768509770983,4.559946053,0.438701914431396));
#148524=CARTESIAN_POINT('Ctrl Pts',(7.48851269958758,4.55768986825367,0.424576555020551));
#148525=CARTESIAN_POINT('Ctrl Pts',(7.48934030146532,4.55543368350747,0.4104511956097));
#148526=CARTESIAN_POINT('',(7.18501970007959,4.69005394731586,0.968499827817111));
#148527=CARTESIAN_POINT('Origin',(-0.196731074506683,4.69642264982952,-0.0276122896330641));
#148528=CARTESIAN_POINT('Ctrl Pts',(7.43270510014593,4.650669500567,1.00244445911309));
#148529=CARTESIAN_POINT('Ctrl Pts',(7.39137915761362,4.65692555457027,0.996820785595503));
#148530=CARTESIAN_POINT('Ctrl Pts',(7.35005510013836,4.66333077464795,0.991178688674949));
#148531=CARTESIAN_POINT('Ctrl Pts',(7.26750644425091,4.6764484495285,0.979866966376405));
#148532=CARTESIAN_POINT('Ctrl Pts',(7.22623564101667,4.68316824042381,0.974191012739663));
#148533=CARTESIAN_POINT('Ctrl Pts',(7.18501969968291,4.69005394651994,0.968499829781918));
#148534=CARTESIAN_POINT('Ctrl Pts',(7.038187555,4.559946053,1.73965972));
#148535=CARTESIAN_POINT('Ctrl Pts',(7.133075012,4.62560150099999,1.355771012));
#148536=CARTESIAN_POINT('Ctrl Pts',(7.185646366,4.690829639,0.963839358));
#148537=CARTESIAN_POINT('Ctrl Pts',(7.335987395,4.559946053,1.559900299));
#148538=CARTESIAN_POINT('Ctrl Pts',(7.42107011,4.62560150099999,1.15976849));
#148539=CARTESIAN_POINT('Ctrl Pts',(7.462128226,4.690829639,0.752756495));
#148540=CARTESIAN_POINT('Origin',(-0.192592118064199,4.5535762464635,-0.0487206342586846));
#148541=CARTESIAN_POINT('Ctrl Pts',(6.807217099,4.690837228,2.494853776));
#148542=CARTESIAN_POINT('Ctrl Pts',(6.94329826,4.625180297,2.12355586));
#148543=CARTESIAN_POINT('Ctrl Pts',(7.03818755500001,4.559946053,1.73965972));
#148544=CARTESIAN_POINT('Ctrl Pts',(7.04146938649328,4.55768986808048,1.72638232719811));
#148545=CARTESIAN_POINT('Ctrl Pts',(7.04475121798669,4.55543368316111,1.71310493439622));
#148546=CARTESIAN_POINT('Ctrl Pts',(6.95382258706274,4.690837228,2.81109212166975));
#148547=CARTESIAN_POINT('Ctrl Pts',(7.10715288827251,4.625180297,2.43179764591603));
#148548=CARTESIAN_POINT('Ctrl Pts',(7.21831923756182,4.55994605300001,2.03807626900362));
#148549=CARTESIAN_POINT('Ctrl Pts',(7.22216402559709,4.55768986808048,2.02445906155847));
#148550=CARTESIAN_POINT('Ctrl Pts',(7.22600881363248,4.55543368316112,2.01084185411338));
#148551=CARTESIAN_POINT('',(6.80883909872424,4.69005394729676,2.49042368830192));
#148552=CARTESIAN_POINT('Origin',(-0.186195767971943,4.69642263429418,-0.0692580676992791));
#148553=CARTESIAN_POINT('Ctrl Pts',(7.04343665837363,4.6506695006056,2.57681975190767));
#148554=CARTESIAN_POINT('Ctrl Pts',(7.00428581767017,4.65692555448949,2.56244370101792));
#148555=CARTESIAN_POINT('Ctrl Pts',(6.96514077763763,4.66333077457468,2.54805006238074));
#148556=CARTESIAN_POINT('Ctrl Pts',(6.88695374923352,4.67644844946909,2.51925728100585));
#148557=CARTESIAN_POINT('Ctrl Pts',(6.84786799736152,4.68316824024888,2.50484202554462));
#148558=CARTESIAN_POINT('Ctrl Pts',(6.80883909785788,4.69005394636529,2.49042369020222));
#148559=CARTESIAN_POINT('Ctrl Pts',(6.499663225,4.559946053,3.211989719));
#148560=CARTESIAN_POINT('Ctrl Pts',(6.674856991,4.62560150099999,2.857474115));
#148561=CARTESIAN_POINT('Ctrl Pts',(6.810452976,4.690829639,2.486006892));
#148562=CARTESIAN_POINT('Ctrl Pts',(6.829143632,4.559946053,3.100451136));
#148563=CARTESIAN_POINT('Ctrl Pts',(6.998253672,4.62560150099999,2.727964456));
#148564=CARTESIAN_POINT('Ctrl Pts',(7.125847419,4.690829639,2.339294456));
#148565=CARTESIAN_POINT('Origin',(-0.177616212431316,4.55357612871005,-0.0889833422622244));
#148566=CARTESIAN_POINT('Ctrl Pts',(6.111748332,4.690837228,3.899875938));
#148567=CARTESIAN_POINT('Ctrl Pts',(6.324466068,4.625180297,3.566512188));
#148568=CARTESIAN_POINT('Ctrl Pts',(6.499663225,4.559946053,3.211989719));
#148569=CARTESIAN_POINT('Ctrl Pts',(6.50572257618686,4.55768986802202,3.19972824067412));
#148570=CARTESIAN_POINT('Ctrl Pts',(6.51178192737385,4.55543368304416,3.1874667623483));
#148571=CARTESIAN_POINT('Ctrl Pts',(6.18694436872914,4.690837228,4.24023665216603));
#148572=CARTESIAN_POINT('Ctrl Pts',(6.41822699307544,4.625180297,3.90277135387362));
#148573=CARTESIAN_POINT('Ctrl Pts',(6.61143279187819,4.559946053,3.54215244291806));
#148574=CARTESIAN_POINT('Ctrl Pts',(6.61811498813259,4.55768986802201,3.52968011366611));
#148575=CARTESIAN_POINT('Ctrl Pts',(6.62479718438698,4.55543368304417,3.51720778441416));
#148576=CARTESIAN_POINT('',(6.11428474814677,4.69005394729447,3.89589810483793));
#148577=CARTESIAN_POINT('Origin',(-0.166954220894603,4.69642263991986,-0.107665456760926));
#148578=CARTESIAN_POINT('Ctrl Pts',(6.32482494729747,4.65066950060335,4.03070581739704));
#148579=CARTESIAN_POINT('Ctrl Pts',(6.28967985561794,4.65692555483078,4.00824959584556));
#148580=CARTESIAN_POINT('Ctrl Pts',(6.25454421281184,4.66333077473281,3.9857774466005));
#148581=CARTESIAN_POINT('Ctrl Pts',(6.18437475129858,4.67644844948546,3.94084992472931));
#148582=CARTESIAN_POINT('Ctrl Pts',(6.14930165691324,4.68316824015411,3.91836940879909));
#148583=CARTESIAN_POINT('Ctrl Pts',(6.11428474714911,4.69005394626956,3.89589810607852));
#148584=CARTESIAN_POINT('Ctrl Pts',(5.657221867,4.559946053,4.534130649));
#148585=CARTESIAN_POINT('Ctrl Pts',(5.904530075,4.62560150099999,4.225564904));
#148586=CARTESIAN_POINT('Ctrl Pts',(6.116810374,4.690829639,3.891931506));
#148587=CARTESIAN_POINT('Ctrl Pts',(6.00297670400001,4.559946053,4.496028325));
#148588=CARTESIAN_POINT('Ctrl Pts',(6.24820667,4.62560150099999,4.168603835));
#148589=CARTESIAN_POINT('Ctrl Pts',(6.456369908,4.690829639,3.816449609));
#148590=CARTESIAN_POINT('Origin',(-0.154334695471594,4.5535761299946,-0.125085081307957));
#148591=CARTESIAN_POINT('Ctrl Pts',(5.130501005,4.690837228,5.122544235));
#148592=CARTESIAN_POINT('Ctrl Pts',(5.40990887,4.625180297,4.842702369));
#148593=CARTESIAN_POINT('Ctrl Pts',(5.657221867,4.559946053,4.534130649));
#148594=CARTESIAN_POINT('Ctrl Pts',(5.66577540917009,4.55768986806935,4.52345841886434));
#148595=CARTESIAN_POINT('Ctrl Pts',(5.67432895134019,4.55543368313859,4.51278618872872));
#148596=CARTESIAN_POINT('Ctrl Pts',(5.13077150802369,4.690837228,5.47111243079801));
#148597=CARTESIAN_POINT('Ctrl Pts',(5.42919193653825,4.625180297,5.19125581030626));
#148598=CARTESIAN_POINT('Ctrl Pts',(5.69540309763406,4.559946053,4.88060150441775));
#148599=CARTESIAN_POINT('Ctrl Pts',(5.7046102497862,4.55768986806935,4.86985724617828));
#148600=CARTESIAN_POINT('Ctrl Pts',(5.71381740193835,4.5554336831386,4.85911298793895));
#148601=CARTESIAN_POINT('',(5.13383323721505,4.69005394730716,5.11920465513332));
#148602=CARTESIAN_POINT('Origin',(-0.139906057811033,4.69642266906896,-0.141038569018334));
#148603=CARTESIAN_POINT('Ctrl Pts',(5.31047145097426,4.65066950059662,5.29612055860463));
#148604=CARTESIAN_POINT('Ctrl Pts',(5.280975456191,4.65692555473346,5.26663419557849));
#148605=CARTESIAN_POINT('Ctrl Pts',(5.25149211254357,4.66333077471736,5.23713430764837));
#148606=CARTESIAN_POINT('Ctrl Pts',(5.1926212628331,4.67644844953227,5.17817280592589));
#148607=CARTESIAN_POINT('Ctrl Pts',(5.16320080379083,4.68316824031384,5.14867819294403));
#148608=CARTESIAN_POINT('Ctrl Pts',(5.13383323576555,4.69005394642875,5.11920465637239));
#148609=CARTESIAN_POINT('Ctrl Pts',(4.550255102,4.559946053,5.644260669));
#148610=CARTESIAN_POINT('Ctrl Pts',(4.858113896,4.625601501,5.396072974));
#148611=CARTESIAN_POINT('Ctrl Pts',(5.13715251700001,4.690829639,5.115873729));
#148612=CARTESIAN_POINT('Ctrl Pts',(4.896117256,4.559946053,5.681376225));
#148613=CARTESIAN_POINT('Ctrl Pts',(5.206000469,4.62560150099999,5.41432393300001));
#148614=CARTESIAN_POINT('Ctrl Pts',(5.484999715,4.690829639,5.115151819));
#148615=CARTESIAN_POINT('Origin',(-0.123836949338866,4.55357611375428,-0.155338165372497));
#148616=CARTESIAN_POINT('Ctrl Pts',(3.909357153,4.690837228,6.105688057));
#148617=CARTESIAN_POINT('Ctrl Pts',(4.242390347,4.625180297,5.89245317));
#148618=CARTESIAN_POINT('Ctrl Pts',(4.550255102,4.559946053,5.644260669));
#148619=CARTESIAN_POINT('Ctrl Pts',(4.56090288055171,4.55768986818893,5.63567670884894));
#148620=CARTESIAN_POINT('Ctrl Pts',(4.57155065910353,4.55543368337775,5.62709274869774));
#148621=CARTESIAN_POINT('Ctrl Pts',(3.83468947317842,4.690837228,6.44616507150887));
#148622=CARTESIAN_POINT('Ctrl Pts',(4.1862938986332,4.625180297,6.23700291524664));
#148623=CARTESIAN_POINT('Ctrl Pts',(4.51306268385255,4.559946053,5.99083906467175));
#148624=CARTESIAN_POINT('Ctrl Pts',(4.52436427523683,4.55768986818893,5.98232526721429));
#148625=CARTESIAN_POINT('Ctrl Pts',(4.53566586662106,4.55543368337774,5.97381146975693));
#148626=CARTESIAN_POINT('',(3.91332939128576,4.6900539473128,6.10314288704862));
#148627=CARTESIAN_POINT('Origin',(-0.106316020040327,4.69642264970412,-0.167816826224749));
#148628=CARTESIAN_POINT('Ctrl Pts',(4.04780621107473,4.65066950059032,6.31389458846495));
#148629=CARTESIAN_POINT('Ctrl Pts',(4.02533850998926,4.65692555549962,6.27875682893648));
#148630=CARTESIAN_POINT('Ctrl Pts',(4.00288607620138,4.66333077502009,6.24360858738517));
#148631=CARTESIAN_POINT('Ctrl Pts',(3.95806657571596,4.67644844940684,6.17337008282733));
#148632=CARTESIAN_POINT('Ctrl Pts',(3.93567442061857,4.6831682401762,6.13824050868851));
#148633=CARTESIAN_POINT('Ctrl Pts',(3.91332938909123,4.69005394628826,6.10314288824477));
#148634=CARTESIAN_POINT('Ctrl Pts',(3.230523466,4.559946053,6.490471334));
#148635=CARTESIAN_POINT('Ctrl Pts',(3.58453771,4.625601501,6.314266669));
#148636=CARTESIAN_POINT('Ctrl Pts',(3.917287119,4.690829639,6.100603383));
#148637=CARTESIAN_POINT('Ctrl Pts',(3.560320807,4.559946053,6.601069288));
#148638=CARTESIAN_POINT('Ctrl Pts',(3.920367472,4.625601501,6.406876261));
#148639=CARTESIAN_POINT('Ctrl Pts',(4.257157031,4.690829639,6.174675215));
#148640=CARTESIAN_POINT('Origin',(-0.0875486605970938,4.55357615413023,
-0.178327839154758));
#148641=CARTESIAN_POINT('Ctrl Pts',(2.505416106,4.690837228,6.803336691));
#148642=CARTESIAN_POINT('Ctrl Pts',(2.876502367,4.625180297,6.66667941000001));
#148643=CARTESIAN_POINT('Ctrl Pts',(3.230523466,4.559946053,6.49047133400001));
#148644=CARTESIAN_POINT('Ctrl Pts',(3.24276760300522,4.55768986820418,6.48437701976261));
#148645=CARTESIAN_POINT('Ctrl Pts',(3.2550117400105,4.55543368340826,6.47828270552523));
#148646=CARTESIAN_POINT('Ctrl Pts',(2.35930162164539,4.690837228,7.11980219913421));
#148647=CARTESIAN_POINT('Ctrl Pts',(2.74764941145802,4.625180297,6.99111469553954));
#148648=CARTESIAN_POINT('Ctrl Pts',(3.11969647505973,4.559946053,6.8209516482439));
#148649=CARTESIAN_POINT('Ctrl Pts',(3.13256405620673,4.55768986820418,6.81506640674221));
#148650=CARTESIAN_POINT('Ctrl Pts',(3.14543163735375,4.55543368340825,6.8091811652404));
#148651=CARTESIAN_POINT('',(2.50984261151385,4.69005394727773,6.80170493911411));
#148652=CARTESIAN_POINT('Origin',(-0.0677547966760533,4.69642265928317,
-0.186748302139411));
#148653=CARTESIAN_POINT('Ctrl Pts',(2.59587005248643,4.65066950060226,7.03643792480017));
#148654=CARTESIAN_POINT('Ctrl Pts',(2.58148121593871,4.6569255544196,6.99729178184832));
#148655=CARTESIAN_POINT('Ctrl Pts',(2.5671095390213,4.66333077457138,6.9581386729951));
#148656=CARTESIAN_POINT('Ctrl Pts',(2.53843709451609,4.67644844951328,6.87990743449515));
#148657=CARTESIAN_POINT('Ctrl Pts',(2.52412027548077,4.68316824029878,6.84078551863943));
#148658=CARTESIAN_POINT('Ctrl Pts',(2.50984260926869,4.69005394637568,6.80170493977542));
#148659=CARTESIAN_POINT('Ctrl Pts',(1.759736143,4.559946053,7.033194773));
#148660=CARTESIAN_POINT('Ctrl Pts',(2.143352525,4.625601501,6.937212273));
#148661=CARTESIAN_POINT('Ctrl Pts',(2.514253728,4.690829639,6.800075602));
#148662=CARTESIAN_POINT('Ctrl Pts',(2.058047714,4.559946053,7.212103688));
#148663=CARTESIAN_POINT('Ctrl Pts',(2.451422449,4.62560150099999,7.099850175));
#148664=CARTESIAN_POINT('Ctrl Pts',(2.830254416,4.690829639,6.945477661));
#148665=CARTESIAN_POINT('Origin',(-0.0471666674588023,4.55357609672683,
-0.192979181603469));
#148666=CARTESIAN_POINT('Ctrl Pts',(0.984324587,4.690837228,7.182868863));
#148667=CARTESIAN_POINT('Ctrl Pts',(1.376112332,4.625180297,7.12917913000001));
#148668=CARTESIAN_POINT('Ctrl Pts',(1.759736143,4.559946053,7.03319477300001));
#148669=CARTESIAN_POINT('Ctrl Pts',(1.77300411626669,4.55768986821522,7.02987506800209));
#148670=CARTESIAN_POINT('Ctrl Pts',(1.78627208953345,4.55543368343031,7.02655536300417));
#148671=CARTESIAN_POINT('Ctrl Pts',(0.773595447487644,4.690837228,7.46052528797172));
#148672=CARTESIAN_POINT('Ctrl Pts',(1.18052789164313,4.625180297,7.41832972190833));
#148673=CARTESIAN_POINT('Ctrl Pts',(1.58045672673534,4.559946053,7.33212411374831));
#148674=CARTESIAN_POINT('Ctrl Pts',(1.5942886238711,4.55768986821521,7.32914261554172));
#148675=CARTESIAN_POINT('Ctrl Pts',(1.60812052100694,4.55543368343032,7.32616111733499));
#148676=CARTESIAN_POINT('',(0.988998381079286,4.69005394732039,7.18222682883565));
#148677=CARTESIAN_POINT('Origin',(-0.0260253471886281,4.696422661911,-0.196947453086742));
#148678=CARTESIAN_POINT('Ctrl Pts',(1.02255389472724,4.65066950055004,7.42996524443305));
#148679=CARTESIAN_POINT('Ctrl Pts',(1.01691672373786,4.65692555553897,7.3886411342729));
#148680=CARTESIAN_POINT('Ctrl Pts',(1.01129781035109,4.6633307750339,7.34731392216206));
#148681=CARTESIAN_POINT('Ctrl Pts',(1.00011311603079,4.67644844948152,7.26474796181685));
#148682=CARTESIAN_POINT('Ctrl Pts',(0.994541071871806,4.68316824025307,
7.22346300196127));
#148683=CARTESIAN_POINT('Ctrl Pts',(0.988998378924648,4.69005394639712,
7.18222682897109));
#148684=CARTESIAN_POINT('Ctrl Pts',(0.206665513,4.559946053,7.24705384));
#148685=CARTESIAN_POINT('Ctrl Pts',(0.601946558,4.625601501,7.235781541));
#148686=CARTESIAN_POINT('Ctrl Pts',(0.993656627,4.690829639,7.18158384400001));
#148687=CARTESIAN_POINT('Ctrl Pts',(0.459542598,4.559946053,7.48590813500001));
#148688=CARTESIAN_POINT('Ctrl Pts',(0.867851637,4.625601501,7.460842987));
#148689=CARTESIAN_POINT('Ctrl Pts',(1.271012251,4.690829639,7.391517291));
#148690=CARTESIAN_POINT('Origin',(-0.00457906475628513,4.55357619680332,
-0.198606302057152));
#148691=CARTESIAN_POINT('Ctrl Pts',(-0.582792857,4.690837228,7.226538071));
#148692=CARTESIAN_POINT('Ctrl Pts',(-0.188623186,4.625180297,7.25832635800001));
#148693=CARTESIAN_POINT('Ctrl Pts',(0.206665513,4.559946053,7.24705384000001));
#148694=CARTESIAN_POINT('Ctrl Pts',(0.220336926796758,4.55768986822747,
7.24666396986584));
#148695=CARTESIAN_POINT('Ctrl Pts',(0.23400834059351,4.55543368345483,7.24627409973171));
#148696=CARTESIAN_POINT('Ctrl Pts',(-0.848283189425317,4.690837228,7.4524025062321));
#148697=CARTESIAN_POINT('Ctrl Pts',(-0.441793800398394,4.625180297,7.49867189599384));
#148698=CARTESIAN_POINT('Ctrl Pts',(-0.0326834214049662,4.559946053,7.50045460502951));
#148699=CARTESIAN_POINT('Ctrl Pts',(-0.0185339724226994,4.55768986822747,
7.50051626161866));
#148700=CARTESIAN_POINT('Ctrl Pts',(-0.00438452344043182,4.55543368345484,
7.50057791820777));
#148701=CARTESIAN_POINT('Origin',(0.0169209768713816,4.69642267005817,-0.197936617773742));
#148702=CARTESIAN_POINT('Ctrl Pts',(0.185936733414184,1.19354381562152,
7.24766508350195));
#148703=CARTESIAN_POINT('Ctrl Pts',(0.199362613707092,1.19575849481077,
7.24727086225092));
#148704=CARTESIAN_POINT('Ctrl Pts',(0.212788494,1.197973174,7.24687664100001));
#148705=CARTESIAN_POINT('Ctrl Pts',(0.605187736,1.262701774,7.235354706));
#148706=CARTESIAN_POINT('Ctrl Pts',(0.994048608,1.327878141,7.181529598));
#148707=CARTESIAN_POINT('Ctrl Pts',(0.438644102144323,1.19354381562152,
7.48773050957685));
#148708=CARTESIAN_POINT('Ctrl Pts',(0.452512997286711,1.19575849481077,
7.48686647008995));
#148709=CARTESIAN_POINT('Ctrl Pts',(0.4663818924291,1.197973174,7.48600243060295));
#148710=CARTESIAN_POINT('Ctrl Pts',(0.871729163708226,1.262701774,7.46074908167134));
#148711=CARTESIAN_POINT('Ctrl Pts',(1.27197966967496,1.327878141,7.39187474060707));
#148712=CARTESIAN_POINT('',(0.465867290474915,1.19797317454244,7.48551719487009));
#148713=CARTESIAN_POINT('',(1.02478075909889,1.28783500463657,7.42965843038126));
#148714=CARTESIAN_POINT('Origin',(-0.0343001365998186,1.3392712291817,-0.188172451741534));
#148715=CARTESIAN_POINT('Ctrl Pts',(0.989408718109874,1.32710049318168,
7.18217031322073));
#148716=CARTESIAN_POINT('Ctrl Pts',(0.995257838777893,1.32022179850708,
7.22336221123387));
#148717=CARTESIAN_POINT('Ctrl Pts',(1.00113448834787,1.31351590008605,7.26460533817788));
#148718=CARTESIAN_POINT('Ctrl Pts',(1.01292420902814,1.30043858906419,7.34708728067027));
#148719=CARTESIAN_POINT('Ctrl Pts',(1.01884421512627,1.29405949360237,7.38837459858889));
#148720=CARTESIAN_POINT('Ctrl Pts',(1.02478075183884,1.28783500497465,7.42965843147621));
#148721=CARTESIAN_POINT('',(0.33932788589724,1.19797317561448,7.36619691796539));
#148722=CARTESIAN_POINT('Origin',(1.68105546843877E-13,1.28891220999972,
1.7056668577542E-12));
#148723=CARTESIAN_POINT('',(1.03018391903461,1.10830076261691,7.42891116439694));
#148724=CARTESIAN_POINT('Origin',(-0.0506334157325571,0.946580201577215,
-0.177557611465953));
#148725=CARTESIAN_POINT('',(1.58702106594482,1.19797317379345,7.33016808366918));
#148726=CARTESIAN_POINT('Origin',(-0.0611523990559881,1.3391753255225,-0.175905147922946));
#148727=CARTESIAN_POINT('Ctrl Pts',(1.02478076605977,1.28783500273371,7.42965842925219));
#148728=CARTESIAN_POINT('Ctrl Pts',(1.17943657663153,1.26310656756624,7.40832658743055));
#148729=CARTESIAN_POINT('Ctrl Pts',(1.33303195897402,1.23856749894444,7.38221557285522));
#148730=CARTESIAN_POINT('Ctrl Pts',(1.48513956610284,1.21428571401564,7.35148695569467));
#148731=CARTESIAN_POINT('Ctrl Pts',(1.51912281059599,1.20886077966551,7.3446216968484));
#148732=CARTESIAN_POINT('Ctrl Pts',(1.55308500096562,1.20342302059143,7.33751542487673));
#148733=CARTESIAN_POINT('Ctrl Pts',(1.58702106529159,1.1979731751026,7.33016808322343));
#148734=CARTESIAN_POINT('Ctrl Pts',(0.984685745,1.327885473,7.182819362));
#148735=CARTESIAN_POINT('Ctrl Pts',(1.329357467,1.27059961,7.135568649));
#148736=CARTESIAN_POINT('Ctrl Pts',(1.667921256,1.214285714,7.055532488));
#148737=CARTESIAN_POINT('Ctrl Pts',(1.71688224,1.20614195,7.043958157));
#148738=CARTESIAN_POINT('Ctrl Pts',(1.76567788,1.197973174,7.031705456));
#148739=CARTESIAN_POINT('Ctrl Pts',(0.774406033,1.327885473,7.45991255300001));
#148740=CARTESIAN_POINT('Ctrl Pts',(1.132374232,1.27059961,7.422752234));
#148741=CARTESIAN_POINT('Ctrl Pts',(1.485139566,1.214285714,7.351486956));
#148742=CARTESIAN_POINT('Ctrl Pts',(1.536154289,1.20614195,7.341181016));
#148743=CARTESIAN_POINT('Ctrl Pts',(1.587021072,1.197973174,7.330168082));
#148744=CARTESIAN_POINT('',(1.67634947204994,1.19797317334243,7.18093676992212));
#148745=CARTESIAN_POINT('Ctrl Pts',(1.73962338946964,1.19354381543301,7.03824780020232));
#148746=CARTESIAN_POINT('Ctrl Pts',(1.75265063473478,1.19575849471651,7.03497662810107));
#148747=CARTESIAN_POINT('Ctrl Pts',(1.76567788,1.197973174,7.031705456));
#148748=CARTESIAN_POINT('Ctrl Pts',(2.146426169,1.262701774,6.93609866));
#148749=CARTESIAN_POINT('Ctrl Pts',(2.514624883,1.327878141,6.79993836));
#148750=CARTESIAN_POINT('Ctrl Pts',(2.0380295685556,1.19354381543301,7.21837601620528));
#148751=CARTESIAN_POINT('Ctrl Pts',(2.05138847430055,1.19575849471651,7.21455077483569));
#148752=CARTESIAN_POINT('Ctrl Pts',(2.06474738004543,1.197973174,7.21072553346622));
#148753=CARTESIAN_POINT('Ctrl Pts',(2.45518913513104,1.262701774,7.09892491278304));
#148754=CARTESIAN_POINT('Ctrl Pts',(2.83127605897128,1.327878141,6.94561878728958));
#148755=CARTESIAN_POINT('',(2.06414049783414,1.19797317454228,7.21036226646249));
#148756=CARTESIAN_POINT('',(2.59797889809418,1.28783500532718,7.03565957433808));
#148757=CARTESIAN_POINT('Origin',(-0.0739496577934162,1.33927125484505,
-0.176399334544752));
#148758=CARTESIAN_POINT('Ctrl Pts',(2.51023120581304,1.32710049342706,6.80156153359947));
#148759=CARTESIAN_POINT('Ctrl Pts',(2.52479861772659,1.32022179873707,6.84053299994383));
#148760=CARTESIAN_POINT('Ctrl Pts',(2.53940392803343,1.31351590010745,6.879548580739));
#148761=CARTESIAN_POINT('Ctrl Pts',(2.56864919096453,1.30043858906367,6.9575676999095));
#148762=CARTESIAN_POINT('Ctrl Pts',(2.58330634344234,1.29405949359074,6.9966171170184));
#148763=CARTESIAN_POINT('Ctrl Pts',(2.59797889086842,1.2878350049529,7.03565957699392));
#148764=CARTESIAN_POINT('',(1.91490918273655,1.19797317561398,7.12103386262548));
#148765=CARTESIAN_POINT('Origin',(-5.00684563253806E-13,1.28891221000011,
-1.27068494615301E-12));
#148766=CARTESIAN_POINT('',(2.60309509487799,1.10830076264129,7.03376825908983));
#148767=CARTESIAN_POINT('Origin',(-0.0876193715913992,0.946580153350199,
-0.162521999439057));
#148768=CARTESIAN_POINT('',(3.12568685541228,1.19797317358554,6.81763021082559));
#148769=CARTESIAN_POINT('Origin',(-0.0975371600697084,1.33917533439657,
-0.158646804040897));
#148770=CARTESIAN_POINT('Ctrl Pts',(2.59797890492865,1.28783500479139,7.03565957174917));
#148771=CARTESIAN_POINT('Ctrl Pts',(2.74443323278555,1.26310656825283,6.98158002875429));
#148772=CARTESIAN_POINT('Ctrl Pts',(2.88882454394555,1.23856749894685,6.92306100842335));
#148773=CARTESIAN_POINT('Ctrl Pts',(3.03077021551452,1.21428571428671,6.86035217031531));
#148774=CARTESIAN_POINT('Ctrl Pts',(3.06248312300961,1.20886077964635,6.84634202432027));
#148775=CARTESIAN_POINT('Ctrl Pts',(3.09412365775973,1.20342302038954,6.83210102606699));
#148776=CARTESIAN_POINT('Ctrl Pts',(3.12568685454725,1.19797317447889,6.8176302105138));
#148777=CARTESIAN_POINT('Ctrl Pts',(2.50575818,1.327885473,6.803210709));
#148778=CARTESIAN_POINT('Ctrl Pts',(2.832214162,1.27059961,6.68297046));
#148779=CARTESIAN_POINT('Ctrl Pts',(3.145657109,1.214285714,6.532024292));
#148780=CARTESIAN_POINT('Ctrl Pts',(3.190985273,1.20614195,6.510195399));
#148781=CARTESIAN_POINT('Ctrl Pts',(3.236006129,1.197973174,6.487739539));
#148782=CARTESIAN_POINT('Ctrl Pts',(2.359961536,1.327885473,7.119029537));
#148783=CARTESIAN_POINT('Ctrl Pts',(2.701572267,1.27059961,7.005785424));
#148784=CARTESIAN_POINT('Ctrl Pts',(3.030770215,1.214285714,6.86035217));
#148785=CARTESIAN_POINT('Ctrl Pts',(3.07837677,1.20614195,6.83932052));
#148786=CARTESIAN_POINT('Ctrl Pts',(3.125686861,1.197973174,6.817630208));
#148787=CARTESIAN_POINT('',(3.18084649134048,1.19797317334242,6.65268487524972));
#148788=CARTESIAN_POINT('Ctrl Pts',(3.21196718935855,1.19354381559223,6.49972987172989));
#148789=CARTESIAN_POINT('Ctrl Pts',(3.22398665917931,1.19575849479612,6.49373470536499));
#148790=CARTESIAN_POINT('Ctrl Pts',(3.236006129,1.197973174,6.487739539));
#148791=CARTESIAN_POINT('Ctrl Pts',(3.587300101,1.262701774,6.312518349));
#148792=CARTESIAN_POINT('Ctrl Pts',(3.917620093,1.327878141,6.100389562));
#148793=CARTESIAN_POINT('Ctrl Pts',(3.54211904043812,1.19354381559227,6.61149828219364));
#148794=CARTESIAN_POINT('Ctrl Pts',(3.55434330812815,1.19575849479612,6.60489070320868));
#148795=CARTESIAN_POINT('Ctrl Pts',(3.56656757581818,1.197973174,6.59828312422371));
#148796=CARTESIAN_POINT('Ctrl Pts',(3.92384719094914,1.262701774,6.40516290331904));
#148797=CARTESIAN_POINT('Ctrl Pts',(4.2581851262025,1.327878141,6.17459341925963));
#148798=CARTESIAN_POINT('',(3.56589679053256,1.19797317454273,6.59805881195249));
#148799=CARTESIAN_POINT('',(4.04969843096104,1.28783500531603,6.31268109581324));
#148800=CARTESIAN_POINT('Origin',(-0.110141529144904,1.33927128274808,-0.156378435332287));
#148801=CARTESIAN_POINT('Ctrl Pts',(3.91367807191636,1.32710049343035,6.10291929740531));
#148802=CARTESIAN_POINT('Ctrl Pts',(3.93628261917909,1.32022179874713,6.13784806949174));
#148803=CARTESIAN_POINT('Ctrl Pts',(3.95893366204737,1.31351590012205,6.17281177761949));
#148804=CARTESIAN_POINT('Ctrl Pts',(4.00426699143525,1.30043858907086,6.24271998600702));
#148805=CARTESIAN_POINT('Ctrl Pts',(4.02697593828508,1.2940594935786,6.27770559496417));
#148806=CARTESIAN_POINT('Ctrl Pts',(4.04969842453934,1.28783500493535,6.31268109991297));
#148807=CARTESIAN_POINT('',(3.40095145402154,1.19797317561536,6.54289917816694));
#148808=CARTESIAN_POINT('Origin',(-1.27719015918792E-13,1.28891221000006,
-3.73399228204008E-13));
#148809=CARTESIAN_POINT('',(4.05428843735942,1.10830076263197,6.30973416717019));
#148810=CARTESIAN_POINT('Origin',(-0.120508283964545,0.946580168666976,
-0.139886719195316));
#148811=CARTESIAN_POINT('',(4.5181990013075,1.19797317358556,5.98630752524413));
#148812=CARTESIAN_POINT('Origin',(-0.12936110692105,1.33917530843295,-0.133970025641706));
#148813=CARTESIAN_POINT('Ctrl Pts',(4.0496984370823,1.28783500479117,6.31268109195239));
#148814=CARTESIAN_POINT('Ctrl Pts',(4.18110324087616,1.26310656824494,6.22838254735657));
#148815=CARTESIAN_POINT('Ctrl Pts',(4.30953890387345,1.2385674989391,6.14019180548056));
#148816=CARTESIAN_POINT('Ctrl Pts',(4.43468541808166,1.21428571428671,6.04843494159059));
#148817=CARTESIAN_POINT('Ctrl Pts',(4.46264512820046,1.20886077964635,6.0279350073175));
#148818=CARTESIAN_POINT('Ctrl Pts',(4.49048453128707,1.20342302038954,6.00722517591836));
#148819=CARTESIAN_POINT('Ctrl Pts',(4.51819900073097,1.1979731744789,5.98630752549464));
#148820=CARTESIAN_POINT('Ctrl Pts',(3.909664147,1.327885473,6.105491484));
#148821=CARTESIAN_POINT('Ctrl Pts',(4.202639671,1.27059961,5.917883999));
#148822=CARTESIAN_POINT('Ctrl Pts',(4.476305531,1.214285714,5.703085901));
#148823=CARTESIAN_POINT('Ctrl Pts',(4.515881381,1.20614195,5.672023139));
#148824=CARTESIAN_POINT('Ctrl Pts',(4.555022329,1.197973174,5.640414132));
#148825=CARTESIAN_POINT('Ctrl Pts',(3.83516786,1.327885473,6.445268612));
#148826=CARTESIAN_POINT('Ctrl Pts',(4.144447785,1.27059961,6.261235875));
#148827=CARTESIAN_POINT('Ctrl Pts',(4.434685418,1.214285714,6.048434942));
#148828=CARTESIAN_POINT('Ctrl Pts',(4.476657775,1.20614195,6.017660998));
#148829=CARTESIAN_POINT('Ctrl Pts',(4.518199006,1.197973174,5.986307521));
#148830=CARTESIAN_POINT('',(4.53661066430225,1.19797317334244,5.81336082899545));
#148831=CARTESIAN_POINT('Ctrl Pts',(4.53412297316432,1.19354381550648,5.65729179919426));
#148832=CARTESIAN_POINT('Ctrl Pts',(4.54457265108221,1.19575849475325,5.64885296559718));
#148833=CARTESIAN_POINT('Ctrl Pts',(4.555022329,1.197973174,5.640414132));
#148834=CARTESIAN_POINT('Ctrl Pts',(4.860435866,1.262701774,5.393771696));
#148835=CARTESIAN_POINT('Ctrl Pts',(5.137431742,1.327878141,5.115593328));
#148836=CARTESIAN_POINT('Ctrl Pts',(4.88058296147161,1.19354381550649,5.6954742368475));
#148837=CARTESIAN_POINT('Ctrl Pts',(4.89110099861214,1.19575849475325,5.68639328303249));
#148838=CARTESIAN_POINT('Ctrl Pts',(4.90161903575277,1.197973174,5.67731232921733));
#148839=CARTESIAN_POINT('Ctrl Pts',(5.20903051299453,1.262701774,5.41190259641749));
#148840=CARTESIAN_POINT('Ctrl Pts',(5.48598619042316,1.327878141,5.11485092450687));
#148841=CARTESIAN_POINT('',(4.90091571257073,1.19797317454213,5.67723746024605));
#148842=CARTESIAN_POINT('',(5.3120585661549,1.28783500526933,5.29452866540395));
#148843=CARTESIAN_POINT('Origin',(-0.141183120933982,1.33927122549754,-0.129045132535002));
#148844=CARTESIAN_POINT('Ctrl Pts',(5.13412570213364,1.32710049328122,5.11891133824004));
#148845=CARTESIAN_POINT('Ctrl Pts',(5.16371042111886,1.32022179857526,5.14816418556892));
#148846=CARTESIAN_POINT('Ctrl Pts',(5.19334805826089,1.31351590007935,5.1774411563661));
#148847=CARTESIAN_POINT('Ctrl Pts',(5.25264971787425,1.30043858901147,5.2359696239467));
#148848=CARTESIAN_POINT('Ctrl Pts',(5.28234861391981,1.29405949351238,5.26525553654629));
#148849=CARTESIAN_POINT('Ctrl Pts',(5.31205856075306,1.28783500486646,5.29452867077809));
#148850=CARTESIAN_POINT('',(4.72796901574343,1.19797317561354,5.65882579998064));
#148851=CARTESIAN_POINT('Origin',(-1.15055534544162E-12,1.28891221000022,
-1.02955838299224E-12));
#148852=CARTESIAN_POINT('',(5.31590775787216,1.1083007626196,5.29066391891825));
#148853=CARTESIAN_POINT('Origin',(-0.147762399972118,0.946580160935038,
-0.110710555889455));
#148854=CARTESIAN_POINT('',(5.69944518326462,1.19797317358555,4.87507175408001));
#148855=CARTESIAN_POINT('Origin',(-0.155136266855465,1.33917526459104,-0.103029040302565));
#148856=CARTESIAN_POINT('Ctrl Pts',(5.31205857130684,1.28783500479147,5.29452866032525));
#148857=CARTESIAN_POINT('Ctrl Pts',(5.4222695085429,1.26310656822242,5.18395282036736));
#148858=CARTESIAN_POINT('Ctrl Pts',(5.52874401441177,1.23856749891666,5.07021405812116));
#148859=CARTESIAN_POINT('Ctrl Pts',(5.63123965918988,1.21428571428671,4.95369961753505));
#148860=CARTESIAN_POINT('Ctrl Pts',(5.65413880693855,1.20886077964635,4.92766844913164));
#148861=CARTESIAN_POINT('Ctrl Pts',(5.67687533869773,1.20342302038954,4.90145815332447));
#148862=CARTESIAN_POINT('Ctrl Pts',(5.69944518263217,1.1979731744789,4.87507175436124));
#148863=CARTESIAN_POINT('Ctrl Pts',(5.130758564,1.327885473,5.122286263));
#148864=CARTESIAN_POINT('Ctrl Pts',(5.376554419,1.27059961,4.87608386));
#148865=CARTESIAN_POINT('Ctrl Pts',(5.597646882,1.214285714,4.607477551));
#148866=CARTESIAN_POINT('Ctrl Pts',(5.629619895,1.20614195,4.568633382));
#148867=CARTESIAN_POINT('Ctrl Pts',(5.661050747,1.197973174,4.529349229));
#148868=CARTESIAN_POINT('Ctrl Pts',(5.131045997,1.327885473,5.470134091));
#148869=CARTESIAN_POINT('Ctrl Pts',(5.393533531,1.27059961,5.223917895));
#148870=CARTESIAN_POINT('Ctrl Pts',(5.631239659,1.214285714,4.953699618));
#148871=CARTESIAN_POINT('Ctrl Pts',(5.66561523700001,1.20614195,4.914622335));
#148872=CARTESIAN_POINT('Ctrl Pts',(5.69944518700001,1.197973174,4.875071749));
#148873=CARTESIAN_POINT('',(5.68005599221442,1.19797317334244,4.70048187952442));
#148874=CARTESIAN_POINT('Ctrl Pts',(5.64426820565414,1.19354381542033,4.5503250498189));
#148875=CARTESIAN_POINT('Ctrl Pts',(5.65265947632706,1.19575849471018,4.53983713940944));
#148876=CARTESIAN_POINT('Ctrl Pts',(5.661050747,1.197973174,4.529349229));
#148877=CARTESIAN_POINT('Ctrl Pts',(5.906303053,1.262701774,4.222818274));
#148878=CARTESIAN_POINT('Ctrl Pts',(6.117022792,1.327878141,3.891597635));
#148879=CARTESIAN_POINT('Ctrl Pts',(5.99083624772278,1.19354381542033,4.51313614705207));
#148880=CARTESIAN_POINT('Ctrl Pts',(5.99915624252742,1.19575849471018,4.50200643361165));
#148881=CARTESIAN_POINT('Ctrl Pts',(6.00747623733207,1.197973174,4.49087672017117));
#148882=CARTESIAN_POINT('Ctrl Pts',(6.2506453581102,1.262701774,4.16558773918303));
#148883=CARTESIAN_POINT('Ctrl Pts',(6.45726863652832,1.327878141,3.81594368619315));
#148884=CARTESIAN_POINT('',(6.00677326593869,1.19797317455196,4.49095479280212));
#148885=CARTESIAN_POINT('',(6.32603274683486,1.28783500530512,4.02880995908792));
#148886=CARTESIAN_POINT('Origin',(-0.165623100425537,1.33927121971452,-0.0956778453126561));
#148887=CARTESIAN_POINT('Ctrl Pts',(6.11450732031872,1.32710049321789,3.89554877299147));
#148888=CARTESIAN_POINT('Ctrl Pts',(6.14968886265092,1.32022179849916,3.91775786528613));
#148889=CARTESIAN_POINT('Ctrl Pts',(6.18492727127714,1.31351590008441,3.93997914081815));
#148890=CARTESIAN_POINT('Ctrl Pts',(6.25542438165227,1.3004385890187,3.9843911417831));
#148891=CARTESIAN_POINT('Ctrl Pts',(6.29072453942237,1.29405949355432,4.00660798123664));
#148892=CARTESIAN_POINT('Ctrl Pts',(6.32603274273498,1.28783500492533,4.02880996550155));
#148893=CARTESIAN_POINT('',(5.83391200081423,1.1979731756145,4.51015201700134));
#148894=CARTESIAN_POINT('Origin',(-2.24213009270002E-13,1.28891221000022,
-1.85615411929518E-13));
#148895=CARTESIAN_POINT('',(6.3289611403479,1.10830076260042,4.02420810597705));
#148896=CARTESIAN_POINT('Origin',(-0.16810700650616,0.94658017581024,-0.0763574613611706));
#148897=CARTESIAN_POINT('',(6.61419164333604,1.19797317358555,3.53588304568532));
#148898=CARTESIAN_POINT('Origin',(-0.173657580831476,1.33917535067201,-0.0672706207730239));
#148899=CARTESIAN_POINT('Ctrl Pts',(6.32603275069163,1.2878350047913,4.02880995297333));
#148900=CARTESIAN_POINT('Ctrl Pts',(6.40989648052783,1.26310656823714,3.89712722091806));
#148901=CARTESIAN_POINT('Ctrl Pts',(6.4894311999038,1.23856749893131,3.76315873619561));
#148902=CARTESIAN_POINT('Ctrl Pts',(6.56448339291637,1.21428571428671,3.62733480452593));
#148903=CARTESIAN_POINT('Ctrl Pts',(6.58125123958283,1.20886077964635,3.59698959050278));
#148904=CARTESIAN_POINT('Ctrl Pts',(6.59782176496324,1.20342302038954,3.5665043947356));
#148905=CARTESIAN_POINT('Ctrl Pts',(6.61419164258928,1.1979731744789,3.53588304601582));
#148906=CARTESIAN_POINT('Ctrl Pts',(6.11194441300001,1.327885473,3.89956863));
#148907=CARTESIAN_POINT('Ctrl Pts',(6.299067458,1.27059961,3.606283458));
#148908=CARTESIAN_POINT('Ctrl Pts',(6.457248486,1.214285714,3.296428672));
#148909=CARTESIAN_POINT('Ctrl Pts',(6.48012364,1.20614195,3.251619405));
#148910=CARTESIAN_POINT('Ctrl Pts',(6.50237472400001,1.197973174,3.20649699));
#148911=CARTESIAN_POINT('Ctrl Pts',(6.187002127,1.327885473,4.239222179));
#148912=CARTESIAN_POINT('Ctrl Pts',(6.390423644,1.27059961,3.94233532));
#148913=CARTESIAN_POINT('Ctrl Pts',(6.564483393,1.214285714,3.627334805));
#148914=CARTESIAN_POINT('Ctrl Pts',(6.589654828,1.20614195,3.581781394));
#148915=CARTESIAN_POINT('Ctrl Pts',(6.61419164600001,1.197973174,3.53588304));
#148916=CARTESIAN_POINT('',(6.55772409853652,1.19797317334244,3.36954308835721));
#148917=CARTESIAN_POINT('Ctrl Pts',(6.49049373074944,1.19354381548256,3.23059015776105));
#148918=CARTESIAN_POINT('Ctrl Pts',(6.49643422737473,1.19575849474129,3.21854357388049));
#148919=CARTESIAN_POINT('Ctrl Pts',(6.502374724,1.197973174,3.20649699));
#148920=CARTESIAN_POINT('Ctrl Pts',(6.675998073,1.262701774,2.854410562));
#148921=CARTESIAN_POINT('Ctrl Pts',(6.810588656,1.327878141,2.485635163));
#148922=CARTESIAN_POINT('Ctrl Pts',(6.82096468986463,1.19354381548255,3.11976882592563));
#148923=CARTESIAN_POINT('Ctrl Pts',(6.82669760832052,1.19575849474129,3.10711076623171));
#148924=CARTESIAN_POINT('Ctrl Pts',(6.83243052677644,1.197973174,3.09445270653778));
#148925=CARTESIAN_POINT('Ctrl Pts',(6.99998697275172,1.262701774,2.72449462819314));
#148926=CARTESIAN_POINT('Ctrl Pts',(7.12661637784409,1.327878141,2.3386071622032));
#148927=CARTESIAN_POINT('',(6.83176077378476,1.19797317455225,3.09468007193932));
#148928=CARTESIAN_POINT('',(7.04420866687487,1.28783500530334,2.57470857667843));
#148929=CARTESIAN_POINT('Origin',(-0.182318938186159,1.33927122879218,-0.0578369172733556));
#148930=CARTESIAN_POINT('Ctrl Pts',(6.80898137204789,1.32710049322087,2.49003467782965));
#148931=CARTESIAN_POINT('Ctrl Pts',(6.84811468746185,1.32022179853825,2.50416154198524));
#148932=CARTESIAN_POINT('Ctrl Pts',(6.88730615901088,1.31351590010567,2.51828808012451));
#148933=CARTESIAN_POINT('Ctrl Pts',(6.96570235315265,1.30043858905459,2.54650695806681));
#148934=CARTESIAN_POINT('Ctrl Pts',(7.00495317668262,1.29405949355901,2.5606158896811));
#148935=CARTESIAN_POINT('Ctrl Pts',(7.04420866416314,1.28783500491492,2.574708583835));
#148936=CARTESIAN_POINT('',(6.66706774467661,1.19797317561536,3.1505885381489));
#148937=CARTESIAN_POINT('Origin',(8.38738800634786E-13,1.28891221000011,
2.08600497986211E-13));
#148938=CARTESIAN_POINT('',(7.04607933373821,1.10830076258659,2.56958479416805));
#148939=CARTESIAN_POINT('Origin',(-0.180591217215621,0.946580170630017,
-0.0384341701045315));
#148940=CARTESIAN_POINT('',(7.21966585287252,1.19797317358556,2.03136037523598));
#148941=CARTESIAN_POINT('Origin',(-0.184058831876451,1.33917531484635,-0.0283666496420124));
#148942=CARTESIAN_POINT('Ctrl Pts',(7.04420866953866,1.28783500479116,2.57470856991552));
#148943=CARTESIAN_POINT('Ctrl Pts',(7.09780381709453,1.26310656824127,2.42807628404456));
#148944=CARTESIAN_POINT('Ctrl Pts',(7.1466797948153,1.23856749893545,2.28014229432938));
#148945=CARTESIAN_POINT('Ctrl Pts',(7.19077917881114,1.21428571428671,2.13135984797882));
#148946=CARTESIAN_POINT('Ctrl Pts',(7.20063167850662,1.20886077964635,2.09811949687777));
#148947=CARTESIAN_POINT('Ctrl Pts',(7.21026137828297,1.20342302038954,2.06478485484036));
#148948=CARTESIAN_POINT('Ctrl Pts',(7.21966585263086,1.1979731744789,2.03136037579649));
#148949=CARTESIAN_POINT('Ctrl Pts',(6.80734253400001,1.327885473,2.494511501));
#148950=CARTESIAN_POINT('Ctrl Pts',(6.927043104,1.27059961,2.167857251));
#148951=CARTESIAN_POINT('Ctrl Pts',(7.014916327,1.214285714,1.831242452));
#148952=CARTESIAN_POINT('Ctrl Pts',(7.02762400500001,1.20614195,1.782563319));
#148953=CARTESIAN_POINT('Ctrl Pts',(7.039654886,1.197973174,1.733712515));
#148954=CARTESIAN_POINT('Ctrl Pts',(6.953660913,1.327885473,2.810088949));
#148955=CARTESIAN_POINT('Ctrl Pts',(7.088504649,1.27059961,2.476413527));
#148956=CARTESIAN_POINT('Ctrl Pts',(7.190779179,1.214285714,2.131359848));
#148957=CARTESIAN_POINT('Ctrl Pts',(7.20556948400001,1.20614195,2.081460337));
#148958=CARTESIAN_POINT('Ctrl Pts',(7.219665854,1.197973174,2.031360369));
#148959=CARTESIAN_POINT('',(7.12966036896448,1.19797317334244,1.88253644592181));
#148960=CARTESIAN_POINT('Ctrl Pts',(7.03323098254006,1.19354381539971,1.75979646067424));
#148961=CARTESIAN_POINT('Ctrl Pts',(7.03644293427003,1.19575849469986,1.74675448783709));
#148962=CARTESIAN_POINT('Ctrl Pts',(7.039654886,1.197973174,1.733712515));
#148963=CARTESIAN_POINT('Ctrl Pts',(7.133530843,1.262701774,1.352533785));
#148964=CARTESIAN_POINT('Ctrl Pts',(7.185698963,1.327878141,0.963447153));
#148965=CARTESIAN_POINT('Ctrl Pts',(7.33215240352332,1.19354381539971,1.58052458316709));
#148966=CARTESIAN_POINT('Ctrl Pts',(7.33503018093462,1.19575849469986,1.56693005361739));
#148967=CARTESIAN_POINT('Ctrl Pts',(7.33790795834591,1.197973174,1.55333552406776));
#148968=CARTESIAN_POINT('Ctrl Pts',(7.4220169771698,1.262701774,1.15600717709109));
#148969=CARTESIAN_POINT('Ctrl Pts',(7.46273145832251,1.327878141,0.751919966756011));
#148970=CARTESIAN_POINT('',(7.33730273884919,1.19797317454273,1.55370155447371));
#148971=CARTESIAN_POINT('',(7.43300521898484,1.28783500531797,1.0002166830984));
#148972=CARTESIAN_POINT('Origin',(-0.190489516960962,1.33927123107037,-0.0172915188586062));
#148973=CARTESIAN_POINT('Ctrl Pts',(7.18507502228507,1.32710049324288,0.968089327893436));
#148974=CARTESIAN_POINT('Ctrl Pts',(7.22633028080292,1.3202217985532,0.973473407793488));
#148975=CARTESIAN_POINT('Ctrl Pts',(7.26764226558942,1.31351590013534,0.978844667424469));
#148976=CARTESIAN_POINT('Ctrl Pts',(7.35027182497301,1.30043858907801,0.989550939350619));
#148977=CARTESIAN_POINT('Ctrl Pts',(7.39163798930367,1.29405949358365,0.994892245192935));
#148978=CARTESIAN_POINT('Ctrl Pts',(7.4330052179612,1.28783500493846,1.00021669060776));
#148979=CARTESIAN_POINT('',(7.18847881074442,1.19797317561536,1.64370704086441));
#148980=CARTESIAN_POINT('Origin',(1.31838984174237E-13,1.28891221000017,
6.00648003556969E-14));
#148981=CARTESIAN_POINT('',(7.43373068909104,1.10830076258966,0.994810553290111));
#148982=CARTESIAN_POINT('Origin',(-0.184631607997902,0.946580187296585,
0.00128611533052506));
#148983=CARTESIAN_POINT('',(7.48755651189144,1.19797317358555,0.431853552262778));
#148984=CARTESIAN_POINT('Origin',(-0.185853746529759,1.33917529040736,0.0118637316038857));
#148985=CARTESIAN_POINT('Ctrl Pts',(7.43300522003748,1.28783500479117,1.00021667597356));
#148986=CARTESIAN_POINT('Ctrl Pts',(7.45382573580307,1.26310656824412,0.845491198897445));
#148987=CARTESIAN_POINT('Ctrl Pts',(7.46975758543086,1.23856749893828,0.690508933277066));
#148988=CARTESIAN_POINT('Ctrl Pts',(7.48084212235679,1.21428571428671,0.535724873766687));
#148989=CARTESIAN_POINT('Ctrl Pts',(7.4833185831773,1.20886077964635,0.501143667390705));
#148990=CARTESIAN_POINT('Ctrl Pts',(7.48555718325301,1.20342302038954,0.466518269919723));
#148991=CARTESIAN_POINT('Ctrl Pts',(7.48755651123012,1.1979731744789,0.431853552880365));
#148992=CARTESIAN_POINT('Ctrl Pts',(7.18443688400001,1.327885473,0.972813787));
#148993=CARTESIAN_POINT('Ctrl Pts',(7.231117913,1.27059961,0.628064447));
#148994=CARTESIAN_POINT('Ctrl Pts',(7.244574478,1.214285714,0.28042937));
#148995=CARTESIAN_POINT('Ctrl Pts',(7.246520483,1.20614195,0.230156553));
#148996=CARTESIAN_POINT('Ctrl Pts',(7.247768609,1.197973174,0.17986157));
#148997=CARTESIAN_POINT('Ctrl Pts',(7.395174244,1.327885473,1.249559084));
#148998=CARTESIAN_POINT('Ctrl Pts',(7.455135056,1.27059961,0.894697389999999));
#148999=CARTESIAN_POINT('Ctrl Pts',(7.480842122,1.214285714,0.535724874));
#149000=CARTESIAN_POINT('Ctrl Pts',(7.484559718,1.20614195,0.483812507));
#149001=CARTESIAN_POINT('Ctrl Pts',(7.487556512,1.197973174,0.431853546));
#149002=CARTESIAN_POINT('',(7.36766256033176,1.19797317334244,0.305857562052724));
#149003=CARTESIAN_POINT('Ctrl Pts',(7.24710217013975,1.19354381559283,0.206716635708786));
#149004=CARTESIAN_POINT('Ctrl Pts',(7.24743538956988,1.19575849479642,0.193289102854393));
#149005=CARTESIAN_POINT('Ctrl Pts',(7.247768609,1.197973174,0.17986157));
#149006=CARTESIAN_POINT('Ctrl Pts',(7.25750763900001,1.262701774,-0.212585969));
#149007=CARTESIAN_POINT('Ctrl Pts',(7.224813973,1.327878141,-0.603790576));
#149008=CARTESIAN_POINT('Ctrl Pts',(7.50049682043428,1.19354381559283,-0.0326232345733736));
#149009=CARTESIAN_POINT('Ctrl Pts',(7.50038489498958,1.19575849479642,-0.0465185680631247));
#149010=CARTESIAN_POINT('Ctrl Pts',(7.50027296954502,1.197973174,-0.0604139015528768));
#149011=CARTESIAN_POINT('Ctrl Pts',(7.49700171593858,1.262701774,-0.466533885824836));
#149012=CARTESIAN_POINT('Ctrl Pts',(7.44989751091891,1.327878141,-0.869926171191936));
#149013=CARTESIAN_POINT('',(7.4997605859831,1.19797317455027,-0.0599263262953898));
#149014=CARTESIAN_POINT('',(7.47424270829533,1.28783500531214,-0.621044231484297));
#149015=CARTESIAN_POINT('Origin',(-0.189753473192996,1.3392712669591,0.0240623826805827));
#149016=CARTESIAN_POINT('Ctrl Pts',(7.22520254964774,1.32710049321762,-0.599122803118063));
#149017=CARTESIAN_POINT('Ctrl Pts',(7.26665070116499,1.32022179856296,-0.602733261078277));
#149018=CARTESIAN_POINT('Ctrl Pts',(7.30815149716335,1.31351590009954,-0.60636843412573));
#149019=CARTESIAN_POINT('Ctrl Pts',(7.39115075537979,1.30043858906754,-0.613675381739156));
#149020=CARTESIAN_POINT('Ctrl Pts',(7.43269802464555,1.29405949358074,-0.617351455288066));
#149021=CARTESIAN_POINT('Ctrl Pts',(7.47424270891332,1.28783500493303,-0.621044223892722));
#149022=CARTESIAN_POINT('',(7.37376459691771,1.19797317561536,0.0599676291186608));
#149023=CARTESIAN_POINT('Origin',(-5.98913280080993E-13,1.28891220999994,
7.57958962521038E-14));
#149024=CARTESIAN_POINT('',(7.47378905921366,1.10830076262361,-0.626479923766747));
#149025=CARTESIAN_POINT('Origin',(-0.180038565926405,0.946580182915173,
0.0409463866725945));
#149026=CARTESIAN_POINT('',(7.40533734948143,1.19797317358556,-1.18784626286482));
#149027=CARTESIAN_POINT('Origin',(-0.178957929364433,1.33917531698094,0.0515394024328136));
#149028=CARTESIAN_POINT('Ctrl Pts',(7.47424270769856,1.28783500479116,-0.621044238693877));
#149029=CARTESIAN_POINT('Ctrl Pts',(7.46131504745461,1.26310656824169,-0.776628115470739));
#149030=CARTESIAN_POINT('Ctrl Pts',(7.44355781343537,1.23856749893588,-0.93141185843771));
#149031=CARTESIAN_POINT('Ctrl Pts',(7.4211092026572,1.21428571428671,-1.08496000029333));
#149032=CARTESIAN_POINT('Ctrl Pts',(7.41609382804624,1.20886077964635,-1.11926508312602));
#149033=CARTESIAN_POINT('Ctrl Pts',(7.41083665397242,1.20342302038954,-1.15356219079986));
#149034=CARTESIAN_POINT('Ctrl Pts',(7.40533734932788,1.1979731744789,-1.18784626221134));
#149035=CARTESIAN_POINT('Ctrl Pts',(7.22559495,1.327885473,-0.594371618));
#149036=CARTESIAN_POINT('Ctrl Pts',(7.197073686,1.27059961,-0.941095951));
#149037=CARTESIAN_POINT('Ctrl Pts',(7.135484378,1.214285714,-1.283496277));
#149038=CARTESIAN_POINT('Ctrl Pts',(7.126577716,1.20614195,-1.333012078));
#149039=CARTESIAN_POINT('Ctrl Pts',(7.116984728,1.197973174,-1.382399502));
#149040=CARTESIAN_POINT('Ctrl Pts',(7.490897446,1.327885473,-0.369398776));
#149041=CARTESIAN_POINT('Ctrl Pts',(7.473171633,1.27059961,-0.728853803));
#149042=CARTESIAN_POINT('Ctrl Pts',(7.421109203,1.214285714,-1.08496));
#149043=CARTESIAN_POINT('Ctrl Pts',(7.413580259,1.20614195,-1.136457858));
#149044=CARTESIAN_POINT('Ctrl Pts',(7.405337348,1.197973174,-1.187846269));
#149045=CARTESIAN_POINT('',(7.26116103870691,1.19797317334244,-1.28512288150586));
#149046=CARTESIAN_POINT('Ctrl Pts',(7.1221069156548,1.19354381541858,-1.35602902712435));
#149047=CARTESIAN_POINT('Ctrl Pts',(7.1195458218274,1.1957584947093,-1.3692142645622));
#149048=CARTESIAN_POINT('Ctrl Pts',(7.116984728,1.197973174,-1.382399502));
#149049=CARTESIAN_POINT('Ctrl Pts',(7.04213144400001,1.262701774,-1.767765439));
#149050=CARTESIAN_POINT('Ctrl Pts',(6.926104711,1.327878141,-2.142795728));
#149051=CARTESIAN_POINT('Ctrl Pts',(7.31812634173865,1.19354381541858,-1.64424562360488));
#149052=CARTESIAN_POINT('Ctrl Pts',(7.31502994699515,1.1957584947093,-1.65779203180329));
#149053=CARTESIAN_POINT('Ctrl Pts',(7.31193355225165,1.197973174,-1.67133844000171));
#149054=CARTESIAN_POINT('Ctrl Pts',(7.22143498767998,1.262701774,-2.06726034228003));
#149055=CARTESIAN_POINT('Ctrl Pts',(7.08871463480692,1.327878141,-2.45109552827173));
#149056=CARTESIAN_POINT('',(7.31153796209935,1.19797317454273,-1.67075211474223));
#149057=CARTESIAN_POINT('',(7.1659929155684,1.28783500526628,-2.21326580745523));
#149058=CARTESIAN_POINT('Origin',(-0.180144164879942,1.33927126523448,0.0642911260606757));
#149059=CARTESIAN_POINT('Ctrl Pts',(6.9274876363475,1.32710049319203,-2.13832061771533));
#149060=CARTESIAN_POINT('Ctrl Pts',(6.96719061146471,1.32022179851475,-2.1507567924955));
#149061=CARTESIAN_POINT('Ctrl Pts',(7.00693968702447,1.31351590007216,-2.16322842146589));
#149062=CARTESIAN_POINT('Ctrl Pts',(7.0864276911202,1.30043858901132,-2.18820692365546));
#149063=CARTESIAN_POINT('Ctrl Pts',(7.12621336121677,1.29405949351721,-2.20072848734333));
#149064=CARTESIAN_POINT('Ctrl Pts',(7.16599291782655,1.28783500485895,-2.21326580008813));
#149065=CARTESIAN_POINT('',(7.21426134609485,1.19797317561536,-1.52657580210022));
#149066=CARTESIAN_POINT('Origin',(-8.25294693695966E-13,1.28891221000017,
3.3436794999453E-13));
#149067=CARTESIAN_POINT('',(7.16438135929131,1.10830076263124,-2.21847689478545));
#149068=CARTESIAN_POINT('Origin',(-0.167026977383227,0.9465801840733,0.07869201776906));
#149069=CARTESIAN_POINT('',(6.9768528436404,1.19797317358556,-2.75200370729668));
#149070=CARTESIAN_POINT('Origin',(-0.163694659924108,1.33917530233932,0.0888051357193126));
#149071=CARTESIAN_POINT('Ctrl Pts',(7.16599291338407,1.28783500479116,-2.2132658144311));
#149072=CARTESIAN_POINT('Ctrl Pts',(7.11992156021712,1.2631065682245,-2.36243316168405));
#149073=CARTESIAN_POINT('Ctrl Pts',(7.06930555112514,1.23856749891882,-2.50978086632341));
#149074=CARTESIAN_POINT('Ctrl Pts',(7.01437346458419,1.21428571428671,-2.65491335062694));
#149075=CARTESIAN_POINT('Ctrl Pts',(7.00210076784224,1.20886077964635,-2.68733824251475));
#149076=CARTESIAN_POINT('Ctrl Pts',(6.98959363920698,1.20342302038954,-2.71970336592745));
#149077=CARTESIAN_POINT('Ctrl Pts',(6.97685284345389,1.1979731744789,-2.75200370653627));
#149078=CARTESIAN_POINT('Ctrl Pts',(6.928892227,1.327885473,-2.133764867));
#149079=CARTESIAN_POINT('Ctrl Pts',(6.826502291,1.27059961,-2.466251749));
#149080=CARTESIAN_POINT('Ctrl Pts',(6.692746959,1.214285714,-2.787407065));
#149081=CARTESIAN_POINT('Ctrl Pts',(6.673404096,1.20614195,-2.833850545));
#149082=CARTESIAN_POINT('Ctrl Pts',(6.65341855,1.197973174,-2.88002111));
#149083=CARTESIAN_POINT('Ctrl Pts',(7.236354609,1.327885473,-1.971083959));
#149084=CARTESIAN_POINT('Ctrl Pts',(7.14177101,1.27059961,-2.318324601));
#149085=CARTESIAN_POINT('Ctrl Pts',(7.014373465,1.214285714,-2.65491335));
#149086=CARTESIAN_POINT('Ctrl Pts',(6.995950026,1.20614195,-2.703588717));
#149087=CARTESIAN_POINT('Ctrl Pts',(6.976852841,1.197973174,-2.752003713));
#149088=CARTESIAN_POINT('',(6.815135697049,1.19797317334244,-2.8160124077512));
#149089=CARTESIAN_POINT('Ctrl Pts',(6.66408985650852,1.19354381535312,-2.85536828075232));
#149090=CARTESIAN_POINT('Ctrl Pts',(6.65875420325428,1.19575849467657,-2.86769469537616));
#149091=CARTESIAN_POINT('Ctrl Pts',(6.65341854999999,1.197973174,-2.88002111));
#149092=CARTESIAN_POINT('Ctrl Pts',(6.497473009,1.262701774,-3.240286162));
#149093=CARTESIAN_POINT('Ctrl Pts',(6.303538491,1.327878141,-3.581606133));
#149094=CARTESIAN_POINT('Ctrl Pts',(6.79356840984586,1.19354381535312,-3.17898491578651));
#149095=CARTESIAN_POINT('Ctrl Pts',(6.78763232966878,1.19575849467657,-3.19154898332476));
#149096=CARTESIAN_POINT('Ctrl Pts',(6.7816962494918,1.197973174,-3.20411305086303));
#149097=CARTESIAN_POINT('Ctrl Pts',(6.60820198543364,1.262701774,-3.57132400255763));
#149098=CARTESIAN_POINT('Ctrl Pts',(6.39607134065686,1.327878141,-3.91765438273399));
#149099=CARTESIAN_POINT('',(6.78143595059185,1.19797317454273,-3.20345539331613));
#149100=CARTESIAN_POINT('',(6.52266925830075,1.28783500530872,-3.70199753484471));
#149101=CARTESIAN_POINT('Origin',(-0.162111689526208,1.3392712357706,0.101513649847844));
#149102=CARTESIAN_POINT('Ctrl Pts',(6.30585109992902,1.32710049333678,-3.57753293576106));
#149103=CARTESIAN_POINT('Ctrl Pts',(6.34195246648704,1.32022179198259,-3.59821334618977));
#149104=CARTESIAN_POINT('Ctrl Pts',(6.37809124102865,1.31351588629104,-3.61893829604711));
#149105=CARTESIAN_POINT('Ctrl Pts',(6.45035114375322,1.30043858906411,-3.66042034248003));
#149106=CARTESIAN_POINT('Ctrl Pts',(6.48651488093728,1.29405949358396,-3.68120190204836));
#149107=CARTESIAN_POINT('Ctrl Pts',(6.52266926205248,1.28783500493332,-3.70199752820974));
#149108=CARTESIAN_POINT('',(6.71742725267403,1.19797317561536,-3.041738245782));
#149109=CARTESIAN_POINT('Origin',(-1.56775634141404E-12,1.28891220999994,
7.56556275960385E-13));
#149110=CARTESIAN_POINT('',(6.51997514986712,1.10830076264337,-3.70674035236029));
#149111=CARTESIAN_POINT('Origin',(-0.146205722694455,0.946580186364563,
0.112758217822082));
#149112=CARTESIAN_POINT('',(6.22213845282096,1.19797317358555,-4.18748051700546));
#149113=CARTESIAN_POINT('Origin',(-0.140777006185144,1.33917528229682,0.121918379441862));
#149114=CARTESIAN_POINT('Ctrl Pts',(6.52266925465969,1.28783500479116,-3.70199754110091));
#149115=CARTESIAN_POINT('Ctrl Pts',(6.44560845380337,1.26310656823854,-3.83777345961638));
#149116=CARTESIAN_POINT('Ctrl Pts',(6.364500417915,1.23856749893275,-3.97079531107751));
#149117=CARTESIAN_POINT('Ctrl Pts',(6.27965341901354,1.21428571428671,-4.10072590367506));
#149118=CARTESIAN_POINT('Ctrl Pts',(6.26069725783425,1.20886077964635,-4.12975445256057));
#149119=CARTESIAN_POINT('Ctrl Pts',(6.24152499419278,1.20342302038954,-4.15867423426439));
#149120=CARTESIAN_POINT('Ctrl Pts',(6.22213845282379,1.1979731744789,-4.18748051624025));
#149121=CARTESIAN_POINT('Ctrl Pts',(6.308202204,1.327885473,-3.573385642));
#149122=CARTESIAN_POINT('Ctrl Pts',(6.136731237,1.27059961,-3.876088357));
#149123=CARTESIAN_POINT('Ctrl Pts',(5.93706413,1.214285714,-4.160981797));
#149124=CARTESIAN_POINT('Ctrl Pts',(5.908189518,1.20614195,-4.20218131));
#149125=CARTESIAN_POINT('Ctrl Pts',(5.878745916,1.197973174,-4.242976131));
#149126=CARTESIAN_POINT('Ctrl Pts',(6.643447873,1.327885473,-3.480603448));
#149127=CARTESIAN_POINT('Ctrl Pts',(6.476429113,1.27059961,-3.799393119));
#149128=CARTESIAN_POINT('Ctrl Pts',(6.279653419,1.214285714,-4.100725903));
#149129=CARTESIAN_POINT('Ctrl Pts',(6.25119694500001,1.20614195,-4.144302772));
#149130=CARTESIAN_POINT('Ctrl Pts',(6.222138449,1.197973174,-4.187480522));
#149131=CARTESIAN_POINT('',(6.0504421848187,1.19797317334243,-4.2152283231718));
#149132=CARTESIAN_POINT('Ctrl Pts',(5.89446736251345,1.19354381545263,-4.22119368712617));
#149133=CARTESIAN_POINT('Ctrl Pts',(5.88660663925671,1.19575849472632,-4.23208490906309));
#149134=CARTESIAN_POINT('Ctrl Pts',(5.878745916,1.197973174,-4.242976131));
#149135=CARTESIAN_POINT('Ctrl Pts',(5.648999958,1.262701774,-4.56129470500001));
#149136=CARTESIAN_POINT('Ctrl Pts',(5.386225817,1.327878141,-4.852944616));
#149137=CARTESIAN_POINT('Ctrl Pts',(5.95135076798055,1.19354381545264,-4.56507840749032));
#149138=CARTESIAN_POINT('Ctrl Pts',(5.94285256712257,1.19575849472632,-4.57607265208447));
#149139=CARTESIAN_POINT('Ctrl Pts',(5.93435436626472,1.197973174,-4.58706689667855));
#149140=CARTESIAN_POINT('Ctrl Pts',(5.68597680180873,1.262701774,-4.9083965217357));
#149141=CARTESIAN_POINT('Ctrl Pts',(5.40435486065015,1.327878141,-5.20102807168802));
#149142=CARTESIAN_POINT('',(5.93424152994601,1.19797317454255,-4.58636865826812));
#149143=CARTESIAN_POINT('',(5.57435283624376,1.28783500529315,-5.01762797127261));
#149144=CARTESIAN_POINT('Origin',(-0.136499289031298,1.33927126171856,0.133989635138438));
#149145=CARTESIAN_POINT('Ctrl Pts',(5.38935997513011,1.32710049341366,-4.8494637911487));
#149146=CARTESIAN_POINT('Ctrl Pts',(5.42017160522032,1.3202217986986,-4.87742140436003));
#149147=CARTESIAN_POINT('Ctrl Pts',(5.451010188688,1.31351590010789,-4.90543055249013));
#149148=CARTESIAN_POINT('Ctrl Pts',(5.51266334654728,1.30043858903252,-4.9614765737824));
#149149=CARTESIAN_POINT('Ctrl Pts',(5.54351417461199,1.29405949355007,-4.98954640642331));
#149150=CARTESIAN_POINT('Ctrl Pts',(5.57435284139363,1.28783500490135,-5.01762796553027));
#149151=CARTESIAN_POINT('',(5.906493726556,1.19797317561482,-4.41467238939753));
#149152=CARTESIAN_POINT('Origin',(2.43772016461641E-12,1.28891220999983,
-2.21610924056037E-12));
#149153=CARTESIAN_POINT('',(5.57070214838859,1.1083007626525,-5.02168075129053));
#149154=CARTESIAN_POINT('Origin',(-0.118547812998999,0.94658017878209,0.141551885277263));
#149155=CARTESIAN_POINT('',(5.17648378289701,1.19797317358556,-5.42715539201615));
#149156=CARTESIAN_POINT('Origin',(-0.111276857755188,1.33917532586237,0.149330892566997));
#149157=CARTESIAN_POINT('Ctrl Pts',(5.57435283129608,1.28783500479126,-5.01762797666601));
#149158=CARTESIAN_POINT('Ctrl Pts',(5.46990586017375,1.26310656823713,-5.13366373537583));
#149159=CARTESIAN_POINT('Ctrl Pts',(5.36209831904503,1.23856749893132,-5.2461397797822));
#149160=CARTESIAN_POINT('Ctrl Pts',(5.25130375913421,1.21428571428671,-5.35479307063336));
#149161=CARTESIAN_POINT('Ctrl Pts',(5.22655050253382,1.20886077964635,-5.37906793386744));
#149162=CARTESIAN_POINT('Ctrl Pts',(5.20160957745708,1.20342302038954,-5.40319011729261));
#149163=CARTESIAN_POINT('Ctrl Pts',(5.17648378317611,1.1979731744789,-5.42715539141038));
#149164=CARTESIAN_POINT('Ctrl Pts',(5.392547658,1.327885473,-4.845918877));
#149165=CARTESIAN_POINT('Ctrl Pts',(5.160013451,1.27059961,-5.10468338));
#149166=CARTESIAN_POINT('Ctrl Pts',(4.903770781,1.214285714,-5.339993645));
#149167=CARTESIAN_POINT('Ctrl Pts',(4.866714564,1.20614195,-5.374022748));
#149168=CARTESIAN_POINT('Ctrl Pts',(4.829189657,1.197973174,-5.40753430500001));
#149169=CARTESIAN_POINT('Ctrl Pts',(5.739900898,1.327885473,-4.827373787));
#149170=CARTESIAN_POINT('Ctrl Pts',(5.50825658799999,1.27059961,-5.102806236));
#149171=CARTESIAN_POINT('Ctrl Pts',(5.251303759,1.214285714,-5.35479307));
#149172=CARTESIAN_POINT('Ctrl Pts',(5.214144843,1.20614195,-5.391233835));
#149173=CARTESIAN_POINT('Ctrl Pts',(5.176483778,1.197973174,-5.427155396));
#149174=CARTESIAN_POINT('',(5.00110024987486,1.19797317334244,-5.41724674229405));
#149175=CARTESIAN_POINT('Ctrl Pts',(4.84922612612734,1.19354381550591,-5.38964076904563));
#149176=CARTESIAN_POINT('Ctrl Pts',(4.83920789156366,1.19575849475297,-5.39858753702288));
#149177=CARTESIAN_POINT('Ctrl Pts',(4.829189657,1.197973174,-5.407534305));
#149178=CARTESIAN_POINT('Ctrl Pts',(4.536385948,1.262701774,-5.669022178));
#149179=CARTESIAN_POINT('Ctrl Pts',(4.21705921,1.327878141,-5.897364803));
#149180=CARTESIAN_POINT('Ctrl Pts',(4.8308545800179,1.19354381550591,-5.73771390554859));
#149181=CARTESIAN_POINT('Ctrl Pts',(4.82019162486587,1.19575849475297,-5.74662424873047));
#149182=CARTESIAN_POINT('Ctrl Pts',(4.80952866971385,1.197973174,-5.75553459191248));
#149183=CARTESIAN_POINT('Ctrl Pts',(4.49788166269152,1.262701774,-6.01595787463447));
#149184=CARTESIAN_POINT('Ctrl Pts',(4.15993675249693,1.327878141,-6.24120746922401));
#149185=CARTESIAN_POINT('',(4.80956857104774,1.19797317455043,-5.75482842296611));
#149186=CARTESIAN_POINT('',(4.36538587067711,1.28783500456851,-6.09863970055502));
#149187=CARTESIAN_POINT('Origin',(-0.104504270684904,1.33927127350409,0.160200449407045));
#149188=CARTESIAN_POINT('Ctrl Pts',(4.22086836875467,1.32710049315245,-5.8946391097756));
#149189=CARTESIAN_POINT('Ctrl Pts',(4.24494957945847,1.3202217984799,-5.9285666791748));
#149190=CARTESIAN_POINT('Ctrl Pts',(4.26904603430032,1.31351590009086,-5.96255037194016));
#149191=CARTESIAN_POINT('Ctrl Pts',(4.3172095375045,1.30043858904136,-6.03053967491418));
#149192=CARTESIAN_POINT('Ctrl Pts',(4.34130490602236,1.29405949355654,-6.06458526663132));
#149193=CARTESIAN_POINT('Ctrl Pts',(4.36538587674004,1.2878350049083,-6.09863969632983));
#149194=CARTESIAN_POINT('',(4.81937911915879,1.19797317561536,-5.5811813588866));
#149195=CARTESIAN_POINT('Origin',(-6.17561557447743E-13,1.28891221000039,
8.67795418857398E-13));
#149196=CARTESIAN_POINT('',(4.36094930658774,1.10830076259545,-6.10181293897598));
#149197=CARTESIAN_POINT('Origin',(-0.0853466450309831,0.946580177243603,
0.16372661055274));
#149198=CARTESIAN_POINT('',(3.8887824855194,1.19797317379345,-6.41306251204082));
#149199=CARTESIAN_POINT('Origin',(-0.0765736300821324,1.33917535499471,
0.169761002796281));
#149200=CARTESIAN_POINT('Ctrl Pts',(4.36538586477892,1.28783500266228,-6.09863970449737));
#149201=CARTESIAN_POINT('Ctrl Pts',(4.23843654752548,1.26310656752412,-6.18950960074403));
#149202=CARTESIAN_POINT('Ctrl Pts',(4.10897046193337,1.23856749892619,-6.27618058321672));
#149203=CARTESIAN_POINT('Ctrl Pts',(3.97740897184098,1.2142857140719,-6.35847606461084));
#149204=CARTESIAN_POINT('Ctrl Pts',(3.94801605496087,1.20886077973443,-6.37686217615265));
#149205=CARTESIAN_POINT('Ctrl Pts',(3.91847267837239,1.20342302059143,-6.39505883492393));
#149206=CARTESIAN_POINT('Ctrl Pts',(3.88878248571163,1.1979731751026,-6.41306251127484));
#149207=CARTESIAN_POINT('Ctrl Pts',(4.224743576,1.327885473,-5.89186233000001));
#149208=CARTESIAN_POINT('Ctrl Pts',(3.94201917,1.27059961,-6.094589083));
#149209=CARTESIAN_POINT('Ctrl Pts',(3.641182561,1.214285714,-6.269313324));
#149210=CARTESIAN_POINT('Ctrl Pts',(3.597677446,1.20614195,-6.294580855));
#149211=CARTESIAN_POINT('Ctrl Pts',(3.553825856,1.197973174,-6.319242184));
#149212=CARTESIAN_POINT('Ctrl Pts',(4.567962537,1.327885473,-5.948421493));
#149213=CARTESIAN_POINT('Ctrl Pts',(4.282524107,1.27059961,-6.167617806));
#149214=CARTESIAN_POINT('Ctrl Pts',(3.977408972,1.214285714,-6.358476065));
#149215=CARTESIAN_POINT('Ctrl Pts',(3.933285124,1.20614195,-6.38607679600001));
#149216=CARTESIAN_POINT('Ctrl Pts',(3.88878248,1.197973174,-6.413062515));
#149217=CARTESIAN_POINT('',(3.72130417150183,1.19797317334244,-6.36615234745303));
#149218=CARTESIAN_POINT('Ctrl Pts',(3.5772404657506,1.19354381534562,-6.30607423705896));
#149219=CARTESIAN_POINT('Ctrl Pts',(3.56553316087531,1.19575849467282,-6.31265821052942));
#149220=CARTESIAN_POINT('Ctrl Pts',(3.553825856,1.197973174,-6.319242184));
#149221=CARTESIAN_POINT('Ctrl Pts',(3.211655572,1.262701774,-6.511672474));
#149222=CARTESIAN_POINT('Ctrl Pts',(2.850707601,1.327878141,-6.666030766));
#149223=CARTESIAN_POINT('Ctrl Pts',(3.48447300063436,1.19354381534562,-6.64206027784984));
#149224=CARTESIAN_POINT('Ctrl Pts',(3.47214387864852,1.19575849467282,-6.64847008224919));
#149225=CARTESIAN_POINT('Ctrl Pts',(3.45981475666261,1.197973174,-6.65487988664856));
#149226=CARTESIAN_POINT('Ctrl Pts',(3.09947057699739,1.262701774,-6.84221972404721));
#149227=CARTESIAN_POINT('Ctrl Pts',(2.72100462632398,1.327878141,-6.98955494174905));
#149228=CARTESIAN_POINT('',(3.46000553056191,1.19797317455044,-6.6541988051439));
#149229=CARTESIAN_POINT('',(2.95229831384228,1.28783500532053,-6.89448581602087));
#149230=CARTESIAN_POINT('Origin',(-0.0676225476017656,1.33927124513901,
0.178920113634683));
#149231=CARTESIAN_POINT('Ctrl Pts',(2.85501364690942,1.32710049333567,-6.66418765315929));
#149232=CARTESIAN_POINT('Ctrl Pts',(2.87123842778919,1.32022179868456,-6.70249876327353));
#149233=CARTESIAN_POINT('Ctrl Pts',(2.88746603208701,1.31351590010048,-6.74086796289427));
#149234=CARTESIAN_POINT('Ctrl Pts',(2.91988780911154,1.30043858907498,-6.81762144325761));
#149235=CARTESIAN_POINT('Ctrl Pts',(2.93610104555493,1.29405949359601,-6.85605085997186));
#149236=CARTESIAN_POINT('Ctrl Pts',(2.95229832091699,1.28783500494432,-6.89448581297852));
#149237=CARTESIAN_POINT('',(3.50691569940141,1.19797317561536,-6.48672049068763));
#149238=CARTESIAN_POINT('Origin',(-5.07406616723216E-13,1.28891220999994,
1.13364179155084E-12));
#149239=CARTESIAN_POINT('',(2.94728332132464,1.10830076261527,-6.89663113553974));
#149240=CARTESIAN_POINT('Origin',(-0.048155014798249,0.946580161353691,
0.178246000753397));
#149241=CARTESIAN_POINT('',(2.41924604010438,1.19797317358556,-7.09910195741526));
#149242=CARTESIAN_POINT('Origin',(-0.0382896729873458,1.33917527452691,
0.182252827141014));
#149243=CARTESIAN_POINT('Ctrl Pts',(2.95229830709036,1.28783500479117,-6.894485818823));
#149244=CARTESIAN_POINT('Ctrl Pts',(2.8087826528535,1.26310656824939,-6.95594087641231));
#149245=CARTESIAN_POINT('Ctrl Pts',(2.66371171324971,1.23856749894351,-7.01275415801446));
#149246=CARTESIAN_POINT('Ctrl Pts',(2.51753496156429,1.21428571428671,-7.06484378576778));
#149247=CARTESIAN_POINT('Ctrl Pts',(2.48487676386419,1.20886077964635,-7.0764814322586));
#149248=CARTESIAN_POINT('Ctrl Pts',(2.45211235138882,1.20342302038954,-7.08790171038468));
#149249=CARTESIAN_POINT('Ctrl Pts',(2.41924604060176,1.1979731744789,-7.09910195694024));
#149250=CARTESIAN_POINT('Ctrl Pts',(2.85939518,1.327885473,-6.66230884900001));
#149251=CARTESIAN_POINT('Ctrl Pts',(2.539700455,1.27059961,-6.799518573));
#149252=CARTESIAN_POINT('Ctrl Pts',(2.208336691,1.214285714,-6.905486881));
#149253=CARTESIAN_POINT('Ctrl Pts',(2.16041693,1.20614195,-6.920811357));
#149254=CARTESIAN_POINT('Ctrl Pts',(2.112289109,1.197973174,-6.93546932199999));
#149255=CARTESIAN_POINT('Ctrl Pts',(3.182431324,1.327885473,-6.791327622));
#149256=CARTESIAN_POINT('Ctrl Pts',(2.856545558,1.27059961,-6.944038421));
#149257=CARTESIAN_POINT('Ctrl Pts',(2.517534962,1.214285714,-7.064843786));
#149258=CARTESIAN_POINT('Ctrl Pts',(2.468509363,1.20614195,-7.082313904));
#149259=CARTESIAN_POINT('Ctrl Pts',(2.419246034,1.197973174,-7.099101959));
#149260=CARTESIAN_POINT('',(2.26576757536,1.19797317334244,-7.01728563925367));
#149261=CARTESIAN_POINT('Ctrl Pts',(2.13798701621293,1.19354381558494,-6.92764268374129));
#149262=CARTESIAN_POINT('Ctrl Pts',(2.12513806260643,1.19575849479248,-6.93155600287059));
#149263=CARTESIAN_POINT('Ctrl Pts',(2.112289109,1.197973174,-6.935469322));
#149264=CARTESIAN_POINT('Ctrl Pts',(1.736751751,1.262701774,-7.049844202));
#149265=CARTESIAN_POINT('Ctrl Pts',(1.351060074,1.327878141,-7.123000539));
#149266=CARTESIAN_POINT('Ctrl Pts',(1.97516133521341,1.19354381558494,-7.2358312953567));
#149267=CARTESIAN_POINT('Ctrl Pts',(1.96174254347939,1.19575849479248,-7.23944084507777));
#149268=CARTESIAN_POINT('Ctrl Pts',(1.94832375174542,1.197973174,-7.24305039479882));
#149269=CARTESIAN_POINT('Ctrl Pts',(1.55613169084436,1.262701774,-7.34854698287401));
#149270=CARTESIAN_POINT('Ctrl Pts',(1.15484134686268,1.327878141,-7.41107859406688));
#149271=CARTESIAN_POINT('',(1.94865647594488,1.19797317455223,-7.2424262484091));
#149272=CARTESIAN_POINT('',(1.40116456872723,1.28783500529828,-7.3679534371202));
#149273=CARTESIAN_POINT('Origin',(-0.0275791123912514,1.33927124802198,
0.189274290450747));
#149274=CARTESIAN_POINT('Ctrl Pts',(1.3556616617783,1.3271004931861,-7.12212619073517));
#149275=CARTESIAN_POINT('Ctrl Pts',(1.363271367675,1.32022179142973,-7.1630294988622));
#149276=CARTESIAN_POINT('Ctrl Pts',(1.37087134459537,1.31351588546559,-7.20399015161181));
#149277=CARTESIAN_POINT('Ctrl Pts',(1.38603537174766,1.30043858905527,-7.28591881024255));
#149278=CARTESIAN_POINT('Ctrl Pts',(1.39360836300028,1.29405949356432,-7.32693513514737));
#149279=CARTESIAN_POINT('Ctrl Pts',(1.40116457621226,1.28783500491313,-7.3679534356829));
#149280=CARTESIAN_POINT('',(2.03047280022782,1.19797317561536,-7.08894778221368));
#149281=CARTESIAN_POINT('Origin',(3.27049585330252E-13,1.28891220999989,
-1.46757606067638E-12));
#149282=CARTESIAN_POINT('',(1.39580564426377,1.10830076261413,-7.36897052498051));
#149283=CARTESIAN_POINT('Origin',(-0.00871150746413529,0.946580172873321,
0.184430426260994));
#149284=CARTESIAN_POINT('',(0.83658833931585,1.19797317358555,-7.45319528481688));
#149285=CARTESIAN_POINT('Origin',(0.00178446839071103,1.33917534057801,
0.186223212724637));
#149286=CARTESIAN_POINT('Ctrl Pts',(1.40116456161428,1.28783500479117,-7.36795343845741));
#149287=CARTESIAN_POINT('Ctrl Pts',(1.24779320284748,1.26310656823488,-7.39712008757723));
#149288=CARTESIAN_POINT('Ctrl Pts',(1.0939007651504,1.23856749892911,-7.42141914245925));
#149289=CARTESIAN_POINT('Ctrl Pts',(0.939943814464729,1.21428571428671,
-7.44086726300433));
#149290=CARTESIAN_POINT('Ctrl Pts',(0.905547397265625,1.20886077964635,
-7.44521228065392));
#149291=CARTESIAN_POINT('Ctrl Pts',(0.871093976328095,1.20342302038954,
-7.4493221788494));
#149292=CARTESIAN_POINT('Ctrl Pts',(0.836588339905451,1.1979731744789,-7.45319528454301));
#149293=CARTESIAN_POINT('Ctrl Pts',(1.360344644,1.327885473,-7.121233211));
#149294=CARTESIAN_POINT('Ctrl Pts',(1.018628168,1.27059961,-7.186510132));
#149295=CARTESIAN_POINT('Ctrl Pts',(0.672231452,1.214285714,-7.218767545));
#149296=CARTESIAN_POINT('Ctrl Pts',(0.622137718,1.20614195,-7.223432411));
#149297=CARTESIAN_POINT('Ctrl Pts',(0.57198407,1.197973174,-7.227401623));
#149298=CARTESIAN_POINT('Ctrl Pts',(1.64809316,1.327885473,-7.316678819));
#149299=CARTESIAN_POINT('Ctrl Pts',(1.296998114,1.27059961,-7.395763518));
#149300=CARTESIAN_POINT('Ctrl Pts',(0.939943815,1.214285714,-7.440867263));
#149301=CARTESIAN_POINT('Ctrl Pts',(0.888308847999999,1.20614195,-7.447389885));
#149302=CARTESIAN_POINT('Ctrl Pts',(0.836588333,1.197973174,-7.453195285));
#149303=CARTESIAN_POINT('',(0.704286205537718,1.19797317334243,-7.34029845361259));
#149304=CARTESIAN_POINT('Ctrl Pts',(0.58215939042632,1.19629017123951,-7.22659633756481));
#149305=CARTESIAN_POINT('Ctrl Pts',(0.577071730213161,1.19713167261975,
-7.2269989802824));
#149306=CARTESIAN_POINT('Ctrl Pts',(0.57198407,1.197973174,-7.227401623));
#149307=CARTESIAN_POINT('Ctrl Pts',(0.180639349,1.262701774,-7.258373051));
#149308=CARTESIAN_POINT('Ctrl Pts',(-0.211761522,1.327878141,-7.246906723));
#149309=CARTESIAN_POINT('Ctrl Pts',(0.356564099953848,1.19629017123951,
-7.49172316926537));
#149310=CARTESIAN_POINT('Ctrl Pts',(0.351290030198813,1.19713167261975,
-7.49196674389207));
#149311=CARTESIAN_POINT('Ctrl Pts',(0.346015960443778,1.197973174,-7.49221031851878));
#149312=CARTESIAN_POINT('Ctrl Pts',(-0.0596674520371902,1.262701774,-7.51094616964391));
#149313=CARTESIAN_POINT('Ctrl Pts',(-0.465002005850376,1.327878141,-7.48576753873542));
#149314=CARTESIAN_POINT('Ctrl Pts',(-0.207079557678091,1.32710049326789,
-7.24704202133301));
#149315=CARTESIAN_POINT('Ctrl Pts',(-0.208440763000792,1.32022179860809,
-7.28862485198612));
#149316=CARTESIAN_POINT('Ctrl Pts',(-0.209823796958759,1.31351590008895,
-7.33026158825384));
#149317=CARTESIAN_POINT('Ctrl Pts',(-0.212626538934049,1.3004385890535,
-7.41353471129152));
#149318=CARTESIAN_POINT('Ctrl Pts',(-0.214047897279587,1.29405949356574,
-7.4552200665951));
#149319=CARTESIAN_POINT('Ctrl Pts',(-0.215486066129174,1.28783500491842,
-7.49690374451352));
#149320=CARTESIAN_POINT('',(0.459087249099366,1.19797317561536,-7.35970375387002));
#149321=CARTESIAN_POINT('Ctrl Pts',(-0.202314096,1.327885473,-7.247176623));
#149322=CARTESIAN_POINT('Ctrl Pts',(-0.550074039,1.27059961,-7.237468465));
#149323=CARTESIAN_POINT('Ctrl Pts',(-0.895306583,1.214285714,-7.194506663));
#149324=CARTESIAN_POINT('Ctrl Pts',(-0.945231961,1.20614195,-7.188293795));
#149325=CARTESIAN_POINT('Ctrl Pts',(-0.995066308,1.197973174,-7.18138865700001));
#149326=CARTESIAN_POINT('Ctrl Pts',(0.036691991,1.327885473,-7.499910246));
#149327=CARTESIAN_POINT('Ctrl Pts',(-0.32319552,1.27059961,-7.501670932));
#149328=CARTESIAN_POINT('Ctrl Pts',(-0.68159806,1.214285714,-7.468964057));
#149329=CARTESIAN_POINT('Ctrl Pts',(-0.733428001,1.20614195,-7.464234193));
#149330=CARTESIAN_POINT('Ctrl Pts',(-0.785187309000001,1.197973174,-7.458785484));
#149331=CARTESIAN_POINT('',(-0.891176199469163,1.19797317334243,-7.31870008685522));
#149332=CARTESIAN_POINT('Ctrl Pts',(-0.968457199100814,1.19354381560796,
-7.18507566364082));
#149333=CARTESIAN_POINT('Ctrl Pts',(-0.981761753550408,1.19575849480399,
-7.18323216032035));
#149334=CARTESIAN_POINT('Ctrl Pts',(-0.995066308,1.197973174,-7.181388657));
#149335=CARTESIAN_POINT('Ctrl Pts',(-1.383919549,1.262701774,-7.127508443));
#149336=CARTESIAN_POINT('Ctrl Pts',(-1.764681383,1.327878141,-7.031955604));
#149337=CARTESIAN_POINT('Ctrl Pts',(-1.2456388240592,1.19354381560796,-7.39641134329257));
#149338=CARTESIAN_POINT('Ctrl Pts',(-1.25933300010969,1.19575849480399,
-7.39405287748723));
#149339=CARTESIAN_POINT('Ctrl Pts',(-1.27302717616021,1.197973174,-7.39169441168189));
#149340=CARTESIAN_POINT('Ctrl Pts',(-1.67326791779803,1.262701774,-7.3227633493398));
#149341=CARTESIAN_POINT('Ctrl Pts',(-2.06372551153718,1.327878141,-7.21101806044767));
#149342=CARTESIAN_POINT('',(-1.27246312940616,1.19797317455041,-7.39126765888065));
#149343=CARTESIAN_POINT('',(-1.82206082722797,1.28783500530981,-7.27530716460066));
#149344=CARTESIAN_POINT('Origin',(0.0544441017013819,1.33927126085593,0.183360881233009));
#149345=CARTESIAN_POINT('Ctrl Pts',(-1.76013796609859,1.32710049327885,
-7.03309422332733));
#149346=CARTESIAN_POINT('Ctrl Pts',(-1.77040642661513,1.32022179858301,
-7.07341225150022));
#149347=CARTESIAN_POINT('Ctrl Pts',(-1.78070779347286,1.31351590010311,
-7.11377823212063));
#149348=CARTESIAN_POINT('Ctrl Pts',(-1.80134626890961,1.30043858904812,
-7.19450196890768));
#149349=CARTESIAN_POINT('Ctrl Pts',(-1.81169551593028,1.29405949356084,
-7.23490719362557));
#149350=CARTESIAN_POINT('Ctrl Pts',(-1.82206081984535,1.28783500492573,
-7.27530716638796));
#149351=CARTESIAN_POINT('',(-1.13376471150132,1.19797317561536,-7.28632815855581));
#149352=CARTESIAN_POINT('Origin',(-2.23020386880268E-13,1.28891221000011,
-6.04551131377917E-13));
#149353=CARTESIAN_POINT('',(-1.82735151989587,1.10830076259781,-7.27398009464002));
#149354=CARTESIAN_POINT('Origin',(0.0695339604227713,0.946580200554579,
0.171042320190786));
#149355=CARTESIAN_POINT('',(-2.37024845919407,1.19797317358555,-7.11561116450251));
#149356=CARTESIAN_POINT('Origin',(0.0798126674574673,1.33917527750901,0.168262470116188));
#149357=CARTESIAN_POINT('Ctrl Pts',(-1.82206083427004,1.28783500479117,
-7.27530716301513));
#149358=CARTESIAN_POINT('Ctrl Pts',(-1.97350366785731,1.26310656824179,
-7.23737913475084));
#149359=CARTESIAN_POINT('Ctrl Pts',(-2.12337557015445,1.23856749893597,
-7.19481460220206));
#149360=CARTESIAN_POINT('Ctrl Pts',(-2.27126916793713,1.21428571428671,
-7.14782039273359));
#149361=CARTESIAN_POINT('Ctrl Pts',(-2.30431093621273,1.20886077964635,
-7.13732114325402));
#149362=CARTESIAN_POINT('Ctrl Pts',(-2.33730571565235,1.20342302038954,
-7.12658456987032));
#149363=CARTESIAN_POINT('Ctrl Pts',(-2.37024845855447,1.1979731744789,-7.11561116452552));
#149364=CARTESIAN_POINT('Ctrl Pts',(-1.755512854,1.327885473,-7.034250111));
#149365=CARTESIAN_POINT('Ctrl Pts',(-2.093055395,1.27059961,-6.950010816));
#149366=CARTESIAN_POINT('Ctrl Pts',(-2.420981077,1.214285714,-6.833838645));
#149367=CARTESIAN_POINT('Ctrl Pts',(-2.468403645,1.20614195,-6.81703855));
#149368=CARTESIAN_POINT('Ctrl Pts',(-2.515588492,1.197973174,-6.799581939));
#149369=CARTESIAN_POINT('Ctrl Pts',(-1.576424854,1.327885473,-7.332454206));
#149370=CARTESIAN_POINT('Ctrl Pts',(-1.928276891,1.27059961,-7.256808551));
#149371=CARTESIAN_POINT('Ctrl Pts',(-2.271269168,1.214285714,-7.147820393));
#149372=CARTESIAN_POINT('Ctrl Pts',(-2.320870572,1.20614195,-7.132059205));
#149373=CARTESIAN_POINT('Ctrl Pts',(-2.370248465,1.197973174,-7.115611162));
#149374=CARTESIAN_POINT('',(-2.44291847467279,1.19797317334243,-6.95759655184379));
#149375=CARTESIAN_POINT('Ctrl Pts',(-2.49039408591104,1.1935438154537,-6.80890291765712));
#149376=CARTESIAN_POINT('Ctrl Pts',(-2.50299128895552,1.19575849472686,
-6.80424242832863));
#149377=CARTESIAN_POINT('Ctrl Pts',(-2.515588492,1.197973174,-6.799581939));
#149378=CARTESIAN_POINT('Ctrl Pts',(-2.883767906,1.262701774,-6.663369462));
#149379=CARTESIAN_POINT('Ctrl Pts',(-3.235086705,1.327878141,-6.488198056));
#149380=CARTESIAN_POINT('Ctrl Pts',(-2.80652628216,1.1935438154537,-6.95571182999812));
#149381=CARTESIAN_POINT('Ctrl Pts',(-2.81939329600743,1.19575849472686,
-6.95046466061263));
#149382=CARTESIAN_POINT('Ctrl Pts',(-2.8322603098548,1.197973174,-6.94521749122715));
#149383=CARTESIAN_POINT('Ctrl Pts',(-3.20832550476615,1.262701774,-6.79185807146668));
#149384=CARTESIAN_POINT('Ctrl Pts',(-3.56563248304387,1.327878141,-6.59878848428515));
#149385=CARTESIAN_POINT('',(-2.8316177091298,1.19797317454273,-6.94492196922394));
#149386=CARTESIAN_POINT('',(-3.34343804166085,1.28783500532529,-6.7135253081941));
#149387=CARTESIAN_POINT('Origin',(0.0925882930369026,1.33927124656572,0.1673699350441));
#149388=CARTESIAN_POINT('Ctrl Pts',(-3.23089427947231,1.32710049338896,
-6.49028675465296));
#149389=CARTESIAN_POINT('Ctrl Pts',(-3.24958985330599,1.32022179872908,
-6.52745475421011));
#149390=CARTESIAN_POINT('Ctrl Pts',(-3.26832787295305,1.31351590012493,
-6.56466251208682));
#149391=CARTESIAN_POINT('Ctrl Pts',(-3.30583704956096,1.30043858908713,
-6.63906231072451));
#149392=CARTESIAN_POINT('Ctrl Pts',(-3.32463026587,1.2940594936109,-6.67629810155961));
#149393=CARTESIAN_POINT('Ctrl Pts',(-3.34343803473179,1.28783500495311,
-6.71352531163254));
#149394=CARTESIAN_POINT('',(-2.67360309456954,1.19797317561536,-6.87225195616886));
#149395=CARTESIAN_POINT('Origin',(5.89589141397617E-13,1.28891220999994,
1.17961196366423E-12));
#149396=CARTESIAN_POINT('',(-3.34831975995875,1.10830076259067,-6.71109192160037));
#149397=CARTESIAN_POINT('Origin',(0.104677516905148,0.9465801534167,0.15209608589477));
#149398=CARTESIAN_POINT('',(-3.84447943177203,1.19797317358555,-6.43971877546426));
#149399=CARTESIAN_POINT('Origin',(0.11411821151431,1.33917529218569,0.147171347802511));
#149400=CARTESIAN_POINT('Ctrl Pts',(-3.34343804816636,1.28783500479116,
-6.71352530479133));
#149401=CARTESIAN_POINT('Ctrl Pts',(-3.48318682739452,1.26310656825249,
-6.6439282802113));
#149402=CARTESIAN_POINT('Ctrl Pts',(-3.62040469149621,1.23856749894659,
-6.57014085403775));
#149403=CARTESIAN_POINT('Ctrl Pts',(-3.75473825356999,1.21428571428671,
-6.49245259106127));
#149404=CARTESIAN_POINT('Ctrl Pts',(-3.78475049544037,1.20886077964635,
-6.47509580469347));
#149405=CARTESIAN_POINT('Ctrl Pts',(-3.81466582933347,1.20342302038954,
-6.45751734418185));
#149406=CARTESIAN_POINT('Ctrl Pts',(-3.84447943092854,1.1979731744789,-6.43971877531678));
#149407=CARTESIAN_POINT('Ctrl Pts',(-3.226625782,1.327885473,-6.492409881));
#149408=CARTESIAN_POINT('Ctrl Pts',(-3.538167808,1.27059961,-6.337578385));
#149409=CARTESIAN_POINT('Ctrl Pts',(-3.833453187,1.214285714,-6.153627927));
#149410=CARTESIAN_POINT('Ctrl Pts',(-3.876155517,1.20614195,-6.127026159));
#149411=CARTESIAN_POINT('Ctrl Pts',(-3.918484554,1.197973174,-6.099834326));
#149412=CARTESIAN_POINT('Ctrl Pts',(-3.115829826,1.327885473,-6.822140756));
#149413=CARTESIAN_POINT('Ctrl Pts',(-3.443194178,1.27059961,-6.672625868));
#149414=CARTESIAN_POINT('Ctrl Pts',(-3.754738253,1.214285714,-6.492452591));
#149415=CARTESIAN_POINT('Ctrl Pts',(-3.799791815,1.20614195,-6.466397055));
#149416=CARTESIAN_POINT('Ctrl Pts',(-3.844479437,1.197973174,-6.439718772));
#149417=CARTESIAN_POINT('',(-3.88148199205115,1.19797317334243,-6.26977655113511));
#149418=CARTESIAN_POINT('Ctrl Pts',(-3.89588291386022,1.19354381541423,
-6.11435343807459));
#149419=CARTESIAN_POINT('Ctrl Pts',(-3.90718373393015,1.19575849470712,
-6.10709388203729));
#149420=CARTESIAN_POINT('Ctrl Pts',(-3.918484554,1.197973174,-6.099834326));
#149421=CARTESIAN_POINT('Ctrl Pts',(-4.248774481,1.262701774,-5.88765873000001));
#149422=CARTESIAN_POINT('Ctrl Pts',(-4.554222968,1.327878141,-5.64105957800001));
#149423=CARTESIAN_POINT('Ctrl Pts',(-4.23618369053357,1.19354381541423,
-6.18977096269262));
#149424=CARTESIAN_POINT('Ctrl Pts',(-4.24762189454677,1.19575849470712,
-6.18188044151138));
#149425=CARTESIAN_POINT('Ctrl Pts',(-4.25906009855998,1.197973174,-6.17398992033001));
#149426=CARTESIAN_POINT('Ctrl Pts',(-4.59336535651276,1.262701774,-5.94337305811416));
#149427=CARTESIAN_POINT('Ctrl Pts',(-4.90081444214904,1.327878141,-5.67800689188693));
#149428=CARTESIAN_POINT('',(-4.25836899300359,1.19797317454273,-6.17383944762984));
#149429=CARTESIAN_POINT('',(-4.70847980871937,1.28783500530451,-5.8378264697988));
#149430=CARTESIAN_POINT('Origin',(0.126403182263362,1.33927124458626,0.143553125576412));
#149431=CARTESIAN_POINT('Ctrl Pts',(-4.55057756705452,1.32710049336331,
-5.64400069165213));
#149432=CARTESIAN_POINT('Ctrl Pts',(-4.57682609843695,1.32022179125174,
-5.67628076316447));
#149433=CARTESIAN_POINT('Ctrl Pts',(-4.60312463505521,1.31351588473637,
-5.70859054488373));
#149434=CARTESIAN_POINT('Ctrl Pts',(-4.65575056354625,1.30043858906023,
-5.77318747748391));
#149435=CARTESIAN_POINT('Ctrl Pts',(-4.68210899927401,1.29405949356967,
-5.80551273035381));
#149436=CARTESIAN_POINT('Ctrl Pts',(-4.70847980266873,1.28783500491202,
-5.83782647466103));
#149437=CARTESIAN_POINT('',(-4.08842676807871,1.19797317561536,-6.13683689011035));
#149438=CARTESIAN_POINT('Origin',(4.31512464649231E-13,1.28891221,4.57533316788883E-13));
#149439=CARTESIAN_POINT('',(-4.7127242894234,1.10830076263122,-5.83440054895487));
#149440=CARTESIAN_POINT('Origin',(0.134926314667311,0.946580160217586,0.126037513835028));
#149441=CARTESIAN_POINT('',(-5.13894681866872,1.19797317358555,-5.46271229354926));
#149442=CARTESIAN_POINT('Origin',(0.143087622784005,1.33917531549964,0.119198448529405));
#149443=CARTESIAN_POINT('Ctrl Pts',(-4.70847981442621,1.28783500479116,
-5.83782646514444));
#149444=CARTESIAN_POINT('Ctrl Pts',(-4.83000004185364,1.26310656824579,
-5.73981472373645));
#149445=CARTESIAN_POINT('Ctrl Pts',(-4.9481477130839,1.23856749893994,-5.63825462191149));
#149446=CARTESIAN_POINT('Ctrl Pts',(-5.06263995080713,1.21428571428671,
-5.5335049226048));
#149447=CARTESIAN_POINT('Ctrl Pts',(-5.0882193270905,1.20886077964635,-5.51010218345481));
#149448=CARTESIAN_POINT('Ctrl Pts',(-5.11365640767485,1.20342302038954,
-5.48650378512226));
#149449=CARTESIAN_POINT('Ctrl Pts',(-5.13894681787265,1.1979731744789,-5.46271229363917));
#149450=CARTESIAN_POINT('Ctrl Pts',(-4.546865274,1.327885473,-5.646991781));
#149451=CARTESIAN_POINT('Ctrl Pts',(-4.817839426,1.27059961,-5.428807833));
#149452=CARTESIAN_POINT('Ctrl Pts',(-5.066677286,1.214285714,-5.185680407));
#149453=CARTESIAN_POINT('Ctrl Pts',(-5.102662666,1.20614195,-5.150520834));
#149454=CARTESIAN_POINT('Ctrl Pts',(-5.138156632,1.197973174,-5.11486524));
#149455=CARTESIAN_POINT('Ctrl Pts',(-4.509542057,1.327885473,-5.992831587));
#149456=CARTESIAN_POINT('Ctrl Pts',(-4.79711153099999,1.27059961,-5.776438615));
#149457=CARTESIAN_POINT('Ctrl Pts',(-5.062639951,1.214285714,-5.533504923));
#149458=CARTESIAN_POINT('Ctrl Pts',(-5.101039015,1.20614195,-5.498373367));
#149459=CARTESIAN_POINT('Ctrl Pts',(-5.138946823,1.197973174,-5.462712289));
#149460=CARTESIAN_POINT('',(-5.1385517245908,1.19797317334244,-5.28878876732656));
#149461=CARTESIAN_POINT('Ctrl Pts',(-5.11920458538267,1.19354381539211,
-5.13390358796375));
#149462=CARTESIAN_POINT('Ctrl Pts',(-5.12868060869134,1.19575849469606,
-5.12438441398191));
#149463=CARTESIAN_POINT('Ctrl Pts',(-5.138156632,1.197973174,-5.11486524));
#149464=CARTESIAN_POINT('Ctrl Pts',(-5.415113084,1.262701774,-4.83664762));
#149465=CARTESIAN_POINT('Ctrl Pts',(-5.660408826,1.327878141,-4.530151423));
#149466=CARTESIAN_POINT('Ctrl Pts',(-5.46776185838861,1.19354381539211,
-5.13440328426325));
#149467=CARTESIAN_POINT('Ctrl Pts',(-5.47723641480399,1.19575849469606,
-5.12423836326934));
#149468=CARTESIAN_POINT('Ctrl Pts',(-5.48671097121949,1.197973174,-5.11407344227553));
#149469=CARTESIAN_POINT('Ctrl Pts',(-5.76362455022114,1.262701774,-4.81698252537818));
#149470=CARTESIAN_POINT('Ctrl Pts',(-6.00683976539369,1.327878141,-4.491728007792));
#149471=CARTESIAN_POINT('',(-5.48600367772827,1.19797317455045,-5.11407505386022));
#149472=CARTESIAN_POINT('',(-5.85335829410381,1.28783500453097,-4.68915735316194));
#149473=CARTESIAN_POINT('Origin',(0.154307624290183,1.33927127224265,0.113023985986638));
#149474=CARTESIAN_POINT('Ctrl Pts',(-5.65748090612999,1.32710049329292,
-4.53380742867848));
#149475=CARTESIAN_POINT('Ctrl Pts',(-5.69005498758505,1.32022179858842,
-4.55969012397402));
#149476=CARTESIAN_POINT('Ctrl Pts',(-5.72268428531977,1.31351590006272,
-4.585591079946));
#149477=CARTESIAN_POINT('Ctrl Pts',(-5.78796635628563,1.30043858911412,
-4.63736481368175));
#149478=CARTESIAN_POINT('Ctrl Pts',(-5.82065751952999,1.29405949377568,
-4.6632680349132));
#149479=CARTESIAN_POINT('Ctrl Pts',(-5.85335828919288,1.28783500490905,
-4.68915735945583));
#149480=CARTESIAN_POINT('',(-5.31208014948166,1.19797317561536,-5.11447015178951));
#149481=CARTESIAN_POINT('Ctrl Pts',(-5.6544984,1.327885473,-4.537526622));
#149482=CARTESIAN_POINT('Ctrl Pts',(-5.87223422700001,1.27059961,-4.266192261));
#149483=CARTESIAN_POINT('Ctrl Pts',(-6.062989186,1.214285714,-3.975256234));
#149484=CARTESIAN_POINT('Ctrl Pts',(-6.090574979,1.20614195,-3.93318288));
#149485=CARTESIAN_POINT('Ctrl Pts',(-6.117574218,1.197973174,-3.89073074));
#149486=CARTESIAN_POINT('Ctrl Pts',(-5.692393115,1.327885473,-4.883304274));
#149487=CARTESIAN_POINT('Ctrl Pts',(-5.926721282,1.27059961,-4.610151513));
#149488=CARTESIAN_POINT('Ctrl Pts',(-6.133818231,1.214285714,-4.315816714));
#149489=CARTESIAN_POINT('Ctrl Pts',(-6.163767301,1.20614195,-4.27325185));
#149490=CARTESIAN_POINT('Ctrl Pts',(-6.193122768,1.197973174,-4.23027545));
#149491=CARTESIAN_POINT('',(-6.19312276474044,1.19797317358555,-4.23027545534309));
#149492=CARTESIAN_POINT('Ctrl Pts',(-5.85335829882788,1.28783500243923,
-4.68915734706597));
#149493=CARTESIAN_POINT('Ctrl Pts',(-5.95096782342481,1.26310656739011,
-4.56731380918563));
#149494=CARTESIAN_POINT('Ctrl Pts',(-6.04452084762123,1.23856749886486,
-4.44272986964504));
#149495=CARTESIAN_POINT('Ctrl Pts',(-6.13381823140048,1.21428571428671,
-4.31581671345517));
#149496=CARTESIAN_POINT('Ctrl Pts',(-6.15376867898799,1.20886077964635,
-4.28746230749643));
#149497=CARTESIAN_POINT('Ctrl Pts',(-6.17353809688187,1.20342302038954,
-4.25894740590532));
#149498=CARTESIAN_POINT('Ctrl Pts',(-6.19312276398085,1.1979731744789,-4.23027545560123));
#149499=CARTESIAN_POINT('',(-6.15534849076645,1.19797317334244,-4.06050309838586));
#149500=CARTESIAN_POINT('Origin',(-4.3454823073219E-13,1.28891221000039,
-3.61689844741164E-13));
#149501=CARTESIAN_POINT('',(-5.85676706859327,1.10830076259405,-4.68489909144703));
#149502=CARTESIAN_POINT('Origin',(0.158866080899274,0.946580167380763,0.0940856020174308));
#149503=CARTESIAN_POINT('Origin',(0.165366462737506,1.33917528531327,0.0856520574936748));
#149504=CARTESIAN_POINT('Ctrl Pts',(-6.10315794204819,1.19354381548963,
-3.91339811126932));
#149505=CARTESIAN_POINT('Ctrl Pts',(-6.11036608002404,1.19575849474482,
-3.9020644256347));
#149506=CARTESIAN_POINT('Ctrl Pts',(-6.117574218,1.197973174,-3.89073074));
#149507=CARTESIAN_POINT('Ctrl Pts',(-6.328247018,1.262701774,-3.559480243));
#149508=CARTESIAN_POINT('Ctrl Pts',(-6.501920259,1.327878141,-3.207418423));
#149509=CARTESIAN_POINT('Ctrl Pts',(-6.4436735601197,1.19354381548963,-3.83895661449708));
#149510=CARTESIAN_POINT('Ctrl Pts',(-6.45074144893707,1.19575849474482,
-3.82699259442523));
#149511=CARTESIAN_POINT('Ctrl Pts',(-6.45780933775458,1.197973174,-3.81502857435344));
#149512=CARTESIAN_POINT('Ctrl Pts',(-6.66438306487192,1.262701774,-3.46535524454349));
#149513=CARTESIAN_POINT('Ctrl Pts',(-6.83199193698954,1.327878141,-3.09542091445431));
#149514=CARTESIAN_POINT('',(-6.45711892681566,1.19797317455041,-3.81518219547778));
#149515=CARTESIAN_POINT('',(-6.28734656821292,1.19797317561532,-3.85295647362759));
#149516=CARTESIAN_POINT('',(-6.72454025005821,1.28783500528777,-3.32122845155774));
#149517=CARTESIAN_POINT('Origin',(0.17499692100152,1.33927123071157,0.0772100261152464));
#149518=CARTESIAN_POINT('Ctrl Pts',(-6.49984672608352,1.32710049312117,
-3.21161837007158));
#149519=CARTESIAN_POINT('Ctrl Pts',(-6.53722325789545,1.32022179843905,
-3.22989347770123));
#149520=CARTESIAN_POINT('Ctrl Pts',(-6.57465763980289,1.31351590006666,
-3.24817454885908));
#149521=CARTESIAN_POINT('Ctrl Pts',(-6.64954327505303,1.30043858901477,
-3.28470412634283));
#149522=CARTESIAN_POINT('Ctrl Pts',(-6.68703856467982,1.29405949354876,
-3.30297411135391));
#149523=CARTESIAN_POINT('Ctrl Pts',(-6.72454024663977,1.2878350049003,-3.32122845844845));
#149524=CARTESIAN_POINT('Origin',(1.40729441988618E-12,1.28891221000011,
6.29704621779581E-13));
#149525=CARTESIAN_POINT('',(-6.95771517296809,1.19797317358553,-2.80003563894104));
#149526=CARTESIAN_POINT('Ctrl Pts',(-6.72454025316532,1.28783500479118,
-3.32122844495214));
#149527=CARTESIAN_POINT('Ctrl Pts',(-6.79367496246426,1.26310656823154,
-3.18125037862002));
#149528=CARTESIAN_POINT('Ctrl Pts',(-6.85825890481461,1.2385674989258,-3.03946800716173));
#149529=CARTESIAN_POINT('Ctrl Pts',(-6.91818598841636,1.21428571428671,
-2.896325711946));
#149530=CARTESIAN_POINT('Ctrl Pts',(-6.93157464648079,1.20886077964635,
-2.86434545977925));
#149531=CARTESIAN_POINT('Ctrl Pts',(-6.94475200541248,1.20342302038954,
-2.83224738030942));
#149532=CARTESIAN_POINT('Ctrl Pts',(-6.9577151722647,1.19797317447889,-2.80003563935131));
#149533=CARTESIAN_POINT('',(-6.72695392951754,1.10830076261231,-3.31633695910702));
#149534=CARTESIAN_POINT('Origin',(0.175377431229771,0.946580208288621,0.0577343816384296));
#149535=CARTESIAN_POINT('Origin',(0.179912927810285,1.33917528002472,0.0481006479961876));
#149536=CARTESIAN_POINT('Ctrl Pts',(-6.497733465,1.327885473,-3.215891761));
#149537=CARTESIAN_POINT('Ctrl Pts',(-6.652049883,1.27059961,-2.90409428));
#149538=CARTESIAN_POINT('Ctrl Pts',(-6.775802451,1.214285714,-2.578953498));
#149539=CARTESIAN_POINT('Ctrl Pts',(-6.793698776,1.20614195,-2.531933665));
#149540=CARTESIAN_POINT('Ctrl Pts',(-6.810940832,1.197973174,-2.484669994));
#149541=CARTESIAN_POINT('Ctrl Pts',(-6.609074196,1.327885473,-3.54543908));
#149542=CARTESIAN_POINT('Ctrl Pts',(-6.779204132,1.27059961,-3.22829885));
#149543=CARTESIAN_POINT('Ctrl Pts',(-6.918185988,1.214285714,-2.896325712));
#149544=CARTESIAN_POINT('Ctrl Pts',(-6.938284678,1.20614195,-2.848317827));
#149545=CARTESIAN_POINT('Ctrl Pts',(-6.957715175,1.197973174,-2.800035633));
#149546=CARTESIAN_POINT('',(-6.88432800204646,1.19797317334241,-2.64235281728703));
#149547=CARTESIAN_POINT('Ctrl Pts',(-6.80173441512177,1.19354381538544,
-2.50990648843726));
#149548=CARTESIAN_POINT('Ctrl Pts',(-6.80633762356097,1.19575849469273,
-2.49728824121862));
#149549=CARTESIAN_POINT('Ctrl Pts',(-6.81094083199999,1.197973174,-2.484669994));
#149550=CARTESIAN_POINT('Ctrl Pts',(-6.945479154,1.262701774,-2.115875526));
#149551=CARTESIAN_POINT('Ctrl Pts',(-7.039409127,1.327878141,-1.734710103));
#149552=CARTESIAN_POINT('Ctrl Pts',(-7.11828624563922,1.19354381538545,
-2.36400460114487));
#149553=CARTESIAN_POINT('Ctrl Pts',(-7.12261698060608,1.19575849469273,
-2.35080090573385));
#149554=CARTESIAN_POINT('Ctrl Pts',(-7.12694771557288,1.197973174,-2.33759721032276));
#149555=CARTESIAN_POINT('Ctrl Pts',(-7.25352243474422,1.262701774,-1.9516918036216));
#149556=CARTESIAN_POINT('Ctrl Pts',(-7.33768775821218,1.327878141,-1.55437537983679));
#149557=CARTESIAN_POINT('',(-7.12630647006304,1.19797317455045,-2.33789565779545));
#149558=CARTESIAN_POINT('',(-7.2812901780632,1.287835005315,-1.79800259824859));
#149559=CARTESIAN_POINT('Origin',(0.187503276413901,1.33927124186361,0.0377856823255016));
#149560=CARTESIAN_POINT('Ctrl Pts',(-7.03828693514388,1.32710049342982,
-1.73925760526499));
#149561=CARTESIAN_POINT('Ctrl Pts',(-7.07871823223496,1.32022179874537,
-1.74907060143247));
#149562=CARTESIAN_POINT('Ctrl Pts',(-7.11920731040392,1.31351590012465,
-1.75887698603503));
#149563=CARTESIAN_POINT('Ctrl Pts',(-7.20019494033615,1.30043858906984,
-1.77845432421383));
#149564=CARTESIAN_POINT('Ctrl Pts',(-7.24074111772171,1.29405949358374,
-1.78823678820374));
#149565=CARTESIAN_POINT('Ctrl Pts',(-7.28129017620987,1.28783500493425,
-1.79800260570121));
#149566=CARTESIAN_POINT('',(-6.96862364819113,1.19797317561536,-2.41128283256266));
#149567=CARTESIAN_POINT('Origin',(-1.96891114523368E-13,1.28891221000006,
3.64291929955129E-14));
#149568=CARTESIAN_POINT('',(-7.28259590084126,1.10830076259393,-1.79270659643711));
#149569=CARTESIAN_POINT('Origin',(0.183688148092492,0.946580188782692,0.0186835548852868));
#149570=CARTESIAN_POINT('',(-7.39697255240153,1.19797317358549,-1.23886926827323));
#149571=CARTESIAN_POINT('Origin',(0.186046560972666,1.33917528776439,0.00830004920121169));
#149572=CARTESIAN_POINT('Ctrl Pts',(-7.28129017978068,1.28783500479116,
-1.79800259116314));
#149573=CARTESIAN_POINT('Ctrl Pts',(-7.31871741147635,1.26310656824645,
-1.64643521526425));
#149574=CARTESIAN_POINT('Ctrl Pts',(-7.35131239835908,1.23856749894059,
-1.49408399825204));
#149575=CARTESIAN_POINT('Ctrl Pts',(-7.37906705786735,1.21428571428673,
-1.34140573858062));
#149576=CARTESIAN_POINT('Ctrl Pts',(-7.38526788766403,1.20886077964635,
-1.30729500118915));
#149577=CARTESIAN_POINT('Ctrl Pts',(-7.39123702897003,1.20342302038953,
-1.2731146144405));
#149578=CARTESIAN_POINT('Ctrl Pts',(-7.39697255197882,1.19797317447889,
-1.23886926883833));
#149579=CARTESIAN_POINT('Ctrl Pts',(-7.037141735,1.327885473,-1.743885375));
#149580=CARTESIAN_POINT('Ctrl Pts',(-7.120823079,1.27059961,-1.406204078));
#149581=CARTESIAN_POINT('Ctrl Pts',(-7.171786724,1.214285714,-1.062061763));
#149582=CARTESIAN_POINT('Ctrl Pts',(-7.179156768,1.20614195,-1.012294047));
#149583=CARTESIAN_POINT('Ctrl Pts',(-7.185835423,1.197973174,-0.962428842));
#149584=CARTESIAN_POINT('Ctrl Pts',(-7.216722314,1.327885473,-2.041793095));
#149585=CARTESIAN_POINT('Ctrl Pts',(-7.314698931,1.27059961,-1.69549452));
#149586=CARTESIAN_POINT('Ctrl Pts',(-7.379067058,1.214285714,-1.341405739));
#149587=CARTESIAN_POINT('Ctrl Pts',(-7.38837557500001,1.20614195,-1.290199627));
#149588=CARTESIAN_POINT('Ctrl Pts',(-7.396972553,1.197973174,-1.238869262));
#149589=CARTESIAN_POINT('',(-7.29140398739447,1.19797317334234,-1.10064905601137));
#149590=CARTESIAN_POINT('Ctrl Pts',(-7.18226934733144,1.19354381530488,
-0.989054429223104));
#149591=CARTESIAN_POINT('Ctrl Pts',(-7.18405238516571,1.19575849465245,
-0.97574163561155));
#149592=CARTESIAN_POINT('Ctrl Pts',(-7.185835423,1.197973174,-0.962428841999999));
#149593=CARTESIAN_POINT('Ctrl Pts',(-7.23794840400001,1.262701774,-0.573334821));
#149594=CARTESIAN_POINT('Ctrl Pts',(-7.247743048,1.327878141,-0.180888666));
#149595=CARTESIAN_POINT('Ctrl Pts',(-7.46005577827158,1.19354381530488,
-0.778514360307321));
#149596=CARTESIAN_POINT('Ctrl Pts',(-7.46144685888638,1.19575849465245,
-0.764688379697061));
#149597=CARTESIAN_POINT('Ctrl Pts',(-7.46283793950117,1.197973174,-0.750862399086782));
#149598=CARTESIAN_POINT('Ctrl Pts',(-7.50349515734272,1.262701774,-0.346769423045057));
#149599=CARTESIAN_POINT('Ctrl Pts',(-7.50028145566704,1.327878141,0.0593510209700458));
#149600=CARTESIAN_POINT('',(-7.46227584405872,1.19797317455226,-0.751291715791706));
#149601=CARTESIAN_POINT('',(-7.49757506980534,1.28783500459391,-0.19070414176217));
#149602=CARTESIAN_POINT('Origin',(0.191242272114438,1.33927122495846,-0.00340538665022094));
#149603=CARTESIAN_POINT('Ctrl Pts',(-7.24762467125097,1.32710049336744,
-0.185571088325219));
#149604=CARTESIAN_POINT('Ctrl Pts',(-7.28922021123486,1.32022179866829,
-0.186463128251078));
#149605=CARTESIAN_POINT('Ctrl Pts',(-7.33087075978761,1.31351590009004,
-0.187336290002792));
#149606=CARTESIAN_POINT('Ctrl Pts',(-7.414173492925,1.30043858903658,-0.189045974345836));
#149607=CARTESIAN_POINT('Ctrl Pts',(-7.45587466365107,1.2940594935756,-0.189883500134146));
#149608=CARTESIAN_POINT('Ctrl Pts',(-7.4975750697091,1.28783500493827,-0.190704149264586));
#149609=CARTESIAN_POINT('',(-7.32405563182418,1.19797317561536,-0.856860287050402));
#149610=CARTESIAN_POINT('Origin',(-1.21127066710081E-12,1.28891221000044,
-1.97595845935483E-14));
#149611=CARTESIAN_POINT('',(-7.49771178195635,1.10830076263343,-0.185251266036125));
#149612=CARTESIAN_POINT('Origin',(0.183410112802487,0.946580183562984,-0.0212407687145654));
#149613=CARTESIAN_POINT('',(-7.49035571664319,1.19797317379343,0.380225251774696));
#149614=CARTESIAN_POINT('Origin',(0.183481502120748,1.33917532238901,-0.0318885222450997));
#149615=CARTESIAN_POINT('Ctrl Pts',(-7.49757506964849,1.28783500267511,
-0.190704134563331));
#149616=CARTESIAN_POINT('Ctrl Pts',(-7.50154476801412,1.26310656754432,
-0.0346345710151447));
#149617=CARTESIAN_POINT('Ctrl Pts',(-7.50062669414218,1.23856749894096,
0.121161718051112));
#149618=CARTESIAN_POINT('Ctrl Pts',(-7.49491115271031,1.21428571404002,
0.276236876004533));
#149619=CARTESIAN_POINT('Ctrl Pts',(-7.49363421046727,1.20886077969537,
0.310883118078491));
#149620=CARTESIAN_POINT('Ctrl Pts',(-7.49211602372626,1.20342302059146,
0.345547575253918));
#149621=CARTESIAN_POINT('Ctrl Pts',(-7.49035571612108,1.19797317510268,
0.380225251182368));
#149622=CARTESIAN_POINT('Ctrl Pts',(-7.247501079,1.327885473,-0.190336848));
#149623=CARTESIAN_POINT('Ctrl Pts',(-7.256634502,1.27059961,0.157438664));
#149624=CARTESIAN_POINT('Ctrl Pts',(-7.23242622,1.214285714,0.5044908));
#149625=CARTESIAN_POINT('Ctrl Pts',(-7.22892537,1.20614195,0.554679316));
#149626=CARTESIAN_POINT('Ctrl Pts',(-7.224728336,1.197973174,0.604814414));
#149627=CARTESIAN_POINT('Ctrl Pts',(-7.486924517,1.327885473,-0.442675134));
#149628=CARTESIAN_POINT('Ctrl Pts',(-7.50816653800001,1.27059961,-0.0834107510000001));
#149629=CARTESIAN_POINT('Ctrl Pts',(-7.494911153,1.214285714,0.276236876));
#149630=CARTESIAN_POINT('Ctrl Pts',(-7.492994242,1.20614195,0.328246873));
#149631=CARTESIAN_POINT('Ctrl Pts',(-7.490355716,1.197973174,0.380225258));
#149632=CARTESIAN_POINT('',(-7.35754202627095,1.19797317334235,0.492519831952287));
#149633=CARTESIAN_POINT('Ctrl Pts',(-7.22696934725185,1.19354381553843,
0.578044718798007));
#149634=CARTESIAN_POINT('Ctrl Pts',(-7.22584884162587,1.19575849476922,
0.59142956639901));
#149635=CARTESIAN_POINT('Ctrl Pts',(-7.224728336,1.197973174,0.604814414));
#149636=CARTESIAN_POINT('Ctrl Pts',(-7.191979232,1.262701774,0.996014383));
#149637=CARTESIAN_POINT('Ctrl Pts',(-7.117180559,1.327878141,1.381390924));
#149638=CARTESIAN_POINT('Ctrl Pts',(-7.45300139473422,1.19354381553843,
0.843378349190491));
#149639=CARTESIAN_POINT('Ctrl Pts',(-7.45138777556092,1.19575849476922,
0.857180126555084));
#149640=CARTESIAN_POINT('Ctrl Pts',(-7.44977415638769,1.197973174,0.870981903919677));
#149641=CARTESIAN_POINT('Ctrl Pts',(-7.40261278486015,1.262701774,1.27436751114721));
#149642=CARTESIAN_POINT('Ctrl Pts',(-7.31217032832715,1.327878141,1.67030223292065));
#149643=CARTESIAN_POINT('',(-7.44931749258291,1.19797317455044,0.870441788346016));
#149644=CARTESIAN_POINT('',(-7.36328168430241,1.28783500460275,1.42551142857604));
#149645=CARTESIAN_POINT('Origin',(0.18603945373218,1.33927128329711,-0.0444372817464886));
#149646=CARTESIAN_POINT('Ctrl Pts',(-7.11807153346965,1.32710049315711,
1.37679252683296));
#149647=CARTESIAN_POINT('Ctrl Pts',(-7.1588863551378,1.32022179848698,1.38486315380969));
#149648=CARTESIAN_POINT('Ctrl Pts',(-7.19975083979558,1.31351590012017,
1.39296404265902));
#149649=CARTESIAN_POINT('Ctrl Pts',(-7.28147353295054,1.30043858906693,
1.40920195516011));
#149650=CARTESIAN_POINT('Ctrl Pts',(-7.32237979679447,1.29405949359075,
1.41734852940739));
#149651=CARTESIAN_POINT('Ctrl Pts',(-7.36328168579721,1.2878350049424,1.42551142134503));
#149652=CARTESIAN_POINT('',(-7.33702291451221,1.19797317561536,0.737628093931804));
#149653=CARTESIAN_POINT('Origin',(-1.02912470212324E-12,1.28891221000017,
3.18809648819363E-13));
#149654=CARTESIAN_POINT('',(-7.36224299305575,1.10830076258289,1.43086620813176));
#149655=CARTESIAN_POINT('Origin',(0.1745561198956,0.946580177742715,-0.0601719581631782));
#149656=CARTESIAN_POINT('',(-7.23349817293615,1.19797317379341,1.98154086307437));
#149657=CARTESIAN_POINT('Origin',(0.172336708625885,1.33917532517151,-0.070586075733608));
#149658=CARTESIAN_POINT('Ctrl Pts',(-7.36328168274246,1.28783500269651,
1.42551143549193));
#149659=CARTESIAN_POINT('Ctrl Pts',(-7.33360822908143,1.26310656754608,
1.57878554712408));
#149660=CARTESIAN_POINT('Ctrl Pts',(-7.29922002229186,1.23856749893657,
1.73074204666147));
#149661=CARTESIAN_POINT('Ctrl Pts',(-7.2603015315847,1.21428571404458,1.88096296098956));
#149662=CARTESIAN_POINT('Ctrl Pts',(-7.25160652535969,1.20886077970096,
1.91452468837021));
#149663=CARTESIAN_POINT('Ctrl Pts',(-7.24267199974596,1.20342302059146,
1.94805234476405));
#149664=CARTESIAN_POINT('Ctrl Pts',(-7.23349817258391,1.19797317510269,
1.98154086236766));
#149665=CARTESIAN_POINT('Ctrl Pts',(-7.118975327,1.327885473,1.372111619));
#149666=CARTESIAN_POINT('Ctrl Pts',(-7.053133761,1.27059961,1.713719749));
#149667=CARTESIAN_POINT('Ctrl Pts',(-6.954885505,1.214285714,2.047453934));
#149668=CARTESIAN_POINT('Ctrl Pts',(-6.940677455,1.20614195,2.095716491));
#149669=CARTESIAN_POINT('Ctrl Pts',(-6.925800981,1.197973174,2.14377722));
#149670=CARTESIAN_POINT('Ctrl Pts',(-7.407046451,1.327885473,1.177141824));
#149671=CARTESIAN_POINT('Ctrl Pts',(-7.35056062300001,1.27059961,1.532573212));
#149672=CARTESIAN_POINT('Ctrl Pts',(-7.260301532,1.214285714,1.880962961));
#149673=CARTESIAN_POINT('Ctrl Pts',(-7.247248825,1.20614195,1.931344914));
#149674=CARTESIAN_POINT('Ctrl Pts',(-7.233498171,1.197973174,1.981540869));
#149675=CARTESIAN_POINT('',(-7.0796495771348,1.19797317334232,2.06265904060503));
#149676=CARTESIAN_POINT('Ctrl Pts',(-6.93374429210158,1.19354381539086,
2.11811513570332));
#149677=CARTESIAN_POINT('Ctrl Pts',(-6.92977263655074,1.19575849469544,
2.13094617785169));
#149678=CARTESIAN_POINT('Ctrl Pts',(-6.925800981,1.197973174,2.14377722));
#149679=CARTESIAN_POINT('Ctrl Pts',(-6.809721103,1.262701774,2.518791062));
#149680=CARTESIAN_POINT('Ctrl Pts',(-6.653826618,1.327878141,2.87907821));
#149681=CARTESIAN_POINT('Ctrl Pts',(-7.09745294900091,1.19354381539086,
2.42583562210593));
#149682=CARTESIAN_POINT('Ctrl Pts',(-7.09291008107509,1.19575849469544,
2.43896784156803));
#149683=CARTESIAN_POINT('Ctrl Pts',(-7.0883672131494,1.197973174,2.45210006103019));
#149684=CARTESIAN_POINT('Ctrl Pts',(-6.95559246774463,1.262701774,2.83591643522334));
#149685=CARTESIAN_POINT('Ctrl Pts',(-6.78215024268148,1.327878141,3.20315196996456));
#149686=CARTESIAN_POINT('',(-7.08803733486135,1.19797317454272,2.45147440199206));
#149687=CARTESIAN_POINT('',(-6.88468943126012,1.28783500530378,2.9750716687908));
#149688=CARTESIAN_POINT('Origin',(0.172137015649187,1.33927119313551,-0.0833912361227418));
#149689=CARTESIAN_POINT('Ctrl Pts',(-6.65568528020384,1.32710049335983,
2.87477885322754));
#149690=CARTESIAN_POINT('Ctrl Pts',(-6.69381092757056,1.3202217986674,2.89143477361773));
#149691=CARTESIAN_POINT('Ctrl Pts',(-6.73197857279038,1.3135159000738,2.90813092494699));
#149692=CARTESIAN_POINT('Ctrl Pts',(-6.80829996347872,1.3004385890334,2.9415571672601));
#149693=CARTESIAN_POINT('Ctrl Pts',(-6.84649858912149,1.29405949354624,
2.95830691665649));
#149694=CARTESIAN_POINT('Ctrl Pts',(-6.8846894342928,1.28783500491216,2.97507166173683));
#149695=CARTESIAN_POINT('',(-7.00691915965291,1.19797317561536,2.29762580488479));
#149696=CARTESIAN_POINT('Origin',(-1.52525561625261E-12,1.28891220999967,
5.94576471391051E-13));
#149697=CARTESIAN_POINT('',(-6.8825239041631,1.10830076262221,2.98007796857407));
#149698=CARTESIAN_POINT('Origin',(0.157539934978953,0.946580157411726,-0.0962895971539018));
#149699=CARTESIAN_POINT('',(-6.63841029328656,1.19797317358555,3.49020182563242));
#149700=CARTESIAN_POINT('Origin',(0.153133620362348,1.33917525765928,-0.105983085559498));
#149701=CARTESIAN_POINT('Ctrl Pts',(-6.88468942840868,1.28783500479116,
2.97507167549922));
#149702=CARTESIAN_POINT('Ctrl Pts',(-6.82276032021009,1.26310656824261,
3.11838340813306));
#149703=CARTESIAN_POINT('Ctrl Pts',(-6.75650993499366,1.23856749893679,
3.25939480124276));
#149704=CARTESIAN_POINT('Ctrl Pts',(-6.68620828108259,1.21428571428671,
3.39773730914892));
#149705=CARTESIAN_POINT('Ctrl Pts',(-6.67050177997188,1.20886077964635,
3.42864521292078));
#149706=CARTESIAN_POINT('Ctrl Pts',(-6.65456868331845,1.20342302038954,
3.45946835206213));
#149707=CARTESIAN_POINT('Ctrl Pts',(-6.63841029324666,1.19797317447889,
3.49020182489734));
#149708=CARTESIAN_POINT('Ctrl Pts',(-6.657574201,1.327885473,2.870401672));
#149709=CARTESIAN_POINT('Ctrl Pts',(-6.51983632400001,1.27059961,3.189869203));
#149710=CARTESIAN_POINT('Ctrl Pts',(-6.352142073,1.214285714,3.494680397));
#149711=CARTESIAN_POINT('Ctrl Pts',(-6.327891176,1.20614195,3.538760292));
#149712=CARTESIAN_POINT('Ctrl Pts',(-6.30303087,1.197973174,3.582499385));
#149713=CARTESIAN_POINT('Ctrl Pts',(-6.980823125,1.327885473,2.741916938));
#149714=CARTESIAN_POINT('Ctrl Pts',(-6.849250662,1.27059961,3.076895755));
#149715=CARTESIAN_POINT('Ctrl Pts',(-6.686208281,1.214285714,3.397737309));
#149716=CARTESIAN_POINT('Ctrl Pts',(-6.662630109,1.20614195,3.444135414));
#149717=CARTESIAN_POINT('Ctrl Pts',(-6.63841029,1.197973174,3.490201831));
#149718=CARTESIAN_POINT('',(-6.46904368484552,1.19797317334243,3.53681209221154));
#149719=CARTESIAN_POINT('Ctrl Pts',(-6.31630506021735,1.19354381545683,
3.55914484335768));
#149720=CARTESIAN_POINT('Ctrl Pts',(-6.30966796510867,1.19575849472843,
3.57082211417883));
#149721=CARTESIAN_POINT('Ctrl Pts',(-6.30303087,1.197973174,3.582499385));
#149722=CARTESIAN_POINT('Ctrl Pts',(-6.109047985,1.262701774,3.92379187));
#149723=CARTESIAN_POINT('Ctrl Pts',(-5.879347139,1.327878141,4.242142999));
#149724=CARTESIAN_POINT('Ctrl Pts',(-6.41003549123835,1.19354381545683,
3.8948635183192));
#149725=CARTESIAN_POINT('Ctrl Pts',(-6.4027757941272,1.19575849472843,3.90671213131973));
#149726=CARTESIAN_POINT('Ctrl Pts',(-6.39551609701611,1.197973174,3.91856074432019));
#149727=CARTESIAN_POINT('Ctrl Pts',(-6.1833363758006,1.262701774,4.26486106026454));
#149728=CARTESIAN_POINT('Ctrl Pts',(-5.93500435021084,1.327878141,4.5862258796775));
#149729=CARTESIAN_POINT('',(-6.3953284293054,1.19797317454266,3.91787879879043));
#149730=CARTESIAN_POINT('',(-6.0841767517999,1.28783500457832,4.38552086391292));
#149731=CARTESIAN_POINT('Origin',(0.150185964198979,1.33927126630319,-0.118446022870446));
#149732=CARTESIAN_POINT('Ctrl Pts',(-5.88208658127338,1.32710049336774,
4.23834371602909));
#149733=CARTESIAN_POINT('Ctrl Pts',(-5.91574034173286,1.32022179868773,
4.26280611729209));
#149734=CARTESIAN_POINT('Ctrl Pts',(-5.94942646977985,1.31351590006783,
4.28731683742319));
#149735=CARTESIAN_POINT('Ctrl Pts',(-6.0167778546574,1.30043858903083,4.33636843565603));
#149736=CARTESIAN_POINT('Ctrl Pts',(-6.05048271649278,1.29405949355569,
4.36093816053791));
#149737=CARTESIAN_POINT('Ctrl Pts',(-6.08417675618337,1.28783500491729,
4.38552085799059));
#149738=CARTESIAN_POINT('',(-6.34917965264557,1.19797317561517,3.7501890862884));
#149739=CARTESIAN_POINT('Origin',(-3.20056481317721E-13,1.28891220999967,
3.15719672627779E-13));
#149740=CARTESIAN_POINT('',(-6.08098564727152,1.10830076263549,4.38994459505371));
#149741=CARTESIAN_POINT('Origin',(0.133157366289638,0.946580186166513,-0.127904849618447));
#149742=CARTESIAN_POINT('',(-5.73291772724531,1.19797317379345,4.83566482943543));
#149743=CARTESIAN_POINT('Origin',(0.126770238043511,1.33917530768453,-0.136424485866898));
#149744=CARTESIAN_POINT('Ctrl Pts',(-6.08417674749869,1.2878350026744,4.38552086952979));
#149745=CARTESIAN_POINT('Ctrl Pts',(-5.99288772115719,1.26310656752983,
4.51216912600509));
#149746=CARTESIAN_POINT('Ctrl Pts',(-5.89787295184485,1.23856749892762,
4.63564187660495));
#149747=CARTESIAN_POINT('Ctrl Pts',(-5.79947536162801,1.21428571401319,
4.75563723596286));
#149748=CARTESIAN_POINT('Ctrl Pts',(-5.77749178415566,1.20886077966251,
4.78244609664098));
#149749=CARTESIAN_POINT('Ctrl Pts',(-5.7553051308146,1.20342302059143,4.80912346338656));
#149750=CARTESIAN_POINT('Ctrl Pts',(-5.73291772722294,1.1979731751026,4.8356648286461));
#149751=CARTESIAN_POINT('Ctrl Pts',(-5.884872305,1.327885473,4.234474933));
#149752=CARTESIAN_POINT('Ctrl Pts',(-5.681678587,1.27059961,4.516863918));
#149753=CARTESIAN_POINT('Ctrl Pts',(-5.452379538,1.214285714,4.77849949));
#149754=CARTESIAN_POINT('Ctrl Pts',(-5.419219739,1.20614195,4.81633559500001));
#149755=CARTESIAN_POINT('Ctrl Pts',(-5.385538041,1.197973174,4.853707861));
#149756=CARTESIAN_POINT('Ctrl Pts',(-6.228184269,1.327885473,4.178483064));
#149757=CARTESIAN_POINT('Ctrl Pts',(-6.027677353,1.27059961,4.477346072));
#149758=CARTESIAN_POINT('Ctrl Pts',(-5.799475362,1.214285714,4.755637236));
#149759=CARTESIAN_POINT('Ctrl Pts',(-5.766474213,1.20614195,4.795881969));
#149760=CARTESIAN_POINT('Ctrl Pts',(-5.73291772300001,1.197973174,4.835664834));
#149761=CARTESIAN_POINT('',(-5.55922788466497,1.19797317334242,4.84468634444197));
#149762=CARTESIAN_POINT('Ctrl Pts',(-5.4035224239318,1.19354381550955,4.8337528943271));
#149763=CARTESIAN_POINT('Ctrl Pts',(-5.39453023246583,1.19575849475478,
4.84373037766356));
#149764=CARTESIAN_POINT('Ctrl Pts',(-5.385538041,1.197973174,4.853707861));
#149765=CARTESIAN_POINT('Ctrl Pts',(-5.122722572,1.262701774,5.145320531));
#149766=CARTESIAN_POINT('Ctrl Pts',(-4.829955922,1.327878141,5.406849895));
#149767=CARTESIAN_POINT('Ctrl Pts',(-5.4228918982709,1.19354381550955,5.18177192569324));
#149768=CARTESIAN_POINT('Ctrl Pts',(-5.41325482741167,1.19575849475478,
5.19178290428964));
#149769=CARTESIAN_POINT('Ctrl Pts',(-5.40361775655257,1.197973174,5.20179388288622));
#149770=CARTESIAN_POINT('Ctrl Pts',(-5.12195434811186,1.262701774,5.49438552141966));
#149771=CARTESIAN_POINT('Ctrl Pts',(-4.81034425078659,1.327878141,5.7548529655605));
#149772=CARTESIAN_POINT('',(-5.40358107453905,1.19797317454273,5.20108753783366));
#149773=CARTESIAN_POINT('',(-4.9991747298791,1.28783500529405,5.59090797826665));
#149774=CARTESIAN_POINT('Origin',(0.121212383058121,1.33927125351804,-0.147962438566965));
#149775=CARTESIAN_POINT('Ctrl Pts',(-4.83344805204249,1.32710049314202,
5.40372833781476));
#149776=CARTESIAN_POINT('Ctrl Pts',(-4.86105631324101,1.32022179845642,
5.43485338557291));
#149777=CARTESIAN_POINT('Ctrl Pts',(-4.88868579701985,1.31351590010628,
5.46603257927555));
#149778=CARTESIAN_POINT('Ctrl Pts',(-4.94391790055482,1.30043858904295,
5.52841593545202));
#149779=CARTESIAN_POINT('Ctrl Pts',(-4.97155299698495,1.29405949356062,
5.55965678285503));
#149780=CARTESIAN_POINT('Ctrl Pts',(-4.99917473559828,1.28783500490659,
5.59090797313452));
#149781=CARTESIAN_POINT('',(-5.39455956189882,1.19797317561536,5.02739769459734));
#149782=CARTESIAN_POINT('Origin',(5.11309744544164E-13,1.28891220999989,
-5.71591385334358E-13));
#149783=CARTESIAN_POINT('',(-4.99510726048495,1.1083007625976,5.59454229148354));
#149784=CARTESIAN_POINT('Origin',(0.10254829428874,0.946580187984479,-0.153539229833606));
#149785=CARTESIAN_POINT('',(-4.55936029919686,1.19797317358555,5.95501752046846));
#149786=CARTESIAN_POINT('Origin',(0.0944792294308422,1.33917530994407,-0.16048687199922));
#149787=CARTESIAN_POINT('Ctrl Pts',(-4.99917472438475,1.28783500479116,
5.59090798306256));
#149788=CARTESIAN_POINT('Ctrl Pts',(-4.88279435342643,1.26310656823528,
5.69497083129256));
#149789=CARTESIAN_POINT('Ctrl Pts',(-4.76345798519044,1.23856749892951,
5.79513149076926));
#149790=CARTESIAN_POINT('Ctrl Pts',(-4.64156542093359,1.21428571428671,
5.89116885203553));
#149791=CARTESIAN_POINT('Ctrl Pts',(-4.61433269467536,1.20886077964635,
5.91262511711513));
#149792=CARTESIAN_POINT('Ctrl Pts',(-4.58692990753181,1.20342302038954,
5.93390930696844));
#149793=CARTESIAN_POINT('Ctrl Pts',(-4.55936029942225,1.19797317447889,
5.95501751970994));
#149794=CARTESIAN_POINT('Ctrl Pts',(-4.83700032,1.327885473,5.400548852));
#149795=CARTESIAN_POINT('Ctrl Pts',(-4.577851874,1.27059961,5.632655097));
#149796=CARTESIAN_POINT('Ctrl Pts',(-4.297669796,1.214285714,5.838881257));
#149797=CARTESIAN_POINT('Ctrl Pts',(-4.25715161,1.20614195,5.868704398));
#149798=CARTESIAN_POINT('Ctrl Pts',(-4.216223439,1.197973174,5.897962352));
#149799=CARTESIAN_POINT('Ctrl Pts',(-5.18432243800001,1.327885473,5.419667966));
#149800=CARTESIAN_POINT('Ctrl Pts',(-4.92425655,1.27059961,5.668440663));
#149801=CARTESIAN_POINT('Ctrl Pts',(-4.641565421,1.214285714,5.891168852));
#149802=CARTESIAN_POINT('Ctrl Pts',(-4.600684393,1.20614195,5.923378414));
#149803=CARTESIAN_POINT('Ctrl Pts',(-4.55936029400001,1.197973174,5.955017524));
#149804=CARTESIAN_POINT('',(-4.38779186976006,1.19797317334242,5.92648993558636));
#149805=CARTESIAN_POINT('Ctrl Pts',(-4.23807708524811,1.19354381545801,
5.88234003187642));
#149806=CARTESIAN_POINT('Ctrl Pts',(-4.2271502621241,1.19575849472901,5.89015119193821));
#149807=CARTESIAN_POINT('Ctrl Pts',(-4.216223439,1.197973174,5.897962352));
#149808=CARTESIAN_POINT('Ctrl Pts',(-3.896864346,1.262701774,6.126259723));
#149809=CARTESIAN_POINT('Ctrl Pts',(-3.554721335,1.327878141,6.3187385));
#149810=CARTESIAN_POINT('Ctrl Pts',(-4.18217990780254,1.193543815458,6.22638643642344));
#149811=CARTESIAN_POINT('Ctrl Pts',(-4.17061608171156,1.19575849472901,
6.23409167861179));
#149812=CARTESIAN_POINT('Ctrl Pts',(-4.15905225562061,1.197973174,6.24179692080016));
#149813=CARTESIAN_POINT('Ctrl Pts',(-3.82107542831418,1.262701774,6.46699862203382));
#149814=CARTESIAN_POINT('Ctrl Pts',(-3.46075780018589,1.327878141,6.65438952165839));
#149815=CARTESIAN_POINT('',(-4.1591682718737,1.19797317455222,6.24109920712169));
#149816=CARTESIAN_POINT('',(-3.68041685394524,1.28783500529536,6.53487044871798));
#149817=CARTESIAN_POINT('Origin',(0.0865708812706306,1.33927122581219,-0.170560125300614));
#149818=CARTESIAN_POINT('Ctrl Pts',(-3.5588028629224,1.32710049336213,6.31644062642552));
#149819=CARTESIAN_POINT('Ctrl Pts',(-3.57907469298459,1.32022179868322,
6.35277294787677));
#149820=CARTESIAN_POINT('Ctrl Pts',(-3.59935561044513,1.31351590010244,
6.38916271284325));
#149821=CARTESIAN_POINT('Ctrl Pts',(-3.63988584051283,1.30043858904339,
6.4619608502902));
#149822=CARTESIAN_POINT('Ctrl Pts',(-3.66015898505743,1.29405949355478,
6.49841203285239));
#149823=CARTESIAN_POINT('Ctrl Pts',(-3.68041686065727,1.28783500490144,
6.53487044492123));
#149824=CARTESIAN_POINT('',(-4.18769586182889,1.19797317561536,6.06953077425346));
#149825=CARTESIAN_POINT('Origin',(-4.98516158908835E-13,1.28891221000006,
6.29270940910587E-13));
#149826=CARTESIAN_POINT('',(-3.67566320884938,1.10830076262376,6.53754540854673));
#149827=CARTESIAN_POINT('Origin',(0.0671445181503139,0.946580160389495,
-0.171994674781133));
#149828=CARTESIAN_POINT('',(-3.17261225178722,1.19797317358555,6.79592021059555));
#149829=CARTESIAN_POINT('Origin',(0.0577704175746957,1.33917529164855,-0.177044994166941));
#149830=CARTESIAN_POINT('Ctrl Pts',(-3.68041684755842,1.28783500479116,
6.53487045228963));
#149831=CARTESIAN_POINT('Ctrl Pts',(-3.54438694874804,1.26310656823919,
6.6114820293681));
#149832=CARTESIAN_POINT('Ctrl Pts',(-3.40630901743123,1.23856749893339,
6.68364719669204));
#149833=CARTESIAN_POINT('Ctrl Pts',(-3.26662103946597,1.21428571428671,
6.75123595977197));
#149834=CARTESIAN_POINT('Ctrl Pts',(-3.23541253640364,1.20886077964635,
6.76633635817622));
#149835=CARTESIAN_POINT('Ctrl Pts',(-3.20407493953323,1.20342302038954,
6.78123214628162));
#149836=CARTESIAN_POINT('Ctrl Pts',(-3.17261225212519,1.19797317447889,
6.7959202097777));
#149837=CARTESIAN_POINT('Ctrl Pts',(-3.562955577,1.327885473,6.31409910900001));
#149838=CARTESIAN_POINT('Ctrl Pts',(-3.259969896,1.27059961,6.485069584));
#149839=CARTESIAN_POINT('Ctrl Pts',(-2.94200579,1.214285714,6.626243425));
#149840=CARTESIAN_POINT('Ctrl Pts',(-2.896023804,1.20614195,6.646659106));
#149841=CARTESIAN_POINT('Ctrl Pts',(-2.849762915,1.197973174,6.666434679));
#149842=CARTESIAN_POINT('Ctrl Pts',(-3.898047452,1.327885473,6.407435217));
#149843=CARTESIAN_POINT('Ctrl Pts',(-3.590582984,1.27059961,6.594485268));
#149844=CARTESIAN_POINT('Ctrl Pts',(-3.26662104,1.214285714,6.75123596));
#149845=CARTESIAN_POINT('Ctrl Pts',(-3.219771683,1.20614195,6.77390426700001));
#149846=CARTESIAN_POINT('Ctrl Pts',(-3.172612246,1.197973174,6.795920213));
#149847=CARTESIAN_POINT('',(-3.01118758420266,1.19797317334243,6.73117744434362));
#149848=CARTESIAN_POINT('Ctrl Pts',(-2.87446397243517,1.19354381542134,
6.65587548794217));
#149849=CARTESIAN_POINT('Ctrl Pts',(-2.86211344371758,1.19575849471068,
6.66115508347108));
#149850=CARTESIAN_POINT('Ctrl Pts',(-2.849762915,1.197973174,6.666434679));
#149851=CARTESIAN_POINT('Ctrl Pts',(-2.488793073,1.262701774,6.82074181900001));
#149852=CARTESIAN_POINT('Ctrl Pts',(-2.113271928,1.327878141,6.935169916));
#149853=CARTESIAN_POINT('Ctrl Pts',(-2.74591383263932,1.19354381542133,
6.97986203707782));
#149854=CARTESIAN_POINT('Ctrl Pts',(-2.73296396296722,1.19575849471068,
6.98490125425597));
#149855=CARTESIAN_POINT('Ctrl Pts',(-2.72001409329518,1.197973174,6.98994047143423));
#149856=CARTESIAN_POINT('Ctrl Pts',(-2.34152726764351,1.262701774,7.13722205509973));
#149857=CARTESIAN_POINT('Ctrl Pts',(-1.94935016118734,1.327878141,7.24277422096479));
#149858=CARTESIAN_POINT('',(-2.72027738496142,1.19797317455223,6.98928400998415));
#149859=CARTESIAN_POINT('',(-2.18956677597955,1.28783500531006,7.17326964054042));
#149860=CARTESIAN_POINT('Origin',(0.0478815178840269,1.33927122556283,-0.185182686033522));
#149861=CARTESIAN_POINT('Ctrl Pts',(-2.11775200747474,1.32710049331763,
6.9338031727206));
#149862=CARTESIAN_POINT('Ctrl Pts',(-2.12973953050717,1.32022179165342,
6.97364394945073));
#149863=CARTESIAN_POINT('Ctrl Pts',(-2.14172358183174,1.31351588565602,
7.01354278723912));
#149864=CARTESIAN_POINT('Ctrl Pts',(-2.16565676360449,1.30043858906236,
7.09335165801813));
#149865=CARTESIAN_POINT('Ctrl Pts',(-2.17762000653844,1.29405949359197,
7.13330875899285));
#149866=CARTESIAN_POINT('Ctrl Pts',(-2.18956678342661,1.28783500492658,
7.1732696382543));
#149867=CARTESIAN_POINT('',(-2.7850201573695,1.19797317561536,6.82785934067827));
#149868=CARTESIAN_POINT('Origin',(-1.96565853871622E-13,1.28891221000028,
6.45317133063372E-13));
#149869=CARTESIAN_POINT('',(-2.18434923164404,1.1083007626404,7.17486016787826));
#149870=CARTESIAN_POINT('Origin',(0.0286009841952251,0.946580155216993,
-0.182407723267577));
#149871=CARTESIAN_POINT('',(-1.63751638118294,1.19797317358554,7.31905322493337));
#149872=CARTESIAN_POINT('Origin',(0.0183603401137666,1.33917530561268,-0.185324740845644));
#149873=CARTESIAN_POINT('Ctrl Pts',(-2.1895667688656,1.28783500479116,7.17326964254652));
#149874=CARTESIAN_POINT('Ctrl Pts',(-2.04024794910754,1.26310656824512,
7.21884767627459));
#149875=CARTESIAN_POINT('Ctrl Pts',(-1.88988482534072,1.23856749893928,
7.25964298840125));
#149876=CARTESIAN_POINT('Ctrl Pts',(-1.73893308847782,1.21428571428671,
7.29562277765216));
#149877=CARTESIAN_POINT('Ctrl Pts',(-1.70520808358027,1.20886077964635,
7.30366123149123));
#149878=CARTESIAN_POINT('Ctrl Pts',(-1.6714009882543,1.20342302038954,7.31147210733639));
#149879=CARTESIAN_POINT('Ctrl Pts',(-1.63751638169677,1.19797317447889,
7.31905322426847));
#149880=CARTESIAN_POINT('Ctrl Pts',(-2.12231099,1.327885473,6.932409109));
#149881=CARTESIAN_POINT('Ctrl Pts',(-1.789655348,1.27059961,7.034249424));
#149882=CARTESIAN_POINT('Ctrl Pts',(-1.448776863,1.214285714,7.103769816));
#149883=CARTESIAN_POINT('Ctrl Pts',(-1.399481142,1.20614195,7.11382342199999));
#149884=CARTESIAN_POINT('Ctrl Pts',(-1.350050644,1.197973174,7.12319192899999));
#149885=CARTESIAN_POINT('Ctrl Pts',(-2.429504099,1.327885473,7.095597919));
#149886=CARTESIAN_POINT('Ctrl Pts',(-2.089017748,1.27059961,7.212179072));
#149887=CARTESIAN_POINT('Ctrl Pts',(-1.738933089,1.214285714,7.295622778));
#149888=CARTESIAN_POINT('Ctrl Pts',(-1.688306028,1.20614195,7.307689886));
#149889=CARTESIAN_POINT('Ctrl Pts',(-1.637516375,1.197973174,7.319053226));
#149890=CARTESIAN_POINT('',(-1.49378351347216,1.19797317334243,7.2211225766783));
#149891=CARTESIAN_POINT('Ctrl Pts',(-1.37644411718142,1.19354381561821,
7.11818960337276));
#149892=CARTESIAN_POINT('Ctrl Pts',(-1.36324738059071,1.19575849480912,
7.12069076618631));
#149893=CARTESIAN_POINT('Ctrl Pts',(-1.350050644,1.197973174,7.12319192900001));
#149894=CARTESIAN_POINT('Ctrl Pts',(-0.964348603,1.262701774,7.196293608));
#149895=CARTESIAN_POINT('Ctrl Pts',(-0.573008275,1.327878141,7.227320494));
#149896=CARTESIAN_POINT('Ctrl Pts',(-1.18125187711363,1.19354381561821,
7.40696704708603));
#149897=CARTESIAN_POINT('Ctrl Pts',(-1.16752148607158,1.19575849480912,
7.40910461085876));
#149898=CARTESIAN_POINT('Ctrl Pts',(-1.15379109502954,1.197973174,7.41124217463135));
#149899=CARTESIAN_POINT('Ctrl Pts',(-0.752491894106228,1.262701774,7.47371691633682));
#149900=CARTESIAN_POINT('Ctrl Pts',(-0.346793074702295,1.327878141,7.49249484662523));
#149901=CARTESIAN_POINT('',(-1.15418935087267,1.19797317455211,7.41065766083517));
#149902=CARTESIAN_POINT('',(-0.596334988833152,1.28783500530699,7.47625471614313));
#149903=CARTESIAN_POINT('Origin',(0.00695329922591664,1.33927121911688,
-0.191146606717507));
#149904=CARTESIAN_POINT('Ctrl Pts',(-0.577677421890293,1.32710049333146,
7.22694878924593));
#149905=CARTESIAN_POINT('Ctrl Pts',(-0.580820090687207,1.32022179867905,
7.26843503156666));
#149906=CARTESIAN_POINT('Ctrl Pts',(-0.583946887107583,1.31351590008168,
7.30997722414324));
#149907=CARTESIAN_POINT('Ctrl Pts',(-0.590163983057832,1.30043858905469,
7.39306522602624));
#149908=CARTESIAN_POINT('Ctrl Pts',(-0.593257936403517,1.29405949356778,
7.43465989577418));
#149909=CARTESIAN_POINT('Ctrl Pts',(-0.596334996445522,1.28783500492151,
7.47625471552231));
#149910=CARTESIAN_POINT('',(-1.25212000546965,1.19797317561497,7.26692479278219));
#149911=CARTESIAN_POINT('Origin',(1.50546553847296E-13,1.28891221000011,
-1.49446427455402E-12));
#149912=CARTESIAN_POINT('',(-0.590897511552974,1.10830076263119,7.47668644041972));
#149913=CARTESIAN_POINT('Origin',(-0.0112799890895166,0.946580205613589,
-0.184291155937752));
#149914=CARTESIAN_POINT('',(-0.0258520642582035,1.19797317358555,7.49995544522267));
#149915=CARTESIAN_POINT('Origin',(-0.0219082601936706,1.33917534714528,
-0.184938943114152));
#149916=CARTESIAN_POINT('Ctrl Pts',(-0.596334981605594,1.28783500479122,
7.47625471674912));
#149917=CARTESIAN_POINT('Ctrl Pts',(-0.440709222886166,1.26310656824116,
7.4886680289595));
#149918=CARTESIAN_POINT('Ctrl Pts',(-0.285091719071053,1.23856749893533,
7.49618594244474));
#149919=CARTESIAN_POINT('Ctrl Pts',(-0.129934559142799,1.21428571428671,
7.49887438288844));
#149920=CARTESIAN_POINT('Ctrl Pts',(-0.0952699962297192,1.20886077964635,
7.49947502299387));
#149921=CARTESIAN_POINT('Ctrl Pts',(-0.0605741846837616,1.20342302038954,
7.49983575874006));
#149922=CARTESIAN_POINT('Ctrl Pts',(-0.0258520649117424,1.19797317447889,
7.49995544458365));
#149923=CARTESIAN_POINT('Ctrl Pts',(-0.582429501,1.327885473,7.226567365));
#149924=CARTESIAN_POINT('Ctrl Pts',(-0.235658505,1.27059961,7.25451558));
#149925=CARTESIAN_POINT('Ctrl Pts',(0.112195259,1.214285714,7.249131826));
#149926=CARTESIAN_POINT('Ctrl Pts',(0.162499702,1.20614195,7.248353261));
#149927=CARTESIAN_POINT('Ctrl Pts',(0.212788494,1.197973174,7.246876641));
#149928=CARTESIAN_POINT('Ctrl Pts',(-0.847359835,1.327885473,7.451978349));
#149929=CARTESIAN_POINT('Ctrl Pts',(-0.489772364,1.27059961,7.492639398));
#149930=CARTESIAN_POINT('Ctrl Pts',(-0.129934559,1.214285714,7.498874383));
#149931=CARTESIAN_POINT('Ctrl Pts',(-0.07789706,1.20614195,7.499776047));
#149932=CARTESIAN_POINT('Ctrl Pts',(-0.025852058,1.197973174,7.499955445));
#149933=CARTESIAN_POINT('',(0.0946614167047613,1.19797317334243,7.37215064903207));
#149934=CARTESIAN_POINT('Ctrl Pts',(-1.64905696123129,4.559162772,7.31700065795431));
#149935=CARTESIAN_POINT('Ctrl Pts',(-1.24995303110202,4.624819703,7.40694804799773));
#149936=CARTESIAN_POINT('Ctrl Pts',(-0.843433619605153,4.690053947,7.45295291918589));
#149937=CARTESIAN_POINT('Ctrl Pts',(-0.829373780711526,4.69231013190792,
7.45454403896745));
#149938=CARTESIAN_POINT('Ctrl Pts',(-0.815313941817894,4.69456631681569,
7.45613515874913));
#149939=CARTESIAN_POINT('Ctrl Pts',(-1.360702703,4.559162772,7.12116480300001));
#149940=CARTESIAN_POINT('Ctrl Pts',(-0.97228059,4.624819703,7.19538398400001));
#149941=CARTESIAN_POINT('Ctrl Pts',(-0.578090317,4.690053947,7.226915773));
#149942=CARTESIAN_POINT('Ctrl Pts',(-0.564456892432628,4.69231013190792,
7.22800632823754));
#149943=CARTESIAN_POINT('Ctrl Pts',(-0.550823467865264,4.69456631681568,
7.2290968834751));
#149944=CARTESIAN_POINT('',(-0.842885263317961,4.69005394784289,7.45248581030807));
#149945=CARTESIAN_POINT('',(-0.710487785962877,4.69005394666591,7.33970078119719));
#149946=CARTESIAN_POINT('',(-1.40337283195863,4.59933049943207,7.36753314834207));
#149947=CARTESIAN_POINT('Origin',(0.0430257849586406,4.5535839336865,-0.186571753848842));
#149948=CARTESIAN_POINT('Ctrl Pts',(-1.35606856849621,4.55994605589074,
7.12204873926192));
#149949=CARTESIAN_POINT('Ctrl Pts',(-1.36398279156896,4.56683176235715,
7.1628961219797));
#149950=CARTESIAN_POINT('Ctrl Pts',(-1.37188477500109,4.57355155126864,
7.2037990962851));
#149951=CARTESIAN_POINT('Ctrl Pts',(-1.3876490014487,4.58666922563405,7.28561428031784));
#149952=CARTESIAN_POINT('Ctrl Pts',(-1.39552006202443,4.59307444478169,
7.32657226946014));
#149953=CARTESIAN_POINT('Ctrl Pts',(-1.40337283024197,4.59933049942395,
7.36753314861101));
#149954=CARTESIAN_POINT('Origin',(1.4658413372004E-13,4.78597145200391,
-9.49761103097301E-14));
#149955=CARTESIAN_POINT('',(-1.58832892089749,4.74999999914956,7.32988480407119));
#149956=CARTESIAN_POINT('',(-1.39282737490266,4.78575691075475,7.33314099135338));
#149957=CARTESIAN_POINT('Origin',(-1.36764295382465,4.80792738371137,-0.48930545689145));
#149958=CARTESIAN_POINT('',(-1.21292875863641,4.75000000020817,7.401270399065));
#149959=CARTESIAN_POINT('Origin',(0.,4.75,0.));
#149960=CARTESIAN_POINT('Origin',(1.42856873648812,5.02638720352195,0.290380960526179));
#149961=CARTESIAN_POINT('Ctrl Pts',(-1.954774922,4.690053947,7.24077723800001));
#149962=CARTESIAN_POINT('Ctrl Pts',(-1.559836226,4.624398499,7.347397871));
#149963=CARTESIAN_POINT('Ctrl Pts',(-1.155643991,4.559170361,7.410430957));
#149964=CARTESIAN_POINT('Ctrl Pts',(-2.118148151,4.690053947,6.933682168));
#149965=CARTESIAN_POINT('Ctrl Pts',(-1.739959553,4.624398499,7.04921378));
#149966=CARTESIAN_POINT('Ctrl Pts',(-1.351448856,4.559170361,7.122926785));
#149967=CARTESIAN_POINT('',(-1.95477491753716,4.69005394803158,7.24077722740733));
#149968=CARTESIAN_POINT('Origin',(0.0511912506964596,4.6964256407958,-0.185659103279333));
#149969=CARTESIAN_POINT('',(-2.03646151908971,4.690053949938,7.08722970800272));
#149970=CARTESIAN_POINT('Origin',(1.11347563114261E-13,4.75000000000022,
-6.74373751285984E-13));
#149971=CARTESIAN_POINT('Origin',(0.0695854055266315,4.55370521606813,-0.174272083749276));
#149972=CARTESIAN_POINT('Origin',(0.0227099788655557,4.69643082077873,-0.19168659541468));
#149973=CARTESIAN_POINT('Ctrl Pts',(-3.18344177802041,4.559162772,6.79143474775637));
#149974=CARTESIAN_POINT('Ctrl Pts',(-2.81300470640529,4.624819703,6.96507476537178));
#149975=CARTESIAN_POINT('Ctrl Pts',(-2.42587918041204,4.690053947,7.09739372561723));
#149976=CARTESIAN_POINT('Ctrl Pts',(-2.41249009668655,4.6923101318704,7.10197009560121));
#149977=CARTESIAN_POINT('Ctrl Pts',(-2.39910101296107,4.69456631674065,
7.10654646558524));
#149978=CARTESIAN_POINT('Ctrl Pts',(-2.859730162,4.559162772,6.662165068));
#149979=CARTESIAN_POINT('Ctrl Pts',(-2.496344072,4.624819703,6.818148319));
#149980=CARTESIAN_POINT('Ctrl Pts',(-2.118148151,4.690053947,6.933682168));
#149981=CARTESIAN_POINT('Ctrl Pts',(-2.1050679056767,4.6923101318704,6.93767800984849));
#149982=CARTESIAN_POINT('Ctrl Pts',(-2.09198766035339,4.69456631674065,
6.94167385169711));
#149983=CARTESIAN_POINT('',(-2.42524322977434,4.69005394784288,7.09705541788261));
#149984=CARTESIAN_POINT('',(-2.2716956840529,4.69005394666591,7.01536878363051));
#149985=CARTESIAN_POINT('',(-2.95436459941101,4.5993304993972,6.89360064207624));
#149986=CARTESIAN_POINT('Origin',(0.082127310480036,4.55358392275416,-0.172960595508864));
#149987=CARTESIAN_POINT('Ctrl Pts',(-2.85539439212089,4.55994605579451,
6.66402454021117));
#149988=CARTESIAN_POINT('Ctrl Pts',(-2.87190456475552,4.56683176223659,
6.7022156097041));
#149989=CARTESIAN_POINT('Ctrl Pts',(-2.88841473474086,4.57355155123228,
6.74046360281252));
#149990=CARTESIAN_POINT('Ctrl Pts',(-2.92139824828119,4.58666922557382,
6.81697715040149));
#149991=CARTESIAN_POINT('Ctrl Pts',(-2.93789004470618,4.59307444471158,
6.85528551903663));
#149992=CARTESIAN_POINT('Ctrl Pts',(-2.95436459776838,4.59933049937157,
6.89360064259002));
#149993=CARTESIAN_POINT('Origin',(-1.83338587367299E-12,4.78597145199609,
4.7045700668491E-12));
#149994=CARTESIAN_POINT('',(-3.12690323603191,4.74999999914954,6.81707240326556));
#149995=CARTESIAN_POINT('',(-2.9366723912812,4.78575691078144,6.86227951640224));
#149996=CARTESIAN_POINT('Origin',(-1.23048235575978,4.80792820156638,-0.771867751245));
#149997=CARTESIAN_POINT('',(-2.77562551529351,4.75000000043579,6.96748898019576));
#149998=CARTESIAN_POINT('Origin',(0.,4.75,0.));
#149999=CARTESIAN_POINT('Origin',(1.33274604232867,5.02638717842108,0.590692412348867));
#150000=CARTESIAN_POINT('Ctrl Pts',(-3.465626441,4.690053947,6.651273064));
#150001=CARTESIAN_POINT('Ctrl Pts',(-3.102841477,4.624398499,6.840301112));
#150002=CARTESIAN_POINT('Ctrl Pts',(-2.721649282,4.559170361,6.988749902));
#150003=CARTESIAN_POINT('Ctrl Pts',(-3.559163733,4.690053947,6.31623729200001));
#150004=CARTESIAN_POINT('Ctrl Pts',(-3.214652856,4.624398499,6.51036720800001));
#150005=CARTESIAN_POINT('Ctrl Pts',(-2.85107144,4.559170361,6.66587516));
#150006=CARTESIAN_POINT('',(-3.4656264343989,4.69005394803158,6.65127305476895));
#150007=CARTESIAN_POINT('Origin',(0.0899055760333051,4.69642563605647,-0.170313721247756));
#150008=CARTESIAN_POINT('',(-3.51239507107219,4.690053949938,6.48375518662845));
#150009=CARTESIAN_POINT('Origin',(-3.12467066110322E-13,4.75000000000067,
8.85142653617166E-13));
#150010=CARTESIAN_POINT('Origin',(0.105421885409696,4.55370520201922,-0.155238891963012));
#150011=CARTESIAN_POINT('Origin',(0.0633858622240569,4.69643084883136,-0.182322700843673));
#150012=CARTESIAN_POINT('Ctrl Pts',(-4.56897239582895,4.559162772,5.94830889694042));
#150013=CARTESIAN_POINT('Ctrl Pts',(-4.24452340807861,4.624819703,6.19752232791606));
#150014=CARTESIAN_POINT('Ctrl Pts',(-3.89489332647558,4.690053947,6.40996828923204));
#150015=CARTESIAN_POINT('Ctrl Pts',(-3.88280105622734,4.69231013189195,
6.41731592352486));
#150016=CARTESIAN_POINT('Ctrl Pts',(-3.87070878597903,4.69456631678401,
6.42466355781763));
#150017=CARTESIAN_POINT('Ctrl Pts',(-4.225039818,4.559162772,5.891649899));
#150018=CARTESIAN_POINT('Ctrl Pts',(-3.903681281,4.624819703,6.122103616));
#150019=CARTESIAN_POINT('Ctrl Pts',(-3.559163733,4.690053947,6.316237292));
#150020=CARTESIAN_POINT('Ctrl Pts',(-3.54724828431613,4.69231013189195,
6.32295157946552));
#150021=CARTESIAN_POINT('Ctrl Pts',(-3.53533283563221,4.69456631678401,
6.32966586693117));
#150022=CARTESIAN_POINT('',(-3.89419951784842,4.69005394784288,6.409774601533));
#150023=CARTESIAN_POINT('',(-3.72668161723396,4.69005394666591,6.36300593903434));
#150024=CARTESIAN_POINT('',(-4.36721356148467,4.59933049939503,6.09733103136705));
#150025=CARTESIAN_POINT('Origin',(0.117388618729205,4.55358391550433,-0.151261904255742));
#150026=CARTESIAN_POINT('Ctrl Pts',(-4.22120514702725,4.55994605599275,
5.89439796090948));
#150027=CARTESIAN_POINT('Ctrl Pts',(-4.24553927227261,4.56683176247112,
5.9281469455694));
#150028=CARTESIAN_POINT('Ctrl Pts',(-4.2698856310428,4.57355155128922,5.96195152251035));
#150029=CARTESIAN_POINT('Ctrl Pts',(-4.3185461596293,4.58666922564275,6.02958574563612));
#150030=CARTESIAN_POINT('Ctrl Pts',(-4.34288755391428,4.59307444476057,
6.06345323712583));
#150031=CARTESIAN_POINT('Ctrl Pts',(-4.36721356001292,4.59933049938345,
6.09733103232237));
#150032=CARTESIAN_POINT('Origin',(6.50174358796107E-12,4.78597145200196,
-8.92428492216268E-12));
#150033=CARTESIAN_POINT('',(-4.51926703050333,4.74999999914954,5.985501274402));
#150034=CARTESIAN_POINT('',(-4.34320187092104,4.78575691083943,6.07054547816828));
#150035=CARTESIAN_POINT('Origin',(-1.03578489673937,4.80792705939401,-1.01834026732815));
#150036=CARTESIAN_POINT('',(-4.20853710611605,4.75000000032413,6.2079155212003));
#150037=CARTESIAN_POINT('Origin',(0.,4.75,0.));
#150038=CARTESIAN_POINT('Origin',(1.17460506913819,5.02638735993946,0.86338410375381));
#150039=CARTESIAN_POINT('Ctrl Pts',(-4.814429119,4.690053947,5.750762755));
#150040=CARTESIAN_POINT('Ctrl Pts',(-4.500761309,4.624398499,6.013359475));
#150041=CARTESIAN_POINT('Ctrl Pts',(-4.160393277,4.559170361,6.240282668));
#150042=CARTESIAN_POINT('Ctrl Pts',(-4.833756773,4.690053947,5.403452179));
#150043=CARTESIAN_POINT('Ctrl Pts',(-4.539032563,4.624398499,5.667103101));
#150044=CARTESIAN_POINT('Ctrl Pts',(-4.217381091,4.559170361,5.89713462));
#150045=CARTESIAN_POINT('',(-4.8144291105,4.69005394803159,5.75076274725657));
#150046=CARTESIAN_POINT('Origin',(0.124415970663431,4.6964256537254,-0.147004747925249));
#150047=CARTESIAN_POINT('',(-4.82409293229943,4.690053949938,5.57710747885074));
#150048=CARTESIAN_POINT('Origin',(7.6739829768524E-13,4.75000000000111,
-9.20270804005696E-13));
#150049=CARTESIAN_POINT('Origin',(0.136328968154141,4.55370504339895,-0.12894688215776));
#150050=CARTESIAN_POINT('Origin',(0.101098175086282,4.69643090266516,-0.164434388615765));
#150051=CARTESIAN_POINT('Ctrl Pts',(-5.74086294261692,4.559162772,4.82704673403553));
#150052=CARTESIAN_POINT('Ctrl Pts',(-5.47757291236792,4.624819703,5.14018063457475));
#150053=CARTESIAN_POINT('Ctrl Pts',(-5.18178659019463,4.690053947,5.42281985940272));
#150054=CARTESIAN_POINT('Ctrl Pts',(-5.17155655501913,4.69231013182244,
5.43259519042792));
#150055=CARTESIAN_POINT('Ctrl Pts',(-5.1613265198436,4.69456631664473,5.44237052145306));
#150056=CARTESIAN_POINT('Ctrl Pts',(-5.392791307,4.559162772,4.845647729));
#150057=CARTESIAN_POINT('Ctrl Pts',(-5.128486691,4.624819703,5.139796152));
#150058=CARTESIAN_POINT('Ctrl Pts',(-4.833756773,4.690053947,5.403452179));
#150059=CARTESIAN_POINT('Ctrl Pts',(-4.82356327451006,4.69231013182244,
5.41257095910662));
#150060=CARTESIAN_POINT('Ctrl Pts',(-4.81336977602019,4.69456631664474,
5.42168973921324));
#150061=CARTESIAN_POINT('',(-5.18106736531322,4.69005394784288,5.42277984836034));
#150062=CARTESIAN_POINT('',(-5.0074120594976,4.69005394666591,5.4131160078898));
#150063=CARTESIAN_POINT('',(-5.57585647103438,4.59933049939397,5.01595699876924));
#150064=CARTESIAN_POINT('Origin',(0.147161107532244,4.55358393747605,-0.122490540720301));
#150065=CARTESIAN_POINT('Ctrl Pts',(-5.38963704103988,4.55994605602018,
4.84915588374512));
#150066=CARTESIAN_POINT('Ctrl Pts',(-5.42065728195095,4.56683176249916,
4.87688471837224));
#150067=CARTESIAN_POINT('Ctrl Pts',(-5.45170142089153,4.57355155126975,
4.90466521549262));
#150068=CARTESIAN_POINT('Ctrl Pts',(-5.51376365214984,4.58666922565576,
4.96025761304181));
#150069=CARTESIAN_POINT('Ctrl Pts',(-5.54481646773506,4.5930744447807,4.98810062122209));
#150070=CARTESIAN_POINT('Ctrl Pts',(-5.57585646980821,4.59933049939462,
5.0159570001354));
#150071=CARTESIAN_POINT('Origin',(6.74980904502576E-12,4.78597145199218,
-6.06632799549089E-12));
#150072=CARTESIAN_POINT('',(-5.70031492331358,4.74999999914956,4.87405475696322));
#150073=CARTESIAN_POINT('',(-5.54664805908661,4.78575691071307,4.99495947977542));
#150074=CARTESIAN_POINT('Origin',(-0.79265687257552,4.80792843462252,-1.21719416012186));
#150075=CARTESIAN_POINT('',(-5.44466217910404,4.75000000024935,5.15806683250066));
#150076=CARTESIAN_POINT('Origin',(0.,4.75,0.));
#150077=CARTESIAN_POINT('Origin',(0.961543110245088,5.02638714566244,1.09570289596845));
#150078=CARTESIAN_POINT('Ctrl Pts',(-5.938114442,4.690053947,4.58135317));
#150079=CARTESIAN_POINT('Ctrl Pts',(-5.688230544,4.624398499,4.905239832));
#150080=CARTESIAN_POINT('Ctrl Pts',(-5.404601906,4.559170361,5.200026753));
#150081=CARTESIAN_POINT('Ctrl Pts',(-5.88232872,4.690053947,4.238007649));
#150082=CARTESIAN_POINT('Ctrl Pts',(-5.651172152,4.624398499,4.55885155200001));
#150083=CARTESIAN_POINT('Ctrl Pts',(-5.38649069,4.559170361,4.85265062));
#150084=CARTESIAN_POINT('',(-5.93811443220641,4.69005394803172,4.58135316459078));
#150085=CARTESIAN_POINT('Origin',(0.153108846385023,4.69642566755726,-0.116822071375633));
#150086=CARTESIAN_POINT('',(-5.9102215701673,4.690053949938,4.40968042401888));
#150087=CARTESIAN_POINT('Origin',(7.66314095512755E-13,4.75000000000111,
-5.6248408708548E-13));
#150088=CARTESIAN_POINT('Origin',(0.1608614299865,4.55370522017207,-0.0966255048229053));
#150089=CARTESIAN_POINT('Origin',(0.134082974767383,4.69643082048456,-0.138856792678627));
#150090=CARTESIAN_POINT('Ctrl Pts',(-6.64431711850405,4.559162772,3.48007722957719));
#150091=CARTESIAN_POINT('Ctrl Pts',(-6.45449719571892,4.624819703,3.84248980807567));
#150092=CARTESIAN_POINT('Ctrl Pts',(-6.22638527105153,4.690053947,4.18210640002668));
#150093=CARTESIAN_POINT('Ctrl Pts',(-6.21849581514646,4.69231013195081,
4.19385234505228));
#150094=CARTESIAN_POINT('Ctrl Pts',(-6.21060635924137,4.69456631690173,
4.20559829007785));
#150095=CARTESIAN_POINT('Ctrl Pts',(-6.308381869,4.559162772,3.573068457));
#150096=CARTESIAN_POINT('Ctrl Pts',(-6.113489763,4.624819703,3.917157533));
#150097=CARTESIAN_POINT('Ctrl Pts',(-5.88232872,4.690053947,4.238007649));
#150098=CARTESIAN_POINT('Ctrl Pts',(-5.87433380759733,4.69231013195081,
4.24910453859052));
#150099=CARTESIAN_POINT('Ctrl Pts',(-5.86633889519477,4.69456631690174,
4.2602014281811));
#150100=CARTESIAN_POINT('',(-6.22567426174319,4.69005394784375,4.18222193495617));
#150101=CARTESIAN_POINT('',(-6.05400147933149,4.69005394666591,4.21011478918028));
#150102=CARTESIAN_POINT('',(-6.52377852944664,4.59933049942132,3.70004239165948));
#150103=CARTESIAN_POINT('Origin',(0.170052081414587,4.55358395657544,-0.0879913042010755));
#150104=CARTESIAN_POINT('Ctrl Pts',(-6.30605549606936,4.559946055829,3.57717266655216));
#150105=CARTESIAN_POINT('Ctrl Pts',(-6.34231138060885,4.56683176227916,
3.59758478132714));
#150106=CARTESIAN_POINT('Ctrl Pts',(-6.37860171146201,4.57355155122711,
3.61804221409297));
#150107=CARTESIAN_POINT('Ctrl Pts',(-6.45116368431535,4.58666922560421,
3.65899334696384));
#150108=CARTESIAN_POINT('Ctrl Pts',(-6.48747592626896,4.59307444477225,
3.67950996376723));
#150109=CARTESIAN_POINT('Ctrl Pts',(-6.52377852856624,4.59933049942196,
3.70004239321589));
#150110=CARTESIAN_POINT('Origin',(-2.42731182376055E-12,4.78597145201565,
1.54542177666084E-12));
#150111=CARTESIAN_POINT('',(-6.61482242500904,4.74999999914956,3.53470285698283));
#150112=CARTESIAN_POINT('',(-6.49073914775451,4.78575691081326,3.6858147281543));
#150113=CARTESIAN_POINT('Origin',(-0.512463312253307,4.80792746182712,-1.35913516485433));
#150114=CARTESIAN_POINT('',(-6.42620090124917,4.75000000041766,3.86703266952255));
#150115=CARTESIAN_POINT('Origin',(0.,4.75,0.));
#150116=CARTESIAN_POINT('Origin',(0.703517659165372,5.02638719619019,1.27678982373001));
#150117=CARTESIAN_POINT('Ctrl Pts',(-6.784140134,4.690053947,3.197724603));
#150118=CARTESIAN_POINT('Ctrl Pts',(-6.609724441,4.624398499,3.567756627));
#150119=CARTESIAN_POINT('Ctrl Pts',(-6.396097357,4.559170361,3.916623367));
#150120=CARTESIAN_POINT('Ctrl Pts',(-6.655849513,4.690053947,2.874398591));
#150121=CARTESIAN_POINT('Ctrl Pts',(-6.499069213,4.624398499,3.237433171));
#150122=CARTESIAN_POINT('Ctrl Pts',(-6.303733971,4.559170361,3.581262071));
#150123=CARTESIAN_POINT('',(-6.78414012329034,4.69005394803158,3.19772459975686));
#150124=CARTESIAN_POINT('Origin',(0.174642508548841,4.69642565886706,-0.0811769417586056));
#150125=CARTESIAN_POINT('',(-6.71999481604169,4.690053949938,3.03606161350816));
#150126=CARTESIAN_POINT('Origin',(-1.83880688453542E-13,4.75,9.34582272682505E-14));
#150127=CARTESIAN_POINT('Origin',(0.177872206404633,4.55370521646147,-0.0597860011261758));
#150128=CARTESIAN_POINT('Origin',(0.160798419335299,4.69643083574111,-0.106786606827317));
#150129=CARTESIAN_POINT('Ctrl Pts',(-7.23709041014682,4.559162772,1.97038318208332));
#150130=CARTESIAN_POINT('Ctrl Pts',(-7.12961636368533,4.624819703,2.36512842789401));
#150131=CARTESIAN_POINT('Ctrl Pts',(-6.9798450978861,4.690053947,2.74584229452194));
#150132=CARTESIAN_POINT('Ctrl Pts',(-6.97466512414919,4.69231013191546,
2.7590096255176));
#150133=CARTESIAN_POINT('Ctrl Pts',(-6.96948515041213,4.69456631683104,
2.77217695651325));
#150134=CARTESIAN_POINT('Ctrl Pts',(-6.928999505,4.559162772,2.133416475));
#150135=CARTESIAN_POINT('Ctrl Pts',(-6.81263284900001,4.624819703,2.511356981));
#150136=CARTESIAN_POINT('Ctrl Pts',(-6.655849513,4.690053947,2.874398591));
#150137=CARTESIAN_POINT('Ctrl Pts',(-6.65042702051765,4.69231013191547,
2.88695471112877));
#150138=CARTESIAN_POINT('Ctrl Pts',(-6.64500452803529,4.69456631683105,
2.89951083125753));
#150139=CARTESIAN_POINT('',(-6.97917554816538,4.69005394784373,2.74610797431514));
#150140=CARTESIAN_POINT('',(-6.81751251872002,4.69005394666591,2.81025328239219));
#150141=CARTESIAN_POINT('',(-7.16665595452082,4.59933049939104,2.21111791413529));
#150142=CARTESIAN_POINT('Origin',(0.184991967529409,4.55358391946441,-0.0493779535858213));
#150143=CARTESIAN_POINT('Ctrl Pts',(-6.92760980580543,4.55994605578795,
2.13792483126066));
#150144=CARTESIAN_POINT('Ctrl Pts',(-6.96740604917396,4.56683176223428,
2.15006577864964));
#150145=CARTESIAN_POINT('Ctrl Pts',(-7.00724567573898,4.57355155121141,
2.16224357964001));
#150146=CARTESIAN_POINT('Ctrl Pts',(-7.08691447293298,4.58666922557449,
2.18663861849105));
#150147=CARTESIAN_POINT('Ctrl Pts',(-7.12678822097081,4.59307444474121,
2.19886950955597));
#150148=CARTESIAN_POINT('Ctrl Pts',(-7.16665595398282,4.5993304993895,2.21111791583575));
#150149=CARTESIAN_POINT('Origin',(-8.44376651931711E-12,4.78597145200978,
2.51209643364891E-12));
#150150=CARTESIAN_POINT('',(-7.2200281815243,4.74999999914955,2.03007218087754));
#150151=CARTESIAN_POINT('',(-7.13133048793648,4.78575691086606,2.20432537650669));
#150152=CARTESIAN_POINT('Origin',(-0.208307341171341,4.80792652016166,-1.43752411711541));
#150153=CARTESIAN_POINT('',(-7.10725761039956,4.75000000036324,2.39518035872432));
#150154=CARTESIAN_POINT('Origin',(0.,4.75,0.));
#150155=CARTESIAN_POINT('Origin',(0.412597202993568,5.02638727525261,1.39817477437911));
#150156=CARTESIAN_POINT('Ctrl Pts',(-7.31294697400001,4.690053947,1.664573988));
#150157=CARTESIAN_POINT('Ctrl Pts',(-7.222154969,4.624398499,2.063449087));
#150158=CARTESIAN_POINT('Ctrl Pts',(-7.088518405,4.559170361,2.450083024));
#150159=CARTESIAN_POINT('Ctrl Pts',(-7.118150181,4.690053947,1.376385849));
#150160=CARTESIAN_POINT('Ctrl Pts',(-7.04307702,4.624398499,1.764636013));
#150161=CARTESIAN_POINT('Ctrl Pts',(-6.926221658,4.559170361,2.142417687));
#150162=CARTESIAN_POINT('',(-7.31294696254952,4.69005394803158,1.66457398698021));
#150163=CARTESIAN_POINT('Origin',(0.188010372622518,4.69642563634723,-0.0417361779614356));
#150164=CARTESIAN_POINT('',(-7.21554857376483,4.690053949938,1.52047993622552));
#150165=CARTESIAN_POINT('Origin',(-1.26721549920106E-12,4.749999999998,
4.4202922572234E-13));
#150166=CARTESIAN_POINT('Origin',(0.186565874649461,4.55370510921501,-0.0201509532732519));
#150167=CARTESIAN_POINT('Origin',(0.179994575064681,4.6964308930497,-0.0697229056221557));
#150168=CARTESIAN_POINT('Ctrl Pts',(-7.49146539826354,4.559162772,0.368556206873501));
#150169=CARTESIAN_POINT('Ctrl Pts',(-7.47136259381077,4.624819703,0.777176271114208));
#150170=CARTESIAN_POINT('Ctrl Pts',(-7.40693512428512,4.690053947,1.18118565370734));
#150171=CARTESIAN_POINT('Ctrl Pts',(-7.40470684240947,4.69231013189519,
1.19515868091854));
#150172=CARTESIAN_POINT('Ctrl Pts',(-7.40247856053368,4.69456631679024,
1.20913170812974));
#150173=CARTESIAN_POINT('Ctrl Pts',(-7.225624826,4.559162772,0.594008309));
#150174=CARTESIAN_POINT('Ctrl Pts',(-7.193224795,4.624819703,0.988128168));
#150175=CARTESIAN_POINT('Ctrl Pts',(-7.118150181,4.690053947,1.376385849));
#150176=CARTESIAN_POINT('Ctrl Pts',(-7.11555365807383,4.69231013189516,
1.38981408946994));
#150177=CARTESIAN_POINT('Ctrl Pts',(-7.11295713514763,4.69456631679043,
1.40324232993988));
#150178=CARTESIAN_POINT('',(-7.40633834158946,4.69005394784375,1.18158905541658));
#150179=CARTESIAN_POINT('',(-7.26224424964502,4.69005394666591,1.27898745451562));
#150180=CARTESIAN_POINT('',(-7.4744285120745,4.59933049941584,0.618804020612643));
#150181=CARTESIAN_POINT('Origin',(0.191281838050076,4.5535839226781,-0.00845573802668184));
#150182=CARTESIAN_POINT('Ctrl Pts',(-7.22523678067821,4.55994605584178,
0.598710006831215));
#150183=CARTESIAN_POINT('Ctrl Pts',(-7.26671255482508,4.56683176228833,
0.602012089829403));
#150184=CARTESIAN_POINT('Ctrl Pts',(-7.3082386201527,4.57355155124429,0.605340838621054));
#150185=CARTESIAN_POINT('Ctrl Pts',(-7.39128901723494,4.5866692255987,0.612039098694847));
#150186=CARTESIAN_POINT('Ctrl Pts',(-7.4328598190213,4.59307444474485,0.615412361133979));
#150187=CARTESIAN_POINT('Ctrl Pts',(-7.47442851183252,4.5993304994014,0.618804022328887));
#150188=CARTESIAN_POINT('Origin',(1.75944328550948E-12,4.78597145199609,
-4.27175655959289E-14));
#150189=CARTESIAN_POINT('',(-7.48763344518716,4.74999999914954,0.430517586105534));
#150190=CARTESIAN_POINT('',(-7.43846874086193,4.78575691070391,0.619764219138516));
#150191=CARTESIAN_POINT('Origin',(0.105587353985421,4.80792502932653,-1.44869507804596));
#150192=CARTESIAN_POINT('',(-7.45598685320312,4.75000000025783,0.81133207620068));
#150193=CARTESIAN_POINT('Origin',(0.,4.75,0.));
#150194=CARTESIAN_POINT('Origin',(0.102386161494812,5.02638459270935,1.45418205555291));
#150195=CARTESIAN_POINT('Ctrl Pts',(-7.49980854,4.690053947,0.053589743));
#150196=CARTESIAN_POINT('Ctrl Pts',(-7.496885558,4.624398499,0.462656961));
#150197=CARTESIAN_POINT('Ctrl Pts',(-7.44948821,4.559170361,0.868979523));
#150198=CARTESIAN_POINT('Ctrl Pts',(-7.247614057,4.690053947,-0.185985165));
#150199=CARTESIAN_POINT('Ctrl Pts',(-7.257758374,4.624398499,0.209326436));
#150200=CARTESIAN_POINT('Ctrl Pts',(-7.224846918,4.559170361,0.603396233));
#150201=CARTESIAN_POINT('',(-7.49980852884078,4.69005394803158,0.0535897445321675));
#150202=CARTESIAN_POINT('Origin',(0.192586677601929,4.6964256536905,-0.000343718717236777));
#150203=CARTESIAN_POINT('',(-7.37371129866262,4.690053949938,-0.0661976928859446));
#150204=CARTESIAN_POINT('Origin',(8.89045781438114E-13,4.75000000000067,
-3.97631146759059E-14));
#150205=CARTESIAN_POINT('Origin',(0.186535920086122,4.55370495027973,0.0204263384372728));
#150206=CARTESIAN_POINT('Origin',(0.190775278630512,4.69643086004083,-0.0293994050625012));
#150207=CARTESIAN_POINT('Ctrl Pts',(-7.39554779059847,4.559162772,-1.25050404738331));
#150208=CARTESIAN_POINT('Ctrl Pts',(-7.46375621384794,4.624819703,-0.847115783895782));
#150209=CARTESIAN_POINT('Ctrl Pts',(-7.48768509773944,4.690053947,-0.438701914462572));
#150210=CARTESIAN_POINT('Ctrl Pts',(-7.48851269966669,4.692310131881,-0.424576554208365));
#150211=CARTESIAN_POINT('Ctrl Pts',(-7.48934030159381,4.69456631676211,
-0.410451193954152));
#150212=CARTESIAN_POINT('Ctrl Pts',(-7.184387961,4.559162772,-0.973175025));
#150213=CARTESIAN_POINT('Ctrl Pts',(-7.237469544,4.624819703,-0.581304421));
#150214=CARTESIAN_POINT('Ctrl Pts',(-7.247614057,4.690053947,-0.185985165));
#150215=CARTESIAN_POINT('Ctrl Pts',(-7.24796491408752,4.692310131881,-0.172312693704705));
#150216=CARTESIAN_POINT('Ctrl Pts',(-7.24831577117507,4.6945663167621,-0.158640222409418));
#150217=CARTESIAN_POINT('',(-7.4871889869311,4.69005394784374,-0.438179653401754));
#150218=CARTESIAN_POINT('',(-7.36740151108662,4.69005394666591,-0.312082404455189));
#150219=CARTESIAN_POINT('',(-7.43270509999558,4.59933049944584,-1.00244446088511));
#150220=CARTESIAN_POINT('Origin',(0.188627548303029,4.55358393625757,0.0328618978331841));
#150221=CARTESIAN_POINT('Ctrl Pts',(-7.18501971321785,4.55994605574127,
-0.96849983165087));
#150222=CARTESIAN_POINT('Ctrl Pts',(-7.22623565686466,4.56683176218549,
-0.974191014923011));
#150223=CARTESIAN_POINT('Ctrl Pts',(-7.26750644887087,4.57355155122374,
-0.979866967011814));
#150224=CARTESIAN_POINT('Ctrl Pts',(-7.35005510186625,4.58666922560854,
-0.991178688909446));
#150225=CARTESIAN_POINT('Ctrl Pts',(-7.39137915337171,4.5930744447878,-0.996820785018313));
#150226=CARTESIAN_POINT('Ctrl Pts',(-7.43270510023496,4.59933049944648,
-1.00244445912524));
#150227=CARTESIAN_POINT('Origin',(-1.53384249745869E-11,4.78597145198239,
-2.16975959768662E-12));
#150228=CARTESIAN_POINT('',(-7.40512529081742,4.74999999776862,-1.18916754046224));
#150229=CARTESIAN_POINT('',(-7.39779246229846,4.78575691078591,-0.993776423367131));
#150230=CARTESIAN_POINT('Origin',(0.414536447211268,4.80792594780388,-1.39212700636851));
#150231=CARTESIAN_POINT('',(-7.45608243946475,4.74999999872292,-0.810453186416921));
#150232=CARTESIAN_POINT('Origin',(0.,4.74999999751669,0.));
#150233=CARTESIAN_POINT('Origin',(-0.212620297068353,5.02638752233421,1.44219252886256));
#150234=CARTESIAN_POINT('Ctrl Pts',(-7.335987395,4.690053947,-1.559900299));
#150235=CARTESIAN_POINT('Ctrl Pts',(-7.42107011,4.624398499,-1.15976849));
#150236=CARTESIAN_POINT('Ctrl Pts',(-7.462128226,4.559170361,-0.752756495));
#150237=CARTESIAN_POINT('Ctrl Pts',(-7.038187555,4.690053947,-1.73965972));
#150238=CARTESIAN_POINT('Ctrl Pts',(-7.133075012,4.624398499,-1.355771012));
#150239=CARTESIAN_POINT('Ctrl Pts',(-7.185646366,4.559170361,-0.963839358));
#150240=CARTESIAN_POINT('',(-7.33598738428273,4.69005394803158,-1.55990029511267));
#150241=CARTESIAN_POINT('Origin',(0.188158183055879,4.69642564641174,0.0410647845106853));
#150242=CARTESIAN_POINT('',(-7.18708747905281,4.690053949938,-1.6497799918444));
#150243=CARTESIAN_POINT('Origin',(1.421172207694E-12,4.75090401630852,1.44659674863878E-13));
#150244=CARTESIAN_POINT('Origin',(0.17778370261965,4.55370429861311,0.0600485860377439));
#150245=CARTESIAN_POINT('Origin',(0.192635712568098,4.69643090866594,0.0122990365265791));
#150246=CARTESIAN_POINT('Ctrl Pts',(-6.95382258707868,4.559162772,-2.81109212170412));
#150247=CARTESIAN_POINT('Ctrl Pts',(-7.10715288829031,4.624819703,-2.43179764594953));
#150248=CARTESIAN_POINT('Ctrl Pts',(-7.21831923758139,4.690053947,-2.03807626903604));
#150249=CARTESIAN_POINT('Ctrl Pts',(-7.22216402555688,4.69231013188439,
-2.02445906180291));
#150250=CARTESIAN_POINT('Ctrl Pts',(-7.2260088135324,4.69456631676863,-2.01084185456972));
#150251=CARTESIAN_POINT('Ctrl Pts',(-6.807217099,4.559162772,-2.494853776));
#150252=CARTESIAN_POINT('Ctrl Pts',(-6.94329826,4.624819703,-2.12355586));
#150253=CARTESIAN_POINT('Ctrl Pts',(-7.038187555,4.690053947,-1.73965972));
#150254=CARTESIAN_POINT('Ctrl Pts',(-7.04146938644222,4.69231013188436,
-1.72638232740484));
#150255=CARTESIAN_POINT('Ctrl Pts',(-7.04475121788429,4.69456631676882,
-1.71310493480973));
#150256=CARTESIAN_POINT('',(-7.21794699633072,4.69005394784288,-2.03745956668756));
#150257=CARTESIAN_POINT('',(-7.12806726602417,4.69005394666591,-1.88855963752162));
#150258=CARTESIAN_POINT('',(-7.04343665786128,4.59933049941141,-2.57681975364456));
#150259=CARTESIAN_POINT('Origin',(0.177153211421694,4.55358396568391,0.072642954591845));
#150260=CARTESIAN_POINT('Ctrl Pts',(-6.80883911044133,4.55994605585476,
-2.49042369485092));
#150261=CARTESIAN_POINT('Ctrl Pts',(-6.84786801208649,4.56683176231117,
-2.50484203097927));
#150262=CARTESIAN_POINT('Ctrl Pts',(-6.88695375350926,4.57355155126602,
-2.51925728258282));
#150263=CARTESIAN_POINT('Ctrl Pts',(-6.9651407789688,4.5866692256309,-2.5480500628686));
#150264=CARTESIAN_POINT('Ctrl Pts',(-7.00428581311489,4.59307444478289,
-2.5624436993453));
#150265=CARTESIAN_POINT('Ctrl Pts',(-7.04343665848406,4.59933049941205,
-2.57681975194824));
#150266=CARTESIAN_POINT('Origin',(-6.99180296992452E-12,4.78597145200196,
-2.51990268929081E-12));
#150267=CARTESIAN_POINT('',(-6.97636170828729,4.74999999998991,-2.75324850177502));
#150268=CARTESIAN_POINT('',(-7.01120363040642,4.78575691087914,-2.56084918463864));
#150269=CARTESIAN_POINT('Origin',(0.704118751076819,4.80792822099414,-1.27046583472849));
#150270=CARTESIAN_POINT('',(-7.10753989332788,4.75000000059599,-2.39434257212809));
#150271=CARTESIAN_POINT('Origin',(0.,4.750000000594,0.));
#150272=CARTESIAN_POINT('Origin',(-0.517673241365713,5.02638728507947,1.3627706118265));
#150273=CARTESIAN_POINT('Ctrl Pts',(-6.829143632,4.690053947,-3.100451136));
#150274=CARTESIAN_POINT('Ctrl Pts',(-6.998253672,4.624398499,-2.727964456));
#150275=CARTESIAN_POINT('Ctrl Pts',(-7.125847419,4.559170361,-2.339294456));
#150276=CARTESIAN_POINT('Ctrl Pts',(-6.499663225,4.690053947,-3.211989719));
#150277=CARTESIAN_POINT('Ctrl Pts',(-6.674856991,4.624398499,-2.857474115));
#150278=CARTESIAN_POINT('Ctrl Pts',(-6.810452976,4.559170361,-2.486006892));
#150279=CARTESIAN_POINT('',(-6.82914362262778,4.69005394803157,-3.10045112994256));
#150280=CARTESIAN_POINT('Origin',(0.174931139540757,4.69642566604463,0.0805530469035581));
#150281=CARTESIAN_POINT('',(-6.66440343625348,4.690053949938,-3.15622041112841));
#150282=CARTESIAN_POINT('Origin',(-4.90926743701436E-13,4.74999999999889,
-1.89735380184963E-13));
#150283=CARTESIAN_POINT('Origin',(0.160718645717512,4.55370518580565,0.0968628134508132));
#150284=CARTESIAN_POINT('Origin',(0.185486980252586,4.69643091730784,0.0534221683155373));
#150285=CARTESIAN_POINT('Ctrl Pts',(-6.18694436873807,4.559162772,-4.24023665220644));
#150286=CARTESIAN_POINT('Ctrl Pts',(-6.41822699308657,4.624819703,-3.90277135391354));
#150287=CARTESIAN_POINT('Ctrl Pts',(-6.61143279189146,4.690053947,-3.54215244295726));
#150288=CARTESIAN_POINT('Ctrl Pts',(-6.61811498807727,4.6923101319548,-3.52968011383345));
#150289=CARTESIAN_POINT('Ctrl Pts',(-6.62479718426306,4.69456631690948,
-3.51720778470964));
#150290=CARTESIAN_POINT('Ctrl Pts',(-6.111748332,4.559162772,-3.899875938));
#150291=CARTESIAN_POINT('Ctrl Pts',(-6.324466068,4.624819703,-3.566512188));
#150292=CARTESIAN_POINT('Ctrl Pts',(-6.499663225,4.690053947,-3.211989719));
#150293=CARTESIAN_POINT('Ctrl Pts',(-6.50572257612459,4.6923101319548,-3.19972824080011));
#150294=CARTESIAN_POINT('Ctrl Pts',(-6.51178192724931,4.69456631690947,
-3.1874667626003));
#150295=CARTESIAN_POINT('',(-6.61120182620016,4.69005394784288,-3.54147013788702));
#150296=CARTESIAN_POINT('',(-6.55543251743721,4.69005394666591,-3.37672992068055));
#150297=CARTESIAN_POINT('',(-6.324824946348,4.59933049939799,-4.03070581890792));
#150298=CARTESIAN_POINT('Origin',(0.15739515689109,4.55358394795306,0.109027173086295));
#150299=CARTESIAN_POINT('Ctrl Pts',(-6.11428475835871,4.5599460559347,-3.89589811327206));
#150300=CARTESIAN_POINT('Ctrl Pts',(-6.14930167003365,4.56683176238811,
-3.91836941721311));
#150301=CARTESIAN_POINT('Ctrl Pts',(-6.18437475511205,4.57355155124519,
-3.94084992717363));
#150302=CARTESIAN_POINT('Ctrl Pts',(-6.25454421474505,4.58666922561086,
-3.98577744783568));
#150303=CARTESIAN_POINT('Ctrl Pts',(-6.28967985332806,4.59307444476164,
-4.00824959438245));
#150304=CARTESIAN_POINT('Ctrl Pts',(-6.32482494730784,4.5993304993985,-4.0307058174037));
#150305=CARTESIAN_POINT('Origin',(6.25367813089639E-12,4.78597145201565,
3.54599162533109E-12));
#150306=CARTESIAN_POINT('',(-6.22139120646213,4.74999999914955,-4.18859062908611));
#150307=CARTESIAN_POINT('',(-6.29677870893683,4.7857569106907,-4.00817948537505));
#150308=CARTESIAN_POINT('Origin',(0.960770280213318,4.80792507653282,-1.08939736573568));
#150309=CARTESIAN_POINT('',(-6.42665668426536,4.75000000025304,-3.86627515258916));
#150310=CARTESIAN_POINT('Origin',(0.,4.75,0.));
#150311=CARTESIAN_POINT('Origin',(-0.79852459252602,5.02638720279362,1.21962634968895));
#150312=CARTESIAN_POINT('Ctrl Pts',(-6.002976704,4.690053947,-4.496028325));
#150313=CARTESIAN_POINT('Ctrl Pts',(-6.24820667,4.624398499,-4.168603835));
#150314=CARTESIAN_POINT('Ctrl Pts',(-6.456369908,4.559170361,-3.816449609));
#150315=CARTESIAN_POINT('Ctrl Pts',(-5.657221867,4.690053947,-4.534130649));
#150316=CARTESIAN_POINT('Ctrl Pts',(-5.904530075,4.624398499,-4.225564904));
#150317=CARTESIAN_POINT('Ctrl Pts',(-6.116810374,4.559170361,-3.891931506));
#150318=CARTESIAN_POINT('',(-6.00297669575905,4.69005394803158,-4.496028316913));
#150319=CARTESIAN_POINT('Origin',(0.153525257493488,4.69642563941649,0.11627507186809));
#150320=CARTESIAN_POINT('',(-5.83009929659162,4.690053949938,-4.51507947267794));
#150321=CARTESIAN_POINT('Origin',(-5.55111512312578E-14,4.75,5.42101086242752E-15));
#150322=CARTESIAN_POINT('Origin',(0.136138464028436,4.55370498751413,0.129147991651934));
#150323=CARTESIAN_POINT('Origin',(0.169666505435107,4.69643086886799,0.0920475538402357));
#150324=CARTESIAN_POINT('Ctrl Pts',(-5.13077150802372,4.559162772,-5.47111243083583));
#150325=CARTESIAN_POINT('Ctrl Pts',(-5.42919193654034,4.624819703,-5.19125581034408));
#150326=CARTESIAN_POINT('Ctrl Pts',(-5.69540309763819,4.690053947,-4.88060150445534));
#150327=CARTESIAN_POINT('Ctrl Pts',(-5.70461024965117,4.69231013189656,
-4.86985724637842));
#150328=CARTESIAN_POINT('Ctrl Pts',(-5.71381740166407,4.69456631679295,
-4.85911298830139));
#150329=CARTESIAN_POINT('Ctrl Pts',(-5.130501005,4.559162772,-5.122544235));
#150330=CARTESIAN_POINT('Ctrl Pts',(-5.40990887,4.624819703,-4.842702369));
#150331=CARTESIAN_POINT('Ctrl Pts',(-5.657221867,4.690053947,-4.534130649));
#150332=CARTESIAN_POINT('Ctrl Pts',(-5.66577540904071,4.69231013189655,
-4.52345841902579));
#150333=CARTESIAN_POINT('Ctrl Pts',(-5.67432895108152,4.69456631679296,
-4.51278618905156));
#150334=CARTESIAN_POINT('',(-5.6953242072177,4.69005394784288,-4.87988550052245));
#150335=CARTESIAN_POINT('',(-5.67627303080642,4.69005394666591,-4.70700806542456));
#150336=CARTESIAN_POINT('',(-5.3104714497277,4.5993304994063,-5.29612055988535));
#150337=CARTESIAN_POINT('Origin',(0.130277873032469,4.55358394138756,0.140313616842009));
#150338=CARTESIAN_POINT('Ctrl Pts',(-5.13383324548519,4.55994605585018,
-5.11920466612713));
#150339=CARTESIAN_POINT('Ctrl Pts',(-5.16320081518432,4.56683176231821,
-5.14867820437159));
#150340=CARTESIAN_POINT('Ctrl Pts',(-5.19262126617189,4.57355155123034,
-5.17817280927312));
#150341=CARTESIAN_POINT('Ctrl Pts',(-5.25149211409,4.58666922560857,-5.23713430919394));
#150342=CARTESIAN_POINT('Ctrl Pts',(-5.28097545383409,4.59307444476671,
-5.26663419322239));
#150343=CARTESIAN_POINT('Ctrl Pts',(-5.31047145099105,4.59933049940695,
-5.29612055862145));
#150344=CARTESIAN_POINT('Origin',(6.03206720684035E-12,4.78597145201174,
5.96918348083619E-12));
#150345=CARTESIAN_POINT('',(-5.17551536425395,4.74999999914956,-5.42807891551251));
#150346=CARTESIAN_POINT('',(-5.2879234136685,4.78575691078485,-5.26809176705119));
#150347=CARTESIAN_POINT('Origin',(1.17249541205182,4.80792850072533,-0.857391987530597));
#150348=CARTESIAN_POINT('',(-5.4452701498066,4.75000000047412,-5.15742500529851));
#150349=CARTESIAN_POINT('Origin',(0.,4.75,0.));
#150350=CARTESIAN_POINT('Origin',(-1.04203959986824,5.02638720628501,1.01945233902109));
#150351=CARTESIAN_POINT('Ctrl Pts',(-4.896117256,4.690053947,-5.681376225));
#150352=CARTESIAN_POINT('Ctrl Pts',(-5.206000469,4.624398499,-5.414323933));
#150353=CARTESIAN_POINT('Ctrl Pts',(-5.484999715,4.559170361,-5.115151819));
#150354=CARTESIAN_POINT('Ctrl Pts',(-4.550255102,4.690053947,-5.644260669));
#150355=CARTESIAN_POINT('Ctrl Pts',(-4.858113896,4.624398499,-5.396072974));
#150356=CARTESIAN_POINT('Ctrl Pts',(-5.13715251700001,4.559170361,-5.115873729));
#150357=CARTESIAN_POINT('',(-4.89611725000693,4.69005394803158,-5.68137621554656));
#150358=CARTESIAN_POINT('Origin',(0.124939912224816,4.69642566560811,0.14655971460778));
#150359=CARTESIAN_POINT('',(-4.72318619291109,4.690053949938,-5.66281843539718));
#150360=CARTESIAN_POINT('Origin',(-1.17354043149831E-12,4.74999999999845,
-1.13190706807487E-12));
#150361=CARTESIAN_POINT('Origin',(0.105192656758101,4.5537052143291,0.155394314114667));
#150362=CARTESIAN_POINT('Origin',(0.145911959404404,4.696430882499,0.126368526012341));
#150363=CARTESIAN_POINT('Ctrl Pts',(-3.83468947316923,4.559162772,-6.44616507155078));
#150364=CARTESIAN_POINT('Ctrl Pts',(-4.18629389862629,4.624819703,-6.23700291528905));
#150365=CARTESIAN_POINT('Ctrl Pts',(-4.51306268384797,4.690053947,-5.99083906471441));
#150366=CARTESIAN_POINT('Ctrl Pts',(-4.52436427590561,4.69231013194548,
-5.98232526674977));
#150367=CARTESIAN_POINT('Ctrl Pts',(-4.53566586796319,4.69456631689107,
-5.97381146878521));
#150368=CARTESIAN_POINT('Ctrl Pts',(-3.909357153,4.559162772,-6.105688057));
#150369=CARTESIAN_POINT('Ctrl Pts',(-4.242390347,4.624819703,-5.89245317));
#150370=CARTESIAN_POINT('Ctrl Pts',(-4.550255102,4.690053947,-5.644260669));
#150371=CARTESIAN_POINT('Ctrl Pts',(-4.56090288118604,4.69231013194548,
-5.63567670833756));
#150372=CARTESIAN_POINT('Ctrl Pts',(-4.57155066037219,4.69456631689108,
-5.62709274767499));
#150373=CARTESIAN_POINT('',(-4.5131395575211,4.69005394784288,-5.99012284143654));
#150374=CARTESIAN_POINT('',(-4.53169732561459,4.69005394666591,-5.8171917447422));
#150375=CARTESIAN_POINT('',(-4.04780620967149,4.5993304994234,-6.31389458947704));
#150376=CARTESIAN_POINT('Origin',(0.0970686768313267,4.55358391569743,0.165038936601301));
#150377=CARTESIAN_POINT('Ctrl Pts',(-3.91332939641532,4.55994605596869,
-6.10314289974883));
#150378=CARTESIAN_POINT('Ctrl Pts',(-3.93567442920366,4.5668317624299,-6.13824052216406));
#150379=CARTESIAN_POINT('Ctrl Pts',(-3.95806657822901,4.57355155134733,
-6.17337008676992));
#150380=CARTESIAN_POINT('Ctrl Pts',(-4.00288607861997,4.58666922566913,
-6.24360859117123));
#150381=CARTESIAN_POINT('Ctrl Pts',(-4.02533851102381,4.59307444478845,
-6.27875683055447));
#150382=CARTESIAN_POINT('Ctrl Pts',(-4.04780621107526,4.59933049940983,
-6.31389458846582));
#150383=CARTESIAN_POINT('Origin',(-6.75284481110872E-12,4.78597145199413,
-1.08307460222612E-11));
#150384=CARTESIAN_POINT('',(-3.88763817760581,4.74999999914954,-6.41375626277432));
#150385=CARTESIAN_POINT('',(-4.03181069685682,4.78575691085142,-6.2816739328473));
#150386=CARTESIAN_POINT('Origin',(1.32939753871551,4.80792768536083,-0.585294039397131));
#150387=CARTESIAN_POINT('',(-4.20926883649175,4.75000000037377,-6.20741939563398));
#150388=CARTESIAN_POINT('Origin',(0.,4.75,0.));
#150389=CARTESIAN_POINT('Origin',(-1.23682972024279,5.02638723642215,0.771609693634924));
#150390=CARTESIAN_POINT('Ctrl Pts',(-3.560320807,4.690053947,-6.601069288));
#150391=CARTESIAN_POINT('Ctrl Pts',(-3.920367472,4.624398499,-6.406876261));
#150392=CARTESIAN_POINT('Ctrl Pts',(-4.257157031,4.559170361,-6.174675215));
#150393=CARTESIAN_POINT('Ctrl Pts',(-3.230523466,4.690053947,-6.490471334));
#150394=CARTESIAN_POINT('Ctrl Pts',(-3.58453771,4.624398499,-6.314266669));
#150395=CARTESIAN_POINT('Ctrl Pts',(-3.917287119,4.559170361,-6.100603383));
#150396=CARTESIAN_POINT('',(-3.56032080319409,4.69005394803158,-6.60106927749502));
#150397=CARTESIAN_POINT('Origin',(0.0905127851222914,4.69642564207801,0.169991447369243));
#150398=CARTESIAN_POINT('',(-3.39542215258012,4.690053949938,-6.54577030265893));
#150399=CARTESIAN_POINT('Origin',(1.18394877235417E-13,4.75000000000067,
1.196959198424E-13));
#150400=CARTESIAN_POINT('Origin',(0.0693281085175074,4.55370510242446,0.17437459689732));
#150401=CARTESIAN_POINT('Origin',(0.115335243645399,4.69643087673821,0.154781016914751));
#150402=CARTESIAN_POINT('Ctrl Pts',(-2.35930162162706,4.559162772,-7.11980219917393));
#150403=CARTESIAN_POINT('Ctrl Pts',(-2.74764941144185,4.624819703,-6.99111469558026));
#150404=CARTESIAN_POINT('Ctrl Pts',(-3.11969647504582,4.690053947,-6.82095164828537));
#150405=CARTESIAN_POINT('Ctrl Pts',(-3.1325640569744,4.69231013193285,-6.81506640642627));
#150406=CARTESIAN_POINT('Ctrl Pts',(-3.14543163890304,4.69456631686582,
-6.80918116456703));
#150407=CARTESIAN_POINT('Ctrl Pts',(-2.505416106,4.559162772,-6.803336691));
#150408=CARTESIAN_POINT('Ctrl Pts',(-2.876502367,4.624819703,-6.66667941000001));
#150409=CARTESIAN_POINT('Ctrl Pts',(-3.230523466,4.690053947,-6.49047133400001));
#150410=CARTESIAN_POINT('Ctrl Pts',(-3.24276760374887,4.69231013193285,
-6.48437701939248));
#150411=CARTESIAN_POINT('Ctrl Pts',(-3.2550117414978,4.69456631686581,-6.47828270478494));
#150412=CARTESIAN_POINT('',(-3.11992551648257,4.69005394784374,-6.82026869691982));
#150413=CARTESIAN_POINT('',(-3.17522449034723,4.6900539466659,-6.6553700036187));
#150414=CARTESIAN_POINT('',(-2.59587005084126,4.59933049942066,-7.03643792557235));
#150415=CARTESIAN_POINT('Origin',(0.0593208058217742,4.55358392054283,0.18204736950036));
#150416=CARTESIAN_POINT('Ctrl Pts',(-2.50984261394196,4.55994605587811,
-6.80170495256708));
#150417=CARTESIAN_POINT('Ctrl Pts',(-2.52412028095697,4.56683176230192,
-6.84078553361449));
#150418=CARTESIAN_POINT('Ctrl Pts',(-2.53843709611326,4.57355155123639,
-6.87990743885963));
#150419=CARTESIAN_POINT('Ctrl Pts',(-2.56710953945787,4.58666922560941,
-6.9581386741797));
#150420=CARTESIAN_POINT('Ctrl Pts',(-2.5814812140756,4.59307444477075,-6.99729177677978));
#150421=CARTESIAN_POINT('Ctrl Pts',(-2.5958700525406,4.5993304994213,-7.03643792494762));
#150422=CARTESIAN_POINT('Origin',(1.46215504981395E-12,4.78597145199609,
3.35495520253914E-12));
#150423=CARTESIAN_POINT('',(-2.41797935133364,4.74999999914954,-7.09953349559792));
#150424=CARTESIAN_POINT('',(-2.5871749920055,4.78575691069861,-7.00153200784835));
#150425=CARTESIAN_POINT('Origin',(1.42413838529096,4.80792638182854,-0.28582768614912));
#150426=CARTESIAN_POINT('',(-2.77644679082714,4.75000000025891,-6.9671617542923));
#150427=CARTESIAN_POINT('Origin',(0.,4.75,0.));
#150428=CARTESIAN_POINT('Origin',(-1.37378626611183,5.02638716985328,0.487689787695301));
#150429=CARTESIAN_POINT('Ctrl Pts',(-2.058047714,4.690053947,-7.212103688));
#150430=CARTESIAN_POINT('Ctrl Pts',(-2.451422449,4.624398499,-7.099850175));
#150431=CARTESIAN_POINT('Ctrl Pts',(-2.830254416,4.559170361,-6.945477661));
#150432=CARTESIAN_POINT('Ctrl Pts',(-1.759736143,4.690053947,-7.033194773));
#150433=CARTESIAN_POINT('Ctrl Pts',(-2.143352525,4.624398499,-6.937212273));
#150434=CARTESIAN_POINT('Ctrl Pts',(-2.514253728,4.559170361,-6.800075602));
#150435=CARTESIAN_POINT('',(-2.05804771252564,4.69005394803173,-7.21210367677717));
#150436=CARTESIAN_POINT('Origin',(0.051853611895134,4.69642561041417,0.185474986327538));
#150437=CARTESIAN_POINT('',(-1.90889194599726,4.690053949938,-7.12264922581068));
#150438=CARTESIAN_POINT('Origin',(1.95806912350882E-13,4.75000000000067,
1.39211558947139E-13));
#150439=CARTESIAN_POINT('Origin',(0.0302218524976797,4.55370498643004,0.185201308694485));
#150440=CARTESIAN_POINT('Origin',(0.0793656699151506,4.696430839033,0.175956526080664));
#150441=CARTESIAN_POINT('Ctrl Pts',(-0.773595447463978,4.559162772,-7.4605252880029));
#150442=CARTESIAN_POINT('Ctrl Pts',(-1.18052789162116,4.624819703,-7.41832972194081));
#150443=CARTESIAN_POINT('Ctrl Pts',(-1.5804567267152,4.690053947,-7.33212411378188));
#150444=CARTESIAN_POINT('Ctrl Pts',(-1.59428862460278,4.6923101319074,-7.32914261541329));
#150445=CARTESIAN_POINT('Ctrl Pts',(-1.60812052249042,4.69456631681494,
-7.32616111704456));
#150446=CARTESIAN_POINT('Ctrl Pts',(-0.984324587,4.559162772,-7.182868863));
#150447=CARTESIAN_POINT('Ctrl Pts',(-1.376112332,4.624819703,-7.12917913000001));
#150448=CARTESIAN_POINT('Ctrl Pts',(-1.759736143,4.690053947,-7.03319477300001));
#150449=CARTESIAN_POINT('Ctrl Pts',(-1.77300411698779,4.69231013190741,
-7.02987506782166));
#150450=CARTESIAN_POINT('Ctrl Pts',(-1.78627209097565,4.69456631681493,
-7.02655536264332));
#150451=CARTESIAN_POINT('',(-1.58082722970849,4.69005394784289,-7.33150636557383));
#150452=CARTESIAN_POINT('',(-1.6702816869935,4.6900539466659,-7.18235055803641));
#150453=CARTESIAN_POINT('',(-1.02255389306326,4.59933049943543,-7.42996524456859));
#150454=CARTESIAN_POINT('Origin',(0.0187991191944201,4.55358393308258,0.190543474815297));
#150455=CARTESIAN_POINT('Ctrl Pts',(-0.988998380749847,4.55994605587036,
-7.18222684255029));
#150456=CARTESIAN_POINT('Ctrl Pts',(-0.994541074017316,4.56683176236791,
-7.22346301788626));
#150457=CARTESIAN_POINT('Ctrl Pts',(-1.00011311666342,4.57355155128146,
-7.26474796650435));
#150458=CARTESIAN_POINT('Ctrl Pts',(-1.01129781094312,4.58666922563949,
-7.34731392651533));
#150459=CARTESIAN_POINT('Ctrl Pts',(-1.0169167240055,4.59307444475724,-7.38864113623438));
#150460=CARTESIAN_POINT('Ctrl Pts',(-1.02255389468507,4.5993304994032,-7.42996524412411));
#150461=CARTESIAN_POINT('Origin',(1.82026702738591E-12,4.78597145200587,
1.19509437068732E-11));
#150462=CARTESIAN_POINT('',(-0.835258513063531,4.75000000340508,-7.45334442874213));
#150463=CARTESIAN_POINT('',(-1.0215658608059,4.78575691075516,-7.39400622716639));
#150464=CARTESIAN_POINT('Origin',(1.45228678331533,4.8079250825528,0.0270015665869461));
#150465=CARTESIAN_POINT('',(-1.21380116044022,4.75000000415435,-7.4011273722088));
#150466=CARTESIAN_POINT('Origin',(0.,4.7500000057058,0.));
#150467=CARTESIAN_POINT('Origin',(-1.44650689480819,5.02638711396738,0.180966637540554));
#150468=CARTESIAN_POINT('Ctrl Pts',(-0.459542598,4.690053947,-7.48590813500001));
#150469=CARTESIAN_POINT('Ctrl Pts',(-0.867851637,4.624398499,-7.460842987));
#150470=CARTESIAN_POINT('Ctrl Pts',(-1.271012251,4.559170361,-7.391517291));
#150471=CARTESIAN_POINT('Ctrl Pts',(-0.206665513,4.690053947,-7.24705384));
#150472=CARTESIAN_POINT('Ctrl Pts',(-0.601946558,4.624398499,-7.235781541));
#150473=CARTESIAN_POINT('Ctrl Pts',(-0.993656627,4.559170361,-7.18158384400001));
#150474=CARTESIAN_POINT('',(-0.459542598855283,4.69005394803158,-7.48590812356305));
#150475=CARTESIAN_POINT('Origin',(0.0107696487616114,4.69642563687689,0.192285589499794));
#150476=CARTESIAN_POINT('',(-0.333104073596248,4.690053949938,-7.36648098668171));
#150477=CARTESIAN_POINT('Origin',(-7.98243849492453E-14,4.75000000000044,
-2.38524477946811E-13));
#150478=CARTESIAN_POINT('Origin',(-0.010297498977334,4.55370514355358,0.187368216690001));
#150479=CARTESIAN_POINT('Origin',(0.039684243872064,4.6964308192229,0.188901957144474));
#150480=CARTESIAN_POINT('Ctrl Pts',(0.848283189457317,4.559162772,-7.45240250625932));
#150481=CARTESIAN_POINT('Ctrl Pts',(0.441793800428909,4.624819703,-7.49867189602281));
#150482=CARTESIAN_POINT('Ctrl Pts',(0.0326834214338154,4.690053947,-7.50045460506005));
#150483=CARTESIAN_POINT('Ctrl Pts',(0.0185339716261254,4.69231013190414,
-7.50051626165285));
#150484=CARTESIAN_POINT('Ctrl Pts',(0.00438452181843482,4.69456631680839,
-7.50057791824562));
#150485=CARTESIAN_POINT('Ctrl Pts',(0.582792857,4.559162772,-7.226538071));
#150486=CARTESIAN_POINT('Ctrl Pts',(0.188623186,4.624819703,-7.25832635800001));
#150487=CARTESIAN_POINT('Ctrl Pts',(-0.206665513,4.690053947,-7.24705384000001));
#150488=CARTESIAN_POINT('Ctrl Pts',(-0.220336927594239,4.69231013190414,
-7.2466639698431));
#150489=CARTESIAN_POINT('Ctrl Pts',(-0.234008342188472,4.69456631680839,
-7.24627409968621));
#150490=CARTESIAN_POINT('',(0.0321887829827294,4.69005394784288,-7.49993094664959));
#150491=CARTESIAN_POINT('',(-0.0872383680465477,4.6900539466659,-7.37349238247579));
#150492=CARTESIAN_POINT('',(0.598575747913816,4.59933049944211,-7.47607564637949));
#150493=CARTESIAN_POINT('Origin',(-0.0226016148045383,4.55358392282057,
0.190129924982587));
#150494=CARTESIAN_POINT('Ctrl Pts',(0.578090317678936,4.5599460558702,-7.22691578740445));
#150495=CARTESIAN_POINT('Ctrl Pts',(0.581541768273302,4.5668317623654,-7.26837939903823));
#150496=CARTESIAN_POINT('Ctrl Pts',(0.584975040463299,4.57355155126758,
-7.30989695284797));
#150497=CARTESIAN_POINT('Ctrl Pts',(0.591801078882446,4.58666922564616,
-7.39293694531079));
#150498=CARTESIAN_POINT('Ctrl Pts',(0.595197661341285,4.59307444478516,
-7.43450584816564));
#150499=CARTESIAN_POINT('Ctrl Pts',(0.598575746204673,4.59933049942523,
-7.47607564640007));
#150500=CARTESIAN_POINT('Origin',(-5.73082163321526E-13,4.7859714520137,
8.00574884163296E-12));
#150501=CARTESIAN_POINT('',(0.786518118240955,4.74999999914956,-7.45864526901614));
#150502=CARTESIAN_POINT('',(0.591810554745355,4.78575691077897,-7.44074493328967));
#150503=CARTESIAN_POINT('Origin',(1.41252907240432,4.807928318978,0.338567896634023));
#150504=CARTESIAN_POINT('',(0.405600429422982,4.7500000004036,-7.48902450137449));
#150505=CARTESIAN_POINT('Origin',(0.,4.75,0.));
#150506=CARTESIAN_POINT('Origin',(-1.45158988728563,5.0263873102246,-0.134224246665127));
#150507=CARTESIAN_POINT('Ctrl Pts',(1.16045022,4.690053947,-7.409679837));
#150508=CARTESIAN_POINT('Ctrl Pts',(0.756298953000001,4.624398499,-7.47297507200001));
#150509=CARTESIAN_POINT('Ctrl Pts',(0.347661035,4.559170361,-7.491937787));
#150510=CARTESIAN_POINT('Ctrl Pts',(1.356068566,4.690053947,-7.122048725));
#150511=CARTESIAN_POINT('Ctrl Pts',(0.967605761,4.624398499,-7.196013706));
#150512=CARTESIAN_POINT('Ctrl Pts',(0.573402753,4.559170361,-7.227289207));
#150513=CARTESIAN_POINT('',(1.16045021669141,4.69005394803158,-7.40967982615787));
#150514=CARTESIAN_POINT('Origin',(-0.0308178595828214,4.69642561677658,
0.190105271132082));
#150515=CARTESIAN_POINT('',(1.25825937515092,4.690053949938,-7.265864284091));
#150516=CARTESIAN_POINT('Origin',(-3.05101267600999E-14,4.75000000000067,
7.27716498172271E-13));
#150517=CARTESIAN_POINT('Origin',(-0.0503353653922689,4.55370522141256,
0.180773999130557));
#150518=CARTESIAN_POINT('Origin',(-0.00185191242419259,4.69643088564423,
0.193018537816066));
#150519=CARTESIAN_POINT('Ctrl Pts',(2.43049704745381,4.559162772,-7.09581366672906));
#150520=CARTESIAN_POINT('Ctrl Pts',(2.04345770503465,4.624819703,-7.22838450697445));
#150521=CARTESIAN_POINT('Ctrl Pts',(1.64429532976121,4.690053947,-7.31807217464651));
#150522=CARTESIAN_POINT('Ctrl Pts',(1.63048994031571,4.69231013194975,-7.32117410322842));
#150523=CARTESIAN_POINT('Ctrl Pts',(1.61668455087021,4.6945663168996,-7.32427603181019));
#150524=CARTESIAN_POINT('Ctrl Pts',(2.122659554,4.559162772,-6.932302389));
#150525=CARTESIAN_POINT('Ctrl Pts',(1.744538893,4.624819703,-7.04808231200001));
#150526=CARTESIAN_POINT('Ctrl Pts',(1.356068566,4.690053947,-7.122048725));
#150527=CARTESIAN_POINT('Ctrl Pts',(1.34263297065216,4.69231013194975,-7.12460691986156));
#150528=CARTESIAN_POINT('Ctrl Pts',(1.32919737530432,4.69456631689961,-7.12716511472311));
#150529=CARTESIAN_POINT('',(1.64369968460078,4.69005394784289,-7.3176670917166));
#150530=CARTESIAN_POINT('',(1.49988411999609,4.69005394666591,-7.2198578984163));
#150531=CARTESIAN_POINT('',(2.19171665251882,4.5993304993999,-7.17261306051613));
#150532=CARTESIAN_POINT('Origin',(-0.0629454646808558,4.55358396244398,
0.180825979175384));
#150533=CARTESIAN_POINT('Ctrl Pts',(2.11814815554888,4.55994605589016,-6.93368218179206));
#150534=CARTESIAN_POINT('Ctrl Pts',(2.13043236396242,4.56683176230701,-6.97343443721287));
#150535=CARTESIAN_POINT('Ctrl Pts',(2.14271041516511,4.57355155128209,-7.01324328231874));
#150536=CARTESIAN_POINT('Ctrl Pts',(2.16722800827723,4.58666922560028,-7.09287444942555));
#150537=CARTESIAN_POINT('Ctrl Pts',(2.17948126587846,4.59307444474345,-7.13274132976735));
#150538=CARTESIAN_POINT('Ctrl Pts',(2.19171665082185,4.59933049938899,-7.17261306095534));
#150539=CARTESIAN_POINT('Origin',(8.5717023756704E-13,4.78597145200391,
-2.99760216648792E-12));
#150540=CARTESIAN_POINT('',(2.37151803891094,4.7499999938475,-7.11518813706192));
#150541=CARTESIAN_POINT('',(2.17751456608805,4.78575691087531,-7.13956267624426));
#150542=CARTESIAN_POINT('Origin',(1.30672564833516,4.8079276597757,0.634279716635853));
#150543=CARTESIAN_POINT('',(2.00603658800724,4.74999999555741,-7.22674317728731));
#150544=CARTESIAN_POINT('Origin',(0.,4.74999999326975,0.));
#150545=CARTESIAN_POINT('Origin',(-1.38878602413738,5.02638845336712,-0.443159275849884));
#150546=CARTESIAN_POINT('Ctrl Pts',(2.726181675,4.690053947,-6.986983146));
#150547=CARTESIAN_POINT('Ctrl Pts',(2.345085845,4.624398499,-7.135679149));
#150548=CARTESIAN_POINT('Ctrl Pts',(1.950078078,4.559170361,-7.24204359900001));
#150549=CARTESIAN_POINT('Ctrl Pts',(2.855394386,4.690053947,-6.664024527));
#150550=CARTESIAN_POINT('Ctrl Pts',(2.491913911,4.624398499,-6.819768268));
#150551=CARTESIAN_POINT('Ctrl Pts',(2.113650457,4.559170361,-6.93505456));
#150552=CARTESIAN_POINT('',(2.72618166935645,4.69005394803174,-6.98698313594653));
#150553=CARTESIAN_POINT('Origin',(-0.0709643567426155,4.69642561864978,
0.179035762751935));
#150554=CARTESIAN_POINT('',(2.7907880137327,4.690053949938,-6.82550384335576));
#150555=CARTESIAN_POINT('Origin',(-4.50052321798733E-13,4.75090401395802,
1.38300829122251E-12));
#150556=CARTESIAN_POINT('Origin',(-0.0880199733596998,4.55370251574272,
0.165726709096222));
#150557=CARTESIAN_POINT('Origin',(-0.0433024939353446,4.69643084185895,
0.188110501452672));
#150558=CARTESIAN_POINT('Ctrl Pts',(3.89906356438713,4.559162772,-6.40743246671499));
#150559=CARTESIAN_POINT('Ctrl Pts',(3.54957179941302,4.624819703,-6.6201058918965));
#150560=CARTESIAN_POINT('Ctrl Pts',(3.17902181505483,4.690053947,-6.79350482402605));
#150561=CARTESIAN_POINT('Ctrl Pts',(3.16620601100702,4.69231013192402,-6.79950198184572));
#150562=CARTESIAN_POINT('Ctrl Pts',(3.15339020695927,4.69456631684815,-6.80549913966536));
#150563=CARTESIAN_POINT('Ctrl Pts',(3.563273049,4.559162772,-6.313919953));
#150564=CARTESIAN_POINT('Ctrl Pts',(3.2188819,4.624819703,-6.508277771));
#150565=CARTESIAN_POINT('Ctrl Pts',(2.855394386,4.690053947,-6.664024527));
#150566=CARTESIAN_POINT('Ctrl Pts',(2.84282284383327,4.69231013192402,-6.66941116845251));
#150567=CARTESIAN_POINT('Ctrl Pts',(2.83025130166646,4.69456631684816,-6.67479780990509));
#150568=CARTESIAN_POINT('',(3.1783530148737,4.69005394784287,-6.79323725781927));
#150569=CARTESIAN_POINT('',(3.01687369313244,4.69005394666591,-6.72863088383735));
#150570=CARTESIAN_POINT('',(3.68237532182294,4.59933049940066,-6.53376705968035));
#150571=CARTESIAN_POINT('Origin',(-0.10034614614094,4.55358391768731,0.163067068109141));
#150572=CARTESIAN_POINT('Ctrl Pts',(3.55916373987557,4.55994605586385,-6.31623730438967));
#150573=CARTESIAN_POINT('Ctrl Pts',(3.5797063099409,4.56683176228965,-6.35241943252761));
#150574=CARTESIAN_POINT('Ctrl Pts',(3.60025503180654,4.57355155123174,-6.38865815067293));
#150575=CARTESIAN_POINT('Ctrl Pts',(3.64131776415789,4.58666922559734,-6.46115702773757));
#150576=CARTESIAN_POINT('Ctrl Pts',(3.66185474822864,4.59307444476411,-6.49745775448508));
#150577=CARTESIAN_POINT('Ctrl Pts',(3.68237532020963,4.59933049940131,-6.53376706059202));
#150578=CARTESIAN_POINT('Origin',(1.14600169631718E-12,4.78597145199413,
-1.87566975839992E-12));
#150579=CARTESIAN_POINT('',(3.84562837013886,4.74999999914954,-6.43903272537783));
#150580=CARTESIAN_POINT('',(3.66140041776986,4.78575691070765,-6.50454240333656));
#150581=CARTESIAN_POINT('Origin',(1.1398144114279,4.80792588123016,0.900383793170842));
#150582=CARTESIAN_POINT('',(3.51267274782531,4.75000000027185,-6.62654735586201));
#150583=CARTESIAN_POINT('Origin',(0.,4.75,0.));
#150584=CARTESIAN_POINT('Origin',(-1.2610691785014,5.02638720208912,-0.731323920078562));
#150585=CARTESIAN_POINT('Ctrl Pts',(4.164439905,4.690053947,-6.237582888));
#150586=CARTESIAN_POINT('Ctrl Pts',(3.824219129,4.624398499,-6.464726799));
#150587=CARTESIAN_POINT('Ctrl Pts',(3.461311636,4.559170361,-6.653519501));
#150588=CARTESIAN_POINT('Ctrl Pts',(4.221205138,4.690053947,-5.894397949));
#150589=CARTESIAN_POINT('Ctrl Pts',(3.899702935,4.624398499,-6.124638046));
#150590=CARTESIAN_POINT('Ctrl Pts',(3.555066216,4.559170361,-6.318544469));
#150591=CARTESIAN_POINT('',(4.16443989737977,4.69005394803158,-6.23758287935845));
#150592=CARTESIAN_POINT('Origin',(-0.107792655760439,4.69642564592103,0.159594784685343));
#150593=CARTESIAN_POINT('',(4.1928225065985,4.690053949938,-6.06599042879994));
#150594=CARTESIAN_POINT('Origin',(-1.8995222061946E-13,4.74999999999911,
2.71917904859365E-13));
#150595=CARTESIAN_POINT('Origin',(-0.121588202048631,4.55370494317573,0.142930731139171));
#150596=CARTESIAN_POINT('Origin',(-0.0827268737517912,4.69643090457438,
0.174400752628615));
#150597=CARTESIAN_POINT('Ctrl Pts',(5.18531420312347,4.559162772,-5.41944684537583));
#150598=CARTESIAN_POINT('Ctrl Pts',(4.88971186047583,4.624819703,-5.70227848261605));
#150599=CARTESIAN_POINT('Ctrl Pts',(4.56510077449987,4.690053947,-5.95128073642792));
#150600=CARTESIAN_POINT('Ctrl Pts',(4.55387380845167,4.692310131937,-5.9598927030866));
#150601=CARTESIAN_POINT('Ctrl Pts',(4.54264684240356,4.6945663168741,-5.96850466974531));
#150602=CARTESIAN_POINT('Ctrl Pts',(4.837271857,4.559162772,-5.400305637));
#150603=CARTESIAN_POINT('Ctrl Pts',(4.54271356700001,4.624819703,-5.664153394));
#150604=CARTESIAN_POINT('Ctrl Pts',(4.221205138,4.690053947,-5.894397949));
#150605=CARTESIAN_POINT('Ctrl Pts',(4.21008548013084,4.692310131937,-5.90236116379284));
#150606=CARTESIAN_POINT('Ctrl Pts',(4.19896582226168,4.69456631687411,-5.91032437858578));
#150607=CARTESIAN_POINT('',(4.56439009168813,4.69005394784288,-5.9511631980305));
#150608=CARTESIAN_POINT('',(4.39279760585611,4.69005394666591,-5.92278056671925));
#150609=CARTESIAN_POINT('',(5.00085021438104,4.59933049938672,-5.58940937257166));
#150610=CARTESIAN_POINT('Origin',(-0.133054669290137,4.55358395399458,0.137683165336694));
#150611=CARTESIAN_POINT('Ctrl Pts',(4.83375678258189,4.55994605579482,-5.40345218965846));
#150612=CARTESIAN_POINT('Ctrl Pts',(4.86159716688665,4.56683176220404,-5.43437235436266));
#150613=CARTESIAN_POINT('Ctrl Pts',(4.88945572468579,4.57355155121591,-5.46534646398862));
#150614=CARTESIAN_POINT('Ctrl Pts',(4.94514354884021,4.58666922555817,-5.52732308389661));
#150615=CARTESIAN_POINT('Ctrl Pts',(4.97300397295751,4.59307444472928,-5.55836027535948));
#150616=CARTESIAN_POINT('Ctrl Pts',(5.00085021303988,4.59933049938737,-5.58940937377434));
#150617=CARTESIAN_POINT('Origin',(-5.44833275717416E-12,4.78597145200978,
6.35385841163405E-12));
#150618=CARTESIAN_POINT('',(5.13992141746291,4.74999999882868,-5.46179529326095));
#150619=CARTESIAN_POINT('',(4.97408325416057,4.7857569107727,-5.56537695720217));
#150620=CARTESIAN_POINT('Origin',(0.919614054641487,4.80792560169836,1.12435350215151));
#150621=CARTESIAN_POINT('',(4.85506021308921,4.7500000000112,-5.71650155458869));
#150622=CARTESIAN_POINT('Origin',(0.,4.74999999935832,0.));
#150623=CARTESIAN_POINT('Origin',(-1.07437204041214,5.02638715273715,-0.985319364612672));
#150624=CARTESIAN_POINT('Ctrl Pts',(5.407973553,4.690053947,-5.196520186));
#150625=CARTESIAN_POINT('Ctrl Pts',(5.124536177,4.624398499,-5.491491009));
#150626=CARTESIAN_POINT('Ctrl Pts',(4.81069811,4.559170361,-5.753884227));
#150627=CARTESIAN_POINT('Ctrl Pts',(5.38963703,4.690053947,-4.849155874));
#150628=CARTESIAN_POINT('Ctrl Pts',(5.125146184,4.624398499,-5.143126555));
#150629=CARTESIAN_POINT('Ctrl Pts',(4.830251029,4.559170361,-5.406586261));
#150630=CARTESIAN_POINT('',(5.40797354386518,4.69005394803172,-5.19652017958922));
#150631=CARTESIAN_POINT('Origin',(-0.139580695309564,4.69642566362389,0.132691297140924));
#150632=CARTESIAN_POINT('',(5.39880527916107,4.690053949938,-5.02283804326252));
#150633=CARTESIAN_POINT('Origin',(-1.26287869051112E-12,4.74999999999956,
1.40512601554121E-12));
#150634=CARTESIAN_POINT('Origin',(-0.149471413819263,4.55370501835464,0.113451231802965));
#150635=CARTESIAN_POINT('Origin',(-0.118283791850866,4.69643088939873,0.152539578053445));
#150636=CARTESIAN_POINT('Ctrl Pts',(6.22910531271845,4.559162772,-4.17805391237519));
#150637=CARTESIAN_POINT('Ctrl Pts',(6.0012144302889,4.624819703,-4.51781886921915));
#150638=CARTESIAN_POINT('Ctrl Pts',(5.73772069551008,4.690053947,-4.83078137711657));
#150639=CARTESIAN_POINT('Ctrl Pts',(5.72860752801795,4.6923101319233,-4.84160546656077));
#150640=CARTESIAN_POINT('Ctrl Pts',(5.71949436052576,4.69456631684671,-4.85242955600499));
#150641=CARTESIAN_POINT('Ctrl Pts',(5.88508521,4.559162772,-4.234179032));
#150642=CARTESIAN_POINT('Ctrl Pts',(5.65413299700001,4.624819703,-4.5551795));
#150643=CARTESIAN_POINT('Ctrl Pts',(5.38963702999999,4.690053947,-4.849155874));
#150644=CARTESIAN_POINT('Ctrl Pts',(5.38048919940626,4.6923101319233,-4.85932331094969));
#150645=CARTESIAN_POINT('Ctrl Pts',(5.37134136881263,4.69456631684671,-4.86949074789924));
#150646=CARTESIAN_POINT('',(5.73700136077215,4.69005394784288,-4.83081936251135));
#150647=CARTESIAN_POINT('',(5.56331918515664,4.6900539466659,-4.83998761354413));
#150648=CARTESIAN_POINT('',(6.08549090878228,4.59933049942498,-4.38369711544624));
#150649=CARTESIAN_POINT('Origin',(-0.159541754778343,4.55358395733858,0.105861394661615));
#150650=CARTESIAN_POINT('Ctrl Pts',(5.8823287320493,4.55994605591031,-4.23800765756635));
#150651=CARTESIAN_POINT('Ctrl Pts',(5.91616514536365,4.5668317623968,-4.26222006641938));
#150652=CARTESIAN_POINT('Ctrl Pts',(5.95003090265298,4.57355155125049,-4.28648125144309));
#150653=CARTESIAN_POINT('Ctrl Pts',(6.01773991774795,4.5866692256407,-4.3350376563432));
#150654=CARTESIAN_POINT('Ctrl Pts',(6.05162105914308,4.59307444479192,-4.35936004775182));
#150655=CARTESIAN_POINT('Ctrl Pts',(6.08549090774786,4.59933049942563,-4.38369711688568));
#150656=CARTESIAN_POINT('Origin',(-3.96991467477292E-12,4.7859714520137,
2.91780488659299E-12));
#150657=CARTESIAN_POINT('',(6.19387744881142,4.74999999914954,-4.22917038556074));
#150658=CARTESIAN_POINT('',(6.05418348610776,4.78575691089176,-4.36598066988852));
#150659=CARTESIAN_POINT('Origin',(0.656406945464102,4.80792672811356,1.29576130127513));
#150660=CARTESIAN_POINT('',(5.97043045959225,4.75000000037016,-4.53915849232614));
#150661=CARTESIAN_POINT('Origin',(0.,4.75,0.));
#150662=CARTESIAN_POINT('Origin',(-0.837438612039119,5.02638723124253,-1.19324172669549));
#150663=CARTESIAN_POINT('Ctrl Pts',(6.398636369,4.690053947,-3.912473977));
#150664=CARTESIAN_POINT('Ctrl Pts',(6.185235608,4.624398499,-4.261479203));
#150665=CARTESIAN_POINT('Ctrl Pts',(5.935141687,4.559170361,-4.585203721));
#150666=CARTESIAN_POINT('Ctrl Pts',(6.306055484,4.690053947,-3.577172659));
#150667=CARTESIAN_POINT('Ctrl Pts',(6.110943294,4.624398499,-3.921128183));
#150668=CARTESIAN_POINT('Ctrl Pts',(5.879578673,4.559170361,-4.241822088));
#150669=CARTESIAN_POINT('',(6.39863635852685,4.69005394803158,-3.91247397243082));
#150670=CARTESIAN_POINT('Origin',(-0.164842356092871,4.69642565962801,0.0995835179095694));
#150671=CARTESIAN_POINT('',(6.35234591730059,4.690053949938,-3.74482333360496));
#150672=CARTESIAN_POINT('Origin',(-1.02261948908833E-12,4.75,7.79324521582581E-13));
#150673=CARTESIAN_POINT('Origin',(-0.170365513633566,4.55370509620838,0.0786668822203401));
#150674=CARTESIAN_POINT('Origin',(-0.148309793580546,4.69643087912402,0.123545680302601));
#150675=CARTESIAN_POINT('Ctrl Pts',(6.98163038085746,4.559162772,-2.74129982288076));
#150676=CARTESIAN_POINT('Ctrl Pts',(6.83210688281943,4.624819703,-3.12211106707122));
#150677=CARTESIAN_POINT('Ctrl Pts',(6.64205117339044,4.690053947,-3.4844000493798));
#150678=CARTESIAN_POINT('Ctrl Pts',(6.63547792607009,4.69231013188838,-3.49693013905352));
#150679=CARTESIAN_POINT('Ctrl Pts',(6.62890467874978,4.69456631677688,-3.50946022872725));
#150680=CARTESIAN_POINT('Ctrl Pts',(6.657718518,4.559162772,-2.870066921));
#150681=CARTESIAN_POINT('Ctrl Pts',(6.501171452,4.624819703,-3.233210475));
#150682=CARTESIAN_POINT('Ctrl Pts',(6.306055484,4.690053947,-3.577172659));
#150683=CARTESIAN_POINT('Ctrl Pts',(6.29930722309448,4.69231013188838,-3.58906889990256));
#150684=CARTESIAN_POINT('Ctrl Pts',(6.29255896218899,4.69456631677687,-3.60096514080513));
#150685=CARTESIAN_POINT('',(6.64135682204414,4.69005394784288,-3.48459178239997));
#150686=CARTESIAN_POINT('',(6.47370614201999,4.69005394666591,-3.53088221829681));
#150687=CARTESIAN_POINT('',(6.88558081144145,4.59933049941794,-2.97300805372012));
#150688=CARTESIAN_POINT('Origin',(-0.178568932337102,4.55358397399639,0.0690897059675322));
#150689=CARTESIAN_POINT('Ctrl Pts',(6.65584952666731,4.55994605584957,-2.87439859628003));
#150690=CARTESIAN_POINT('Ctrl Pts',(6.6940998151804,4.5668317622885,-2.89077110385448));
#150691=CARTESIAN_POINT('Ctrl Pts',(6.73238924811481,4.57355155126783,-2.90718493953025));
#150692=CARTESIAN_POINT('Ctrl Pts',(6.80895345550018,4.58666922562728,-2.9400506860028));
#150693=CARTESIAN_POINT('Ctrl Pts',(6.84727106988585,4.59307444478919,-2.95652098963909));
#150694=CARTESIAN_POINT('Ctrl Pts',(6.88558081071488,4.59933049941858,-2.97300805540815));
#150695=CARTESIAN_POINT('Origin',(3.95473584435813E-12,4.78597145199804,
-1.96283961306776E-12));
#150696=CARTESIAN_POINT('',(6.95821465503485,4.74999999914954,-2.79879417147286));
#150697=CARTESIAN_POINT('',(6.8511968275965,4.78575691069479,-2.9624359783415));
#150698=CARTESIAN_POINT('Origin',(0.362509295536758,4.80792588316658,1.40657558479531));
#150699=CARTESIAN_POINT('',(6.80663001231747,4.75000000027878,-3.14956942582316));
#150700=CARTESIAN_POINT('Origin',(0.,4.75,0.));
#150701=CARTESIAN_POINT('Origin',(-0.561349968343476,5.0263871185875,-1.3453684552072));
#150702=CARTESIAN_POINT('Ctrl Pts',(7.090106059,4.690053947,-2.445484832));
#150703=CARTESIAN_POINT('Ctrl Pts',(6.95672029700001,4.624398499,-2.832205366));
#150704=CARTESIAN_POINT('Ctrl Pts',(6.782064634,4.559170361,-3.202124185));
#150705=CARTESIAN_POINT('Ctrl Pts',(6.927609792,4.690053947,-2.137924827));
#150706=CARTESIAN_POINT('Ctrl Pts',(6.810999487,4.624398499,-2.515782215));
#150707=CARTESIAN_POINT('Ctrl Pts',(6.653983753,4.559170361,-2.87871503));
#150708=CARTESIAN_POINT('',(7.09010604806595,4.69005394803172,-2.44548483005023));
#150709=CARTESIAN_POINT('Origin',(-0.182395659034899,4.69642565507823,0.0618189606728303));
#150710=CARTESIAN_POINT('',(7.00885791987027,4.690053949938,-2.29170484671772));
#150711=CARTESIAN_POINT('Origin',(1.12757025938492E-13,4.74999999999867,
-4.25007251614318E-14));
#150712=CARTESIAN_POINT('Origin',(-0.183293516937355,4.55370498131794,0.0402041254209368));
#150713=CARTESIAN_POINT('Origin',(-0.17140124332232,4.69643083059612,0.0887751290949265));
#150714=CARTESIAN_POINT('Ctrl Pts',(7.40770217167405,4.559162772,-1.17636559943074));
#150715=CARTESIAN_POINT('Ctrl Pts',(7.34353761132999,4.624819703,-1.58041682070035));
#150716=CARTESIAN_POINT('Ctrl Pts',(7.23580672026506,4.690053947,-1.97509204846267));
#150717=CARTESIAN_POINT('Ctrl Pts',(7.23208075058599,4.692310131951,-1.98874224588683));
#150718=CARTESIAN_POINT('Ctrl Pts',(7.22835478090692,4.69456631690211,-2.00239244331094));
#150719=CARTESIAN_POINT('Ctrl Pts',(7.11904430900001,4.559162772,-1.371753671));
#150720=CARTESIAN_POINT('Ctrl Pts',(7.044222355,4.624819703,-1.760060122));
#150721=CARTESIAN_POINT('Ctrl Pts',(6.927609792,4.690053947,-2.137924827));
#150722=CARTESIAN_POINT('Ctrl Pts',(6.92357664171564,4.692310131951,-2.15099361738777));
#150723=CARTESIAN_POINT('Ctrl Pts',(6.91954349143118,4.69456631690211,-2.1640624077756));
#150724=CARTESIAN_POINT('',(7.23516982050699,4.69005394784373,-1.97542856188366));
#150725=CARTESIAN_POINT('',(7.08138979442916,4.69005394666591,-2.05667669546547));
#150726=CARTESIAN_POINT('',(7.36370860875662,4.59933049944325,-1.42330443902713));
#150727=CARTESIAN_POINT('Origin',(-0.189246121424158,4.55358393686277,0.0290873285901153));
#150728=CARTESIAN_POINT('Ctrl Pts',(7.11815019508415,4.55994605582322,-1.37638585233793));
#150729=CARTESIAN_POINT('Ctrl Pts',(7.15902581871411,4.56683176234725,-1.38415289818672));
#150730=CARTESIAN_POINT('Ctrl Pts',(7.1999485548656,4.57355155123402,-1.39195189089798));
#150731=CARTESIAN_POINT('Ctrl Pts',(7.28178789791662,4.58666922564619,-1.40759021280355));
#150732=CARTESIAN_POINT('Ctrl Pts',(7.32275029616096,4.59307444480266,-1.41543829532522));
#150733=CARTESIAN_POINT('Ctrl Pts',(7.36370860839515,4.59933049943885,-1.42330444072867));
#150734=CARTESIAN_POINT('Origin',(-2.30674854218016E-12,4.785971452,5.12827627585644E-13));
#150735=CARTESIAN_POINT('',(7.39719347865309,4.74999999914955,-1.23754944963554));
#150736=CARTESIAN_POINT('',(7.32785581920364,4.78575691081595,-1.42037107383782));
#150737=CARTESIAN_POINT('Origin',(0.0516638793933411,4.80792777455635,1.45161900251207));
#150738=CARTESIAN_POINT('',(7.32455911116738,4.75000000048191,-1.61270999145831));
#150739=CARTESIAN_POINT('Origin',(0.,4.75,0.));
#150740=CARTESIAN_POINT('Origin',(-0.2590104406192,5.02638720502974,-1.43458817797988));
#150741=CARTESIAN_POINT('Ctrl Pts',(7.450050271,4.690053947,-0.864147535));
#150742=CARTESIAN_POINT('Ctrl Pts',(7.402916477,4.624398499,-1.270500754));
#150743=CARTESIAN_POINT('Ctrl Pts',(7.311865778,4.559170361,-1.669316881));
#150744=CARTESIAN_POINT('Ctrl Pts',(7.225236766,4.690053947,-0.598710006));
#150745=CARTESIAN_POINT('Ctrl Pts',(7.192580914,4.624398499,-0.992801067));
#150746=CARTESIAN_POINT('Ctrl Pts',(7.11725594700001,4.559170361,-1.381002455));
#150747=CARTESIAN_POINT('',(7.45005025959605,4.69005394803157,-0.86414753525958));
#150748=CARTESIAN_POINT('Origin',(-0.1914207062953,4.69642563955896,0.0211640149895437));
#150749=CARTESIAN_POINT('',(7.3376435167032,4.690053949938,-0.731428788525407));
#150750=CARTESIAN_POINT('Origin',(-3.65592972562112E-13,4.74999999999956,
3.09539720244612E-14));
#150751=CARTESIAN_POINT('Origin',(-0.187650922791914,4.55370525479523,-0.000138467856823088));
#150752=CARTESIAN_POINT('Origin',(-0.186477895557537,4.69643089301974,0.0498533727623198));
#150753=CARTESIAN_POINT('Ctrl Pts',(7.48711801033638,4.559162772,0.44327900366248));
#150754=CARTESIAN_POINT('Ctrl Pts',(7.51129654999285,4.624819703,0.0348960660702782));
#150755=CARTESIAN_POINT('Ctrl Pts',(7.49091351203571,4.690053947,-0.373693895907041));
#150756=CARTESIAN_POINT('Ctrl Pts',(7.49060672318581,4.69103579959394,-0.379843658507606));
#150757=CARTESIAN_POINT('Ctrl Pts',(7.49029993433593,4.6920176521879,-0.385993421108172));
#150758=CARTESIAN_POINT('Ctrl Pts',(7.24749149900001,4.559162772,0.190701257));
#150759=CARTESIAN_POINT('Ctrl Pts',(7.25789325,4.624819703,-0.204611314));
#150760=CARTESIAN_POINT('Ctrl Pts',(7.225236766,4.690053947,-0.598710006));
#150761=CARTESIAN_POINT('Ctrl Pts',(7.22474524725832,4.69103579959394,-0.604641657833209));
#150762=CARTESIAN_POINT('Ctrl Pts',(7.22425372851668,4.6920176521879,-0.610573309666416));
#150763=CARTESIAN_POINT('',(7.35795553086503,4.69005394666591,-0.486303255542236));
#150764=CARTESIAN_POINT('Ctrl Pts',(7.24761407171314,4.55994605590014,0.185985165651878));
#150765=CARTESIAN_POINT('Ctrl Pts',(7.28920373119989,4.56683176237926,0.18718675957936));
#150766=CARTESIAN_POINT('Ctrl Pts',(7.3308462695689,4.57355155126511,0.188367281422137));
#150767=CARTESIAN_POINT('Ctrl Pts',(7.41413403124873,4.58666922565181,0.190687614150122));
#150768=CARTESIAN_POINT('Ctrl Pts',(7.45582585715068,4.59307444480204,0.191828720144647));
#150769=CARTESIAN_POINT('Ctrl Pts',(7.49751757552699,4.59933049943424,0.192951307213912));
#150770=CARTESIAN_POINT('Ctrl Pts',(7.461638412,4.690053947,0.75759634));
#150771=CARTESIAN_POINT('Ctrl Pts',(7.50296051,4.624398499,0.350611062));
#150772=CARTESIAN_POINT('Ctrl Pts',(7.499772204,4.559170361,-0.058454175));
#150773=CARTESIAN_POINT('Ctrl Pts',(7.18501969900001,4.690053947,0.96849983));
#150774=CARTESIAN_POINT('Ctrl Pts',(7.237845252,4.624398499,0.576602356));
#150775=CARTESIAN_POINT('Ctrl Pts',(7.247733164,4.559170361,0.181284259));
#150776=CARTESIAN_POINT('',(7.32332905762013,4.690053949938,0.863048067009758));
#150777=CARTESIAN_POINT('Ctrl Pts',(7.21699150219654,4.559162772,2.04277290613802));
#150778=CARTESIAN_POINT('Ctrl Pts',(7.3284140276913,4.624819703,1.64912395011814));
#150779=CARTESIAN_POINT('Ctrl Pts',(7.39635994644821,4.690053947,1.24569138829467));
#150780=CARTESIAN_POINT('Ctrl Pts',(7.3987099170171,4.6923101318642,1.23173831113913));
#150781=CARTESIAN_POINT('Ctrl Pts',(7.40105988758591,4.69456631672851,1.21778523398357));
#150782=CARTESIAN_POINT('Ctrl Pts',(7.037054042,4.559162772,1.744239205));
#150783=CARTESIAN_POINT('Ctrl Pts',(7.132193124,4.624819703,1.360404892));
#150784=CARTESIAN_POINT('Ctrl Pts',(7.185019699,4.690053947,0.96849983));
#150785=CARTESIAN_POINT('Ctrl Pts',(7.1868467534983,4.6923101318642,0.954945441769616));
#150786=CARTESIAN_POINT('Ctrl Pts',(7.18867380799659,4.69456631672851,0.941391053539225));
#150787=CARTESIAN_POINT('',(7.39592321004275,4.69005394784287,1.24511854744902));
#150788=CARTESIAN_POINT('',(7.29047144430719,4.69005394666591,1.10680918397654));
#150789=CARTESIAN_POINT('',(7.28075095287772,4.5993304993567,1.80018486846075));
#150790=CARTESIAN_POINT('Origin',(-0.183968844695832,4.55358393281124,-0.053063498517215));
#150791=CARTESIAN_POINT('Ctrl Pts',(7.03818756905549,4.55994605587417,1.73965972261931));
#150792=CARTESIAN_POINT('Ctrl Pts',(7.07854657820646,4.5668317623275,1.74977377151055));
#150793=CARTESIAN_POINT('Ctrl Pts',(7.11896175983951,4.57355155119665,1.75987860837463));
#150794=CARTESIAN_POINT('Ctrl Pts',(7.19980349683551,4.58666922554476,1.7800491000721));
#150795=CARTESIAN_POINT('Ctrl Pts',(7.24027528686319,4.59307444467864,1.79012603792251));
#150796=CARTESIAN_POINT('Ctrl Pts',(7.2807509531506,4.59933049933453,1.80018486672554));
#150797=CARTESIAN_POINT('Origin',(2.78509854068076E-12,4.78597145200391,
5.46546315149943E-13));
#150798=CARTESIAN_POINT('',(7.23314450266305,4.74999999914954,1.98283146086299));
#150799=CARTESIAN_POINT('',(7.24698015455017,4.78575691066646,1.78779292319316));
#150800=CARTESIAN_POINT('Origin',(-0.562631375081327,4.80792660290743,1.33914652932568));
#150801=CARTESIAN_POINT('',(7.32474915907361,4.75000000027873,1.61184659604922));
#150802=CARTESIAN_POINT('Origin',(0.,4.75,0.));
#150803=CARTESIAN_POINT('Origin',(0.367295502146805,5.02638722262568,-1.4107530368421));
#150804=CARTESIAN_POINT('Ctrl Pts',(7.124328633,4.690053947,2.343915853));
#150805=CARTESIAN_POINT('Ctrl Pts',(7.252174449,4.624398499,1.955328694));
#150806=CARTESIAN_POINT('Ctrl Pts',(7.336997617,4.559170361,1.555141784));
#150807=CARTESIAN_POINT('Ctrl Pts',(6.808839097,4.690053947,2.49042369));
#150808=CARTESIAN_POINT('Ctrl Pts',(6.94467599,4.624398499,2.119044493));
#150809=CARTESIAN_POINT('Ctrl Pts',(7.03931443300001,4.559170361,1.735094322));
#150810=CARTESIAN_POINT('',(7.12432862295937,4.69005394803173,2.34391584792582));
#150811=CARTESIAN_POINT('Origin',(-0.182614947261295,4.69642563816072,-0.0611674429381026));
#150812=CARTESIAN_POINT('',(6.96658387093794,4.690053949938,2.41716975438613));
#150813=CARTESIAN_POINT('Origin',(7.34221711207184E-13,4.75,1.25116930704827E-13));
#150814=CARTESIAN_POINT('Origin',(-0.170249199545465,4.55370499927494,-0.0789182823346504));
#150815=CARTESIAN_POINT('Origin',(-0.19017611680666,4.69643086195197,-0.0330544205486318));
#150816=CARTESIAN_POINT('Ctrl Pts',(6.60912646083892,4.559162772,3.54645385109177));
#150817=CARTESIAN_POINT('Ctrl Pts',(6.80256687883279,4.624819703,3.18596073835499));
#150818=CARTESIAN_POINT('Ctrl Pts',(6.95565033528179,4.690053947,2.80656656940863));
#150819=CARTESIAN_POINT('Ctrl Pts',(6.96094486400092,4.69231013187025,2.79344488160548));
#150820=CARTESIAN_POINT('Ctrl Pts',(6.96623939272004,4.69456631674062,2.78032319380227));
#150821=CARTESIAN_POINT('Ctrl Pts',(6.49757176,4.559162772,3.216218467));
#150822=CARTESIAN_POINT('Ctrl Pts',(6.672999573,4.624819703,2.861810077));
#150823=CARTESIAN_POINT('Ctrl Pts',(6.808839097,4.690053947,2.49042369));
#150824=CARTESIAN_POINT('Ctrl Pts',(6.81353722884059,4.69231013187025,2.47757895852168));
#150825=CARTESIAN_POINT('Ctrl Pts',(6.81823536068105,4.69456631674061,2.46473422704338));
#150826=CARTESIAN_POINT('',(6.95534695338064,4.69005394784287,2.80591323583707));
#150827=CARTESIAN_POINT('',(6.88209301623501,4.6900539466659,2.64816845608985));
#150828=CARTESIAN_POINT('',(6.72354450812389,4.59933049937433,3.32324378386072));
#150829=CARTESIAN_POINT('Origin',(-0.168260686740129,4.55358392025965,-0.0913707750342646));
#150830=CARTESIAN_POINT('Ctrl Pts',(6.49966323789616,4.55994605561308,3.21198972494361));
#150831=CARTESIAN_POINT('Ctrl Pts',(6.53690445392065,4.56683176204481,3.23054330674303));
#150832=CARTESIAN_POINT('Ctrl Pts',(6.57420251092965,4.57355155114227,3.24909996799787));
#150833=CARTESIAN_POINT('Ctrl Pts',(6.64881815344445,4.58666922551254,3.28617746836234));
#150834=CARTESIAN_POINT('Ctrl Pts',(6.68617749202659,4.59307444470469,3.30471905155373));
#150835=CARTESIAN_POINT('Ctrl Pts',(6.72354450892563,4.59933049937499,3.32324378224326));
#150836=CARTESIAN_POINT('Origin',(-1.869164545365E-13,4.78597145201174,
-3.26128013483639E-13));
#150837=CARTESIAN_POINT('',(6.63778745075527,4.74999999914955,3.49138622286761));
#150838=CARTESIAN_POINT('',(6.69322715409837,4.78575691073401,3.30388183192065));
#150839=CARTESIAN_POINT('Origin',(-0.837352477505402,4.80792844078444,1.18688978329396));
#150840=CARTESIAN_POINT('',(6.80700122224742,4.7500000001894,3.14876706890607));
#150841=CARTESIAN_POINT('Origin',(0.,4.75,0.));
#150842=CARTESIAN_POINT('Origin',(0.661979220930704,5.02638726725762,-1.29881225515525));
#150843=CARTESIAN_POINT('Ctrl Pts',(6.453893166,4.690053947,3.820636465));
#150844=CARTESIAN_POINT('Ctrl Pts',(6.66228477,4.624398499,3.468617329));
#150845=CARTESIAN_POINT('Ctrl Pts',(6.831153176,4.559170361,3.096021041));
#150846=CARTESIAN_POINT('Ctrl Pts',(6.114284746,4.690053947,3.895898106));
#150847=CARTESIAN_POINT('Ctrl Pts',(6.326781397,4.624398499,3.562402465));
#150848=CARTESIAN_POINT('Ctrl Pts',(6.501745184,4.559170361,3.207773304));
#150849=CARTESIAN_POINT('',(6.45389315726572,4.69005394803157,3.82063645794471));
#150850=CARTESIAN_POINT('Origin',(-0.165196485025554,4.69642563154551,-0.0989942838258595));
#150851=CARTESIAN_POINT('',(6.28408896547809,4.690053949938,3.85826727006272));
#150852=CARTESIAN_POINT('Origin',(-6.24500451351651E-14,4.75000000000111,
-7.78457159844592E-14));
#150853=CARTESIAN_POINT('Origin',(-0.149303794360807,4.55370519153356,-0.1136717409559));
#150854=CARTESIAN_POINT('Origin',(-0.178624331970231,4.69643085591105,-0.0731639354625961));
#150855=CARTESIAN_POINT('Ctrl Pts',(5.69222601069705,4.559162772,4.88430655567154));
#150856=CARTESIAN_POINT('Ctrl Pts',(5.95863926358972,4.624819703,4.57382554319661));
#150857=CARTESIAN_POINT('Ctrl Pts',(6.18970224441328,4.690053947,4.23620981693912));
#150858=CARTESIAN_POINT('Ctrl Pts',(6.19769376529829,4.69231013196517,4.22453307357731));
#150859=CARTESIAN_POINT('Ctrl Pts',(6.20568528618318,4.69456631693044,4.21285633021548));
#150860=CARTESIAN_POINT('Ctrl Pts',(5.654270243,4.559162772,4.537810928));
#150861=CARTESIAN_POINT('Ctrl Pts',(5.90178398,4.624819703,4.229400204));
#150862=CARTESIAN_POINT('Ctrl Pts',(6.114284746,4.690053947,3.895898106));
#150863=CARTESIAN_POINT('Ctrl Pts',(6.12163427600051,4.69231013196517,3.88436363616904));
#150864=CARTESIAN_POINT('Ctrl Pts',(6.12898380600107,4.69456631693045,3.87282916633803));
#150865=CARTESIAN_POINT('',(6.1895464028051,4.69005394784288,4.23550653979359));
#150866=CARTESIAN_POINT('',(6.15191556712846,4.69005394666591,4.0657023142925));
#150867=CARTESIAN_POINT('',(5.8519525946259,4.59933049938055,4.69091151364114));
#150868=CARTESIAN_POINT('Origin',(-0.144684591781463,4.55358396295006,-0.125405459411204));
#150869=CARTESIAN_POINT('Ctrl Pts',(5.65722187832806,4.55994605571318,4.53413065786506));
#150870=CARTESIAN_POINT('Ctrl Pts',(5.68960394393214,4.56683176216541,4.56025622794808));
#150871=CARTESIAN_POINT('Ctrl Pts',(5.72204085910156,4.57355155117837,4.58639702419375));
#150872=CARTESIAN_POINT('Ctrl Pts',(5.78694146285736,4.58666922554783,4.6386478307439));
#150873=CARTESIAN_POINT('Ctrl Pts',(5.819441468473,4.59307444471782,4.66478707540416));
#150874=CARTESIAN_POINT('Ctrl Pts',(5.85195259571213,4.5993304993756,4.69091151222891));
#150875=CARTESIAN_POINT('Origin',(1.34874750257197E-13,4.78597145199609,
-2.00360561475321E-13));
#150876=CARTESIAN_POINT('',(5.82650629123494,4.78575691079304,4.66548489794723));
#150877=CARTESIAN_POINT('',(5.97096547238726,4.75000000041425,4.53845469496143));
#150878=CARTESIAN_POINT('Origin',(0.92570899729587,5.02638719854594,-1.12614049721395));
#150879=CARTESIAN_POINT('',(5.73205483608437,4.74999999914954,4.8366876429795));
#150880=CARTESIAN_POINT('Origin',(-1.07292243168096,4.80792777578605,0.97913448072838));
#150881=CARTESIAN_POINT('Origin',(0.,4.75,0.));
#150882=CARTESIAN_POINT('Ctrl Pts',(5.481680828,4.690053947,5.118708363));
#150883=CARTESIAN_POINT('Ctrl Pts',(5.76087406,4.624398499,4.819717273));
#150884=CARTESIAN_POINT('Ctrl Pts',(6.005891605,4.559170361,4.492133795));
#150885=CARTESIAN_POINT('Ctrl Pts',(5.133833235,4.690053947,5.119204656));
#150886=CARTESIAN_POINT('Ctrl Pts',(5.413053537,4.624398499,4.839186457));
#150887=CARTESIAN_POINT('Ctrl Pts',(5.660161555,4.559170361,4.530460371));
#150888=CARTESIAN_POINT('',(5.48168082074437,4.69005394803159,5.11870835410218));
#150889=CARTESIAN_POINT('Origin',(-0.14005363540327,4.69642563875725,-0.132192374471661));
#150890=CARTESIAN_POINT('',(5.30775704407508,4.690053949938,5.11895649646111));
#150891=CARTESIAN_POINT('Origin',(8.36136715420821E-13,4.74999999999978,
7.61543605953818E-13));
#150892=CARTESIAN_POINT('Origin',(-0.121377084426482,4.55370515177357,-0.143110064267615));
#150893=CARTESIAN_POINT('Origin',(-0.158719385570818,4.69643090990026,-0.109851836851031));
#150894=CARTESIAN_POINT('Ctrl Pts',(4.50916339979654,4.559162772,5.99377451452989));
#150895=CARTESIAN_POINT('Ctrl Pts',(4.83609229828164,4.624819703,5.74782334937737));
#150896=CARTESIAN_POINT('Ctrl Pts',(5.13433055676917,4.690053947,5.46777260231845));
#150897=CARTESIAN_POINT('Ctrl Pts',(5.14464539467451,4.69231013189109,5.45808679582318));
#150898=CARTESIAN_POINT('Ctrl Pts',(5.15496023257999,4.69456631678204,5.44840098932806));
#150899=CARTESIAN_POINT('Ctrl Pts',(4.546581334,4.559162772,5.647220394));
#150900=CARTESIAN_POINT('Ctrl Pts',(4.85460752600001,4.624819703,5.399228277));
#150901=CARTESIAN_POINT('Ctrl Pts',(5.133833235,4.690053947,5.119204656));
#150902=CARTESIAN_POINT('Ctrl Pts',(5.14349050681334,4.69231013189109,5.10951978768387));
#150903=CARTESIAN_POINT('Ctrl Pts',(5.15314777862652,4.69456631678204,5.09983491936761));
#150904=CARTESIAN_POINT('',(5.13432954246051,4.69005394784287,5.46705226606116));
#150905=CARTESIAN_POINT('',(5.1340813834691,4.69005394666591,5.29312845107505));
#150906=CARTESIAN_POINT('',(4.70672988215593,4.59933049940442,5.83923743480986));
#150907=CARTESIAN_POINT('Origin',(-0.11434362949745,4.55358395443845,-0.153576638647377));
#150908=CARTESIAN_POINT('Ctrl Pts',(4.55025511129988,4.55994605576316,5.644260680249));
#150909=CARTESIAN_POINT('Ctrl Pts',(4.57626387695763,4.5668317622278,5.67673663603041));
#150910=CARTESIAN_POINT('Ctrl Pts',(4.60232293648434,4.57355155120668,5.70923925282838));
#150911=CARTESIAN_POINT('Ctrl Pts',(4.65447382140656,4.58666922558688,5.7742201761127));
#150912=CARTESIAN_POINT('Ctrl Pts',(4.68059483006131,4.59307444475615,5.80673484034052));
#150913=CARTESIAN_POINT('Ctrl Pts',(4.70672988354947,4.59933049940507,5.83923743368921));
#150914=CARTESIAN_POINT('Origin',(-9.19533546528406E-12,4.7859714520137,
-1.14287919406042E-11));
#150915=CARTESIAN_POINT('',(4.55829770857552,4.74999999914954,5.95583092444217));
#150916=CARTESIAN_POINT('',(4.68734446911356,4.78575691068609,5.8089350766075));
#150917=CARTESIAN_POINT('Origin',(-1.25832423490427,4.80792609755448,0.725594838512503));
#150918=CARTESIAN_POINT('',(4.85573401490558,4.75000000031464,5.71592922179221));
#150919=CARTESIAN_POINT('Origin',(0.,4.75,0.));
#150920=CARTESIAN_POINT('Origin',(1.14615261721564,5.02638715152315,-0.900813176263141));
#150921=CARTESIAN_POINT('Ctrl Pts',(4.253151186,4.690053947,6.17743514600001));
#150922=CARTESIAN_POINT('Ctrl Pts',(4.590091282,4.624398499,5.945452595));
#150923=CARTESIAN_POINT('Ctrl Pts',(4.899801218,4.559170361,5.678199365));
#150924=CARTESIAN_POINT('Ctrl Pts',(3.913329389,4.690053947,6.103142887));
#150925=CARTESIAN_POINT('Ctrl Pts',(4.246217311,4.624398499,5.889695469));
#150926=CARTESIAN_POINT('Ctrl Pts',(4.553915063,4.559170361,5.641308146));
#150927=CARTESIAN_POINT('',(4.25315118114086,4.69005394803172,6.17743513593807));
#150928=CARTESIAN_POINT('Origin',(-0.108361582184732,4.69642567909109,-0.159208914794227));
#150929=CARTESIAN_POINT('',(4.08324030258406,4.690053949938,6.14028900646922));
#150930=CARTESIAN_POINT('Origin',(-1.77809156287623E-14,4.74999999999956,
-1.17961196366423E-13));
#150931=CARTESIAN_POINT('Origin',(-0.0877749029782665,4.5537050316539,-0.165856721729633));
#150932=CARTESIAN_POINT('Origin',(-0.131394108785226,4.6964308432268,-0.141403975757775));
#150933=CARTESIAN_POINT('Ctrl Pts',(3.1152573196754,4.559162772,6.82298023810282));
#150934=CARTESIAN_POINT('Ctrl Pts',(3.48741503214274,4.624819703,6.65305932404764));
#150935=CARTESIAN_POINT('Ctrl Pts',(3.83888327806662,4.690053947,6.4436684168068));
#150936=CARTESIAN_POINT('Ctrl Pts',(3.85103912306244,4.6923101319262,6.43642644419198));
#150937=CARTESIAN_POINT('Ctrl Pts',(3.86319496805827,4.69456631685225,6.42918447157713));
#150938=CARTESIAN_POINT('Ctrl Pts',(3.226299335,4.559162772,6.49257211000001));
#150939=CARTESIAN_POINT('Ctrl Pts',(3.58043502,4.624819703,6.316594438));
#150940=CARTESIAN_POINT('Ctrl Pts',(3.913329389,4.690053947,6.10314288700001));
#150941=CARTESIAN_POINT('Ctrl Pts',(3.9248428397782,4.69231013192617,6.09576047337325));
#150942=CARTESIAN_POINT('Ctrl Pts',(3.93635629055647,4.69456631685245,6.08837805974651));
#150943=CARTESIAN_POINT('',(3.83903713682742,4.69005394784374,6.44296470519193));
#150944=CARTESIAN_POINT('',(3.87618326074108,4.69005394666591,6.27305378442417));
#150945=CARTESIAN_POINT('',(3.34142571134262,4.59933049939646,6.71452710297746));
#150946=CARTESIAN_POINT('Origin',(-0.0786558691804817,4.55358394933083,
-0.174566528440784));
#150947=CARTESIAN_POINT('Ctrl Pts',(3.23052347273378,4.55994605588832,6.49047134690414));
#150948=CARTESIAN_POINT('Ctrl Pts',(3.24894279744353,4.56683176235996,6.52777914878455));
#150949=CARTESIAN_POINT('Ctrl Pts',(3.26740550851356,4.57355155122262,6.56512379933834));
#150950=CARTESIAN_POINT('Ctrl Pts',(3.30436815712275,4.58666922561447,6.63979640350505));
#150951=CARTESIAN_POINT('Ctrl Pts',(3.32288877939436,4.5930744447669,6.67716613756715));
#150952=CARTESIAN_POINT('Ctrl Pts',(3.3414257129925,4.5993304993971,6.71452710215876));
#150953=CARTESIAN_POINT('Origin',(-8.93903007170849E-12,4.78597145200196,
-1.72535596920653E-11));
#150954=CARTESIAN_POINT('',(3.17139962945521,4.74999999503922,6.79648618146043));
#150955=CARTESIAN_POINT('',(3.32900762991155,4.78575691070129,6.68076590640131));
#150956=CARTESIAN_POINT('Origin',(-1.38487057762148,4.80792772181027,0.438150558516112));
#150957=CARTESIAN_POINT('',(3.51345384874766,4.74999999648354,6.62613324541698));
#150958=CARTESIAN_POINT('Origin',(0.,4.74999999465775,0.));
#150959=CARTESIAN_POINT('Origin',(1.3130107249243,5.02638811558047,-0.633342583323322));
#150960=CARTESIAN_POINT('Ctrl Pts',(2.825748922,4.690053947,6.947311928));
#150961=CARTESIAN_POINT('Ctrl Pts',(3.204680937,4.624398499,6.79318516));
#150962=CARTESIAN_POINT('Ctrl Pts',(3.564601571,4.559170361,6.598758644));
#150963=CARTESIAN_POINT('Ctrl Pts',(2.509842609,4.690053947,6.801704939));
#150964=CARTESIAN_POINT('Ctrl Pts',(2.880832682,4.624398499,6.66480886600001));
#150965=CARTESIAN_POINT('Ctrl Pts',(3.234732564,4.559170361,6.488374622));
#150966=CARTESIAN_POINT('',(2.82574891932962,4.69005394803157,6.947311917114));
#150967=CARTESIAN_POINT('Origin',(-0.0716030411419838,4.69642565541896,
-0.178781440042297));
#150968=CARTESIAN_POINT('',(2.66779578238773,4.690053949938,6.87450842694637));
#150969=CARTESIAN_POINT('Origin',(2.90566182226115E-13,4.75090401457722,
5.6768825751341E-13));
#150970=CARTESIAN_POINT('Origin',(-0.0500682004489761,4.55370333648812,
-0.180848118809921));
#150971=CARTESIAN_POINT('Origin',(-0.0979257211822305,4.69643083360533,
-0.16634588287032));
#150972=CARTESIAN_POINT('Ctrl Pts',(1.57568526880443,4.559162772,7.33315098855785));
#150973=CARTESIAN_POINT('Ctrl Pts',(1.97567011474391,4.624819703,7.24720563832325));
#150974=CARTESIAN_POINT('Ctrl Pts',(2.36393408427073,4.690053947,7.11826545851253));
#150975=CARTESIAN_POINT('Ctrl Pts',(2.37736254220013,4.69231013188933,7.11380594664459));
#150976=CARTESIAN_POINT('Ctrl Pts',(2.39079100012952,4.69456631677851,7.10934643477668));
#150977=CARTESIAN_POINT('Ctrl Pts',(1.755159165,4.559162772,7.03433837));
#150978=CARTESIAN_POINT('Ctrl Pts',(2.138845352,4.624819703,6.938603662));
#150979=CARTESIAN_POINT('Ctrl Pts',(2.509842609,4.690053947,6.801704939));
#150980=CARTESIAN_POINT('Ctrl Pts',(2.52267388217639,4.6923101318893,6.79697017377152));
#150981=CARTESIAN_POINT('Ctrl Pts',(2.53550515535279,4.69456631677871,6.79223540854287));
#150982=CARTESIAN_POINT('',(2.36423562309891,4.69005394784373,7.11761127437326));
#150983=CARTESIAN_POINT('',(2.43703911643164,4.69005394666591,6.9596580948236));
#150984=CARTESIAN_POINT('',(1.81988018749594,4.59933049940976,7.27585294663606));
#150985=CARTESIAN_POINT('Origin',(-0.0392903036502423,4.55358394247595,
-0.187394020872271));
#150986=CARTESIAN_POINT('Ctrl Pts',(1.7597361460689,4.55994605590214,7.03319478750165));
#150987=CARTESIAN_POINT('Ctrl Pts',(1.76970476263088,4.56683176240597,7.07358996400831));
#150988=CARTESIAN_POINT('Ctrl Pts',(1.77970782980979,4.57355155128323,7.11403045441226));
#150989=CARTESIAN_POINT('Ctrl Pts',(1.79975390958325,4.58666922564794,7.19490313097691));
#150990=CARTESIAN_POINT('Ctrl Pts',(1.80980814176314,4.59307444476964,7.23538056743884));
#150991=CARTESIAN_POINT('Ctrl Pts',(1.81988018914646,4.59933049939345,7.27585294610767));
#150992=CARTESIAN_POINT('Origin',(2.55438031837585E-12,4.78597145199022,
1.08931960673964E-11));
#150993=CARTESIAN_POINT('',(1.63621045854496,4.74999999914954,7.31934528063922));
#150994=CARTESIAN_POINT('',(1.81501009377767,4.78575691086147,7.24021154754731));
#150995=CARTESIAN_POINT('Origin',(-1.4466932228166,4.80792715097801,0.130176519892637));
#150996=CARTESIAN_POINT('',(2.00688844986046,4.75000000041905,7.22650665538518));
#150997=CARTESIAN_POINT('Origin',(0.,4.75,0.));
#150998=CARTESIAN_POINT('Origin',(1.41846174566267,5.02638723621362,-0.336296958183587));
#150999=CARTESIAN_POINT('Ctrl Pts',(1.266217779,4.690053947,7.392340126));
#151000=CARTESIAN_POINT('Ctrl Pts',(1.669423273,4.624398499,7.323275938));
#151001=CARTESIAN_POINT('Ctrl Pts',(2.062725117,4.559170361,7.210767303));
#151002=CARTESIAN_POINT('Ctrl Pts',(0.988998379,4.690053947,7.182226828));
#151003=CARTESIAN_POINT('Ctrl Pts',(1.380743519,4.624398499,7.128283209));
#151004=CARTESIAN_POINT('Ctrl Pts',(1.764297565,4.559170361,7.032051913));
#151005=CARTESIAN_POINT('',(1.26621777864668,4.69005394803159,7.39234011460805));
#151006=CARTESIAN_POINT('Origin',(-0.0314962915716327,4.69642567960048,
-0.189994239868742));
#151007=CARTESIAN_POINT('',(1.12760809690174,4.690053949938,7.28728347422995));
#151008=CARTESIAN_POINT('Origin',(1.29453739394769E-13,4.74999999999889,
3.15719672627779E-13));
#151009=CARTESIAN_POINT('Origin',(-0.0100209414025748,4.55370519417284,
-0.187383212253678));
#151010=CARTESIAN_POINT('Origin',(-0.0598759400814782,4.69643089876513,
-0.183505306097708));
#151011=CARTESIAN_POINT('Ctrl Pts',(-0.0375640731032268,4.559162772,7.50043175008717));
#151012=CARTESIAN_POINT('Ctrl Pts',(0.371545059331102,4.624819703,7.50248067270269));
#151013=CARTESIAN_POINT('Ctrl Pts',(0.778449959937463,4.690053947,7.46002031826955));
#151014=CARTESIAN_POINT('Ctrl Pts',(0.792523131473887,4.69231013193289,
7.45855178876658));
#151015=CARTESIAN_POINT('Ctrl Pts',(0.806596303010307,4.69456631686565,
7.45708325926374));
#151016=CARTESIAN_POINT('Ctrl Pts',(0.201949703,4.559162772,7.247186786));
#151017=CARTESIAN_POINT('Ctrl Pts',(0.597245653,4.624819703,7.236171492));
#151018=CARTESIAN_POINT('Ctrl Pts',(0.988998379000001,4.690053947,7.182226828));
#151019=CARTESIAN_POINT('Ctrl Pts',(1.00254749896548,4.69231013193286,7.1803611033336));
#151020=CARTESIAN_POINT('Ctrl Pts',(1.01609661893097,4.69456631686583,7.17849537866705));
#151021=CARTESIAN_POINT('',(0.778885079207504,4.69005394784374,7.45944625051968));
#151022=CARTESIAN_POINT('',(0.883941732031887,4.69005394666591,7.32083652775466));
#151023=CARTESIAN_POINT('',(0.213239089478733,4.59933049939522,7.49696799334096));
#151024=CARTESIAN_POINT('Origin',(0.00191245021496908,4.55358395884049,
-0.191459008319693));
#151025=CARTESIAN_POINT('Ctrl Pts',(0.206665513682815,4.5599460557616,7.24705385412779));
#151026=CARTESIAN_POINT('Ctrl Pts',(0.207717300597014,4.56683176215896,
7.28864757151797));
#151027=CARTESIAN_POINT('Ctrl Pts',(0.208792991606958,4.5735515511746,7.33029295061067));
#151028=CARTESIAN_POINT('Ctrl Pts',(0.210985170295593,4.58666922554127,
7.41358418388105));
#151029=CARTESIAN_POINT('Ctrl Pts',(0.21210288780751,4.5930744447238,7.45527664356005));
#151030=CARTESIAN_POINT('Ctrl Pts',(0.213239091294778,4.59933049939587,
7.49696799329137));
#151031=CARTESIAN_POINT('Origin',(1.09604369308812E-13,4.78597145199218,
9.84672413051335E-12));
#151032=CARTESIAN_POINT('',(0.0245138913552423,4.74999999914955,7.49995993786108));
#151033=CARTESIAN_POINT('',(0.216144702052854,4.78575691069572,7.46111294405876));
#151034=CARTESIAN_POINT('Origin',(-1.44085448015335,4.80792622602611,-0.183864222010178));
#151035=CARTESIAN_POINT('',(0.40648319694277,4.75000000032292,7.48897663920438));
#151036=CARTESIAN_POINT('Origin',(0.,4.75,0.));
#151037=CARTESIAN_POINT('Origin',(1.45759308339514,5.02638715698334,-0.0235092780933521));
#151038=CARTESIAN_POINT('Ctrl Pts',(-0.3525203,4.690053947,7.491710715));
#151039=CARTESIAN_POINT('Ctrl Pts',(0.056105233,4.624398499,7.510938472));
#151040=CARTESIAN_POINT('Ctrl Pts',(0.464397928,4.559170361,7.485608497));
#151041=CARTESIAN_POINT('Ctrl Pts',(-0.578090317,4.690053947,7.226915773));
#151042=CARTESIAN_POINT('Ctrl Pts',(-0.183907677,4.624398499,7.258446951));
#151043=CARTESIAN_POINT('Ctrl Pts',(0.211365974,4.559170361,7.246918271));
#151044=CARTESIAN_POINT('',(-0.352520297877153,4.69005394803158,7.49171070388639));
#151045=CARTESIAN_POINT('Origin',(0.0100832141964853,4.69642563255268,-0.192323046541649));
#151046=CARTESIAN_POINT('',(-0.465305290421314,4.690053949938,7.35931324514306));
#151047=CARTESIAN_POINT('Origin',(4.69730591229345E-14,4.74999999999911,
1.17961196366423E-13));
#151048=CARTESIAN_POINT('Origin',(0.0304952220692588,4.55370501744875,-0.185156493585492));
#151049=CARTESIAN_POINT('Origin',(-0.0190278903796856,4.69643087780134,
-0.192086882849298));
#151050=CARTESIAN_POINT('Ctrl Pts',(0.438256130634989,1.20239769764516,
7.48776619102291));
#151051=CARTESIAN_POINT('Ctrl Pts',(0.452324716730529,1.20018543582258,
7.48688969052746));
#151052=CARTESIAN_POINT('Ctrl Pts',(0.46639330282608,1.197973174,7.48601319003203));
#151053=CARTESIAN_POINT('Ctrl Pts',(0.874198775531821,1.13384644,7.4606061095738));
#151054=CARTESIAN_POINT('Ctrl Pts',(1.27683106164612,1.068610636,7.39104990055959));
#151055=CARTESIAN_POINT('Ctrl Pts',(0.185550148104057,1.20239769764516,
7.24767643469913));
#151056=CARTESIAN_POINT('Ctrl Pts',(0.199169321052031,1.20018543582258,
7.24727653784951));
#151057=CARTESIAN_POINT('Ctrl Pts',(0.212788494,1.197973174,7.246876641));
#151058=CARTESIAN_POINT('Ctrl Pts',(0.607566848,1.13384644,7.235284849));
#151059=CARTESIAN_POINT('Ctrl Pts',(0.998749843,1.068610636,7.180877297));
#151060=CARTESIAN_POINT('',(0.994070539475332,1.06939092015758,7.18152655971494));
#151061=CARTESIAN_POINT('Origin',(-0.0464232246320195,0.946547068832668,
-0.186800079907797));
#151062=CARTESIAN_POINT('Ctrl Pts',(1.03018392039921,1.1083007626151,7.4289111642017));
#151063=CARTESIAN_POINT('Ctrl Pts',(1.02426895890853,1.10211922686966,7.38762652912021));
#151064=CARTESIAN_POINT('Ctrl Pts',(1.01830226328052,1.09579054188193,7.34634686826034));
#151065=CARTESIAN_POINT('Ctrl Pts',(1.00603423691539,1.08257775698825,7.26228722585719));
#151066=CARTESIAN_POINT('Ctrl Pts',(0.999993344786955,1.07598455113782,
7.2214109573584));
#151067=CARTESIAN_POINT('Ctrl Pts',(0.994070540471644,1.06939092064321,
7.18152656222649));
#151068=CARTESIAN_POINT('Ctrl Pts',(0.779321499,1.068630405,7.45940064599999));
#151069=CARTESIAN_POINT('Ctrl Pts',(0.788211976,1.070029867,7.458471813));
#151070=CARTESIAN_POINT('Ctrl Pts',(0.797100213,1.071428571,7.45752179));
#151071=CARTESIAN_POINT('Ctrl Pts',(1.195462099,1.134117105,7.41494272));
#151072=CARTESIAN_POINT('Ctrl Pts',(1.587021072,1.197973174,7.330168082));
#151073=CARTESIAN_POINT('Ctrl Pts',(0.989418578,1.068630405,7.182168954));
#151074=CARTESIAN_POINT('Ctrl Pts',(0.997978637,1.070029867,7.18098971600001));
#151075=CARTESIAN_POINT('Ctrl Pts',(1.00653586,1.071428571,7.179790078));
#151076=CARTESIAN_POINT('Ctrl Pts',(1.390062022,1.134117105,7.126023487));
#151077=CARTESIAN_POINT('Ctrl Pts',(1.76567788,1.197973174,7.031705456));
#151078=CARTESIAN_POINT('Origin',(-0.0687907708237448,1.33885358158439,
-0.178199474963884));
#151079=CARTESIAN_POINT('Ctrl Pts',(2.03765834002557,1.20239769750531,7.21849426533476));
#151080=CARTESIAN_POINT('Ctrl Pts',(2.05120958830638,1.20018543575265,7.21461392687758));
#151081=CARTESIAN_POINT('Ctrl Pts',(2.06476083658723,1.197973174,7.21073358842053));
#151082=CARTESIAN_POINT('Ctrl Pts',(2.45757027373109,1.13384644,7.09825438844889));
#151083=CARTESIAN_POINT('Ctrl Pts',(2.83583671227409,1.068610636,6.94377032609197));
#151084=CARTESIAN_POINT('Ctrl Pts',(1.73924828446017,1.20239769750532,7.03834198997261));
#151085=CARTESIAN_POINT('Ctrl Pts',(1.75246308223009,1.20018543575264,7.03502372298625));
#151086=CARTESIAN_POINT('Ctrl Pts',(1.76567788,1.197973174,7.031705456));
#151087=CARTESIAN_POINT('Ctrl Pts',(2.148734641,1.13384644,6.935518997));
#151088=CARTESIAN_POINT('Ctrl Pts',(2.519075981,1.068610636,6.798290683));
#151089=CARTESIAN_POINT('',(2.5146456483084,1.06939092019803,6.79993067800517));
#151090=CARTESIAN_POINT('Origin',(-0.085494427019141,0.946547140040651,
-0.172453402570524));
#151091=CARTESIAN_POINT('Ctrl Pts',(2.60309509616357,1.10830076263949,7.03376825860774));
#151092=CARTESIAN_POINT('Ctrl Pts',(2.58844344688322,1.10211922687875,6.99472037711221));
#151093=CARTESIAN_POINT('Ctrl Pts',(2.57374234231561,1.09579054188358,6.95568847492214));
#151094=CARTESIAN_POINT('Ctrl Pts',(2.54369085516861,1.08257778252019,6.87623151676588));
#151095=CARTESIAN_POINT('Ctrl Pts',(2.52900400578861,1.07598457750415,6.83760952313978));
#151096=CARTESIAN_POINT('Ctrl Pts',(2.5146456500351,1.06939092077411,6.79993068076175));
#151097=CARTESIAN_POINT('Ctrl Pts',(2.364652037,1.068630405,7.117472919));
#151098=CARTESIAN_POINT('Ctrl Pts',(2.373134987,1.070029867,7.114654611));
#151099=CARTESIAN_POINT('Ctrl Pts',(2.381611195,1.071428571,7.111816091));
#151100=CARTESIAN_POINT('Ctrl Pts',(2.76150636,1.134117105,6.984596466));
#151101=CARTESIAN_POINT('Ctrl Pts',(3.125686861,1.197973174,6.817630208));
#151102=CARTESIAN_POINT('Ctrl Pts',(2.510240543,1.068630405,6.801558087));
#151103=CARTESIAN_POINT('Ctrl Pts',(2.518346971,1.070029867,6.79856626));
#151104=CARTESIAN_POINT('Ctrl Pts',(2.526446244,1.071428571,6.795555119));
#151105=CARTESIAN_POINT('Ctrl Pts',(2.88944755,1.134117105,6.660598773));
#151106=CARTESIAN_POINT('Ctrl Pts',(3.236006129,1.197973174,6.487739539));
#151107=CARTESIAN_POINT('Origin',(-0.105490039867763,1.33885356374272,-0.15924516305883));
#151108=CARTESIAN_POINT('Ctrl Pts',(3.54178191010228,1.20239769752864,6.61169357039341));
#151109=CARTESIAN_POINT('Ctrl Pts',(3.55418217973039,1.20018543576431,6.60499083425077));
#151110=CARTESIAN_POINT('Ctrl Pts',(3.5665824493585,1.197973174,6.59828809810826));
#151111=CARTESIAN_POINT('Ctrl Pts',(3.9260285170885,1.13384644,6.4039961817453));
#151112=CARTESIAN_POINT('Ctrl Pts',(4.26224178946224,1.068610636,6.17180776755949));
#151113=CARTESIAN_POINT('Ctrl Pts',(3.2116211011738,1.20239769752864,6.49990249637725));
#151114=CARTESIAN_POINT('Ctrl Pts',(3.2238136150869,1.20018543576431,6.49382101768858));
#151115=CARTESIAN_POINT('Ctrl Pts',(3.236006129,1.197973174,6.487739539));
#151116=CARTESIAN_POINT('Ctrl Pts',(3.589429991,1.13384644,6.311455985));
#151117=CARTESIAN_POINT('Ctrl Pts',(3.921612925,1.068610636,6.097823552));
#151118=CARTESIAN_POINT('',(3.91763872170611,1.06939092016878,6.10037759559883));
#151119=CARTESIAN_POINT('Origin',(-0.120568015468822,0.946547110816421,
-0.150042782148584));
#151120=CARTESIAN_POINT('Ctrl Pts',(4.05428843853725,1.10830076263012,6.30973416640618));
#151121=CARTESIAN_POINT('Ctrl Pts',(4.03158519654434,1.10211922687914,6.27474887425661));
#151122=CARTESIAN_POINT('Ctrl Pts',(4.00883709045277,1.09579054186242,6.23978981908073));
#151123=CARTESIAN_POINT('Ctrl Pts',(3.96240709072474,1.08257772486597,6.16865039166828));
#151124=CARTESIAN_POINT('Ctrl Pts',(3.93976101702381,1.07598451458819,6.13408858623298));
#151125=CARTESIAN_POINT('Ctrl Pts',(3.91763872389687,1.06939092074616,6.10037759762989));
#151126=CARTESIAN_POINT('Ctrl Pts',(3.839414072,1.068630405,6.442740068));
#151127=CARTESIAN_POINT('Ctrl Pts',(3.847092844,1.070029867,6.438164067));
#151128=CARTESIAN_POINT('Ctrl Pts',(3.854760685,1.071428571,6.433569776));
#151129=CARTESIAN_POINT('Ctrl Pts',(4.198425653,1.134117105,6.227658244));
#151130=CARTESIAN_POINT('Ctrl Pts',(4.518199006,1.197973174,5.986307521));
#151131=CARTESIAN_POINT('Ctrl Pts',(3.91368645,1.068630405,6.10291392400001));
#151132=CARTESIAN_POINT('Ctrl Pts',(3.9209602,1.070029867,6.09824940200001));
#151133=CARTESIAN_POINT('Ctrl Pts',(3.928222811,1.071428571,6.093567555));
#151134=CARTESIAN_POINT('Ctrl Pts',(4.253725723,1.134117105,5.883731863));
#151135=CARTESIAN_POINT('Ctrl Pts',(4.555022329,1.197973174,5.640414132));
#151136=CARTESIAN_POINT('Origin',(-0.137256662328351,1.33885360303372,-0.132844741481347));
#151137=CARTESIAN_POINT('Ctrl Pts',(4.88029569482903,1.20239769749146,5.69573743188663));
#151138=CARTESIAN_POINT('Ctrl Pts',(4.89096516280296,1.20018543574573,5.68652571066418));
#151139=CARTESIAN_POINT('Ctrl Pts',(4.90163463077696,1.197973174,5.67731398944164));
#151140=CARTESIAN_POINT('Ctrl Pts',(5.21091003004155,1.13384644,5.41029423119707));
#151141=CARTESIAN_POINT('Ctrl Pts',(5.48934917737148,1.068610636,5.11125833880414));
#151142=CARTESIAN_POINT('Ctrl Pts',(4.53382208607388,1.20239769749146,5.65753478623849));
#151143=CARTESIAN_POINT('Ctrl Pts',(4.54442220753694,1.20018543574573,5.64897445911926));
#151144=CARTESIAN_POINT('Ctrl Pts',(4.555022329,1.197973174,5.640414132));
#151145=CARTESIAN_POINT('Ctrl Pts',(4.862287584,1.13384644,5.392276306));
#151146=CARTESIAN_POINT('Ctrl Pts',(5.140779607,1.068610636,5.112228969));
#151147=CARTESIAN_POINT('',(5.137447362684,1.06939092021347,5.11557763715341));
#151148=CARTESIAN_POINT('Origin',(-0.150003984783348,0.946547102134927,
-0.120616314865802));
#151149=CARTESIAN_POINT('Ctrl Pts',(5.31590775884627,1.10830076261777,5.290663917931));
#151150=CARTESIAN_POINT('Ctrl Pts',(5.28621450234346,1.10211922685411,5.26137708832615));
#151151=CARTESIAN_POINT('Ctrl Pts',(5.25648307089843,1.09579054184443,5.23212552680139));
#151152=CARTESIAN_POINT('Ctrl Pts',(5.1958457848372,1.08257774230565,5.17263045558175));
#151153=CARTESIAN_POINT('Ctrl Pts',(5.16629941641204,1.07598453760999,5.14374494207106));
#151154=CARTESIAN_POINT('Ctrl Pts',(5.13744736516035,1.06939092066855,5.11557763789017));
#151155=CARTESIAN_POINT('Ctrl Pts',(5.134649374,1.068630405,5.466751852));
#151156=CARTESIAN_POINT('Ctrl Pts',(5.141164914,1.070029867,5.460632127));
#151157=CARTESIAN_POINT('Ctrl Pts',(5.147665849,1.071428571,5.454496888));
#151158=CARTESIAN_POINT('Ctrl Pts',(5.439031228,1.134117105,5.179521645));
#151159=CARTESIAN_POINT('Ctrl Pts',(5.69944518700001,1.197973174,4.875071749));
#151160=CARTESIAN_POINT('Ctrl Pts',(5.134132729,1.068630405,5.118904289));
#151161=CARTESIAN_POINT('Ctrl Pts',(5.140233688,1.070029867,5.11278518));
#151162=CARTESIAN_POINT('Ctrl Pts',(5.146320044,1.071428571,5.106651545));
#151163=CARTESIAN_POINT('Ctrl Pts',(5.419104408,1.134117105,4.831748191));
#151164=CARTESIAN_POINT('Ctrl Pts',(5.661050747,1.197973174,4.529349229));
#151165=CARTESIAN_POINT('Ctrl Pts',(5.13412756255,1.068630405,5.11542581337));
#151166=CARTESIAN_POINT('Ctrl Pts',(5.14022437574001,1.070029867,5.10930671053001));
#151167=CARTESIAN_POINT('Ctrl Pts',(5.14630658595,1.071428571,5.10317309157));
#151168=CARTESIAN_POINT('Ctrl Pts',(5.4189051398,1.134117105,4.82827045646));
#151169=CARTESIAN_POINT('Ctrl Pts',(5.6606668026,1.197973174,4.5258920038));
#151170=CARTESIAN_POINT('Origin',(-0.162605461207993,1.33885360462888,-0.100232851893934));
#151171=CARTESIAN_POINT('Ctrl Pts',(6.00190831268338,1.19924836941368,4.49746179671395));
#151172=CARTESIAN_POINT('Ctrl Pts',(6.00434078984169,1.19861077170684,4.49420829285698));
#151173=CARTESIAN_POINT('Ctrl Pts',(6.006773267,1.197973174,4.490954789));
#151174=CARTESIAN_POINT('Ctrl Pts',(6.251420972,1.13384644,4.16373188));
#151175=CARTESIAN_POINT('Ctrl Pts',(6.459075062,1.068610636,3.811869534));
#151176=CARTESIAN_POINT('Ctrl Pts',(5.6561442008214,1.19924836941368,4.53548172299217));
#151177=CARTESIAN_POINT('Ctrl Pts',(5.6585974739107,1.19861077170684,4.53241547599609));
#151178=CARTESIAN_POINT('Ctrl Pts',(5.661050747,1.197973174,4.529349229));
#151179=CARTESIAN_POINT('Ctrl Pts',(5.907790014,1.13384644,4.22095978));
#151180=CARTESIAN_POINT('Ctrl Pts',(6.119569149,1.068610636,3.887592241));
#151181=CARTESIAN_POINT('',(6.11703467512529,1.06939092025812,3.89157895330992));
#151182=CARTESIAN_POINT('Origin',(-0.172425869117308,0.946547096142826,
-0.0855499160264561));
#151183=CARTESIAN_POINT('Ctrl Pts',(6.32896114107968,1.10830076259861,4.02420810481511));
#151184=CARTESIAN_POINT('Ctrl Pts',(6.29366629386755,1.10211922687242,4.00198915746824));
#151185=CARTESIAN_POINT('Ctrl Pts',(6.25834174588014,1.09579054191023,3.97981286015405));
#151186=CARTESIAN_POINT('Ctrl Pts',(6.18633291489277,1.08257782875722,3.93474426913298));
#151187=CARTESIAN_POINT('Ctrl Pts',(6.15126776956136,1.07598462355285,3.91288566099629));
#151188=CARTESIAN_POINT('Ctrl Pts',(6.11703467769023,1.06939092074784,3.89157895377656));
#151189=CARTESIAN_POINT('Ctrl Pts',(6.189794177,1.068630405,4.235144395));
#151190=CARTESIAN_POINT('Ctrl Pts',(6.194841828,1.070029867,4.227767098));
#151191=CARTESIAN_POINT('Ctrl Pts',(6.199871879,1.071428571,4.220377789));
#151192=CARTESIAN_POINT('Ctrl Pts',(6.425313749,1.134117105,3.889196369));
#151193=CARTESIAN_POINT('Ctrl Pts',(6.614191646,1.197973174,3.53588304));
#151194=CARTESIAN_POINT('Ctrl Pts',(6.114512667,1.068630405,3.895540379));
#151195=CARTESIAN_POINT('Ctrl Pts',(6.119155562,1.070029867,3.888252805));
#151196=CARTESIAN_POINT('Ctrl Pts',(6.123781072,1.071428571,3.880954185));
#151197=CARTESIAN_POINT('Ctrl Pts',(6.331091794,1.134117105,3.553837343));
#151198=CARTESIAN_POINT('Ctrl Pts',(6.502374724,1.197973174,3.20649699));
#151199=CARTESIAN_POINT('Ctrl Pts',(6.11375985189999,1.068630405,3.89214433884));
#151200=CARTESIAN_POINT('Ctrl Pts',(6.11839869934,1.070029867,3.88485766207));
#151201=CARTESIAN_POINT('Ctrl Pts',(6.12302016393,1.071428571,3.87755994896));
#151202=CARTESIAN_POINT('Ctrl Pts',(6.33014957445,1.134117105,3.55048375274));
#151203=CARTESIAN_POINT('Ctrl Pts',(6.50125655478,1.197973174,3.2032031295));
#151204=CARTESIAN_POINT('Origin',(-0.180351123912226,1.33885356480351,-0.0629342094144608));
#151205=CARTESIAN_POINT('Ctrl Pts',(6.82840837392086,1.19924836941368,3.10208076685929));
#151206=CARTESIAN_POINT('Ctrl Pts',(6.83008457396043,1.19861077170684,3.09838041742964));
#151207=CARTESIAN_POINT('Ctrl Pts',(6.83176077400001,1.197973174,3.094680068));
#151208=CARTESIAN_POINT('Ctrl Pts',(7.000345499,1.13384644,2.722515424));
#151209=CARTESIAN_POINT('Ctrl Pts',(7.127504748,1.068610636,2.334239933));
#151210=CARTESIAN_POINT('Ctrl Pts',(6.4989011950665,1.19924836941368,3.21354087208441));
#151211=CARTESIAN_POINT('Ctrl Pts',(6.50063795953325,1.19861077170684,3.2100189310422));
#151212=CARTESIAN_POINT('Ctrl Pts',(6.50237472400001,1.197973174,3.20649699));
#151213=CARTESIAN_POINT('Ctrl Pts',(6.677050749,1.13384644,2.852275866));
#151214=CARTESIAN_POINT('Ctrl Pts',(6.812214438,1.068610636,2.481176021));
#151215=CARTESIAN_POINT('',(6.81059624420825,1.06939092016605,2.48561436300061));
#151216=CARTESIAN_POINT('Origin',(-0.186785148316005,0.946547087643834,
-0.0464832497890674));
#151217=CARTESIAN_POINT('Ctrl Pts',(7.04607933419032,1.1083007625848,2.56958479291152));
#151218=CARTESIAN_POINT('Ctrl Pts',(7.00683324387316,1.10211922682975,2.55547266099491));
#151219=CARTESIAN_POINT('Ctrl Pts',(6.96756731588649,1.09579054187649,2.54140856685189));
#151220=CARTESIAN_POINT('Ctrl Pts',(6.88755313081598,1.08257775182071,2.5128732584833));
#151221=CARTESIAN_POINT('Ctrl Pts',(6.84860885007912,1.07598454567715,2.49906367012202));
#151222=CARTESIAN_POINT('Ctrl Pts',(6.81059624670237,1.06939092071402,2.48561436286733));
#151223=CARTESIAN_POINT('Ctrl Pts',(6.955511084,1.068630405,2.805506294));
#151224=CARTESIAN_POINT('Ctrl Pts',(6.958854823,1.070029867,2.797216377));
#151225=CARTESIAN_POINT('Ctrl Pts',(6.962178791,1.071428571,2.788918514));
#151226=CARTESIAN_POINT('Ctrl Pts',(7.11115573900001,1.134117105,2.417016594));
#151227=CARTESIAN_POINT('Ctrl Pts',(7.219665854,1.197973174,2.031360369));
#151228=CARTESIAN_POINT('Ctrl Pts',(6.808984789,1.068630405,2.49002533));
#151229=CARTESIAN_POINT('Ctrl Pts',(6.811952522,1.070029867,2.48191005));
#151230=CARTESIAN_POINT('Ctrl Pts',(6.814900903,1.071428571,2.47378772));
#151231=CARTESIAN_POINT('Ctrl Pts',(6.947044364,1.134117105,2.109753011));
#151232=CARTESIAN_POINT('Ctrl Pts',(7.039654886,1.197973174,1.733712515));
#151233=CARTESIAN_POINT('Origin',(-0.189663442092307,1.33885358139159,-0.0226926323759727));
#151234=CARTESIAN_POINT('Ctrl Pts',(7.33208299134599,1.20239769762439,1.5809079574551));
#151235=CARTESIAN_POINT('Ctrl Pts',(7.33500218475563,1.20018543581218,1.56711768275349));
#151236=CARTESIAN_POINT('Ctrl Pts',(7.33792137816545,1.197973174,1.55332740805189));
#151237=CARTESIAN_POINT('Ctrl Pts',(7.422539906702,1.13384644,1.15358933333221));
#151238=CARTESIAN_POINT('Ctrl Pts',(7.46323456897324,1.068610636,0.747024740058699));
#151239=CARTESIAN_POINT('Ctrl Pts',(7.03313849789318,1.20239769762439,1.76017199027748));
#151240=CARTESIAN_POINT('Ctrl Pts',(7.03639669194659,1.20018543581218,1.74694225263871));
#151241=CARTESIAN_POINT('Ctrl Pts',(7.039654886,1.197973174,1.733712515));
#151242=CARTESIAN_POINT('Ctrl Pts',(7.134100011,1.13384644,1.350222703));
#151243=CARTESIAN_POINT('Ctrl Pts',(7.186328152,1.068610636,0.958742768));
#151244=CARTESIAN_POINT('',(7.18570190259806,1.06939092016506,0.96342520766622));
#151245=CARTESIAN_POINT('Origin',(-0.192410959439872,0.94654712134076,-0.00524326309847709));
#151246=CARTESIAN_POINT('Ctrl Pts',(7.43373068926975,1.10830076258783,0.994810551909359));
#151247=CARTESIAN_POINT('Ctrl Pts',(7.39236845954229,1.10211922682979,0.989465103128043));
#151248=CARTESIAN_POINT('Ctrl Pts',(7.35099718228751,1.09579054181713,0.984170833502873));
#151249=CARTESIAN_POINT('Ctrl Pts',(7.26671952059379,1.08257776491292,0.973503360110995));
#151250=CARTESIAN_POINT('Ctrl Pts',(7.22571707860721,1.07598455880364,0.968388500652465));
#151251=CARTESIAN_POINT('Ctrl Pts',(7.18570190540487,1.06939092071891,0.963425207231068));
#151252=CARTESIAN_POINT('Ctrl Pts',(7.395996023,1.068630405,1.244685836));
#151253=CARTESIAN_POINT('Ctrl Pts',(7.3974795,1.070029867,1.235870928));
#151254=CARTESIAN_POINT('Ctrl Pts',(7.398941961,1.071428571,1.227052509));
#151255=CARTESIAN_POINT('Ctrl Pts',(7.464487991,1.134117105,0.83181981));
#151256=CARTESIAN_POINT('Ctrl Pts',(7.487556512,1.197973174,0.431853546));
#151257=CARTESIAN_POINT('Ctrl Pts',(7.18507635,1.068630405,0.968079464));
#151258=CARTESIAN_POINT('Ctrl Pts',(7.186230154,1.070029867,0.95951594));
#151259=CARTESIAN_POINT('Ctrl Pts',(7.187363542,1.071428571,0.95094969));
#151260=CARTESIAN_POINT('Ctrl Pts',(7.238160861,1.134117105,0.567018973000001));
#151261=CARTESIAN_POINT('Ctrl Pts',(7.247768609,1.197973174,0.17986157));
#151262=CARTESIAN_POINT('Origin',(-0.19010752046501,1.33885360244533,0.0186099469742334));
#151263=CARTESIAN_POINT('Ctrl Pts',(7.50051144518414,1.20239769728923,-0.032233902738517));
#151264=CARTESIAN_POINT('Ctrl Pts',(7.50039788805664,1.2001854356446,-0.0463293077195174));
#151265=CARTESIAN_POINT('Ctrl Pts',(7.50028433092912,1.197973174,-0.0604247127005174));
#151266=CARTESIAN_POINT('Ctrl Pts',(7.49699265531406,1.13384644,-0.469007616103169));
#151267=CARTESIAN_POINT('Ctrl Pts',(7.44933652902291,1.068610636,-0.87481510443479));
#151268=CARTESIAN_POINT('Ctrl Pts',(7.24709257550854,1.20239769728923,0.207103266246919));
#151269=CARTESIAN_POINT('Ctrl Pts',(7.24743059225433,1.2001854356446,0.193482418123463));
#151270=CARTESIAN_POINT('Ctrl Pts',(7.247768609,1.197973174,0.17986157));
#151271=CARTESIAN_POINT('Ctrl Pts',(7.257566686,1.13384644,-0.214965374));
#151272=CARTESIAN_POINT('Ctrl Pts',(7.224417148,1.068610636,-0.608520231));
#151273=CARTESIAN_POINT('',(7.22481212632975,1.06939092020671,-0.603812639258374));
#151274=CARTESIAN_POINT('Origin',(-0.189039560576042,0.946547077688595,
0.0362419940864935));
#151275=CARTESIAN_POINT('Ctrl Pts',(7.47378905908849,1.10830076262173,-0.626479925186409));
#151276=CARTESIAN_POINT('Ctrl Pts',(7.43224474213266,1.10211922691993,-0.622808743525731));
#151277=CARTESIAN_POINT('Ctrl Pts',(7.39070259099799,1.0957905419375,-0.61908563424013));
#151278=CARTESIAN_POINT('Ctrl Pts',(7.30610202034383,1.08257775218037,-0.611386494120737));
#151279=CARTESIAN_POINT('Ctrl Pts',(7.26495866855718,1.07598454873877,-0.607567458552055));
#151280=CARTESIAN_POINT('Ctrl Pts',(7.22481212871226,1.06939092068975,-0.603812640279786));
#151281=CARTESIAN_POINT('Ctrl Pts',(7.49065240800001,1.068630405,-0.374334748));
#151282=CARTESIAN_POINT('Ctrl Pts',(7.490206258,1.070029867,-0.383262472));
#151283=CARTESIAN_POINT('Ctrl Pts',(7.489738828,1.071428571,-0.392189107));
#151284=CARTESIAN_POINT('Ctrl Pts',(7.468789081,1.134117105,-0.792271945));
#151285=CARTESIAN_POINT('Ctrl Pts',(7.405337348,1.197973174,-1.187846269));
#151286=CARTESIAN_POINT('Ctrl Pts',(7.225201726,1.068630405,-0.599132722));
#151287=CARTESIAN_POINT('Ctrl Pts',(7.22448765000001,1.070029867,-0.607744069));
#151288=CARTESIAN_POINT('Ctrl Pts',(7.22375305,1.071428571,-0.616353689));
#151289=CARTESIAN_POINT('Ctrl Pts',(7.190829,1.134117105,-1.002228242));
#151290=CARTESIAN_POINT('Ctrl Pts',(7.116984728,1.197973174,-1.382399502));
#151291=CARTESIAN_POINT('Origin',(-0.181662547489728,1.33885359185878,0.0590423750210464));
#151292=CARTESIAN_POINT('Ctrl Pts',(7.31822431973493,1.20239769767987,-1.64386853669405));
#151293=CARTESIAN_POINT('Ctrl Pts',(7.31508332183255,1.20018543583992,-1.65760998871918));
#151294=CARTESIAN_POINT('Ctrl Pts',(7.31194232393021,1.197973174,-1.67135144074435));
#151295=CARTESIAN_POINT('Ctrl Pts',(7.22089435965082,1.13384644,-2.06967428973483));
#151296=CARTESIAN_POINT('Ctrl Pts',(7.08711579269105,1.068610636,-2.45574956582236));
#151297=CARTESIAN_POINT('Ctrl Pts',(7.12218065971982,1.20239769767987,-1.35564937192039));
#151298=CARTESIAN_POINT('Ctrl Pts',(7.11958269385989,1.20018543583992,-1.36902443696019));
#151299=CARTESIAN_POINT('Ctrl Pts',(7.116984728,1.197973174,-1.382399502));
#151300=CARTESIAN_POINT('Ctrl Pts',(7.041677609,1.13384644,-1.770101908));
#151301=CARTESIAN_POINT('Ctrl Pts',(6.92470042800001,1.068610636,-2.147329501));
#151302=CARTESIAN_POINT('',(6.92609816488622,1.06939092015861,-2.14281687848));
#151303=CARTESIAN_POINT('Origin',(-0.176829096809142,0.94654709502762,0.0760326273958178));
#151304=CARTESIAN_POINT('Ctrl Pts',(7.16438135887105,1.1083007626294,-2.2184768961222));
#151305=CARTESIAN_POINT('Ctrl Pts',(7.12459752024626,1.10211922688055,-2.20596074454325));
#151306=CARTESIAN_POINT('Ctrl Pts',(7.08482695982546,1.09579054186779,-2.19339434504393));
#151307=CARTESIAN_POINT('Ctrl Pts',(7.00385935976641,1.08257774698776,-2.16768857502555));
#151308=CARTESIAN_POINT('Ctrl Pts',(6.96449889675582,1.07598454333095,-2.15511422210605));
#151309=CARTESIAN_POINT('Ctrl Pts',(6.92609816709728,1.06939092067094,-2.14281688041309));
#151310=CARTESIAN_POINT('Ctrl Pts',(7.235054212,1.068630405,-1.975851855));
#151311=CARTESIAN_POINT('Ctrl Pts',(7.232699295,1.070029867,-1.984474945));
#151312=CARTESIAN_POINT('Ctrl Pts',(7.230323831,1.071428571,-1.993092396));
#151313=CARTESIAN_POINT('Ctrl Pts',(7.123857894,1.134117105,-2.379317943));
#151314=CARTESIAN_POINT('Ctrl Pts',(6.976852841,1.197973174,-2.752003713));
#151315=CARTESIAN_POINT('Ctrl Pts',(6.92748470000001,1.068630405,-2.138330128));
#151316=CARTESIAN_POINT('Ctrl Pts',(6.924936134,1.070029867,-2.146586641));
#151317=CARTESIAN_POINT('Ctrl Pts',(6.922367894,1.071428571,-2.154837056));
#151318=CARTESIAN_POINT('Ctrl Pts',(6.807261968,1.134117105,-2.524612378));
#151319=CARTESIAN_POINT('Ctrl Pts',(6.65341854999999,1.197973174,-2.88002111));
#151320=CARTESIAN_POINT('Origin',(-0.164722993209007,1.3388535646555,0.096714071594971));
#151321=CARTESIAN_POINT('Ctrl Pts',(6.79374515911296,1.20239769751311,-3.17863770865075));
#151322=CARTESIAN_POINT('Ctrl Pts',(6.78772359020847,1.20018543575654,-3.19138267096105));
#151323=CARTESIAN_POINT('Ctrl Pts',(6.78170202130389,1.197973174,-3.20412763327128));
#151324=CARTESIAN_POINT('Ctrl Pts',(6.60715506895362,1.13384644,-3.57356529384211));
#151325=CARTESIAN_POINT('Ctrl Pts',(6.39350939878208,1.068610636,-3.92185590761168));
#151326=CARTESIAN_POINT('Ctrl Pts',(6.66424349046516,1.20239769751311,-2.85501335574557));
#151327=CARTESIAN_POINT('Ctrl Pts',(6.65883102023257,1.20018543575654,-2.86751723287278));
#151328=CARTESIAN_POINT('Ctrl Pts',(6.65341855,1.197973174,-2.88002111));
#151329=CARTESIAN_POINT('Ctrl Pts',(6.49652751400001,1.13384644,-3.242470445));
#151330=CARTESIAN_POINT('Ctrl Pts',(6.301192412,1.068610636,-3.58573203));
#151331=CARTESIAN_POINT('',(6.30352755149462,1.06939092016514,-3.58162538195189));
#151332=CARTESIAN_POINT('Origin',(-0.156349827179958,0.946547120519208,
0.112267878198516));
#151333=CARTESIAN_POINT('Ctrl Pts',(6.51997514917062,1.10830076264153,-3.70674035357318));
#151334=CARTESIAN_POINT('Ctrl Pts',(6.48381203713835,1.10211922687683,-3.68596447338293));
#151335=CARTESIAN_POINT('Ctrl Pts',(6.44767269474452,1.09579054185558,-3.66514237449989));
#151336=CARTESIAN_POINT('Ctrl Pts',(6.37412364238196,1.08257767322355,-3.62263171337973));
#151337=CARTESIAN_POINT('Ctrl Pts',(6.33838650802529,1.07598446349883,-3.60188999851072));
#151338=CARTESIAN_POINT('Ctrl Pts',(6.30352755295668,1.06939092073101,-3.58162538425232));
#151339=CARTESIAN_POINT('Ctrl Pts',(6.641152922,1.068630405,-3.484980325));
#151340=CARTESIAN_POINT('Ctrl Pts',(6.636999353,1.070029867,-3.492895575));
#151341=CARTESIAN_POINT('Ctrl Pts',(6.632826928,1.071428571,-3.5008009));
#151342=CARTESIAN_POINT('Ctrl Pts',(6.44582303,1.134117105,-3.855109679));
#151343=CARTESIAN_POINT('Ctrl Pts',(6.222138449,1.197973174,-4.187480522));
#151344=CARTESIAN_POINT('Ctrl Pts',(6.30584618800001,1.068630405,-3.577541593));
#151345=CARTESIAN_POINT('Ctrl Pts',(6.3015823,1.070029867,-3.585057207));
#151346=CARTESIAN_POINT('Ctrl Pts',(6.297300509,1.071428571,-3.592562637));
#151347=CARTESIAN_POINT('Ctrl Pts',(6.105394932,1.134117105,-3.928948446));
#151348=CARTESIAN_POINT('Ctrl Pts',(5.878745916,1.197973174,-4.242976131));
#151349=CARTESIAN_POINT('Origin',(-0.14008082696896,1.33885358682711,0.129863289500041));
#151350=CARTESIAN_POINT('Ctrl Pts',(5.95159802469212,1.20239769753535,-4.56477731310792));
#151351=CARTESIAN_POINT('Ctrl Pts',(5.94297744652179,1.20018543576767,-4.57592984602739));
#151352=CARTESIAN_POINT('Ctrl Pts',(5.93435686835148,1.197973174,-4.58708237894685));
#151353=CARTESIAN_POINT('Ctrl Pts',(5.68447255026051,1.13384644,-4.91036035735012));
#151354=CARTESIAN_POINT('Ctrl Pts',(5.40094961069062,1.068610636,-5.20458062606933));
#151355=CARTESIAN_POINT('Ctrl Pts',(5.89469370340292,1.20239769753535,-4.22088008624134));
#151356=CARTESIAN_POINT('Ctrl Pts',(5.88671980970153,1.20018543576767,-4.23192810862066));
#151357=CARTESIAN_POINT('Ctrl Pts',(5.878745916,1.197973174,-4.242976131));
#151358=CARTESIAN_POINT('Ctrl Pts',(5.647607012,1.13384644,-4.563224667));
#151359=CARTESIAN_POINT('Ctrl Pts',(5.383047642,1.068610636,-4.85646971400001));
#151360=CARTESIAN_POINT('',(5.38621099464516,1.06939092021984,-4.85296106368719));
#151361=CARTESIAN_POINT('Origin',(-0.128560173579613,0.946547117492585,
0.143253706418039));
#151362=CARTESIAN_POINT('Ctrl Pts',(5.570702147441,1.10830076265064,-5.02168075233264));
#151363=CARTESIAN_POINT('Ctrl Pts',(5.5398507091389,1.10211922690085,-4.99361660052245));
#151364=CARTESIAN_POINT('Ctrl Pts',(5.50903242037416,1.09579054189062,-4.96551242031142));
#151365=CARTESIAN_POINT('Ctrl Pts',(5.44634166949059,1.0825777217037,-4.90818497254084));
#151366=CARTESIAN_POINT('Ctrl Pts',(5.41589892140718,1.07598451821939,-4.88024577480333));
#151367=CARTESIAN_POINT('Ctrl Pts',(5.38621099577857,1.06939092065068,-4.85296106598922));
#151368=CARTESIAN_POINT('Ctrl Pts',(5.736718702,1.068630405,-4.831154989));
#151369=CARTESIAN_POINT('Ctrl Pts',(5.730960697,1.070029867,-4.83799229));
#151370=CARTESIAN_POINT('Ctrl Pts',(5.72518641,1.071428571,-4.844815845));
#151371=CARTESIAN_POINT('Ctrl Pts',(5.46638864400001,1.134117105,-5.150640772));
#151372=CARTESIAN_POINT('Ctrl Pts',(5.176483778,1.197973174,-5.427155396));
#151373=CARTESIAN_POINT('Ctrl Pts',(5.38935331700001,1.068630405,-4.84947119));
#151374=CARTESIAN_POINT('Ctrl Pts',(5.383573482,1.070029867,-4.855894483));
#151375=CARTESIAN_POINT('Ctrl Pts',(5.377778351,1.071428571,-4.862303981));
#151376=CARTESIAN_POINT('Ctrl Pts',(5.118046414,1.134117105,-5.149571251));
#151377=CARTESIAN_POINT('Ctrl Pts',(4.829189657,1.197973174,-5.407534305));
#151378=CARTESIAN_POINT('Ctrl Pts',(5.38587966315001,1.068630405,-4.84965435201));
#151379=CARTESIAN_POINT('Ctrl Pts',(5.38009960985,1.070029867,-4.85607350493001));
#151380=CARTESIAN_POINT('Ctrl Pts',(5.37430427041,1.071428571,-4.86247886236));
#151381=CARTESIAN_POINT('Ctrl Pts',(5.1145629917,1.134117105,-5.14956055579));
#151382=CARTESIAN_POINT('Ctrl Pts',(4.82571671579,1.197973174,-5.40733809408999));
#151383=CARTESIAN_POINT('Origin',(-0.108889318598229,1.33885360151785,0.156940670213082));
#151384=CARTESIAN_POINT('Ctrl Pts',(4.83116078180512,1.20239769737794,-5.7374730039056));
#151385=CARTESIAN_POINT('Ctrl Pts',(4.82034428343836,1.20018543568896,-5.74651162701026));
#151386=CARTESIAN_POINT('Ctrl Pts',(4.80952778507171,1.197973174,-5.75555025011497));
#151387=CARTESIAN_POINT('Ctrl Pts',(4.49599041422966,1.13384644,-6.01755242754882));
#151388=CARTESIAN_POINT('Ctrl Pts',(4.15584742240734,1.068610636,-6.24394493863673));
#151389=CARTESIAN_POINT('Ctrl Pts',(4.84951458976677,1.20239769737794,-5.38938315709937));
#151390=CARTESIAN_POINT('Ctrl Pts',(4.83935212338343,1.20018543568896,-5.39845873104967));
#151391=CARTESIAN_POINT('Ctrl Pts',(4.829189657,1.197973174,-5.40753430500001));
#151392=CARTESIAN_POINT('Ctrl Pts',(4.53461068300001,1.13384644,-5.670607575));
#151393=CARTESIAN_POINT('Ctrl Pts',(4.213197547,1.068610636,-5.900124272));
#151394=CARTESIAN_POINT('',(4.21704119835776,1.0693909201585,-5.89737767934635));
#151395=CARTESIAN_POINT('Origin',(-0.0947593468883695,0.946547132636281,
0.167541350843304));
#151396=CARTESIAN_POINT('Ctrl Pts',(4.36094930547041,1.10830076259365,-6.10181293976727));
#151397=CARTESIAN_POINT('Ctrl Pts',(4.33685211954456,1.10211922683968,-6.06777276493754));
#151398=CARTESIAN_POINT('Ctrl Pts',(4.31279591317227,1.09579054185722,-6.03370062390097));
#151399=CARTESIAN_POINT('Ctrl Pts',(4.26389471363875,1.08257776763097,-5.96423704338925));
#151400=CARTESIAN_POINT('Ctrl Pts',(4.24016977757793,1.07598455995295,-5.93040672750791));
#151401=CARTESIAN_POINT('Ctrl Pts',(4.21704119895221,1.06939092065416,-5.89737768176648));
#151402=CARTESIAN_POINT('Ctrl Pts',(4.564041892,1.068630405,-5.951430215));
#151403=CARTESIAN_POINT('Ctrl Pts',(4.556948688,1.070029867,-5.956869862));
#151404=CARTESIAN_POINT('Ctrl Pts',(4.549842538,1.071428571,-5.962292586));
#151405=CARTESIAN_POINT('Ctrl Pts',(4.231352001,1.134117105,-6.205333626));
#151406=CARTESIAN_POINT('Ctrl Pts',(3.88878248,1.197973174,-6.413062515));
#151407=CARTESIAN_POINT('Ctrl Pts',(4.220860275,1.068630405,-5.894644903));
#151408=CARTESIAN_POINT('Ctrl Pts',(4.213834751,1.070029867,-5.89967553));
#151409=CARTESIAN_POINT('Ctrl Pts',(4.206797255,1.071428571,-5.904689396));
#151410=CARTESIAN_POINT('Ctrl Pts',(3.891383734,1.134117105,-6.129405827));
#151411=CARTESIAN_POINT('Ctrl Pts',(3.553825856,1.197973174,-6.319242184));
#151412=CARTESIAN_POINT('Origin',(-0.0726058415674252,1.33885357944252,
0.176679306747297));
#151413=CARTESIAN_POINT('Ctrl Pts',(3.48482382869069,1.20239769722685,-6.64189083359813));
#151414=CARTESIAN_POINT('Ctrl Pts',(3.47231717767815,1.20018543561341,-6.64839291107468));
#151415=CARTESIAN_POINT('Ctrl Pts',(3.4598105266656,1.197973174,-6.65489498855133));
#151416=CARTESIAN_POINT('Ctrl Pts',(3.09728076171842,1.13384644,-6.84337043388931));
#151417=CARTESIAN_POINT('Ctrl Pts',(2.71642242712733,1.068610636,-6.99134932534094));
#151418=CARTESIAN_POINT('Ctrl Pts',(3.57757756258052,1.20239769722685,-6.30588466001074));
#151419=CARTESIAN_POINT('Ctrl Pts',(3.56570170929029,1.20018543561341,-6.31256342200547));
#151420=CARTESIAN_POINT('Ctrl Pts',(3.553825856,1.197973174,-6.319242184));
#151421=CARTESIAN_POINT('Ctrl Pts',(3.209580998,1.13384644,-6.512839176));
#151422=CARTESIAN_POINT('Ctrl Pts',(2.846343018,1.068610636,-6.66789557700001));
#151423=CARTESIAN_POINT('',(2.85068724288564,1.06939092013848,-6.66603946941679));
#151424=CARTESIAN_POINT('Origin',(-0.0565274918814662,0.946547102750439,
0.183994782434302));
#151425=CARTESIAN_POINT('Ctrl Pts',(2.94728332000656,1.10830076261339,-6.89663113609631));
#151426=CARTESIAN_POINT('Ctrl Pts',(2.93106714437848,1.10211922686252,-6.85820661904387));
#151427=CARTESIAN_POINT('Ctrl Pts',(2.91489786188007,1.09579054182493,-6.81975969218544));
#151428=CARTESIAN_POINT('Ctrl Pts',(2.88207248594303,1.08257773698977,-6.74140763778961));
#151429=CARTESIAN_POINT('Ctrl Pts',(2.86617475262665,1.07598453111424,-6.70326811364963));
#151430=CARTESIAN_POINT('Ctrl Pts',(2.8506872430964,1.06939092063435,-6.66603947211695));
#151431=CARTESIAN_POINT('Ctrl Pts',(3.177955556,1.068630405,-6.79342317900001));
#151432=CARTESIAN_POINT('Ctrl Pts',(3.169858824,1.070029867,-6.797210821));
#151433=CARTESIAN_POINT('Ctrl Pts',(3.161753086,1.071428571,-6.800979152));
#151434=CARTESIAN_POINT('Ctrl Pts',(2.798462042,1.134117105,-6.969871977));
#151435=CARTESIAN_POINT('Ctrl Pts',(2.419246034,1.197973174,-7.099101959));
#151436=CARTESIAN_POINT('Ctrl Pts',(2.855004498,1.068630405,-6.664191573));
#151437=CARTESIAN_POINT('Ctrl Pts',(2.84706179,1.070029867,-6.667594306));
#151438=CARTESIAN_POINT('Ctrl Pts',(2.839110994,1.071428571,-6.670978097));
#151439=CARTESIAN_POINT('Ctrl Pts',(2.482764276,1.134117105,-6.8226362));
#151440=CARTESIAN_POINT('Ctrl Pts',(2.112289109,1.197973174,-6.935469322));
#151441=CARTESIAN_POINT('Origin',(-0.0329275030577136,1.33885361190165,
0.188156703710749));
#151442=CARTESIAN_POINT('Ctrl Pts',(1.95650203590071,1.19924836941368,-7.24031531054044));
#151443=CARTESIAN_POINT('Ctrl Pts',(1.95257925395036,1.19861077170684,-7.24137077927022));
#151444=CARTESIAN_POINT('Ctrl Pts',(1.948656472,1.197973174,-7.242426248));
#151445=CARTESIAN_POINT('Ctrl Pts',(1.554120557,1.13384644,-7.348580586));
#151446=CARTESIAN_POINT('Ctrl Pts',(1.150387927,1.068610636,-7.411248722));
#151447=CARTESIAN_POINT('Ctrl Pts',(2.11980215310686,1.19924836941368,-6.93318112482194));
#151448=CARTESIAN_POINT('Ctrl Pts',(2.11604563105343,1.19861077170684,-6.93432522341097));
#151449=CARTESIAN_POINT('Ctrl Pts',(2.112289109,1.197973174,-6.93546932199999));
#151450=CARTESIAN_POINT('Ctrl Pts',(1.734474873,1.13384644,-7.050537656));
#151451=CARTESIAN_POINT('Ctrl Pts',(1.346396652,1.068610636,-7.123883495));
#151452=CARTESIAN_POINT('',(1.35103832001002,1.06939092016804,-7.12300466238269));
#151453=CARTESIAN_POINT('Origin',(-0.0156524015825424,0.946547090581574,
0.191844575304695));
#151454=CARTESIAN_POINT('Ctrl Pts',(1.39580564292765,1.10830076261233,-7.36897052522762));
#151455=CARTESIAN_POINT('Ctrl Pts',(1.3882287277522,1.10211922684992,-7.32795835342687));
#151456=CARTESIAN_POINT('Ctrl Pts',(1.38070242688305,1.0957905418705,-7.28693437682775));
#151457=CARTESIAN_POINT('Ctrl Pts',(1.36548790457744,1.08257777103923,-7.20335787924211));
#151458=CARTESIAN_POINT('Ctrl Pts',(1.35816072347702,1.07598456880958,-7.16269250412706));
#151459=CARTESIAN_POINT('Ctrl Pts',(1.35103831922291,1.06939092063558,-7.12300466481012));
#151460=CARTESIAN_POINT('Ctrl Pts',(1.64327155,1.068630405,-7.317763225));
#151461=CARTESIAN_POINT('Ctrl Pts',(1.634549884,1.070029867,-7.319721756));
#151462=CARTESIAN_POINT('Ctrl Pts',(1.625823574,1.071428571,-7.321659491));
#151463=CARTESIAN_POINT('Ctrl Pts',(1.234719107,1.134117105,-7.40850686));
#151464=CARTESIAN_POINT('Ctrl Pts',(0.836588333,1.197973174,-7.453195285));
#151465=CARTESIAN_POINT('Ctrl Pts',(1.355651883,1.068630405,-7.12212805100001));
#151466=CARTESIAN_POINT('Ctrl Pts',(1.347163385,1.070029867,-7.12374378300001));
#151467=CARTESIAN_POINT('Ctrl Pts',(1.338671059,1.071428571,-7.125339276));
#151468=CARTESIAN_POINT('Ctrl Pts',(0.95805352,1.134117105,-7.196847686));
#151469=CARTESIAN_POINT('Ctrl Pts',(0.57198407,1.197973174,-7.227401623));
#151470=CARTESIAN_POINT('Origin',(0.00829042140507816,1.33885358366507,
0.190836349482981));
#151471=CARTESIAN_POINT('Ctrl Pts',(0.356511060962697,1.19962221840631,
-7.49172613854189));
#151472=CARTESIAN_POINT('Ctrl Pts',(0.351263280142558,1.19879769620315,
-7.49196849872099));
#151473=CARTESIAN_POINT('Ctrl Pts',(0.346015499322418,1.197973174,-7.4922108589001));
#151474=CARTESIAN_POINT('Ctrl Pts',(-0.0621275967109266,1.13384644,-7.51106028063581));
#151475=CARTESIAN_POINT('Ctrl Pts',(-0.469903043622183,1.068610636,-7.48546200380075));
#151476=CARTESIAN_POINT('Ctrl Pts',(0.582108670146463,1.19962221840631,
-7.22660035162996));
#151477=CARTESIAN_POINT('Ctrl Pts',(0.577046370073232,1.19879769620315,
-7.22700098731498));
#151478=CARTESIAN_POINT('Ctrl Pts',(0.57198407,1.197973174,-7.227401623));
#151479=CARTESIAN_POINT('Ctrl Pts',(0.178266631,1.13384644,-7.25856083));
#151480=CARTESIAN_POINT('Ctrl Pts',(-0.216505724,1.068610636,-7.246766539));
#151481=CARTESIAN_POINT('',(-0.211783652922205,1.06939092018228,-7.2469060743844));
#151482=CARTESIAN_POINT('Origin',(0.0259544467068482,0.946547088024064,
0.190724426768872));
#151483=CARTESIAN_POINT('Ctrl Pts',(-0.220938355623848,1.10830076264133,
-7.4967450430742));
#151484=CARTESIAN_POINT('Ctrl Pts',(-0.219521722060894,1.10211922691222,
-7.4550629005387));
#151485=CARTESIAN_POINT('Ctrl Pts',(-0.218053119813245,1.09579054189136,
-7.41338010930192));
#151486=CARTESIAN_POINT('Ctrl Pts',(-0.214945473836777,1.08257783683062,
-7.32848733402096));
#151487=CARTESIAN_POINT('Ctrl Pts',(-0.213359497213835,1.07598463444262,
-7.28719754505322));
#151488=CARTESIAN_POINT('Ctrl Pts',(-0.211783654082421,1.06939092059991,
-7.24690607660022));
#151489=CARTESIAN_POINT('Ctrl Pts',(0.031749992,1.068630405,-7.499932796));
#151490=CARTESIAN_POINT('Ctrl Pts',(0.022811208,1.070029867,-7.499970637));
#151491=CARTESIAN_POINT('Ctrl Pts',(0.013872358,1.071428571,-7.499987171));
#151492=CARTESIAN_POINT('Ctrl Pts',(-0.38675792,1.134117105,-7.500728197));
#151493=CARTESIAN_POINT('Ctrl Pts',(-0.785187309,1.197973174,-7.458785484));
#151494=CARTESIAN_POINT('Ctrl Pts',(-0.207089507,1.068630405,-7.247041737));
#151495=CARTESIAN_POINT('Ctrl Pts',(-0.215726884,1.070029867,-7.246794918));
#151496=CARTESIAN_POINT('Ctrl Pts',(-0.224363648,1.071428571,-7.24652751));
#151497=CARTESIAN_POINT('Ctrl Pts',(-0.611454754,1.134117105,-7.234542573));
#151498=CARTESIAN_POINT('Ctrl Pts',(-0.995066308,1.197973174,-7.181388657));
#151499=CARTESIAN_POINT('Ctrl Pts',(-0.20947790199,1.068630405,-7.24451282641));
#151500=CARTESIAN_POINT('Ctrl Pts',(-0.21811226492,1.070029867,-7.24426316081));
#151501=CARTESIAN_POINT('Ctrl Pts',(-0.22674600806,1.071428571,-7.24399291339));
#151502=CARTESIAN_POINT('Ctrl Pts',(-0.61370172234,1.134117105,-7.23188071676));
#151503=CARTESIAN_POINT('Ctrl Pts',(-0.997165097989999,1.197973174,-7.17861468873));
#151504=CARTESIAN_POINT('Origin',(0.049120771256816,1.33885359098496,0.184592545852338));
#151505=CARTESIAN_POINT('Ctrl Pts',(-1.24525698666216,1.20239769734986,
-7.39648876232056));
#151506=CARTESIAN_POINT('Ctrl Pts',(-1.25914833481224,1.20018543567492,
-7.39409631833717));
#151507=CARTESIAN_POINT('Ctrl Pts',(-1.27303968296231,1.197973174,-7.39170387435364));
#151508=CARTESIAN_POINT('Ctrl Pts',(-1.6757075941863,1.13384644,-7.32235420352542));
#151509=CARTESIAN_POINT('Ctrl Pts',(-2.06845928399246,1.068610636,-7.20967352818163));
#151510=CARTESIAN_POINT('Ctrl Pts',(-0.968074109179946,1.20239769734986,
-7.18512874527744));
#151511=CARTESIAN_POINT('Ctrl Pts',(-0.981570208589966,1.20018543567492,
-7.1832587011387));
#151512=CARTESIAN_POINT('Ctrl Pts',(-0.995066308,1.197973174,-7.181388657));
#151513=CARTESIAN_POINT('Ctrl Pts',(-1.386277161,1.13384644,-7.127181768));
#151514=CARTESIAN_POINT('Ctrl Pts',(-1.769284534,1.068610636,-7.030798834));
#151515=CARTESIAN_POINT('',(-1.76470285746994,1.06939092017545,-7.03195021220936));
#151516=CARTESIAN_POINT('Origin',(0.0663477542199706,0.94654708250684,0.180685933335545));
#151517=CARTESIAN_POINT('Ctrl Pts',(-1.82735152120739,1.10830076259602,
-7.27398009430452));
#151518=CARTESIAN_POINT('Ctrl Pts',(-1.81700757923931,1.10211922682501,
-7.23357699113942));
#151519=CARTESIAN_POINT('Ctrl Pts',(-1.80661274423284,1.0957905418318,-7.19318442661767));
#151520=CARTESIAN_POINT('Ctrl Pts',(-1.78532807882825,1.08257768947031,
-7.11094353236947));
#151521=CARTESIAN_POINT('Ctrl Pts',(-1.77490309665638,1.07598448114017,
-7.07096002344486));
#151522=CARTESIAN_POINT('Ctrl Pts',(-1.76470285889488,1.06939092077265,
-7.0319502149922));
#151523=CARTESIAN_POINT('Ctrl Pts',(-1.581256159,1.068630405,-7.331413844));
#151524=CARTESIAN_POINT('Ctrl Pts',(-1.589994095,1.070029867,-7.329529226));
#151525=CARTESIAN_POINT('Ctrl Pts',(-1.598727514,1.071428571,-7.327623785));
#151526=CARTESIAN_POINT('Ctrl Pts',(-1.990150577,1.134117105,-7.242223819));
#151527=CARTESIAN_POINT('Ctrl Pts',(-2.370248465,1.197973174,-7.115611162));
#151528=CARTESIAN_POINT('Ctrl Pts',(-1.760147621,1.068630405,-7.033091806));
#151529=CARTESIAN_POINT('Ctrl Pts',(-1.768530002,1.070029867,-7.030993976));
#151530=CARTESIAN_POINT('Ctrl Pts',(-1.776907359,1.071428571,-7.028876172));
#151531=CARTESIAN_POINT('Ctrl Pts',(-2.152372083,1.134117105,-6.933958291));
#151532=CARTESIAN_POINT('Ctrl Pts',(-2.515588492,1.197973174,-6.799581939));
#151533=CARTESIAN_POINT('Origin',(0.0876542312126244,1.33885357285475,0.169717188211986));
#151534=CARTESIAN_POINT('Ctrl Pts',(-2.80617001522815,1.20239769740834,
-6.95586952263931));
#151535=CARTESIAN_POINT('Ctrl Pts',(-2.81922228681214,1.20018543570416,
-6.95054678334448));
#151536=CARTESIAN_POINT('Ctrl Pts',(-2.83227455839611,1.197973174,-6.94522404404955));
#151537=CARTESIAN_POINT('Ctrl Pts',(-3.21062018829537,1.13384644,-6.79093403112974));
#151538=CARTESIAN_POINT('Ctrl Pts',(-3.56996654686197,1.068610636,-6.59645776536835));
#151539=CARTESIAN_POINT('Ctrl Pts',(-2.49003136393391,1.20239769740834,
-6.80903711112478));
#151540=CARTESIAN_POINT('Ctrl Pts',(-2.50280992796696,1.20018543570416,
-6.80430952506239));
#151541=CARTESIAN_POINT('Ctrl Pts',(-2.515588492,1.197973174,-6.799581939));
#151542=CARTESIAN_POINT('Ctrl Pts',(-2.886000173,1.13384644,-6.662543607));
#151543=CARTESIAN_POINT('Ctrl Pts',(-3.239333565,1.068610636,-6.486078789));
#151544=CARTESIAN_POINT('',(-3.23510651809109,1.06939092015702,-6.48818817439076));
#151545=CARTESIAN_POINT('Origin',(0.103638799473554,0.946547093860595,0.162198973411954));
#151546=CARTESIAN_POINT('Ctrl Pts',(-3.348319761214,1.10830076258882,-6.71109192096732));
#151547=CARTESIAN_POINT('Ctrl Pts',(-3.329532181977,1.10211922683441,-6.6738570618238));
#151548=CARTESIAN_POINT('Ctrl Pts',(-3.31069716493209,1.09579054181929,
-6.63664343517178));
#151549=CARTESIAN_POINT('Ctrl Pts',(-3.2722309301523,1.08257774728062,-6.560901192623));
#151550=CARTESIAN_POINT('Ctrl Pts',(-3.25345441216452,1.07598454419332,
-6.52409355055558));
#151551=CARTESIAN_POINT('Ctrl Pts',(-3.23510652026311,1.06939092068502,
-6.48818817582034));
#151552=CARTESIAN_POINT('Ctrl Pts',(-3.120324531,1.068630405,-6.82008613));
#151553=CARTESIAN_POINT('Ctrl Pts',(-3.128453041,1.070029867,-6.816367176));
#151554=CARTESIAN_POINT('Ctrl Pts',(-3.136572664,1.071428571,-6.812628856));
#151555=CARTESIAN_POINT('Ctrl Pts',(-3.500486005,1.134117105,-6.64508110500001));
#151556=CARTESIAN_POINT('Ctrl Pts',(-3.844479437,1.197973174,-6.43971877199999));
#151557=CARTESIAN_POINT('Ctrl Pts',(-3.23090319,1.068630405,-6.490282319));
#151558=CARTESIAN_POINT('Ctrl Pts',(-3.238638624,1.070029867,-6.486431571));
#151559=CARTESIAN_POINT('Ctrl Pts',(-3.246364857,1.071428571,-6.482562396));
#151560=CARTESIAN_POINT('Ctrl Pts',(-3.592646886,1.134117105,-6.30914982500001));
#151561=CARTESIAN_POINT('Ctrl Pts',(-3.918484554,1.197973174,-6.099834326));
#151562=CARTESIAN_POINT('Origin',(0.122089194624269,1.33885354582984,0.146906389843944));
#151563=CARTESIAN_POINT('Ctrl Pts',(-4.23586965189261,1.2023976974972,-6.19000155562014));
#151564=CARTESIAN_POINT('Ctrl Pts',(-4.24747253727115,1.20018543574859,
-6.18199740627892));
#151565=CARTESIAN_POINT('Ctrl Pts',(-4.25907542264976,1.197973174,-6.17399325693772));
#151566=CARTESIAN_POINT('Ctrl Pts',(-4.59540775076638,1.13384644,-5.9419773320462));
#151567=CARTESIAN_POINT('Ctrl Pts',(-4.90454614294094,1.068610636,-5.67479896766707));
#151568=CARTESIAN_POINT('Ctrl Pts',(-3.89555751945189,1.2023976974972,-6.11456246881635));
#151569=CARTESIAN_POINT('Ctrl Pts',(-3.90702103672596,1.20018543574859,
-6.10719839740816));
#151570=CARTESIAN_POINT('Ctrl Pts',(-3.918484554,1.197973174,-6.099834326));
#151571=CARTESIAN_POINT('Ctrl Pts',(-4.250777025,1.13384644,-5.886372312));
#151572=CARTESIAN_POINT('Ctrl Pts',(-4.557914959,1.068610636,-5.638076909));
#151573=CARTESIAN_POINT('',(-4.5542401936933,1.0693909201846,-5.64104566757719));
#151574=CARTESIAN_POINT('Origin',(0.136083798206407,0.946547087754226,0.136127620145601));
#151575=CARTESIAN_POINT('Ctrl Pts',(-4.71272429052064,1.10830076262936,
-5.83440054806072));
#151576=CARTESIAN_POINT('Ctrl Pts',(-4.68637156050134,1.10211922689068,
-5.80207499348866));
#151577=CARTESIAN_POINT('Ctrl Pts',(-4.65997706604311,1.09579054187506,
-5.76978037268462));
#151578=CARTESIAN_POINT('Ctrl Pts',(-4.60612778559715,1.08257774199474,
-5.70407801871414));
#151579=CARTESIAN_POINT('Ctrl Pts',(-4.57987769066149,1.07598453679128,
-5.67216730677154));
#151580=CARTESIAN_POINT('Ctrl Pts',(-4.55424019597839,1.06939092069683,
-5.64104566923627));
#151581=CARTESIAN_POINT('Ctrl Pts',(-4.513489995,1.068630405,-5.989858769));
#151582=CARTESIAN_POINT('Ctrl Pts',(-4.520629,1.070029867,-5.98447937200001));
#151583=CARTESIAN_POINT('Ctrl Pts',(-4.527755162,1.071428571,-5.979082973));
#151584=CARTESIAN_POINT('Ctrl Pts',(-4.847142598,1.134117105,-5.737221784));
#151585=CARTESIAN_POINT('Ctrl Pts',(-5.138946823,1.197973174,-5.462712289));
#151586=CARTESIAN_POINT('Ctrl Pts',(-4.550585316,1.068630405,-5.643994444));
#151587=CARTESIAN_POINT('Ctrl Pts',(-4.557312103,1.070029867,-5.638570835));
#151588=CARTESIAN_POINT('Ctrl Pts',(-4.564025943,1.071428571,-5.633131207));
#151589=CARTESIAN_POINT('Ctrl Pts',(-4.864933514,1.134117105,-5.389332525));
#151590=CARTESIAN_POINT('Ctrl Pts',(-5.138156632,1.197973174,-5.11486524));
#151591=CARTESIAN_POINT('Origin',(0.150815306188561,1.33885361766223,0.117226161007045));
#151592=CARTESIAN_POINT('Ctrl Pts',(-5.46750473373431,1.20239769723693,
-5.13469599369841));
#151593=CARTESIAN_POINT('Ctrl Pts',(-5.47711569402266,1.20018543561845,
-5.1243847001737));
#151594=CARTESIAN_POINT('Ctrl Pts',(-5.48672665431106,1.197973174,-5.11407340664884));
#151595=CARTESIAN_POINT('Ctrl Pts',(-5.76531915384119,1.13384644,-4.81518037720383));
#151596=CARTESIAN_POINT('Ctrl Pts',(-6.00979461161303,1.068610636,-4.48779287854149));
#151597=CARTESIAN_POINT('Ctrl Pts',(-5.11893173515577,1.20239769723692,
-5.13417768056049));
#151598=CARTESIAN_POINT('Ctrl Pts',(-5.12854418357785,1.20018543561845,
-5.12452146028024));
#151599=CARTESIAN_POINT('Ctrl Pts',(-5.138156632,1.197973174,-5.11486524));
#151600=CARTESIAN_POINT('Ctrl Pts',(-5.416792268,1.13384644,-4.834960791));
#151601=CARTESIAN_POINT('Ctrl Pts',(-5.663373315,1.068610636,-4.526444819));
#151602=CARTESIAN_POINT('',(-5.66042265901186,1.06939092020276,-4.53013413550935));
#151603=CARTESIAN_POINT('Origin',(0.162165348725155,0.946547092345618,0.103690775807711));
#151604=CARTESIAN_POINT('Ctrl Pts',(-5.85676706945754,1.10830076259221,
-4.68489909035697));
#151605=CARTESIAN_POINT('Ctrl Pts',(-5.82408141295832,1.10211922686147,
-4.65899434735455));
#151606=CARTESIAN_POINT('Ctrl Pts',(-5.7913616184495,1.0957905418823,-4.63312879310499));
#151607=CARTESIAN_POINT('Ctrl Pts',(-5.72464727544109,1.08257774895735,
-4.58053855480737));
#151608=CARTESIAN_POINT('Ctrl Pts',(-5.69215102469282,1.07598454214351,
-4.55501688436513));
#151609=CARTESIAN_POINT('Ctrl Pts',(-5.66042266160367,1.06939092069564,
-4.5301341366984));
#151610=CARTESIAN_POINT('Ctrl Pts',(-5.695609683,1.068630405,-4.879552268));
#151611=CARTESIAN_POINT('Ctrl Pts',(-5.701425371,1.070029867,-4.872763963));
#151612=CARTESIAN_POINT('Ctrl Pts',(-5.707224861,1.071428571,-4.865961815));
#151613=CARTESIAN_POINT('Ctrl Pts',(-5.96715219,1.134117105,-4.561096349));
#151614=CARTESIAN_POINT('Ctrl Pts',(-6.193122768,1.197973174,-4.23027545));
#151615=CARTESIAN_POINT('Ctrl Pts',(-5.65748713,1.068630405,-4.533799662));
#151616=CARTESIAN_POINT('Ctrl Pts',(-5.662890733,1.070029867,-4.527056793));
#151617=CARTESIAN_POINT('Ctrl Pts',(-5.668278248,1.071428571,-4.520301063));
#151618=CARTESIAN_POINT('Ctrl Pts',(-5.90974125700001,1.134117105,-4.217516027));
#151619=CARTESIAN_POINT('Ctrl Pts',(-6.11757421800001,1.197973174,-3.89073074));
#151620=CARTESIAN_POINT('Origin',(0.172489465399025,1.33885358243788,0.0820646436682093));
#151621=CARTESIAN_POINT('Ctrl Pts',(-6.44348537030917,1.20239769727684,
-3.83929775550167));
#151622=CARTESIAN_POINT('Ctrl Pts',(-6.45065500842762,1.20018543563844,
-3.82716146182784));
#151623=CARTESIAN_POINT('Ctrl Pts',(-6.45782464654608,1.197973174,-3.81502516815401));
#151624=CARTESIAN_POINT('Ctrl Pts',(-6.66565064167765,1.13384644,-3.46323093972956));
#151625=CARTESIAN_POINT('Ctrl Pts',(-6.83403176425173,1.068610636,-3.09094258099947));
#151626=CARTESIAN_POINT('Ctrl Pts',(-6.10295039234986,1.20239769727684,
-3.91372445118755));
#151627=CARTESIAN_POINT('Ctrl Pts',(-6.11026230517487,1.20018543563845,
-3.90222759559374));
#151628=CARTESIAN_POINT('Ctrl Pts',(-6.11757421800001,1.197973174,-3.89073074));
#151629=CARTESIAN_POINT('Ctrl Pts',(-6.329524324,1.13384644,-3.557471876));
#151630=CARTESIAN_POINT('Ctrl Pts',(-6.504018629,1.068610636,-3.2031612));
#151631=CARTESIAN_POINT('',(-6.50193005203167,1.06939092017978,-3.2073985659925));
#151632=CARTESIAN_POINT('Origin',(0.180664648446098,0.946547090042,0.0664058816374508));
#151633=CARTESIAN_POINT('Ctrl Pts',(-6.72695393012478,1.10830076261049,
-3.31633695786175));
#151634=CARTESIAN_POINT('Ctrl Pts',(-6.68946369205213,1.10211922687114,
-3.29806430321489));
#151635=CARTESIAN_POINT('Ctrl Pts',(-6.65194853850496,1.09579054188135,
-3.27983725979242));
#151636=CARTESIAN_POINT('Ctrl Pts',(-6.57548829285055,1.08257769708028,
-3.24281801837758));
#151637=CARTESIAN_POINT('Ctrl Pts',(-6.53826539480128,1.07598449024056,
-3.22487877187214));
#151638=CARTESIAN_POINT('Ctrl Pts',(-6.50193005463138,1.06939092064217,
-3.20739856646713));
#151639=CARTESIAN_POINT('Ctrl Pts',(-6.611408993,1.068630405,-3.541083327));
#151640=CARTESIAN_POINT('Ctrl Pts',(-6.615629428,1.070029867,-3.533203528));
#151641=CARTESIAN_POINT('Ctrl Pts',(-6.619831069,1.071428571,-3.525313691));
#151642=CARTESIAN_POINT('Ctrl Pts',(-6.808144378,1.134117105,-3.171699118));
#151643=CARTESIAN_POINT('Ctrl Pts',(-6.957715175,1.197973174,-2.800035633));
#151644=CARTESIAN_POINT('Ctrl Pts',(-6.499851134,1.068630405,-3.211609446));
#151645=CARTESIAN_POINT('Ctrl Pts',(-6.503678886,1.070029867,-3.203862607));
#151646=CARTESIAN_POINT('Ctrl Pts',(-6.507488162,1.071428571,-3.196106666));
#151647=CARTESIAN_POINT('Ctrl Pts',(-6.678216068,1.134117105,-2.848493166));
#151648=CARTESIAN_POINT('Ctrl Pts',(-6.810940832,1.197973174,-2.484669994));
#151649=CARTESIAN_POINT('Origin',(0.186098011533374,1.33885358281873,0.0430657848834071));
#151650=CARTESIAN_POINT('Ctrl Pts',(-7.11817579072873,1.20239769742353,
-2.36437822199281));
#151651=CARTESIAN_POINT('Ctrl Pts',(-7.12256886247866,1.20018543571177,
-2.35098440740509));
#151652=CARTESIAN_POINT('Ctrl Pts',(-7.12696193422843,1.197973174,-2.33759059281739));
#151653=CARTESIAN_POINT('Ctrl Pts',(-7.25430371393051,1.13384644,-1.94934467202816));
#151654=CARTESIAN_POINT('Ctrl Pts',(-7.33871718618051,1.068610636,-1.54956324476661));
#151655=CARTESIAN_POINT('Ctrl Pts',(-6.80160187114612,1.20239769742353,
-2.51026981604631));
#151656=CARTESIAN_POINT('Ctrl Pts',(-6.80627135157313,1.20018543571177,
-2.49746990502316));
#151657=CARTESIAN_POINT('Ctrl Pts',(-6.810940832,1.197973174,-2.484669994));
#151658=CARTESIAN_POINT('Ctrl Pts',(-6.946294858,1.13384644,-2.11363953));
#151659=CARTESIAN_POINT('Ctrl Pts',(-7.040543261,1.068610636,-1.730101323));
#151660=CARTESIAN_POINT('',(-7.03941442235458,1.06939092016788,-1.73468860428955));
#151661=CARTESIAN_POINT('Origin',(0.190715988737931,0.946547109884456,0.0260157603669187));
#151662=CARTESIAN_POINT('Ctrl Pts',(-7.28259590116875,1.10830076259209,
-1.79270659508155));
#151663=CARTESIAN_POINT('Ctrl Pts',(-7.24205408327934,1.10211922684959,
-1.78292043793131));
#151664=CARTESIAN_POINT('Ctrl Pts',(-7.20149773745193,1.09579054185039,
-1.77318418171899));
#151665=CARTESIAN_POINT('Ctrl Pts',(-7.118867287594,1.08257773551417,-1.75346717962857));
#151666=CARTESIAN_POINT('Ctrl Pts',(-7.07865822432206,1.07598452917805,
-1.74394916250209));
#151667=CARTESIAN_POINT('Ctrl Pts',(-7.03941442481537,1.06939092068366,
-1.73468860419114));
#151668=CARTESIAN_POINT('Ctrl Pts',(-7.218066166,1.068630405,-2.037037265));
#151669=CARTESIAN_POINT('Ctrl Pts',(-7.220494006,1.070029867,-2.028434422));
#151670=CARTESIAN_POINT('Ctrl Pts',(-7.222901333,1.071428571,-2.019825817));
#151671=CARTESIAN_POINT('Ctrl Pts',(-7.330795302,1.134117105,-1.633996761));
#151672=CARTESIAN_POINT('Ctrl Pts',(-7.396972553,1.197973174,-1.238869262));
#151673=CARTESIAN_POINT('Ctrl Pts',(-7.038289323,1.068630405,-1.739247943));
#151674=CARTESIAN_POINT('Ctrl Pts',(-7.040362243,1.070029867,-1.730859367));
#151675=CARTESIAN_POINT('Ctrl Pts',(-7.042415162,1.071428571,-1.722465874));
#151676=CARTESIAN_POINT('Ctrl Pts',(-7.134424917,1.134117105,-1.346277931));
#151677=CARTESIAN_POINT('Ctrl Pts',(-7.18583542299999,1.197973174,-0.962428841999999));
#151678=CARTESIAN_POINT('Origin',(0.191005223540494,1.33885360436684,0.00205339707159954));
#151679=CARTESIAN_POINT('Ctrl Pts',(-7.46146198490312,1.19924836941368,
-0.759375434223065));
#151680=CARTESIAN_POINT('Ctrl Pts',(-7.46186891395157,1.19861077170684,
-0.755333573111533));
#151681=CARTESIAN_POINT('Ctrl Pts',(-7.462275843,1.197973174,-0.751291712));
#151682=CARTESIAN_POINT('Ctrl Pts',(-7.503202952,1.13384644,-0.344779346));
#151683=CARTESIAN_POINT('Ctrl Pts',(-7.49972886,1.068610636,0.063773298));
#151684=CARTESIAN_POINT('Ctrl Pts',(-7.18479284462103,1.19924836941368,
-0.970213102287846));
#151685=CARTESIAN_POINT('Ctrl Pts',(-7.18531413381051,1.19861077170684,
-0.966320972143922));
#151686=CARTESIAN_POINT('Ctrl Pts',(-7.185835423,1.197973174,-0.962428842));
#151687=CARTESIAN_POINT('Ctrl Pts',(-7.238264365,1.13384644,-0.570975749));
#151688=CARTESIAN_POINT('Ctrl Pts',(-7.24785991500001,1.068610636,-0.176143831));
#151689=CARTESIAN_POINT('',(-7.24774359796863,1.06939092016464,-0.180866531822896));
#151690=CARTESIAN_POINT('Origin',(0.191849688360007,0.946547112772989,-0.0155907848465632));
#151691=CARTESIAN_POINT('Ctrl Pts',(-7.4977117819841,1.10830076263164,-0.185251264675216));
#151692=CARTESIAN_POINT('Ctrl Pts',(-7.4560140745458,1.10211922684026,-0.184409194783553));
#151693=CARTESIAN_POINT('Ctrl Pts',(-7.41431290627305,1.09579054182928,
-0.183618982244394));
#151694=CARTESIAN_POINT('Ctrl Pts',(-7.32937619817292,1.08257780709784,
-0.182126064751401));
#151695=CARTESIAN_POINT('Ctrl Pts',(-7.28806110257299,1.07598460347731,
-0.181474331916232));
#151696=CARTESIAN_POINT('Ctrl Pts',(-7.24774360024735,1.06939092064195,
-0.180866530270857));
#151697=CARTESIAN_POINT('Ctrl Pts',(-7.487214588,1.068630405,-0.437741604));
#151698=CARTESIAN_POINT('Ctrl Pts',(-7.48773631,1.070029867,-0.428817978));
#151699=CARTESIAN_POINT('Ctrl Pts',(-7.488236759,1.071428571,-0.419893133));
#151700=CARTESIAN_POINT('Ctrl Pts',(-7.510666384,1.134117105,-0.019890532));
#151701=CARTESIAN_POINT('Ctrl Pts',(-7.490355716,1.197973174,0.380225258));
#151702=CARTESIAN_POINT('Ctrl Pts',(-7.247624926,1.068630405,-0.185561138));
#151703=CARTESIAN_POINT('Ctrl Pts',(-7.247846087,1.070029867,-0.176923066));
#151704=CARTESIAN_POINT('Ctrl Pts',(-7.248046656,1.071428571,-0.168284491));
#151705=CARTESIAN_POINT('Ctrl Pts',(-7.257035987,1.134117105,0.218887764));
#151706=CARTESIAN_POINT('Ctrl Pts',(-7.224728336,1.197973174,0.604814414000001));
#151707=CARTESIAN_POINT('Origin',(0.186981097361099,1.33885359240906,-0.0390550889411558));
#151708=CARTESIAN_POINT('Ctrl Pts',(-7.45305802788279,1.20239769728737,
0.842992881250072));
#151709=CARTESIAN_POINT('Ctrl Pts',(-7.45142115507788,1.20018543564367,
0.856993380657568));
#151710=CARTESIAN_POINT('Ctrl Pts',(-7.44978428227295,1.197973174,0.870993880065064));
#151711=CARTESIAN_POINT('Ctrl Pts',(-7.402336320024,1.13384644,1.27682575982473));
#151712=CARTESIAN_POINT('Ctrl Pts',(-7.3110840494493,1.068610636,1.67510185406666));
#151713=CARTESIAN_POINT('Ctrl Pts',(-7.22700161094625,1.20239769728737,
0.57765931767797));
#151714=CARTESIAN_POINT('Ctrl Pts',(-7.22586497347307,1.20018543564367,
0.591236865838985));
#151715=CARTESIAN_POINT('Ctrl Pts',(-7.224728336,1.197973174,0.604814414));
#151716=CARTESIAN_POINT('Ctrl Pts',(-7.191780674,1.13384644,0.998386224));
#151717=CARTESIAN_POINT('Ctrl Pts',(-7.116274695,1.068610636,1.38604995));
#151718=CARTESIAN_POINT('',(-7.11717633793565,1.06939092018892,1.38141265923022));
#151719=CARTESIAN_POINT('Origin',(0.184013027001663,0.946547072036405,-0.0564683324673482));
#151720=CARTESIAN_POINT('Ctrl Pts',(-7.36224299279127,1.1083007625811,1.43086620946192));
#151721=CARTESIAN_POINT('Ctrl Pts',(-7.32133913467256,1.10211922683588,
1.4227248176501));
#151722=CARTESIAN_POINT('Ctrl Pts',(-7.2804430444382,1.0957905418693,1.4145320369038));
#151723=CARTESIAN_POINT('Ctrl Pts',(-7.19717121001193,1.08257781249686,
1.39773117588402));
#151724=CARTESIAN_POINT('Ctrl Pts',(-7.1566819324551,1.07598460868545,1.3894861468627));
#151725=CARTESIAN_POINT('Ctrl Pts',(-7.11717634035813,1.0693909206464,1.38141266056319));
#151726=CARTESIAN_POINT('Ctrl Pts',(-7.406269177,1.068630405,1.182022367));
#151727=CARTESIAN_POINT('Ctrl Pts',(-7.404860385,1.070029867,1.190849519));
#151728=CARTESIAN_POINT('Ctrl Pts',(-7.403430556,1.071428571,1.199673288));
#151729=CARTESIAN_POINT('Ctrl Pts',(-7.339347054,1.134117105,1.595145757));
#151730=CARTESIAN_POINT('Ctrl Pts',(-7.233498171,1.197973174,1.981540869));
#151731=CARTESIAN_POINT('Ctrl Pts',(-7.118069642,1.068630405,1.376802299));
#151732=CARTESIAN_POINT('Ctrl Pts',(-7.116428702,1.070029867,1.385285961));
#151733=CARTESIAN_POINT('Ctrl Pts',(-7.114767544,1.071428571,1.393765687));
#151734=CARTESIAN_POINT('Ctrl Pts',(-7.04031611900001,1.134117105,1.77381851));
#151735=CARTESIAN_POINT('Ctrl Pts',(-6.925800981,1.197973174,2.14377722));
#151736=CARTESIAN_POINT('Origin',(0.174213841875577,1.33885354649174,-0.078337391496032));
#151737=CARTESIAN_POINT('Ctrl Pts',(-7.09759112262429,1.20239769754087,
2.42547133988342));
#151738=CARTESIAN_POINT('Ctrl Pts',(-7.09298282519605,1.20018543577042,
2.43879263690317));
#151739=CARTESIAN_POINT('Ctrl Pts',(-7.08837452776767,1.197973174,2.45211393392285));
#151740=CARTESIAN_POINT('Ctrl Pts',(-6.95479401422635,1.13384644,2.83825778088423));
#151741=CARTESIAN_POINT('Ctrl Pts',(-6.78005758344963,1.068610636,3.20760585967038));
#151742=CARTESIAN_POINT('Ctrl Pts',(-6.93385865142889,1.20239769754087,
2.117745680191));
#151743=CARTESIAN_POINT('Ctrl Pts',(-6.92982981621444,1.20018543577042,
2.13076145009547));
#151744=CARTESIAN_POINT('Ctrl Pts',(-6.925800981,1.197973174,2.14377722));
#151745=CARTESIAN_POINT('Ctrl Pts',(-6.809017313,1.13384644,2.521064766));
#151746=CARTESIAN_POINT('Ctrl Pts',(-6.651940379,1.068610636,2.883433576));
#151747=CARTESIAN_POINT('',(-6.65381782292297,1.06939092017145,2.87909852931941));
#151748=CARTESIAN_POINT('Origin',(0.167571566097645,0.946547121045729,-0.0947053690530753));
#151749=CARTESIAN_POINT('Ctrl Pts',(-6.88252390359979,1.10830076262036,
2.9800779698598));
#151750=CARTESIAN_POINT('Ctrl Pts',(-6.84432651353948,1.10211922685067,
2.96333379889362));
#151751=CARTESIAN_POINT('Ctrl Pts',(-6.80614775662968,1.09579054182053,
2.94654111021503));
#151752=CARTESIAN_POINT('Ctrl Pts',(-6.72843428248117,1.08257778223854,
2.91223198284212));
#151753=CARTESIAN_POINT('Ctrl Pts',(-6.69066405871868,1.07598457671899,
2.89547571963673));
#151754=CARTESIAN_POINT('Ctrl Pts',(-6.6538178243887,1.06939092057759,2.87909853129467));
#151755=CARTESIAN_POINT('Ctrl Pts',(-6.979014851,1.068630405,2.746516286));
#151756=CARTESIAN_POINT('Ctrl Pts',(-6.975741419,1.070029867,2.754834216));
#151757=CARTESIAN_POINT('Ctrl Pts',(-6.972448169,1.071428571,2.763144319));
#151758=CARTESIAN_POINT('Ctrl Pts',(-6.824848013,1.134117105,3.135594802));
#151759=CARTESIAN_POINT('Ctrl Pts',(-6.63841029,1.197973174,3.490201831));
#151760=CARTESIAN_POINT('Ctrl Pts',(-6.655681333,1.068630405,2.874787991));
#151761=CARTESIAN_POINT('Ctrl Pts',(-6.652255021,1.070029867,2.882720556));
#151762=CARTESIAN_POINT('Ctrl Pts',(-6.64880981,1.071428571,2.890644931));
#151763=CARTESIAN_POINT('Ctrl Pts',(-6.494398894,1.134117105,3.245807475));
#151764=CARTESIAN_POINT('Ctrl Pts',(-6.30303087,1.197973174,3.582499385));
#151765=CARTESIAN_POINT('Ctrl Pts',(-6.65244799782,1.068630405,2.87607070805));
#151766=CARTESIAN_POINT('Ctrl Pts',(-6.64902015702,1.070029867,2.8839994194));
#151767=CARTESIAN_POINT('Ctrl Pts',(-6.64557342641,1.071428571,2.89191993712));
#151768=CARTESIAN_POINT('Ctrl Pts',(-6.49109440281,1.134117105,3.24690960173));
#151769=CARTESIAN_POINT('Ctrl Pts',(-6.2996770758,1.197973174,3.58342236054));
#151770=CARTESIAN_POINT('Origin',(0.153300462422697,1.33885355272707,-0.11395667019479));
#151771=CARTESIAN_POINT('Ctrl Pts',(-6.41024874438494,1.20239769750625,
3.89453745597396));
#151772=CARTESIAN_POINT('Ctrl Pts',(-6.40288450137365,1.20018543575313,
3.90655666063902));
#151773=CARTESIAN_POINT('Ctrl Pts',(-6.39552025836221,1.197973174,3.91857586530409));
#151774=CARTESIAN_POINT('Ctrl Pts',(-6.18205327054469,1.13384644,4.26697602155056));
#151775=CARTESIAN_POINT('Ctrl Pts',(-5.93200316123656,1.068610636,4.5901257810134));
#151776=CARTESIAN_POINT('Ctrl Pts',(-6.31649616806704,1.20239769750625,
3.55880860922295));
#151777=CARTESIAN_POINT('Ctrl Pts',(-6.3097635190336,1.20018543575313,3.57065399711151));
#151778=CARTESIAN_POINT('Ctrl Pts',(-6.30303087,1.197973174,3.582499385));
#151779=CARTESIAN_POINT('Ctrl Pts',(-6.107871869,1.13384644,3.925861122));
#151780=CARTESIAN_POINT('Ctrl Pts',(-5.876568725,1.068610636,4.245991053));
#151781=CARTESIAN_POINT('',(-5.87933418162948,1.06939092014569,4.24216095191438));
#151782=CARTESIAN_POINT('Origin',(0.143295128420343,0.946547072488477,-0.128514236352059));
#151783=CARTESIAN_POINT('Ctrl Pts',(-6.08098564645011,1.10830076263365,
4.38994459618124));
#151784=CARTESIAN_POINT('Ctrl Pts',(-6.04728079196527,1.10211922686965,
4.36538058482439));
#151785=CARTESIAN_POINT('Ctrl Pts',(-6.01360456489735,1.09579054184488,
4.34077319563695));
#151786=CARTESIAN_POINT('Ctrl Pts',(-5.94508333958708,1.08257776348828,
4.2905600253094));
#151787=CARTESIAN_POINT('Ctrl Pts',(-5.91179827121622,1.07598455844107,
4.26607603671867));
#151788=CARTESIAN_POINT('Ctrl Pts',(-5.87933418351883,1.06939092066381,
4.2421609540683));
#151789=CARTESIAN_POINT('Ctrl Pts',(-6.22542954700001,1.068630405,4.182586157));
#151790=CARTESIAN_POINT('Ctrl Pts',(-6.220444537,1.070029867,4.190005926));
#151791=CARTESIAN_POINT('Ctrl Pts',(-6.215441855,1.071428571,4.197413792));
#151792=CARTESIAN_POINT('Ctrl Pts',(-5.991226664,1.134117105,4.52942692));
#151793=CARTESIAN_POINT('Ctrl Pts',(-5.732917723,1.197973174,4.835664834));
#151794=CARTESIAN_POINT('Ctrl Pts',(-5.882080762,1.068630405,4.238351791));
#151795=CARTESIAN_POINT('Ctrl Pts',(-5.877029288,1.070029867,4.245362341));
#151796=CARTESIAN_POINT('Ctrl Pts',(-5.871961118,1.071428571,4.25236083));
#151797=CARTESIAN_POINT('Ctrl Pts',(-5.64481079600001,1.134117105,4.566026089));
#151798=CARTESIAN_POINT('Ctrl Pts',(-5.385538041,1.197973174,4.853707861));
#151799=CARTESIAN_POINT('Origin',(0.12521894237024,1.33885356109855,-0.144247394630111));
#151800=CARTESIAN_POINT('Ctrl Pts',(-5.42317026021917,1.20239769763789,
5.18149932878505));
#151801=CARTESIAN_POINT('Ctrl Pts',(-5.4133944151325,1.20018543581893,5.19165443686541));
#151802=CARTESIAN_POINT('Ctrl Pts',(-5.40361857004568,1.197973174,5.20180954494577));
#151803=CARTESIAN_POINT('Ctrl Pts',(-5.12024658751617,1.13384644,5.49617520683819));
#151804=CARTESIAN_POINT('Ctrl Pts',(-4.80657486481941,1.068610636,5.75801652210095));
#151805=CARTESIAN_POINT('Ctrl Pts',(-5.40378134486888,1.20239769763789,
4.83346560284931));
#151806=CARTESIAN_POINT('Ctrl Pts',(-5.39465969293444,1.20018543581893,
4.84358673192466));
#151807=CARTESIAN_POINT('Ctrl Pts',(-5.385538041,1.197973174,4.853707861));
#151808=CARTESIAN_POINT('Ctrl Pts',(-5.121129126,1.13384644,5.147088575));
#151809=CARTESIAN_POINT('Ctrl Pts',(-4.826415248,1.068610636,5.410010708));
#151810=CARTESIAN_POINT('',(-4.82993940821834,1.06939092015418,5.40686464364233));
#151811=CARTESIAN_POINT('Origin',(0.112318141206653,0.946547119532799,-0.156313780444191));
#151812=CARTESIAN_POINT('Ctrl Pts',(-4.99510725948456,1.10830076259581,
5.59454229236901));
#151813=CARTESIAN_POINT('Ctrl Pts',(-4.96747094198495,1.10211922681569,
5.56330702642328));
#151814=CARTESIAN_POINT('Ctrl Pts',(-4.93987190779602,1.09579054183511,
5.5320355511299));
#151815=CARTESIAN_POINT('Ctrl Pts',(-4.88374728279049,1.08257782587387,
5.46826659984461));
#151816=CARTESIAN_POINT('Ctrl Pts',(-4.8565037268271,1.07598462233103,5.43719972100207));
#151817=CARTESIAN_POINT('Ctrl Pts',(-4.82993941000098,1.06939092073088,
5.40686464621053));
#151818=CARTESIAN_POINT('Ctrl Pts',(-5.180750076,1.068630405,5.423082947));
#151819=CARTESIAN_POINT('Ctrl Pts',(-5.174286582,1.070029867,5.429257617));
#151820=CARTESIAN_POINT('Ctrl Pts',(-5.167808388,1.071428571,5.435416862));
#151821=CARTESIAN_POINT('Ctrl Pts',(-4.877462215,1.134117105,5.711468069));
#151822=CARTESIAN_POINT('Ctrl Pts',(-4.559360294,1.197973174,5.955017524));
#151823=CARTESIAN_POINT('Ctrl Pts',(-4.833440632,1.068630405,5.403734972));
#151824=CARTESIAN_POINT('Ctrl Pts',(-4.827000198,1.070029867,5.409495702));
#151825=CARTESIAN_POINT('Ctrl Pts',(-4.82054605,1.071428571,5.415241063));
#151826=CARTESIAN_POINT('Ctrl Pts',(-4.531277618,1.134117105,5.672742398));
#151827=CARTESIAN_POINT('Ctrl Pts',(-4.216223439,1.197973174,5.897962352));
#151828=CARTESIAN_POINT('Origin',(0.0912825581236565,1.33885357253129,-0.167793454434852));
#151829=CARTESIAN_POINT('Ctrl Pts',(-4.16592911596048,1.19924836941368,
6.23659367087182));
#151830=CARTESIAN_POINT('Ctrl Pts',(-4.16254869198024,1.19861077170684,
6.23884643943591));
#151831=CARTESIAN_POINT('Ctrl Pts',(-4.159168268,1.197973174,6.241099208));
#151832=CARTESIAN_POINT('Ctrl Pts',(-3.819180299,1.13384644,6.467672624));
#151833=CARTESIAN_POINT('Ctrl Pts',(-3.456591824,1.068610636,6.655972728));
#151834=CARTESIAN_POINT('Ctrl Pts',(-4.22261257419804,1.19924836941368,
5.89339500821418));
#151835=CARTESIAN_POINT('Ctrl Pts',(-4.21941800659903,1.19861077170684,
5.89567868010709));
#151836=CARTESIAN_POINT('Ctrl Pts',(-4.216223439,1.197973174,5.897962352));
#151837=CARTESIAN_POINT('Ctrl Pts',(-3.894928076,1.13384644,6.127643887));
#151838=CARTESIAN_POINT('Ctrl Pts',(-3.550583958,1.068610636,6.321064274));
#151839=CARTESIAN_POINT('',(-3.55470203688038,1.06939092017366,6.3187493536364));
#151840=CARTESIAN_POINT('Origin',(0.0760893310988892,0.946547110468997,
-0.176804295816098));
#151841=CARTESIAN_POINT('Ctrl Pts',(-3.67566320760578,1.10830076262188,
6.53754540923889));
#151842=CARTESIAN_POINT('Ctrl Pts',(-3.65538767083809,1.10211922686063,
6.50109941524943));
#151843=CARTESIAN_POINT('Ctrl Pts',(-3.63515632942574,1.09579054182311,
6.46462607283155));
#151844=CARTESIAN_POINT('Ctrl Pts',(-3.59405206005671,1.08257774660545,
6.39028242294247));
#151845=CARTESIAN_POINT('Ctrl Pts',(-3.57412391075782,1.07598454084017,
6.35408531973988));
#151846=CARTESIAN_POINT('Ctrl Pts',(-3.55470203703904,1.06939092067389,
6.31874935621956));
#151847=CARTESIAN_POINT('Ctrl Pts',(-3.89382449,1.068630405,6.410002406));
#151848=CARTESIAN_POINT('Ctrl Pts',(-3.886184737,1.070029867,6.414643255));
#151849=CARTESIAN_POINT('Ctrl Pts',(-3.878533944,1.071428571,6.419265881));
#151850=CARTESIAN_POINT('Ctrl Pts',(-3.535633054,1.134117105,6.626447319));
#151851=CARTESIAN_POINT('Ctrl Pts',(-3.172612246,1.197973174,6.795920213));
#151852=CARTESIAN_POINT('Ctrl Pts',(-3.558794191,1.068630405,6.316445512));
#151853=CARTESIAN_POINT('Ctrl Pts',(-3.551265944,1.070029867,6.320687056));
#151854=CARTESIAN_POINT('Ctrl Pts',(-3.543727607,1.071428571,6.324910643));
#151855=CARTESIAN_POINT('Ctrl Pts',(-3.205866935,1.134117105,6.514207577));
#151856=CARTESIAN_POINT('Ctrl Pts',(-2.849762915,1.197973174,6.666434679));
#151857=CARTESIAN_POINT('Origin',(0.0530778863023995,1.33885358189054,-0.183493785369463));
#151858=CARTESIAN_POINT('Ctrl Pts',(-2.72784872138814,1.19924836941368,
6.98633719228998));
#151859=CARTESIAN_POINT('Ctrl Pts',(-2.72406305119407,1.19861077170684,
6.98781060114499));
#151860=CARTESIAN_POINT('Ctrl Pts',(-2.720277381,1.197973174,6.98928401));
#151861=CARTESIAN_POINT('Ctrl Pts',(-2.339531555,1.13384644,7.13747290200001));
#151862=CARTESIAN_POINT('Ctrl Pts',(-1.944941241,1.068610636,7.243424851));
#151863=CARTESIAN_POINT('Ctrl Pts',(-2.85698451967887,1.19924836941368,
6.66334759239431));
#151864=CARTESIAN_POINT('Ctrl Pts',(-2.85337371733943,1.19861077170684,
6.66489113569715));
#151865=CARTESIAN_POINT('Ctrl Pts',(-2.849762915,1.197973174,6.666434679));
#151866=CARTESIAN_POINT('Ctrl Pts',(-2.486604518,1.13384644,6.821677381));
#151867=CARTESIAN_POINT('Ctrl Pts',(-2.108731308,1.068610636,6.93655190100001));
#151868=CARTESIAN_POINT('',(-2.1132507478268,1.06939092018769,6.93517636705353));
#151869=CARTESIAN_POINT('Origin',(0.0363027951216388,0.946547113271884,
-0.189027909638053));
#151870=CARTESIAN_POINT('Ctrl Pts',(-2.18434923030014,1.10830076263856,
7.17486016828108));
#151871=CARTESIAN_POINT('Ctrl Pts',(-2.17238253565839,1.1021192268862,7.13490762038882));
#151872=CARTESIAN_POINT('Ctrl Pts',(-2.16046488222171,1.09579054187813,
7.09493786428172));
#151873=CARTESIAN_POINT('Ctrl Pts',(-2.13630354385015,1.08257788288011,
7.01349696441781));
#151874=CARTESIAN_POINT('Ctrl Pts',(-2.1246226002447,1.075984679786,6.97386214325294));
#151875=CARTESIAN_POINT('Ctrl Pts',(-2.11325074774407,1.06939092070939,
6.9351763699027));
#151876=CARTESIAN_POINT('Ctrl Pts',(-2.424827999,1.068630405,7.097197276));
#151877=CARTESIAN_POINT('Ctrl Pts',(-2.416369214,1.070029867,7.100087304));
#151878=CARTESIAN_POINT('Ctrl Pts',(-2.407903564,1.071428571,7.102957161));
#151879=CARTESIAN_POINT('Ctrl Pts',(-2.028481621,1.134117105,7.231581257));
#151880=CARTESIAN_POINT('Ctrl Pts',(-1.637516375,1.197973174,7.319053226));
#151881=CARTESIAN_POINT('Ctrl Pts',(-2.117742488,1.068630405,6.93380608));
#151882=CARTESIAN_POINT('Ctrl Pts',(-2.10947844,1.070029867,6.936330109));
#151883=CARTESIAN_POINT('Ctrl Pts',(-2.1012084,1.071428571,6.938834431));
#151884=CARTESIAN_POINT('Ctrl Pts',(-1.730553477,1.134117105,7.05107565));
#151885=CARTESIAN_POINT('Ctrl Pts',(-1.350050644,1.197973174,7.123191929));
#151886=CARTESIAN_POINT('Origin',(0.0123912359408862,1.3388535675646,-0.190614068400277));
#151887=CARTESIAN_POINT('Ctrl Pts',(-1.16221715234734,1.19924836941368,
7.40940735161141));
#151888=CARTESIAN_POINT('Ctrl Pts',(-1.15820324967367,1.19861077170684,
7.4100325058057));
#151889=CARTESIAN_POINT('Ctrl Pts',(-1.154189347,1.197973174,7.41065766));
#151890=CARTESIAN_POINT('Ctrl Pts',(-0.750488916,1.13384644,7.473532881));
#151891=CARTESIAN_POINT('Ctrl Pts',(-0.342347366,1.068610636,7.492182478));
#151892=CARTESIAN_POINT('Ctrl Pts',(-1.35776704393169,1.19924836941368,
7.12172944830897));
#151893=CARTESIAN_POINT('Ctrl Pts',(-1.35390884396585,1.19861077170684,
7.12246068865448));
#151894=CARTESIAN_POINT('Ctrl Pts',(-1.350050644,1.197973174,7.123191929));
#151895=CARTESIAN_POINT('Ctrl Pts',(-0.962010097,1.13384644,7.196736822));
#151896=CARTESIAN_POINT('Ctrl Pts',(-0.568276727,1.068610636,7.227694069));
#151897=CARTESIAN_POINT('',(-0.572986203455311,1.06939092018801,7.22732224112166));
#151898=CARTESIAN_POINT('Origin',(-0.00518136125522824,0.94654711394043,
-0.19241258054147));
#151899=CARTESIAN_POINT('Ctrl Pts',(-0.590897510175425,1.10830076262937,
7.47668644052261));
#151900=CARTESIAN_POINT('Ctrl Pts',(-0.587799206980913,1.10211922687916,
7.43509547532359));
#151901=CARTESIAN_POINT('Ctrl Pts',(-0.58475249770118,1.09579054188195,
7.39349824672118));
#151902=CARTESIAN_POINT('Ctrl Pts',(-0.578663341299355,1.08257770324263,
7.30876626426851));
#151903=CARTESIAN_POINT('Ctrl Pts',(-0.575775813423528,1.07598449667183,
7.26754705879483));
#151904=CARTESIAN_POINT('Ctrl Pts',(-0.57298620261301,1.06939092059987,
7.22732224306242));
#151905=CARTESIAN_POINT('Ctrl Pts',(-0.842449245,1.068630405,7.45253509));
#151906=CARTESIAN_POINT('Ctrl Pts',(-0.833566951,1.070029867,7.453539162));
#151907=CARTESIAN_POINT('Ctrl Pts',(-0.824682289,1.071428571,7.454522059));
#151908=CARTESIAN_POINT('Ctrl Pts',(-0.426480641,1.134117105,7.498574493));
#151909=CARTESIAN_POINT('Ctrl Pts',(-0.025852058,1.197973174,7.499955445));
#151910=CARTESIAN_POINT('Ctrl Pts',(-0.5776675,1.068630405,7.226949582));
#151911=CARTESIAN_POINT('Ctrl Pts',(-0.56905407,1.070029867,7.22763807400001));
#151912=CARTESIAN_POINT('Ctrl Pts',(-0.560439023,1.071428571,7.228306033));
#151913=CARTESIAN_POINT('Ctrl Pts',(-0.174321262,1.134117105,7.25824326300001));
#151914=CARTESIAN_POINT('Ctrl Pts',(0.212788494,1.197973174,7.246876641));
#151915=CARTESIAN_POINT('Ctrl Pts',(-0.57501968255,1.068630405,7.22469372692));
#151916=CARTESIAN_POINT('Ctrl Pts',(-0.56640894119,1.070029867,7.22537906312));
#151917=CARTESIAN_POINT('Ctrl Pts',(-0.55779659034,1.071428571,7.22604387274));
#151918=CARTESIAN_POINT('Ctrl Pts',(-0.17179966821,1.134117105,7.2558399507));
#151919=CARTESIAN_POINT('Ctrl Pts',(0.21517489952,1.197973174,7.24434585296));
#151920=CARTESIAN_POINT('Origin',(-0.0288748555719699,1.33885357237991,
-0.188821302331477));
#151921=CARTESIAN_POINT('Ctrl Pts',(-1.355629403,4.820162746,7.12213233));
#151922=CARTESIAN_POINT('Ctrl Pts',(-0.969698837,4.755280647,7.195590502));
#151923=CARTESIAN_POINT('Ctrl Pts',(-0.578090317,4.690053947,7.226915773));
#151924=CARTESIAN_POINT('Ctrl Pts',(-0.572170154643126,4.68906787893895,
7.22738933442862));
#151925=CARTESIAN_POINT('Ctrl Pts',(-0.566249992286254,4.68808181087793,
7.22786289585724));
#151926=CARTESIAN_POINT('Ctrl Pts',(-1.64350626427388,4.820162746,7.31794377208008));
#151927=CARTESIAN_POINT('Ctrl Pts',(-1.24696516389368,4.755280647,7.40700127323003));
#151928=CARTESIAN_POINT('Ctrl Pts',(-0.843122611572138,4.690053947,7.45268798177261));
#151929=CARTESIAN_POINT('Ctrl Pts',(-0.837017500589471,4.68906787893895,
7.45337865298712));
#151930=CARTESIAN_POINT('Ctrl Pts',(-0.830912389606805,4.68808181087793,
7.45406932420163));
#151931=CARTESIAN_POINT('',(-1.35103832279166,4.8193909209625,7.12300468390861));
#151932=CARTESIAN_POINT('Origin',(0.0169038419875292,4.69643176852073,-0.198295171745094));
#151933=CARTESIAN_POINT('Origin',(-2.49805601449516,5.70976516819263,14.5140475055271));
#151934=CARTESIAN_POINT('Ctrl Pts',(-2.118148151,4.690053947,6.933682168));
#151935=CARTESIAN_POINT('Ctrl Pts',(-1.7374959,4.755711878,7.049966394));
#151936=CARTESIAN_POINT('Ctrl Pts',(-1.346401839,4.820155008,7.123882515));
#151937=CARTESIAN_POINT('Ctrl Pts',(-1.954774922,4.690053947,7.240777238));
#151938=CARTESIAN_POINT('Ctrl Pts',(-1.557263457,4.755711878,7.348092436));
#151939=CARTESIAN_POINT('Ctrl Pts',(-1.150393323,4.820155008,7.411247884));
#151940=CARTESIAN_POINT('Origin',(0.0771176323196965,4.55371945316075,-0.175153269118729));
#151941=CARTESIAN_POINT('Ctrl Pts',(-2.854983464,4.820162746,6.664200584));
#151942=CARTESIAN_POINT('Ctrl Pts',(-2.493867074,4.755280647,6.818905009));
#151943=CARTESIAN_POINT('Ctrl Pts',(-2.118148151,4.690053947,6.933682168));
#151944=CARTESIAN_POINT('Ctrl Pts',(-2.1124682015092,4.68906787912114,6.93541731740534));
#151945=CARTESIAN_POINT('Ctrl Pts',(-2.10678825201842,4.68808181124226,
6.93715246681066));
#151946=CARTESIAN_POINT('Ctrl Pts',(-3.1782235951834,4.820162746,6.79354904841143));
#151947=CARTESIAN_POINT('Ctrl Pts',(-2.81009813513517,4.755280647,6.96576904967454));
#151948=CARTESIAN_POINT('Ctrl Pts',(-2.4255184898198,4.690053947,7.09720183980452));
#151949=CARTESIAN_POINT('Ctrl Pts',(-2.41970458791905,4.68906787912114,
7.0991887815412));
#151950=CARTESIAN_POINT('Ctrl Pts',(-2.41389068601829,4.68808181124226,
7.1011757232779));
#151951=CARTESIAN_POINT('',(-2.85068725016658,4.81939092091803,6.66603948951303));
#151952=CARTESIAN_POINT('Origin',(0.0591363730587224,4.69643183310118,-0.190025564315469));
#151953=CARTESIAN_POINT('Origin',(-5.55973958744884,5.70977447183052,13.6376944220212));
#151954=CARTESIAN_POINT('Ctrl Pts',(-3.559163733,4.690053947,6.316237292));
#151955=CARTESIAN_POINT('Ctrl Pts',(-3.212408591,4.755711878,6.511631839));
#151956=CARTESIAN_POINT('Ctrl Pts',(-2.846347872,4.820155008,6.667893505));
#151957=CARTESIAN_POINT('Ctrl Pts',(-3.465626441,4.690053947,6.651273064));
#151958=CARTESIAN_POINT('Ctrl Pts',(-3.100478168,4.755711878,6.841532507));
#151959=CARTESIAN_POINT('Ctrl Pts',(-2.716696986,4.820155008,6.99067646800001));
#151960=CARTESIAN_POINT('Origin',(0.112967294143578,4.55371942937115,-0.154479983497169));
#151961=CARTESIAN_POINT('Ctrl Pts',(-4.22084167,4.820162746,5.894658226));
#151962=CARTESIAN_POINT('Ctrl Pts',(-3.90142486,4.755280647,6.123375096));
#151963=CARTESIAN_POINT('Ctrl Pts',(-3.559163733,4.690053947,6.31623729200001));
#151964=CARTESIAN_POINT('Ctrl Pts',(-3.55398958340173,4.68906787912089,
6.31915289583355));
#151965=CARTESIAN_POINT('Ctrl Pts',(-3.54881543380346,4.68808181124179,
6.32206849966711));
#151966=CARTESIAN_POINT('Ctrl Pts',(-4.56433072332386,4.820162746,5.95149552225326));
#151967=CARTESIAN_POINT('Ctrl Pts',(-4.241834042112,4.755280647,6.19882520615937));
#151968=CARTESIAN_POINT('Ctrl Pts',(-3.89449981884596,4.690053947,6.40985842741688));
#151969=CARTESIAN_POINT('Ctrl Pts',(-3.88924897646275,4.68906787912089,
6.41304873262789));
#151970=CARTESIAN_POINT('Ctrl Pts',(-3.88399813407952,4.6880818112418,6.41623903783889));
#151971=CARTESIAN_POINT('',(-4.21704120960913,4.81939092092061,5.89737769746916));
#151972=CARTESIAN_POINT('Origin',(0.0986037219471031,4.69643188759991,-0.172870347922783));
#151973=CARTESIAN_POINT('Origin',(-8.36147418014773,5.70977704265914,12.1237057521521));
#151974=CARTESIAN_POINT('Ctrl Pts',(-4.833756773,4.690053947,5.403452179));
#151975=CARTESIAN_POINT('Ctrl Pts',(-4.537112626,4.755711878,5.668820616));
#151976=CARTESIAN_POINT('Ctrl Pts',(-4.213201843,4.820155008,5.900121205));
#151977=CARTESIAN_POINT('Ctrl Pts',(-4.814429119,4.690053947,5.75076275500001));
#151978=CARTESIAN_POINT('Ctrl Pts',(-4.498717966,4.755711878,6.015070122));
#151979=CARTESIAN_POINT('Ctrl Pts',(-4.155970918,4.820155008,6.24322879));
#151980=CARTESIAN_POINT('Origin',(0.143534806453094,4.5537193991147,-0.126583667889788));
#151981=CARTESIAN_POINT('Ctrl Pts',(-5.389338011,4.820162746,4.8494882));
#151982=CARTESIAN_POINT('Ctrl Pts',(-5.12655635500001,4.755280647,5.14152297));
#151983=CARTESIAN_POINT('Ctrl Pts',(-4.833756773,4.690053947,5.403452179));
#151984=CARTESIAN_POINT('Ctrl Pts',(-4.82933036048759,4.68906787905874,
5.40741190708487));
#151985=CARTESIAN_POINT('Ctrl Pts',(-4.82490394797516,4.68808181111747,
5.41137163516975));
#151986=CARTESIAN_POINT('Ctrl Pts',(-5.73701481973306,4.820162746,4.83115667900776));
#151987=CARTESIAN_POINT('Ctrl Pts',(-5.4752265023282,4.755280647,5.14203118713937));
#151988=CARTESIAN_POINT('Ctrl Pts',(-5.18137866555228,4.690053947,5.42279715860608));
#151989=CARTESIAN_POINT('Ctrl Pts',(-5.17693640599519,4.68906787905874,
5.42704165240171));
#151990=CARTESIAN_POINT('Ctrl Pts',(-5.17249414643811,4.6880818111175,5.43128614619734));
#151991=CARTESIAN_POINT('',(-5.38621100963435,4.81939092093662,4.85296107894373));
#151992=CARTESIAN_POINT('Origin',(0.1334604208639,4.69643183788284,-0.147631864610709));
#151993=CARTESIAN_POINT('Origin',(-10.7723631184045,5.70979140998744,10.0429141545461));
#151994=CARTESIAN_POINT('Ctrl Pts',(-5.88232872,4.690053947,4.238007649));
#151995=CARTESIAN_POINT('Ctrl Pts',(-5.649666317,4.755711878,4.560941642));
#151996=CARTESIAN_POINT('Ctrl Pts',(-5.383051178,4.820155008,4.856465795));
#151997=CARTESIAN_POINT('Ctrl Pts',(-5.938114442,4.690053947,4.58135317));
#151998=CARTESIAN_POINT('Ctrl Pts',(-5.686602712,4.755711878,4.907349744));
#151999=CARTESIAN_POINT('Ctrl Pts',(-5.400916269,4.820155008,5.203854673));
#152000=CARTESIAN_POINT('Origin',(0.16739088947738,4.55371943555998,-0.0927685709538006));
#152001=CARTESIAN_POINT('Ctrl Pts',(-6.305834896,4.820162746,3.577561496));
#152002=CARTESIAN_POINT('Ctrl Pts',(-6.111975772,4.755280647,3.919258944));
#152003=CARTESIAN_POINT('Ctrl Pts',(-5.88232872,4.690053947,4.238007649));
#152004=CARTESIAN_POINT('Ctrl Pts',(-5.87885701914578,4.68906787908345,
4.24282634857307));
#152005=CARTESIAN_POINT('Ctrl Pts',(-5.87538531829157,4.68808181116689,
4.24764504814613));
#152006=CARTESIAN_POINT('Ctrl Pts',(-6.6414424790535,4.820162746,3.48491831938665));
#152007=CARTESIAN_POINT('Ctrl Pts',(-6.45260345686075,4.755280647,3.84480150382246));
#152008=CARTESIAN_POINT('Ctrl Pts',(-6.22598200346879,4.690053947,4.18217192170176));
#152009=CARTESIAN_POINT('Ctrl Pts',(-6.22255604225364,4.68906787908345,
4.18727213595549));
#152010=CARTESIAN_POINT('Ctrl Pts',(-6.21913008103849,4.68808181116689,
4.19237235020922));
#152011=CARTESIAN_POINT('',(-6.3035275691543,4.81939092093462,3.58162539391593));
#152012=CARTESIAN_POINT('Origin',(0.162076923735922,4.69643187830107,-0.115490408366731));
#152013=CARTESIAN_POINT('Origin',(-12.6789187057329,5.70972183643974,7.49205957161615));
#152014=CARTESIAN_POINT('Ctrl Pts',(-6.655849513,4.690053947,2.874398591));
#152015=CARTESIAN_POINT('Ctrl Pts',(-6.49804789100001,4.755711878,3.239798106));
#152016=CARTESIAN_POINT('Ctrl Pts',(-6.301195022,4.820155008,3.585727442));
#152017=CARTESIAN_POINT('Ctrl Pts',(-6.784140134,4.690053947,3.197724603));
#152018=CARTESIAN_POINT('Ctrl Pts',(-6.608588236,4.755711878,3.570167146));
#152019=CARTESIAN_POINT('Ctrl Pts',(-6.393320778,4.820155008,3.921154095));
#152020=CARTESIAN_POINT('Origin',(0.183420107088528,4.55371942284746,-0.0546157082920951));
#152021=CARTESIAN_POINT('Ctrl Pts',(-6.92747795,4.820162746,2.138351993));
#152022=CARTESIAN_POINT('Ctrl Pts',(-6.811605995,4.755280647,2.513734725));
#152023=CARTESIAN_POINT('Ctrl Pts',(-6.655849513,4.690053947,2.874398591));
#152024=CARTESIAN_POINT('Ctrl Pts',(-6.65349485690423,4.68906787923068,
2.87985094431266));
#152025=CARTESIAN_POINT('Ctrl Pts',(-6.65114020080846,4.68808181146138,
2.88530329762533));
#152026=CARTESIAN_POINT('Ctrl Pts',(-7.23532366957013,4.820162746,1.97572905226316));
#152027=CARTESIAN_POINT('Ctrl Pts',(-7.12826384637026,4.755280647,2.36779317546382));
#152028=CARTESIAN_POINT('Ctrl Pts',(-6.97946534366401,4.690053947,2.74599297495909));
#152029=CARTESIAN_POINT('Ctrl Pts',(-6.97721587515433,4.68906787923068,
2.75171042858842));
#152030=CARTESIAN_POINT('Ctrl Pts',(-6.97496640664463,4.68808181146136,
2.75742788221773));
#152031=CARTESIAN_POINT('',(-6.92609818485928,4.81939092094391,2.14281688622834));
#152032=CARTESIAN_POINT('Origin',(0.183114619191084,4.69643185336553,-0.0779485369318891));
#152033=CARTESIAN_POINT('Origin',(-13.993262706542,5.7097470643807,4.59137507535894));
#152034=CARTESIAN_POINT('Ctrl Pts',(-7.118150181,4.690053947,1.376385849));
#152035=CARTESIAN_POINT('Ctrl Pts',(-7.042587967,4.755711878,1.767165211));
#152036=CARTESIAN_POINT('Ctrl Pts',(-6.924701991,4.820155008,2.147324459));
#152037=CARTESIAN_POINT('Ctrl Pts',(-7.312946974,4.690053947,1.664573988));
#152038=CARTESIAN_POINT('Ctrl Pts',(-7.22156351800001,4.755711878,2.0660475));
#152039=CARTESIAN_POINT('Ctrl Pts',(-7.086780713,4.820155008,2.455104709));
#152040=CARTESIAN_POINT('Origin',(0.190872296101794,4.55371947175156,-0.0139088517423921));
#152041=CARTESIAN_POINT('Ctrl Pts',(-7.225199835,4.820162746,0.599155527));
#152042=CARTESIAN_POINT('Ctrl Pts',(-7.192733093,4.755280647,0.990671065));
#152043=CARTESIAN_POINT('Ctrl Pts',(-7.118150181,4.690053947,1.376385849));
#152044=CARTESIAN_POINT('Ctrl Pts',(-7.11702267001631,4.68906787902937,
1.38221691195886));
#152045=CARTESIAN_POINT('Ctrl Pts',(-7.11589515903266,4.68808181105874,
1.38804797491772));
#152046=CARTESIAN_POINT('Ctrl Pts',(-7.49088916700958,4.820162746,0.374156890991696));
#152047=CARTESIAN_POINT('Ctrl Pts',(-7.47061453979235,4.755280647,0.780069469419929));
#152048=CARTESIAN_POINT('Ctrl Pts',(-7.40659664040584,4.690053947,1.18141444721225));
#152049=CARTESIAN_POINT('Ctrl Pts',(-7.40562884654026,4.68906787902937,
1.18748180042454));
#152050=CARTESIAN_POINT('Ctrl Pts',(-7.4046610526747,4.68808181105874,1.19354915363682));
#152051=CARTESIAN_POINT('',(-7.22481214736115,4.81939092093405,0.603812642471597));
#152052=CARTESIAN_POINT('Origin',(0.195589907817557,4.69643185065517,-0.0367618823269955));
#152053=CARTESIAN_POINT('Origin',(-14.6535586857437,5.70979310765313,1.47594165616264));
#152054=CARTESIAN_POINT('Ctrl Pts',(-7.24761405700001,4.690053947,-0.185985165));
#152055=CARTESIAN_POINT('Ctrl Pts',(-7.257824457,4.755711878,0.211901635));
#152056=CARTESIAN_POINT('Ctrl Pts',(-7.224417591,4.820155008,0.608514971));
#152057=CARTESIAN_POINT('Ctrl Pts',(-7.49980854000001,4.690053947,0.053589743));
#152058=CARTESIAN_POINT('Ctrl Pts',(-7.496866517,4.755711878,0.465321769));
#152059=CARTESIAN_POINT('Ctrl Pts',(-7.448870658,4.820155008,0.874257356));
#152060=CARTESIAN_POINT('Origin',(0.189399783009803,4.55371943452198,0.0274482381966176));
#152061=CARTESIAN_POINT('Ctrl Pts',(-7.185079405,4.820162746,-0.968056785));
#152062=CARTESIAN_POINT('Ctrl Pts',(-7.23753598500001,4.755280647,-0.578715273));
#152063=CARTESIAN_POINT('Ctrl Pts',(-7.247614057,4.690053947,-0.185985165));
#152064=CARTESIAN_POINT('Ctrl Pts',(-7.24776641279696,4.6890678788451,-0.18004804641253));
#152065=CARTESIAN_POINT('Ctrl Pts',(-7.24791876859394,4.68808181069019,
-0.174110927825061));
#152066=CARTESIAN_POINT('Ctrl Pts',(-7.39618901257076,4.820162746,-1.2449104313802));
#152067=CARTESIAN_POINT('Ctrl Pts',(-7.46364760078705,4.755280647,-0.844129417606408));
#152068=CARTESIAN_POINT('Ctrl Pts',(-7.48740371130746,4.690053947,-0.438405706039374));
#152069=CARTESIAN_POINT('Ctrl Pts',(-7.48776284558941,4.6890678788451,-0.432272155949239));
#152070=CARTESIAN_POINT('Ctrl Pts',(-7.48812197987134,4.68808181069019,
-0.426138605859105));
#152071=CARTESIAN_POINT('',(-7.18570192408644,4.81939092093424,-0.963425209266199));
#152072=CARTESIAN_POINT('Origin',(0.198919785553169,4.69643189437622,0.00614363754179073));
#152073=CARTESIAN_POINT('Origin',(-14.6279827186348,5.70976925426145,-1.70861569320879));
#152074=CARTESIAN_POINT('Ctrl Pts',(-7.038187555,4.690053947,-1.73965972));
#152075=CARTESIAN_POINT('Ctrl Pts',(-7.133693143,4.755711878,-1.353270226));
#152076=CARTESIAN_POINT('Ctrl Pts',(-7.186327454,4.820155008,-0.958748));
#152077=CARTESIAN_POINT('Ctrl Pts',(-7.335987395,4.690053947,-1.559900299));
#152078=CARTESIAN_POINT('Ctrl Pts',(-7.421624369,4.755711878,-1.157161891));
#152079=CARTESIAN_POINT('Ctrl Pts',(-7.46265969,4.820155008,-0.7474693));
#152080=CARTESIAN_POINT('Origin',(0.179071147294614,4.55371942552132,0.0675218736889965));
#152081=CARTESIAN_POINT('Ctrl Pts',(-6.808992648,4.820162746,-2.490003838));
#152082=CARTESIAN_POINT('Ctrl Pts',(-6.943919739,4.755280647,-2.121041529));
#152083=CARTESIAN_POINT('Ctrl Pts',(-7.038187555,4.690053947,-1.73965972));
#152084=CARTESIAN_POINT('Ctrl Pts',(-7.03961265330949,4.6890678791791,-1.7338941618876));
#152085=CARTESIAN_POINT('Ctrl Pts',(-7.04103775161898,4.68808181135819,
-1.72812860377519));
#152086=CARTESIAN_POINT('Ctrl Pts',(-6.95565128071148,4.820162746,-2.80576712519848));
#152087=CARTESIAN_POINT('Ctrl Pts',(-7.10768879513469,4.755280647,-2.42885775111912));
#152088=CARTESIAN_POINT('Ctrl Pts',(-7.21810810577893,4.690053947,-2.03772649589799));
#152089=CARTESIAN_POINT('Ctrl Pts',(-7.21977737509705,4.6890678791791,-2.03181355005648));
#152090=CARTESIAN_POINT('Ctrl Pts',(-7.22144664441517,4.68808181135819,
-2.02590060421497));
#152091=CARTESIAN_POINT('',(-6.81059626507071,4.819390920953,-2.48561436915926));
#152092=CARTESIAN_POINT('Origin',(0.192948563491753,4.69643189277552,0.0487619033756873));
#152093=CARTESIAN_POINT('Origin',(-13.9185422296696,5.7097552877665,-4.81320545378816));
#152094=CARTESIAN_POINT('Ctrl Pts',(-6.499663225,4.690053947,-3.211989719));
#152095=CARTESIAN_POINT('Ctrl Pts',(-6.675998265,4.755711878,-2.855164676));
#152096=CARTESIAN_POINT('Ctrl Pts',(-6.812212632,4.820155008,-2.481180981));
#152097=CARTESIAN_POINT('Ctrl Pts',(-6.829143632,4.690053947,-3.100451136));
#152098=CARTESIAN_POINT('Ctrl Pts',(-6.999355314,4.755711878,-2.725537947));
#152099=CARTESIAN_POINT('Ctrl Pts',(-7.12750304900001,4.820155008,-2.334245122));
#152100=CARTESIAN_POINT('Origin',(0.160369492462258,4.55371938751372,0.104438319995822));
#152101=CARTESIAN_POINT('Ctrl Pts',(-6.11452496300001,4.820162746,-3.895521079));
#152102=CARTESIAN_POINT('Ctrl Pts',(-6.32561352300001,4.755280647,-3.564190239));
#152103=CARTESIAN_POINT('Ctrl Pts',(-6.499663225,4.690053947,-3.211989719));
#152104=CARTESIAN_POINT('Ctrl Pts',(-6.50229443031012,4.68906787901235,
-3.20666530954798));
#152105=CARTESIAN_POINT('Ctrl Pts',(-6.50492563562025,4.6880818110247,-3.20134090009595));
#152106=CARTESIAN_POINT('Ctrl Pts',(-6.18987502456724,4.820162746,-4.23542926647455));
#152107=CARTESIAN_POINT('Ctrl Pts',(-6.41938236070255,4.755280647,-3.90001539587208));
#152108=CARTESIAN_POINT('Ctrl Pts',(-6.61130178712863,4.690053947,-3.54176546025212));
#152109=CARTESIAN_POINT('Ctrl Pts',(-6.61420313891565,4.68906787901235,
-3.53634959844873));
#152110=CARTESIAN_POINT('Ctrl Pts',(-6.61710449070265,4.68808181102469,
-3.53093373664535));
#152111=CARTESIAN_POINT('',(-6.11703469421881,4.81939092098298,-3.89157896362748));
#152112=CARTESIAN_POINT('Origin',(0.177955156142423,4.69643186978763,0.089100100086858));
#152113=CARTESIAN_POINT('Origin',(-12.5587322634811,5.70978015226369,-7.69292888315619));
#152114=CARTESIAN_POINT('Ctrl Pts',(-5.657221867,4.690053947,-4.534130649));
#152115=CARTESIAN_POINT('Ctrl Pts',(-5.906141128,4.755711878,-4.223554798));
#152116=CARTESIAN_POINT('Ctrl Pts',(-6.119566318,4.820155008,-3.887596697));
#152117=CARTESIAN_POINT('Ctrl Pts',(-6.002976704,4.690053947,-4.496028325));
#152118=CARTESIAN_POINT('Ctrl Pts',(-6.249804185,4.755711878,-4.166470877));
#152119=CARTESIAN_POINT('Ctrl Pts',(-6.459072287,4.820155008,-3.811874236));
#152120=CARTESIAN_POINT('Origin',(0.134168952170949,4.55371938671085,0.136471286468549));
#152121=CARTESIAN_POINT('Ctrl Pts',(-5.134148886,4.820162746,-5.118888084));
#152122=CARTESIAN_POINT('Ctrl Pts',(-5.411528649,4.755280647,-4.840681376));
#152123=CARTESIAN_POINT('Ctrl Pts',(-5.657221867,4.690053947,-4.534130649));
#152124=CARTESIAN_POINT('Ctrl Pts',(-5.66093614652675,4.68906787909637,
-4.52949635303336));
#152125=CARTESIAN_POINT('Ctrl Pts',(-5.66465042605351,4.68808181119276,
-4.52486205706673));
#152126=CARTESIAN_POINT('Ctrl Pts',(-5.13466709208506,4.820162746,-5.46704744287442));
#152127=CARTESIAN_POINT('Ctrl Pts',(-5.43091274263443,4.755280647,-5.18881265472693));
#152128=CARTESIAN_POINT('Ctrl Pts',(-5.69535834553527,4.690053947,-4.880195407032));
#152129=CARTESIAN_POINT('Ctrl Pts',(-5.69935611517983,4.68906787909637,
-4.87552987033527));
#152130=CARTESIAN_POINT('Ctrl Pts',(-5.70335388482441,4.68808181119276,
-4.87086433363855));
#152131=CARTESIAN_POINT('',(-5.13744737884062,4.81939092094632,-5.11557765092014));
#152132=CARTESIAN_POINT('Origin',(0.154640799092037,4.69643183018118,0.125272107351143));
#152133=CARTESIAN_POINT('Origin',(-10.611299383607,5.70977832312957,-10.2127662554641));
#152134=CARTESIAN_POINT('Ctrl Pts',(-4.550255102,4.690053947,-5.644260669));
#152135=CARTESIAN_POINT('Ctrl Pts',(-4.860119396,4.755711878,-5.394456192));
#152136=CARTESIAN_POINT('Ctrl Pts',(-5.14077588500001,4.820155008,-5.112232712));
#152137=CARTESIAN_POINT('Ctrl Pts',(-4.896117256,4.690053947,-5.681376225));
#152138=CARTESIAN_POINT('Ctrl Pts',(-5.208019157,4.755711878,-5.41258426));
#152139=CARTESIAN_POINT('Ctrl Pts',(-5.488622484,4.820155008,-5.11126434800001));
#152140=CARTESIAN_POINT('Origin',(0.101694846917463,4.55371946035496,0.162122973855));
#152141=CARTESIAN_POINT('Ctrl Pts',(-3.913705713,4.820162746,-6.102901571));
#152142=CARTESIAN_POINT('Ctrl Pts',(-4.24440671,4.755280647,-5.890827631));
#152143=CARTESIAN_POINT('Ctrl Pts',(-4.550255102,4.690053947,-5.644260669));
#152144=CARTESIAN_POINT('Ctrl Pts',(-4.55487878052238,4.68906787906646,
-5.6405331804915));
#152145=CARTESIAN_POINT('Ctrl Pts',(-4.55950245904475,4.68808181113291,
-5.63680569198298));
#152146=CARTESIAN_POINT('Ctrl Pts',(-3.83936783390739,4.820162746,-6.44303255698771));
#152147=CARTESIAN_POINT('Ctrl Pts',(-4.18849967985375,4.755280647,-6.23498680147196));
#152148=CARTESIAN_POINT('Ctrl Pts',(-4.51310627696747,4.690053947,-5.99043284123748));
#152149=CARTESIAN_POINT('Ctrl Pts',(-4.5180135336036,4.68906787906646,-5.98673578438489));
#152150=CARTESIAN_POINT('Ctrl Pts',(-4.52292079023975,4.68808181113291,
-5.9830387275323));
#152151=CARTESIAN_POINT('',(-3.91763873447699,4.81939092094378,-6.10037761276723));
#152152=CARTESIAN_POINT('Origin',(0.124095585144508,4.69643185631761,0.155586535597629));
#152153=CARTESIAN_POINT('Origin',(-8.16771175173436,5.70977057295254,-12.2550248833005));
#152154=CARTESIAN_POINT('Ctrl Pts',(-3.230523466,4.690053947,-6.49047133400001));
#152155=CARTESIAN_POINT('Ctrl Pts',(-3.586843883,4.755711878,-6.31311881));
#152156=CARTESIAN_POINT('Ctrl Pts',(-3.921608485,4.820155008,-6.097826407));
#152157=CARTESIAN_POINT('Ctrl Pts',(-3.560320807,4.690053947,-6.601069288));
#152158=CARTESIAN_POINT('Ctrl Pts',(-3.922712942,4.755711878,-6.405611219));
#152159=CARTESIAN_POINT('Ctrl Pts',(-4.261530793,4.820155008,-6.17165741900001));
#152160=CARTESIAN_POINT('Origin',(0.0644657034034357,4.55371945320907,0.180194127272911));
#152161=CARTESIAN_POINT('Ctrl Pts',(-2.510262011,4.820162746,-6.80155016400001));
#152162=CARTESIAN_POINT('Ctrl Pts',(-2.878821031,4.755280647,-6.665525334));
#152163=CARTESIAN_POINT('Ctrl Pts',(-3.230523466,4.690053947,-6.490471334));
#152164=CARTESIAN_POINT('Ctrl Pts',(-3.23584034540781,4.6890678790529,-6.48782494627211));
#152165=CARTESIAN_POINT('Ctrl Pts',(-3.24115722481561,4.68808181110582,
-6.48517855854421));
#152166=CARTESIAN_POINT('Ctrl Pts',(-2.36454400263469,4.820162746,-7.11774863001447));
#152167=CARTESIAN_POINT('Ctrl Pts',(-2.75023702718094,4.755280647,-6.98961989444871));
#152168=CARTESIAN_POINT('Ctrl Pts',(-3.11982637500247,4.690053947,-6.82056429338084));
#152169=CARTESIAN_POINT('Ctrl Pts',(-3.12541366072251,4.6890678790529,-6.81800858675319));
#152170=CARTESIAN_POINT('Ctrl Pts',(-3.13100094644254,4.68808181110579,
-6.81545288012554));
#152171=CARTESIAN_POINT('',(-2.51464565709642,4.81939092092416,-6.79993069751606));
#152172=CARTESIAN_POINT('Origin',(0.087747766164829,4.69643188494964,0.178625850837789));
#152173=CARTESIAN_POINT('Origin',(-5.34229045964354,5.70976774922248,-13.7243426394469));
#152174=CARTESIAN_POINT('Ctrl Pts',(-1.759736143,4.690053947,-7.03319477300001));
#152175=CARTESIAN_POINT('Ctrl Pts',(-2.145851537,4.755711878,-6.936587009));
#152176=CARTESIAN_POINT('Ctrl Pts',(-2.519071031,4.820155008,-6.798292516));
#152177=CARTESIAN_POINT('Ctrl Pts',(-2.058047714,4.690053947,-7.212103688));
#152178=CARTESIAN_POINT('Ctrl Pts',(-2.45398503,4.755711878,-7.099118916));
#152179=CARTESIAN_POINT('Ctrl Pts',(-2.835174659,4.820155008,-6.943470649));
#152180=CARTESIAN_POINT('Origin',(0.0242221099538867,4.55371947014683,0.189839453343754));
#152181=CARTESIAN_POINT('Ctrl Pts',(-0.989441248,4.820162746,-7.182165831));
#152182=CARTESIAN_POINT('Ctrl Pts',(-1.37862488,4.755280647,-7.12855048));
#152183=CARTESIAN_POINT('Ctrl Pts',(-1.759736143,4.690053947,-7.033194773));
#152184=CARTESIAN_POINT('Ctrl Pts',(-1.76549760821494,4.6890678796763,-7.03175322917209));
#152185=CARTESIAN_POINT('Ctrl Pts',(-1.77125907342988,4.68808181235263,
-7.03031168534417));
#152186=CARTESIAN_POINT('Ctrl Pts',(-0.779156721531463,4.820162746,-7.4596466868318));
#152187=CARTESIAN_POINT('Ctrl Pts',(-1.18337634817097,4.755280647,-7.41742612955641));
#152188=CARTESIAN_POINT('Ctrl Pts',(-1.58066685966322,4.690053947,-7.33177373946158));
#152189=CARTESIAN_POINT('Ctrl Pts',(-1.58667291533359,4.6890678796763,-7.33047888592662));
#152190=CARTESIAN_POINT('Ctrl Pts',(-1.59267897100398,4.68808181235263,
-7.32918403239166));
#152191=CARTESIAN_POINT('',(-0.994070543459548,4.81939092091392,-7.18152658034752));
#152192=CARTESIAN_POINT('Origin',(0.0472970145023902,4.69643190404216,0.193313016087062));
#152193=CARTESIAN_POINT('Origin',(-2.26709724430376,5.70979447745367,-14.5520995818287));
#152194=CARTESIAN_POINT('Ctrl Pts',(-0.206665513,4.690053947,-7.24705384000001));
#152195=CARTESIAN_POINT('Ctrl Pts',(-0.604521557,4.755711878,-7.235708109));
#152196=CARTESIAN_POINT('Ctrl Pts',(-0.998744615,4.820155008,-7.180878024));
#152197=CARTESIAN_POINT('Ctrl Pts',(-0.459542598,4.690053947,-7.485908135));
#152198=CARTESIAN_POINT('Ctrl Pts',(-0.870511505,4.755711878,-7.460679703));
#152199=CARTESIAN_POINT('Ctrl Pts',(-1.276248909,4.820155008,-7.390614908));
#152200=CARTESIAN_POINT('Origin',(-0.0171541142577276,4.55371940144747,
0.190607825220247));
#152201=CARTESIAN_POINT('Ctrl Pts',(0.577644689,4.820162746,-7.226951405));
#152202=CARTESIAN_POINT('Ctrl Pts',(0.186034238,4.755280647,-7.25825252900001));
#152203=CARTESIAN_POINT('Ctrl Pts',(-0.206665513,4.690053947,-7.24705384));
#152204=CARTESIAN_POINT('Ctrl Pts',(-0.212602171644338,4.68906787901444,
-7.24688454324418));
#152205=CARTESIAN_POINT('Ctrl Pts',(-0.218538830288674,4.6880818110289,
-7.24671524648837));
#152206=CARTESIAN_POINT('Ctrl Pts',(0.842663062086272,4.820162746,-7.4527399563928));
#152207=CARTESIAN_POINT('Ctrl Pts',(0.438817693973189,4.755280647,-7.49840176325853));
#152208=CARTESIAN_POINT('Ctrl Pts',(0.0324028813005472,4.690053947,-7.5001575948203));
#152209=CARTESIAN_POINT('Ctrl Pts',(0.0262588845073336,4.68906787901444,
-7.50018413869407));
#152210=CARTESIAN_POINT('Ctrl Pts',(0.0201148877141198,4.68808181102888,
-7.50021068256784));
#152211=CARTESIAN_POINT('',(0.572986204252882,4.81939092094349,-7.22732226279767));
#152212=CARTESIAN_POINT('Origin',(0.00463468354769389,4.69643187856393,
0.198960769951227));
#152213=CARTESIAN_POINT('Origin',(0.914164899364814,5.70976303909231,-14.6989833446639));
#152214=CARTESIAN_POINT('Ctrl Pts',(1.356068566,4.690053947,-7.122048725));
#152215=CARTESIAN_POINT('Ctrl Pts',(0.965075178000001,4.755711878,-7.19649554));
#152216=CARTESIAN_POINT('Ctrl Pts',(0.568281989,4.820155008,-7.227693656));
#152217=CARTESIAN_POINT('Ctrl Pts',(1.16045022,4.690053947,-7.409679837));
#152218=CARTESIAN_POINT('Ctrl Pts',(0.75366617,4.755711878,-7.473387399));
#152219=CARTESIAN_POINT('Ctrl Pts',(0.342352821,4.820155008,-7.49218222900001));
#152220=CARTESIAN_POINT('Origin',(-0.057728145566843,4.55371939146095,0.182464146260932));
#152221=CARTESIAN_POINT('Ctrl Pts',(2.117720602,4.820162746,-6.933812764));
#152222=CARTESIAN_POINT('Ctrl Pts',(1.741994603,4.755280647,-7.048566756));
#152223=CARTESIAN_POINT('Ctrl Pts',(1.356068566,4.690053947,-7.122048725));
#152224=CARTESIAN_POINT('Ctrl Pts',(1.35023430029195,4.68906787748777,-7.12315959415833));
#152225=CARTESIAN_POINT('Ctrl Pts',(1.3444000345839,4.68808180797554,-7.12427046331664));
#152226=CARTESIAN_POINT('Ctrl Pts',(2.42508085697513,4.820162746,-7.09735138887713));
#152227=CARTESIAN_POINT('Ctrl Pts',(2.04049310773383,4.755280647,-7.22876046452689));
#152228=CARTESIAN_POINT('Ctrl Pts',(1.64395750021218,4.690053947,-7.31784241626901));
#152229=CARTESIAN_POINT('Ctrl Pts',(1.63796284352882,4.68906787748777,-7.31918911933237));
#152230=CARTESIAN_POINT('Ctrl Pts',(1.63196818684546,4.68808180797554,-7.3205358223957));
#152231=CARTESIAN_POINT('',(2.11325075291932,4.81939092093509,-6.93517638828184));
#152232=CARTESIAN_POINT('Origin',(-0.0382443478991329,4.69643188114676,
0.195305453577753));
#152233=CARTESIAN_POINT('Origin',(4.05250436150527,5.7097037009075,-14.1583157295763));
#152234=CARTESIAN_POINT('Ctrl Pts',(2.855394386,4.690053947,-6.664024527));
#152235=CARTESIAN_POINT('Ctrl Pts',(2.489546071,4.755711878,-6.82078283800001));
#152236=CARTESIAN_POINT('Ctrl Pts',(2.108736358,4.820155008,-6.936550365));
#152237=CARTESIAN_POINT('Ctrl Pts',(2.726181675,4.690053947,-6.986983146));
#152238=CARTESIAN_POINT('Ctrl Pts',(2.342603253,4.755711878,-7.136647807));
#152239=CARTESIAN_POINT('Ctrl Pts',(1.944946514,4.820155008,-7.243423435));
#152240=CARTESIAN_POINT('Origin',(-0.0956029415668058,4.55371945245238,
0.165788556452092));
#152241=CARTESIAN_POINT('Ctrl Pts',(3.558774254,4.820162746,-6.31645674500001));
#152242=CARTESIAN_POINT('Ctrl Pts',(3.216501235,4.755280647,-6.509297835));
#152243=CARTESIAN_POINT('Ctrl Pts',(2.855394386,4.690053947,-6.664024527));
#152244=CARTESIAN_POINT('Ctrl Pts',(2.84993533537919,4.68906787914193,-6.66636361540654));
#152245=CARTESIAN_POINT('Ctrl Pts',(2.84447628475839,4.68808181128384,-6.66870270381308));
#152246=CARTESIAN_POINT('Ctrl Pts',(3.89410456666928,4.820162746,-6.41009855793305));
#152247=CARTESIAN_POINT('Ctrl Pts',(3.54675733240121,4.755280647,-6.62111036091056));
#152248=CARTESIAN_POINT('Ctrl Pts',(3.17864249231939,4.690053947,-6.79335306055965));
#152249=CARTESIAN_POINT('Ctrl Pts',(3.17307749804736,4.68906787914193,-6.79595694807676));
#152250=CARTESIAN_POINT('Ctrl Pts',(3.16751250377533,4.68808181128384,-6.79856083559384));
#152251=CARTESIAN_POINT('',(3.55470204576132,4.81939092093285,-6.31874937272934));
#152252=CARTESIAN_POINT('Origin',(-0.0793350926111663,4.69643185062215,
0.182517857647713));
#152253=CARTESIAN_POINT('Origin',(7.00174251657518,5.70979219759973,-12.9568246707818));
#152254=CARTESIAN_POINT('Ctrl Pts',(4.221205138,4.690053947,-5.894397949));
#152255=CARTESIAN_POINT('Ctrl Pts',(3.897608556,4.755711878,-6.12613791));
#152256=CARTESIAN_POINT('Ctrl Pts',(3.55058856,4.820155008,-6.321061689));
#152257=CARTESIAN_POINT('Ctrl Pts',(4.164439905,4.690053947,-6.237582888));
#152258=CARTESIAN_POINT('Ctrl Pts',(3.822002811,4.755711878,-6.466206494));
#152259=CARTESIAN_POINT('Ctrl Pts',(3.45659667,4.820155008,-6.655970212));
#152260=CARTESIAN_POINT('Origin',(-0.129007324901403,4.5537194263835,0.141360543891498));
#152261=CARTESIAN_POINT('Ctrl Pts',(4.833423576,4.820162746,-5.403750228));
#152262=CARTESIAN_POINT('Ctrl Pts',(4.540607845,4.755280647,-5.665661383));
#152263=CARTESIAN_POINT('Ctrl Pts',(4.221205138,4.690053947,-5.894397949));
#152264=CARTESIAN_POINT('Ctrl Pts',(4.21637655121232,4.68906787902086,-5.89785588575582));
#152265=CARTESIAN_POINT('Ctrl Pts',(4.21154796442465,4.68808181104171,-5.90131382251167));
#152266=CARTESIAN_POINT('Ctrl Pts',(5.18104427449542,4.820162746,-5.4231166428033));
#152267=CARTESIAN_POINT('Ctrl Pts',(4.88717912567789,4.755280647,-5.70386449521244));
#152268=CARTESIAN_POINT('Ctrl Pts',(4.56469769549388,4.690053947,-5.95121406428968));
#152269=CARTESIAN_POINT('Ctrl Pts',(4.55982256595072,4.68906787902086,-5.95495338407317));
#152270=CARTESIAN_POINT('Ctrl Pts',(4.55494743640757,4.68808181104171,-5.95869270385665));
#152271=CARTESIAN_POINT('',(4.82993942138855,4.81939092091076,-5.40686466020919));
#152272=CARTESIAN_POINT('Origin',(-0.116716233036883,4.69643189652617,0.161195976188948));
#152273=CARTESIAN_POINT('Origin',(9.62327638418686,5.70978009376185,-11.1486127013645));
#152274=CARTESIAN_POINT('Ctrl Pts',(5.38963702999999,4.690053947,-4.849155874));
#152275=CARTESIAN_POINT('Ctrl Pts',(5.123423198,4.755711878,-5.145041583));
#152276=CARTESIAN_POINT('Ctrl Pts',(4.826419186,4.820155008,-5.410007194));
#152277=CARTESIAN_POINT('Ctrl Pts',(5.407973553,4.690053947,-5.196520186));
#152278=CARTESIAN_POINT('Ctrl Pts',(5.122689766,4.755711878,-5.493412553));
#152279=CARTESIAN_POINT('Ctrl Pts',(4.806620207,4.820155008,-5.75729121900001));
#152280=CARTESIAN_POINT('Origin',(-0.156379662974808,4.55371942472877,0.110322979267742));
#152281=CARTESIAN_POINT('Ctrl Pts',(5.88206738500001,4.820162746,-4.238370357));
#152282=CARTESIAN_POINT('Ctrl Pts',(5.65240067800001,4.755280647,-4.557104901));
#152283=CARTESIAN_POINT('Ctrl Pts',(5.38963703000001,4.690053947,-4.849155874));
#152284=CARTESIAN_POINT('Ctrl Pts',(5.38566468745547,4.6890678791119,-4.85357096913988));
#152285=CARTESIAN_POINT('Ctrl Pts',(5.38169234491093,4.68808181122383,-4.85798606427976));
#152286=CARTESIAN_POINT('Ctrl Pts',(6.22572411048738,4.820162746,-4.18255582068996));
#152287=CARTESIAN_POINT('Ctrl Pts',(5.99908185506762,4.755280647,-4.51991226473341));
#152288=CARTESIAN_POINT('Ctrl Pts',(5.73731270770339,4.690053947,-4.83080291380854));
#152289=CARTESIAN_POINT('Ctrl Pts',(5.73335539957178,4.6890678791119,-4.83550281869043));
#152290=CARTESIAN_POINT('Ctrl Pts',(5.72939809144017,4.68808181122383,-4.84020272357233));
#152291=CARTESIAN_POINT('',(5.87933419816497,4.81939092091779,-4.24216096526778));
#152292=CARTESIAN_POINT('Origin',(-0.148639930760657,4.69643189193197,0.132336833229253));
#152293=CARTESIAN_POINT('Origin',(11.7947999796108,5.70976647600791,-8.8191591276217));
#152294=CARTESIAN_POINT('Ctrl Pts',(6.306055484,4.690053947,-3.577172659));
#152295=CARTESIAN_POINT('Ctrl Pts',(6.109672265,4.755711878,-3.92336883));
#152296=CARTESIAN_POINT('Ctrl Pts',(5.87657181600001,4.820155008,-4.245986775));
#152297=CARTESIAN_POINT('Ctrl Pts',(6.398636369,4.690053947,-3.912473977));
#152298=CARTESIAN_POINT('Ctrl Pts',(6.183845441,4.755711878,-4.263752746));
#152299=CARTESIAN_POINT('Ctrl Pts',(5.931891526,4.820155008,-4.589407688));
#152300=CARTESIAN_POINT('Origin',(-0.176439461085779,4.55371945041668,0.0741264761620436));
#152301=CARTESIAN_POINT('Ctrl Pts',(6.655672259,4.820162746,-2.874808998));
#152302=CARTESIAN_POINT('Ctrl Pts',(6.49989353800001,4.755280647,-3.235463259));
#152303=CARTESIAN_POINT('Ctrl Pts',(6.306055484,4.690053947,-3.577172659));
#152304=CARTESIAN_POINT('Ctrl Pts',(6.30312512740184,4.68906787905938,-3.58233846816018));
#152305=CARTESIAN_POINT('Ctrl Pts',(6.30019477080367,4.68808181111875,-3.58750427732035));
#152306=CARTESIAN_POINT('Ctrl Pts',(6.9792960067535,4.820162746,-2.74642333683019));
#152307=CARTESIAN_POINT('Ctrl Pts',(6.83047418407916,4.755280647,-3.12461396070996));
#152308=CARTESIAN_POINT('Ctrl Pts',(6.64165735389054,4.69005394700001,-3.48450878786627));
#152309=CARTESIAN_POINT('Ctrl Pts',(6.63880290589765,4.68906787905938,-3.48994951614247));
#152310=CARTESIAN_POINT('Ctrl Pts',(6.63594845790476,4.68808181111875,-3.49539024441867));
#152311=CARTESIAN_POINT('',(6.65381784207734,4.81939092093234,-2.87909853897346));
#152312=CARTESIAN_POINT('Origin',(-0.173613277267033,4.69643187308239,0.0972896797464246));
#152313=CARTESIAN_POINT('Origin',(13.4152092529715,5.70979856953057,-6.07757981371294));
#152314=CARTESIAN_POINT('Ctrl Pts',(6.927609792,4.690053947,-2.137924827));
#152315=CARTESIAN_POINT('Ctrl Pts',(6.81023984700001,4.755711878,-2.518243711));
#152316=CARTESIAN_POINT('Ctrl Pts',(6.651942479,4.820155008,-2.883428734));
#152317=CARTESIAN_POINT('Ctrl Pts',(7.090106059,4.690053947,-2.445484832));
#152318=CARTESIAN_POINT('Ctrl Pts',(6.955851376,4.755711878,-2.8347246));
#152319=CARTESIAN_POINT('Ctrl Pts',(6.779794189,4.820155008,-3.206928554));
#152320=CARTESIAN_POINT('Origin',(-0.188249734327377,4.55371942637612,0.0344642920532923));
#152321=CARTESIAN_POINT('Ctrl Pts',(7.118065296,4.820162746,-1.376824766));
#152322=CARTESIAN_POINT('Ctrl Pts',(7.0434586,4.755280647,-1.762534951));
#152323=CARTESIAN_POINT('Ctrl Pts',(6.927609792,4.690053947,-2.137924827));
#152324=CARTESIAN_POINT('Ctrl Pts',(6.92585844207668,4.68906787922757,-2.14359980149389));
#152325=CARTESIAN_POINT('Ctrl Pts',(6.92410709215334,4.68808181145512,-2.1492747759878));
#152326=CARTESIAN_POINT('Ctrl Pts',(7.4065237781206,4.820162746,-1.18187115117692));
#152327=CARTESIAN_POINT('Ctrl Pts',(7.34248113186987,4.755280647,-1.58321218054904));
#152328=CARTESIAN_POINT('Ctrl Pts',(7.23544548359059,4.690053947,-1.97528290426303));
#152329=CARTESIAN_POINT('Ctrl Pts',(7.23382736703296,4.68906787922757,-1.98121005227403));
#152330=CARTESIAN_POINT('Ctrl Pts',(7.23220925047533,4.68808181145512,-1.98713720028501));
#152331=CARTESIAN_POINT('',(7.11717635827304,4.81939092091954,-1.38141266451028));
#152332=CARTESIAN_POINT('Origin',(-0.190468596064708,4.69643185312465,0.0576933420284076));
#152333=CARTESIAN_POINT('Origin',(14.4079253287426,5.7097819075629,-3.05158571821218));
#152334=CARTESIAN_POINT('Ctrl Pts',(7.225236766,4.690053947,-0.598710006));
#152335=CARTESIAN_POINT('Ctrl Pts',(7.192368183,4.755711878,-0.995368314));
#152336=CARTESIAN_POINT('Ctrl Pts',(7.11627570400001,4.820155008,-1.386044769));
#152337=CARTESIAN_POINT('Ctrl Pts',(7.450050271,4.690053947,-0.864147535));
#152338=CARTESIAN_POINT('Ctrl Pts',(7.402609431,4.755711878,-1.273147882));
#152339=CARTESIAN_POINT('Ctrl Pts',(7.310681212,4.820155008,-1.674497005));
#152340=CARTESIAN_POINT('Origin',(-0.191257348511611,4.55371940857812,-0.00680959593364436));
#152341=CARTESIAN_POINT('Ctrl Pts',(7.24762551100001,4.820162746,0.185538262));
#152342=CARTESIAN_POINT('Ctrl Pts',(7.257679367,4.755280647,-0.207192467));
#152343=CARTESIAN_POINT('Ctrl Pts',(7.225236766,4.690053947,-0.598710006));
#152344=CARTESIAN_POINT('Ctrl Pts',(7.22474631313992,4.68906787866448,-0.604628794594373));
#152345=CARTESIAN_POINT('Ctrl Pts',(7.22425586027986,4.68808181032895,-0.610547583188746));
#152346=CARTESIAN_POINT('Ctrl Pts',(7.48743073003761,4.820162746,0.437944016577193));
#152347=CARTESIAN_POINT('Ctrl Pts',(7.51116182282811,4.755280647,0.0322188422676525));
#152348=CARTESIAN_POINT('Ctrl Pts',(7.49091222439734,4.69005394700001,-0.373694986478134));
#152349=CARTESIAN_POINT('Ctrl Pts',(7.49060609994492,4.68906787866448,-0.37983141179899));
#152350=CARTESIAN_POINT('Ctrl Pts',(7.49029997549253,4.68808181032895,-0.385967837119846));
#152351=CARTESIAN_POINT('',(7.24774361911353,4.81939092094578,0.180866530701085));
#152352=CARTESIAN_POINT('Origin',(-0.198417961527672,4.69643188297084,0.0153993912038071));
#152353=CARTESIAN_POINT('Origin',(14.7269736395706,5.70976965717986,0.117037973839281));
#152354=CARTESIAN_POINT('Ctrl Pts',(7.185019699,4.690053947,0.96849983));
#152355=CARTESIAN_POINT('Ctrl Pts',(7.238189376,4.755711878,0.574049398));
#152356=CARTESIAN_POINT('Ctrl Pts',(7.247859787,4.820155008,0.176149108));
#152357=CARTESIAN_POINT('Ctrl Pts',(7.461638412,4.690053947,0.75759634));
#152358=CARTESIAN_POINT('Ctrl Pts',(7.503229697,4.755711878,0.347959816));
#152359=CARTESIAN_POINT('Ctrl Pts',(7.499728906,4.820155008,-0.063767838));
#152360=CARTESIAN_POINT('Origin',(-0.185321689466242,4.55371943528727,-0.0477650473182711));
#152361=CARTESIAN_POINT('Ctrl Pts',(7.038294813,4.820162746,1.739225727));
#152362=CARTESIAN_POINT('Ctrl Pts',(7.13253911200001,4.755280647,1.357838106));
#152363=CARTESIAN_POINT('Ctrl Pts',(7.18501969900001,4.690053947,0.96849983));
#152364=CARTESIAN_POINT('Ctrl Pts',(7.18581307694984,4.68906787903698,0.962613988761047));
#152365=CARTESIAN_POINT('Ctrl Pts',(7.1866064548997,4.68808181107395,0.956728147522092));
#152366=CARTESIAN_POINT('Ctrl Pts',(7.21823374226126,4.820162746,2.03728140900129));
#152367=CARTESIAN_POINT('Ctrl Pts',(7.3286289343689,4.755280647,1.64614334688791));
#152368=CARTESIAN_POINT('Ctrl Pts',(7.39611223521212,4.690053947,1.24536649294527));
#152369=CARTESIAN_POINT('Ctrl Pts',(7.39713241745345,4.68906787903698,1.23930772842104));
#152370=CARTESIAN_POINT('Ctrl Pts',(7.39815259969477,4.68808181107395,1.23324896389681));
#152371=CARTESIAN_POINT('',(7.03941444328107,4.81939092092237,1.73468860818569));
#152372=CARTESIAN_POINT('Origin',(-0.197089488305159,4.69643185279569,-0.0276146278634712));
#152373=CARTESIAN_POINT('Origin',(14.3578677079183,5.70980883046184,3.28024211300596));
#152374=CARTESIAN_POINT('Ctrl Pts',(6.808839097,4.690053947,2.49042369));
#152375=CARTESIAN_POINT('Ctrl Pts',(6.945560879,4.755711878,2.116625199));
#152376=CARTESIAN_POINT('Ctrl Pts',(7.040542002,4.820155008,1.730106449));
#152377=CARTESIAN_POINT('Ctrl Pts',(7.124328633,4.690053947,2.343915853));
#152378=CARTESIAN_POINT('Ctrl Pts',(7.253007281,4.755711878,1.9527973));
#152379=CARTESIAN_POINT('Ctrl Pts',(7.33809761200001,4.820155008,1.549943043));
#152380=CARTESIAN_POINT('Origin',(-0.170721269218758,4.55371942967028,-0.086487117622841));
#152381=CARTESIAN_POINT('Ctrl Pts',(6.499861271,4.820162746,3.211588931));
#152382=CARTESIAN_POINT('Ctrl Pts',(6.673889256,4.755280647,2.859377679));
#152383=CARTESIAN_POINT('Ctrl Pts',(6.808839097,4.690053947,2.49042369));
#152384=CARTESIAN_POINT('Ctrl Pts',(6.81087920812824,4.68906787902435,2.4848460091877));
#152385=CARTESIAN_POINT('Ctrl Pts',(6.81291931925649,4.68808181104872,2.47926832837541));
#152386=CARTESIAN_POINT('Ctrl Pts',(6.61152016733784,4.820162746,3.54135778708215));
#152387=CARTESIAN_POINT('Ctrl Pts',(6.80341750242848,4.755280647,3.18309601847626));
#152388=CARTESIAN_POINT('Ctrl Pts',(6.95547825829419,4.690053947,2.80619601934055));
#152389=CARTESIAN_POINT('Ctrl Pts',(6.95777704455368,4.68906787902435,2.80049821431333));
#152390=CARTESIAN_POINT('Ctrl Pts',(6.96007583081316,4.68808181104872,2.79480040928613));
#152391=CARTESIAN_POINT('',(6.50193007160717,4.81939092090431,3.20739857423919));
#152392=CARTESIAN_POINT('Origin',(-0.186545351912871,4.69643183132373,-0.0693374519902629));
#152393=CARTESIAN_POINT('Origin',(13.3169049274491,5.709797452772,6.2900119976216));
#152394=CARTESIAN_POINT('Ctrl Pts',(6.114284746,4.690053947,3.895898106));
#152395=CARTESIAN_POINT('Ctrl Pts',(6.328165675,4.755711878,3.560229957));
#152396=CARTESIAN_POINT('Ctrl Pts',(6.50401629700001,4.820155008,3.203165935));
#152397=CARTESIAN_POINT('Ctrl Pts',(6.453893166,4.690053947,3.820636465));
#152398=CARTESIAN_POINT('Ctrl Pts',(6.663642306,4.755711878,3.466324153));
#152399=CARTESIAN_POINT('Ctrl Pts',(6.83334502900001,4.820155008,3.09118031));
#152400=CARTESIAN_POINT('Origin',(-0.148137647083667,4.55371941171401,-0.121165073524416));
#152401=CARTESIAN_POINT('Ctrl Pts',(5.65750144,4.820162746,4.533781805));
#152402=CARTESIAN_POINT('Ctrl Pts',(5.903175755,4.755280647,4.227215929));
#152403=CARTESIAN_POINT('Ctrl Pts',(6.114284746,4.690053947,3.895898106));
#152404=CARTESIAN_POINT('Ctrl Pts',(6.11747619650953,4.68906787916857,3.89088939258605));
#152405=CARTESIAN_POINT('Ctrl Pts',(6.12066764701905,4.68808181133714,3.88588067917208));
#152406=CARTESIAN_POINT('Ctrl Pts',(5.69565925764326,4.820162746,4.87984421090298));
#152407=CARTESIAN_POINT('Ctrl Pts',(5.96008583042904,4.755280647,4.57121065817288));
#152408=CARTESIAN_POINT('Ctrl Pts',(6.18961384778584,4.690053947,4.23581093858657));
#152409=CARTESIAN_POINT('Ctrl Pts',(6.19308374882831,4.68906787916857,4.23074051690108));
#152410=CARTESIAN_POINT('Ctrl Pts',(6.19655364987078,4.68808181133714,4.22567009521558));
#152411=CARTESIAN_POINT('',(5.66042267628095,4.81939092091094,4.53013414754876));
#152412=CARTESIAN_POINT('Origin',(-0.167278715930961,4.69643185358206,-0.107818263156557));
#152413=CARTESIAN_POINT('Origin',(11.6532789256992,5.70978109174142,9.00560699204281));
#152414=CARTESIAN_POINT('Ctrl Pts',(5.133833235,4.690053947,5.119204656));
#152415=CARTESIAN_POINT('Ctrl Pts',(5.414872477,4.755711878,4.83736232));
#152416=CARTESIAN_POINT('Ctrl Pts',(5.663370019,4.820155008,4.526448942));
#152417=CARTESIAN_POINT('Ctrl Pts',(5.481680828,4.690053947,5.11870836300001));
#152418=CARTESIAN_POINT('Ctrl Pts',(5.762692823,4.755711878,4.81776954));
#152419=CARTESIAN_POINT('Ctrl Pts',(6.00907282800001,4.820155008,4.487877421));
#152420=CARTESIAN_POINT('Origin',(-0.118627120782181,4.55371940082309,-0.150177319917639));
#152421=CARTESIAN_POINT('Ctrl Pts',(4.55060313,4.820162746,5.643980081));
#152422=CARTESIAN_POINT('Ctrl Pts',(4.856436318,4.755280647,5.39739426));
#152423=CARTESIAN_POINT('Ctrl Pts',(5.133833235,4.690053947,5.119204656));
#152424=CARTESIAN_POINT('Ctrl Pts',(5.13802679694443,4.68906787905865,5.1149991105697));
#152425=CARTESIAN_POINT('Ctrl Pts',(5.14222035888887,4.68808181111733,5.1107935651394));
#152426=CARTESIAN_POINT('Ctrl Pts',(4.51347565108401,4.820162746,5.99015454228934));
#152427=CARTESIAN_POINT('Ctrl Pts',(4.83806716830898,4.755280647,5.74558056701959));
#152428=CARTESIAN_POINT('Ctrl Pts',(5.13432997385987,4.690053947,5.46736404691458));
#152429=CARTESIAN_POINT('Ctrl Pts',(5.13880874183013,4.68906787905865,5.46315809457868));
#152430=CARTESIAN_POINT('Ctrl Pts',(5.1432875098004,4.68808181111732,5.4589521422428));
#152431=CARTESIAN_POINT('',(4.55424020817694,4.81939092093594,5.64104568324374));
#152432=CARTESIAN_POINT('Origin',(-0.140189866127276,4.69643190112113,-0.141257248052444));
#152433=CARTESIAN_POINT('Origin',(9.44493727481165,5.70978234778588,11.3002261614088));
#152434=CARTESIAN_POINT('Ctrl Pts',(3.913329389,4.690053947,6.103142887));
#152435=CARTESIAN_POINT('Ctrl Pts',(4.24838586,4.755711878,5.888304997));
#152436=CARTESIAN_POINT('Ctrl Pts',(4.557910854,4.820155008,5.638080227));
#152437=CARTESIAN_POINT('Ctrl Pts',(4.253151186,4.690053947,6.177435146));
#152438=CARTESIAN_POINT('Ctrl Pts',(4.592286229,4.755711878,5.943941379));
#152439=CARTESIAN_POINT('Ctrl Pts',(4.903823059,4.820155008,5.674726372));
#152440=CARTESIAN_POINT('Origin',(-0.0835701931440092,4.55371943129,-0.172167829194979));
#152441=CARTESIAN_POINT('Ctrl Pts',(3.230923675,4.820162746,6.490272121));
#152442=CARTESIAN_POINT('Ctrl Pts',(3.582615315,4.755280647,6.315196435));
#152443=CARTESIAN_POINT('Ctrl Pts',(3.913329389,4.690053947,6.10314288700001));
#152444=CARTESIAN_POINT('Ctrl Pts',(3.91832898283825,4.68906787766383,6.09993715221183));
#152445=CARTESIAN_POINT('Ctrl Pts',(3.9233285766765,4.68808180832766,6.09673141742365));
#152446=CARTESIAN_POINT('Ctrl Pts',(3.12024693920707,4.820162746,6.82037190556698));
#152447=CARTESIAN_POINT('Ctrl Pts',(3.48982586236426,4.755280647,6.65129351551268));
#152448=CARTESIAN_POINT('Ctrl Pts',(3.83897053609471,4.690053947,6.44326928801588));
#152449=CARTESIAN_POINT('Ctrl Pts',(3.84424875585212,4.68906787766383,6.44012446677068));
#152450=CARTESIAN_POINT('Ctrl Pts',(3.84952697560952,4.68808180832766,6.4369796455255));
#152451=CARTESIAN_POINT('',(3.23510652906402,4.81939092093346,6.48818819268238));
#152452=CARTESIAN_POINT('Origin',(-0.106546362737626,4.69643187539504,-0.168091752984815));
#152453=CARTESIAN_POINT('Origin',(6.79478071579461,5.70975708926279,13.0661840777453));
#152454=CARTESIAN_POINT('Ctrl Pts',(2.509842609,4.690053947,6.801704939));
#152455=CARTESIAN_POINT('Ctrl Pts',(2.883249442,4.755711878,6.663917077));
#152456=CARTESIAN_POINT('Ctrl Pts',(3.239328843,4.820155008,6.486081147));
#152457=CARTESIAN_POINT('Ctrl Pts',(2.825748922,4.690053947,6.947311928));
#152458=CARTESIAN_POINT('Ctrl Pts',(3.207149434,4.755711878,6.792181124));
#152459=CARTESIAN_POINT('Ctrl Pts',(3.569275975,4.820155008,6.596231425));
#152460=CARTESIAN_POINT('Origin',(-0.0446053174623445,4.55371940454967,
-0.186107667785016));
#152461=CARTESIAN_POINT('Ctrl Pts',(1.76016982,4.820162746,7.03308625));
#152462=CARTESIAN_POINT('Ctrl Pts',(2.141275202,4.755280647,6.93770704300001));
#152463=CARTESIAN_POINT('Ctrl Pts',(2.509842609,4.690053947,6.801704939));
#152464=CARTESIAN_POINT('Ctrl Pts',(2.5154144445643,4.68906787921457,6.79964892062862));
#152465=CARTESIAN_POINT('Ctrl Pts',(2.5209862801286,4.68808181142913,6.79759290225721));
#152466=CARTESIAN_POINT('Ctrl Pts',(1.58111894904948,4.820162746,7.33167625852239));
#152467=CARTESIAN_POINT('Ctrl Pts',(1.97840417808707,4.755280647,7.24599937154038));
#152468=CARTESIAN_POINT('Ctrl Pts',(2.36410510319515,4.690053947,7.11789441891999));
#152469=CARTESIAN_POINT('Ctrl Pts',(2.3699359555464,4.68906787921457,7.11595778611574));
#152470=CARTESIAN_POINT('Ctrl Pts',(2.37576680789764,4.68808181142913,7.1140211533115));
#152471=CARTESIAN_POINT('',(1.76470286420027,4.81939092092281,7.03195023221659));
#152472=CARTESIAN_POINT('Origin',(-0.0679205185731391,4.69643185801115,
-0.187065872027213));
#152473=CARTESIAN_POINT('Origin',(3.8271353988825,5.70978052766214,14.2215713472656));
#152474=CARTESIAN_POINT('Ctrl Pts',(0.988998379000001,4.690053947,7.182226828));
#152475=CARTESIAN_POINT('Ctrl Pts',(1.383295485,4.755711878,7.127931801));
#152476=CARTESIAN_POINT('Ctrl Pts',(1.769279415,4.820155008,7.030800122));
#152477=CARTESIAN_POINT('Ctrl Pts',(1.266217779,4.690053947,7.392340126));
#152478=CARTESIAN_POINT('Ctrl Pts',(1.672049896,4.755711878,7.32282603));
#152479=CARTESIAN_POINT('Ctrl Pts',(2.067833513,4.820155008,7.209304028));
#152480=CARTESIAN_POINT('Origin',(-0.00355486453146994,4.55371941173134,
-0.191345552622352));
#152481=CARTESIAN_POINT('Ctrl Pts',(0.207112381,4.820162746,7.247041083));
#152482=CARTESIAN_POINT('Ctrl Pts',(0.599811441,4.755280647,7.23581818000001));
#152483=CARTESIAN_POINT('Ctrl Pts',(0.988998379000001,4.690053947,7.182226828));
#152484=CARTESIAN_POINT('Ctrl Pts',(0.994881931555155,4.68906787917506,
7.18141665811707));
#152485=CARTESIAN_POINT('Ctrl Pts',(1.00076548411031,4.6880818113501,7.18060648823417));
#152486=CARTESIAN_POINT('Ctrl Pts',(-0.0319404063266016,4.820162746,7.50015957902518));
#152487=CARTESIAN_POINT('Ctrl Pts',(0.374474513060617,4.755280647,7.5018903498288));
#152488=CARTESIAN_POINT('Ctrl Pts',(0.778696743080096,4.690053947,7.45969471738953));
#152489=CARTESIAN_POINT('Ctrl Pts',(0.784807592397145,4.68906787917506,
7.45905682285399));
#152490=CARTESIAN_POINT('Ctrl Pts',(0.790918441714193,4.6880818113501,7.45841892831845));
#152491=CARTESIAN_POINT('',(0.211783654676978,4.81939092020425,7.24690609579801));
#152492=CARTESIAN_POINT('Origin',(-0.0261189597364792,4.69643185026277,
-0.197293460334176));
#152493=CARTESIAN_POINT('Origin',(0.680450293923213,5.7097907178076,14.7119349338605));
#152494=CARTESIAN_POINT('Ctrl Pts',(-0.578090317,4.690053947,7.226915773));
#152495=CARTESIAN_POINT('Ctrl Pts',(-0.181339832,4.755711878,7.258652356));
#152496=CARTESIAN_POINT('Ctrl Pts',(0.216500448,4.820155008,7.246766697));
#152497=CARTESIAN_POINT('Ctrl Pts',(-0.3525203,4.690053947,7.49171071500001));
#152498=CARTESIAN_POINT('Ctrl Pts',(0.058767163,4.755711878,7.511063729));
#152499=CARTESIAN_POINT('Ctrl Pts',(0.469701454000001,4.820155008,7.485277586));
#152500=CARTESIAN_POINT('Origin',(0.0376619171070517,4.55371932361627,-0.187635523132965));
#152501=CARTESIAN_POINT('Ctrl Pts',(0.208106472,1.198733649,7.247012605));
#152502=CARTESIAN_POINT('Ctrl Pts',(0.602872113000001,1.134619049,7.235676446));
#152503=CARTESIAN_POINT('Ctrl Pts',(0.994070541,1.069390921,7.181526562));
#152504=CARTESIAN_POINT('Ctrl Pts',(0.997993468314819,1.06873681508671,
7.1809835484196));
#152505=CARTESIAN_POINT('Ctrl Pts',(1.00191639562964,1.06808270917341,7.18044053483919));
#152506=CARTESIAN_POINT('Ctrl Pts',(-0.030697537,1.198733649,7.499937177));
#152507=CARTESIAN_POINT('Ctrl Pts',(0.377845634,1.134619049,7.50160936));
#152508=CARTESIAN_POINT('Ctrl Pts',(0.784153080000001,1.069390921,7.458894285));
#152509=CARTESIAN_POINT('Ctrl Pts',(0.788227520140971,1.06873681508671,
7.45846593937671));
#152510=CARTESIAN_POINT('Ctrl Pts',(0.792301960281942,1.06808270917341,
7.45803759375342));
#152511=CARTESIAN_POINT('',(0.221348494829952,1.15903910584966,7.4967329445143));
#152512=CARTESIAN_POINT('',(0.784153071897506,1.06939091992727,7.45889428272056));
#152513=CARTESIAN_POINT('Origin',(-0.0390445917594759,0.94650929176938,
-0.183409434795353));
#152514=CARTESIAN_POINT('',(0.889111791278134,1.06939091791718,7.32021042583469));
#152515=CARTESIAN_POINT('Ctrl Pts',(0.221348496723335,1.15903910498851,
7.49673294432665));
#152516=CARTESIAN_POINT('Ctrl Pts',(0.220029630850789,1.16522285270462,
7.45504792860251));
#152517=CARTESIAN_POINT('Ctrl Pts',(0.218659615824573,1.1715546145733,7.41336222418238));
#152518=CARTESIAN_POINT('Ctrl Pts',(0.215810430745453,1.18452221944203,
7.33009059228574));
#152519=CARTESIAN_POINT('Ctrl Pts',(0.214329599541364,1.19116565504539,
7.28845588949761));
#152520=CARTESIAN_POINT('Ctrl Pts',(0.212788495890653,1.19797317326339,
7.24687664196839));
#152521=CARTESIAN_POINT('Ctrl Pts',(0.986271382025894,1.06811592995212,
7.18260612530439));
#152522=CARTESIAN_POINT('Ctrl Pts',(0.990170961512947,1.06875342547606,
7.18206634365219));
#152523=CARTESIAN_POINT('Ctrl Pts',(0.994070541000001,1.069390921,7.18152656200001));
#152524=CARTESIAN_POINT('Ctrl Pts',(1.000303954,1.070409947,7.18066373));
#152525=CARTESIAN_POINT('Ctrl Pts',(1.00653586,1.071428571,7.179790078));
#152526=CARTESIAN_POINT('Ctrl Pts',(1.392414954,1.134501699,7.125693629));
#152527=CARTESIAN_POINT('Ctrl Pts',(1.770273114,1.198754474,7.030549986));
#152528=CARTESIAN_POINT('Ctrl Pts',(1.26341113293498,1.06811592995212,7.39282480932989));
#152529=CARTESIAN_POINT('Ctrl Pts',(1.26742469796749,1.06875342547606,7.39213441616495));
#152530=CARTESIAN_POINT('Ctrl Pts',(1.271438263,1.069390921,7.391444023));
#152531=CARTESIAN_POINT('Ctrl Pts',(1.27785388,1.070409947,7.39034044099999));
#152532=CARTESIAN_POINT('Ctrl Pts',(1.284267572,1.071428571,7.389225724));
#152533=CARTESIAN_POINT('Ctrl Pts',(1.681402823,1.134501699,7.320202535));
#152534=CARTESIAN_POINT('Ctrl Pts',(2.068852438,1.198754474,7.209011693));
#152535=CARTESIAN_POINT('',(1.27143827033051,1.06939091911159,7.39144401914332));
#152536=CARTESIAN_POINT('',(1.82774947115441,1.15903910585546,7.27388011096424));
#152537=CARTESIAN_POINT('Origin',(-0.0717256750925657,1.3383840921539,-0.168465344956257));
#152538=CARTESIAN_POINT('Ctrl Pts',(1.76567788092872,1.19797317330302,7.0317054563247));
#152539=CARTESIAN_POINT('Ctrl Pts',(1.77612131102255,1.19116562418267,7.07198149530744));
#152540=CARTESIAN_POINT('Ctrl Pts',(1.78651780332373,1.18452215733789,7.11232467093176));
#152541=CARTESIAN_POINT('Ctrl Pts',(1.80720121631984,1.17155461457357,7.19303658126377));
#152542=CARTESIAN_POINT('Ctrl Pts',(1.81750039536026,1.16522285269688,7.23345318439212));
#152543=CARTESIAN_POINT('Ctrl Pts',(1.82774947299082,1.15903910498863,7.27388011036608));
#152544=CARTESIAN_POINT('',(1.13275441898507,1.06939091820872,7.28648528985951));
#152545=CARTESIAN_POINT('Origin',(-1.01047642475649E-13,1.16011713399994,
-1.66967134562768E-13));
#152546=CARTESIAN_POINT('',(1.82142216213811,0.979367659149596,7.27546708527639));
#152547=CARTESIAN_POINT('Origin',(-0.0517297820971196,0.94643634185441,
-0.184811503852839));
#152548=CARTESIAN_POINT('',(2.36926179550939,1.06939091992739,7.115939747572));
#152549=CARTESIAN_POINT('Origin',(-0.0169371445751124,0.803756644740858,
-0.182664612580321));
#152550=CARTESIAN_POINT('Origin',(-0.0775593148305506,0.946509321505581,
-0.1707278100195));
#152551=CARTESIAN_POINT('Ctrl Pts',(1.761134548,1.198733649,7.032844738));
#152552=CARTESIAN_POINT('Ctrl Pts',(2.144233849,1.134619049,6.93691066800001));
#152553=CARTESIAN_POINT('Ctrl Pts',(2.51464565,1.069390921,6.79993068));
#152554=CARTESIAN_POINT('Ctrl Pts',(2.51836012957831,1.06873681508671,6.79855704836438));
#152555=CARTESIAN_POINT('Ctrl Pts',(2.52207460915663,1.06808270917341,6.79718341672874));
#152556=CARTESIAN_POINT('Ctrl Pts',(1.582284951,1.198733649,7.331191877));
#152557=CARTESIAN_POINT('Ctrl Pts',(1.981636079,1.134619049,7.24500026));
#152558=CARTESIAN_POINT('Ctrl Pts',(2.369261804,1.069390921,7.115939748));
#152559=CARTESIAN_POINT('Ctrl Pts',(2.37314890434522,1.06873681508671,7.1146455326567));
#152560=CARTESIAN_POINT('Ctrl Pts',(2.37703600469044,1.06808270917341,7.11335131731341));
#152561=CARTESIAN_POINT('',(2.44195370872946,1.06939091791719,6.95793522041222));
#152562=CARTESIAN_POINT('Ctrl Pts',(2.50726090509695,1.06811592995267,6.80266159234607));
#152563=CARTESIAN_POINT('Ctrl Pts',(2.51095327754848,1.06875342547634,6.80129613617304));
#152564=CARTESIAN_POINT('Ctrl Pts',(2.51464565,1.069390921,6.79993068));
#152565=CARTESIAN_POINT('Ctrl Pts',(2.520547846,1.070409947,6.797748021));
#152566=CARTESIAN_POINT('Ctrl Pts',(2.526446244,1.071428571,6.795555119));
#152567=CARTESIAN_POINT('Ctrl Pts',(2.891674563,1.134501699,6.659770816));
#152568=CARTESIAN_POINT('Ctrl Pts',(3.240245538,1.198754474,6.485623243));
#152569=CARTESIAN_POINT('Ctrl Pts',(2.82311208693778,1.06811592995267,6.94838862489811));
#152570=CARTESIAN_POINT('Ctrl Pts',(2.82688340296889,1.06875342547634,6.94685157544905));
#152571=CARTESIAN_POINT('Ctrl Pts',(2.830654719,1.069390921,6.945314526));
#152572=CARTESIAN_POINT('Ctrl Pts',(2.836683105,1.070409947,6.942857578));
#152573=CARTESIAN_POINT('Ctrl Pts',(2.842707217,1.071428571,6.940390168));
#152574=CARTESIAN_POINT('Ctrl Pts',(3.21571972,1.134501699,6.787608363));
#152575=CARTESIAN_POINT('Ctrl Pts',(3.570208235,1.198754474,6.595726886));
#152576=CARTESIAN_POINT('',(2.83065472529928,1.069390919111,6.94531452062289));
#152577=CARTESIAN_POINT('',(3.34868691359671,1.15903910586187,6.71090872772502));
#152578=CARTESIAN_POINT('Origin',(-0.106263825604032,1.33838398565068,-0.149107832000643));
#152579=CARTESIAN_POINT('Ctrl Pts',(3.23600613130859,1.19797317337953,6.48773953814593));
#152580=CARTESIAN_POINT('Ctrl Pts',(3.25486355744072,1.19116562422889,6.52482891711007));
#152581=CARTESIAN_POINT('Ctrl Pts',(3.27368957558313,1.18452215736987,6.56199395330996));
#152582=CARTESIAN_POINT('Ctrl Pts',(3.3112400966168,1.17155461455324,6.63637254212063));
#152583=CARTESIAN_POINT('Ctrl Pts',(3.32998686140786,1.16522285268755,6.67363020853883));
#152584=CARTESIAN_POINT('Ctrl Pts',(3.34868691525358,1.15903910499673,6.71090872675037));
#152585=CARTESIAN_POINT('',(2.67265020052562,1.0693909182078,6.8726225967679));
#152586=CARTESIAN_POINT('Origin',(-4.88758339356465E-13,1.16011713400006,
-7.53303669442928E-13));
#152587=CARTESIAN_POINT('',(3.34284868628286,0.979367659172238,6.71381878362192));
#152588=CARTESIAN_POINT('Origin',(-0.0902493205394439,0.946436353500672,
-0.169370210595567));
#152589=CARTESIAN_POINT('',(3.84358647165651,1.06939091992733,6.440251779367));
#152590=CARTESIAN_POINT('Origin',(-0.0558087578793248,0.803756666233792,
-0.17475322261742));
#152591=CARTESIAN_POINT('Origin',(-0.112447373940797,0.946509336669416,
-0.150063191541521));
#152592=CARTESIAN_POINT('Ctrl Pts',(3.231813931,1.198733649,6.489828867));
#152593=CARTESIAN_POINT('Ctrl Pts',(3.585333593,1.134619049,6.313782657));
#152594=CARTESIAN_POINT('Ctrl Pts',(3.917638724,1.069390921,6.100377597));
#152595=CARTESIAN_POINT('Ctrl Pts',(3.92097107091642,1.06873681508671,6.09823757679778));
#152596=CARTESIAN_POINT('Ctrl Pts',(3.92430341783284,1.06808270917341,6.09609755659557));
#152597=CARTESIAN_POINT('Ctrl Pts',(3.121281553,1.198733649,6.819648192));
#152598=CARTESIAN_POINT('Ctrl Pts',(3.492767424,1.134619049,6.649623));
#152599=CARTESIAN_POINT('Ctrl Pts',(3.84358648,1.069390921,6.440251778));
#152600=CARTESIAN_POINT('Ctrl Pts',(3.84710448405839,1.06873681508671,6.43815220901677));
#152601=CARTESIAN_POINT('Ctrl Pts',(3.85062248811679,1.06808270917341,6.43605264003352));
#152602=CARTESIAN_POINT('',(3.88061258553506,1.06939091791719,6.27031469768993));
#152603=CARTESIAN_POINT('Ctrl Pts',(3.91101369546957,1.06811592995217,6.10463216359967));
#152604=CARTESIAN_POINT('Ctrl Pts',(3.91432620973478,1.06875342547609,6.10250488029983));
#152605=CARTESIAN_POINT('Ctrl Pts',(3.917638724,1.069390921,6.100377597));
#152606=CARTESIAN_POINT('Ctrl Pts',(3.922933723,1.070409947,6.09697717));
#152607=CARTESIAN_POINT('Ctrl Pts',(3.928222811,1.071428571,6.093567555));
#152608=CARTESIAN_POINT('Ctrl Pts',(4.255722683,1.134501699,5.882444522));
#152609=CARTESIAN_POINT('Ctrl Pts',(4.558707681,1.198754474,5.63743596700001));
#152610=CARTESIAN_POINT('Ctrl Pts',(4.2508074552393,1.06811592995217,6.17905351246949));
#152611=CARTESIAN_POINT('Ctrl Pts',(4.25416018011965,1.06875342547609,6.17674167673474));
#152612=CARTESIAN_POINT('Ctrl Pts',(4.257512905,1.069390921,6.17442984100001));
#152613=CARTESIAN_POINT('Ctrl Pts',(4.26287218,1.070409947,6.17073441));
#152614=CARTESIAN_POINT('Ctrl Pts',(4.268225031,1.071428571,6.167029681));
#152615=CARTESIAN_POINT('Ctrl Pts',(4.599673138,1.134501699,5.937633167));
#152616=CARTESIAN_POINT('Ctrl Pts',(4.90462506300001,1.198754474,5.674033221));
#152617=CARTESIAN_POINT('',(4.25751291014559,1.06939091911149,6.17442983448858));
#152618=CARTESIAN_POINT('',(4.71304347805112,1.15903910585152,5.83414271099935));
#152619=CARTESIAN_POINT('Origin',(-0.13583321860543,1.33838405461728,-0.122778182208158));
#152620=CARTESIAN_POINT('Ctrl Pts',(4.55502233005473,1.19797317335072,5.64041413156831));
#152621=CARTESIAN_POINT('Ctrl Pts',(4.58141200040322,1.1911656242053,5.67258259206166));
#152622=CARTESIAN_POINT('Ctrl Pts',(4.60778726111216,1.18452215734081,5.70483169279222));
#152623=CARTESIAN_POINT('Ctrl Pts',(4.66044906985397,1.17155461458284,5.76939909879967));
#152624=CARTESIAN_POINT('Ctrl Pts',(4.68676684286837,1.16522285268912,5.80175570135455));
#152625=CARTESIAN_POINT('Ctrl Pts',(4.71304347948102,1.15903910497747,5.83414270967234));
#152626=CARTESIAN_POINT('',(4.08757582880698,1.06939091820862,6.13740370947139));
#152627=CARTESIAN_POINT('Origin',(-5.95010152260045E-13,1.16011713400006,
-8.0404433111525E-13));
#152628=CARTESIAN_POINT('',(4.70796732118502,0.9793676591462,5.83823977776835));
#152629=CARTESIAN_POINT('Origin',(-0.12454898017964,0.946436321968166,-0.146009561522032));
#152630=CARTESIAN_POINT('',(5.13818931612299,1.06939091992738,5.46342479616291));
#152631=CARTESIAN_POINT('Origin',(-0.0920707914298757,0.80375664195573,
-0.158670405150794));
#152632=CARTESIAN_POINT('Origin',(-0.142077653826491,0.94650933952944,-0.12238203947585));
#152633=CARTESIAN_POINT('Ctrl Pts',(4.551377285,1.198733649,5.643355811));
#152634=CARTESIAN_POINT('Ctrl Pts',(4.858787123,1.134619049,5.395429187));
#152635=CARTESIAN_POINT('Ctrl Pts',(5.137447365,1.069390921,5.115577638));
#152636=CARTESIAN_POINT('Ctrl Pts',(5.14024176241229,1.06873681508671,5.11277129419315));
#152637=CARTESIAN_POINT('Ctrl Pts',(5.14303615982459,1.06808270917341,5.10996495038631));
#152638=CARTESIAN_POINT('Ctrl Pts',(4.51433049900001,1.198733649,5.989225338));
#152639=CARTESIAN_POINT('Ctrl Pts',(4.840580846,1.134619049,5.74331675900001));
#152640=CARTESIAN_POINT('Ctrl Pts',(5.13818932400001,1.069390921,5.463424793));
#152641=CARTESIAN_POINT('Ctrl Pts',(5.14117373381329,1.06873681508671,5.46061804389256));
#152642=CARTESIAN_POINT('Ctrl Pts',(5.1441581436266,1.06808270917341,5.45781129478513));
#152643=CARTESIAN_POINT('',(5.13781833061056,1.06939091791719,5.28950122899115));
#152644=CARTESIAN_POINT('Ctrl Pts',(5.13189183273593,1.06811592995319,5.12115692152758));
#152645=CARTESIAN_POINT('Ctrl Pts',(5.13466959886796,1.06875342547659,5.11836727976378));
#152646=CARTESIAN_POINT('Ctrl Pts',(5.137447365,1.069390921,5.115577638));
#152647=CARTESIAN_POINT('Ctrl Pts',(5.141887578,1.070409947,5.111118442));
#152648=CARTESIAN_POINT('Ctrl Pts',(5.146320044,1.071428571,5.106651545));
#152649=CARTESIAN_POINT('Ctrl Pts',(5.42077794,1.134501699,4.830061659));
#152650=CARTESIAN_POINT('Ctrl Pts',(5.66400972,1.198754474,4.525648449));
#152651=CARTESIAN_POINT('Ctrl Pts',(5.47973979224852,1.06811592995319,5.1207927256041));
#152652=CARTESIAN_POINT('Ctrl Pts',(5.48251715612426,1.06875342547659,5.11781420230205));
#152653=CARTESIAN_POINT('Ctrl Pts',(5.48529452,1.069390921,5.114835679));
#152654=CARTESIAN_POINT('Ctrl Pts',(5.48973409,1.070409947,5.11007455900001));
#152655=CARTESIAN_POINT('Ctrl Pts',(5.494165387,1.071428571,5.10530574));
#152656=CARTESIAN_POINT('Ctrl Pts',(5.768550952,1.134501699,4.810020844));
#152657=CARTESIAN_POINT('Ctrl Pts',(6.009707074,1.198754474,4.487028069));
#152658=CARTESIAN_POINT('',(5.48529452373196,1.06939091911035,5.1148356715626));
#152659=CARTESIAN_POINT('',(5.85702336747576,1.1590391058667,4.68457866535481));
#152660=CARTESIAN_POINT('Origin',(-0.159051194702147,1.33838407973086,-0.0907075657125889));
#152661=CARTESIAN_POINT('Ctrl Pts',(5.66105074778303,1.19797317332967,4.529349227356));
#152662=CARTESIAN_POINT('Ctrl Pts',(5.6937387104184,1.19116562421628,4.55509260821413));
#152663=CARTESIAN_POINT('Ctrl Pts',(5.72642993554067,1.18452215738145,4.58091784158635));
#152664=CARTESIAN_POINT('Ctrl Pts',(5.79174062461541,1.17155461457221,4.63265496589298));
#152665=CARTESIAN_POINT('Ctrl Pts',(5.82439881566446,1.16522285272192,4.65859754577574));
#152666=CARTESIAN_POINT('Ctrl Pts',(5.85702336856875,1.15903910501501,4.68457866377963));
#152667=CARTESIAN_POINT('',(5.31137095443124,1.06939091820696,5.1152066461112));
#152668=CARTESIAN_POINT('Origin',(-9.51062145704284E-13,1.160117134,-8.09248501543181E-13));
#152669=CARTESIAN_POINT('',(5.8529466364323,0.979367659138719,4.68967116858882));
#152670=CARTESIAN_POINT('Origin',(-0.153024751815678,0.9464363304404,-0.115821519499659));
#152671=CARTESIAN_POINT('',(6.19253613899442,1.06939091992736,4.23113414176147));
#152672=CARTESIAN_POINT('Origin',(-0.124027660136634,0.803756642011697,
-0.135168275672048));
#152673=CARTESIAN_POINT('Origin',(-0.165064522538633,0.946509306495977,
-0.0889783519444282));
#152674=CARTESIAN_POINT('Ctrl Pts',(5.658123296,1.198733649,4.53300571));
#152675=CARTESIAN_POINT('Ctrl Pts',(5.90504916800001,1.134619049,4.224791444));
#152676=CARTESIAN_POINT('Ctrl Pts',(6.117034678,1.069390921,3.891578954));
#152677=CARTESIAN_POINT('Ctrl Pts',(6.11916046299299,1.06873681508671,3.88823750811193));
#152678=CARTESIAN_POINT('Ctrl Pts',(6.12128624798599,1.06808270917341,3.88489606222386));
#152679=CARTESIAN_POINT('Ctrl Pts',(5.696294368,1.198733649,4.878752963));
#152680=CARTESIAN_POINT('Ctrl Pts',(5.962054088,1.134619049,4.568459409));
#152681=CARTESIAN_POINT('Ctrl Pts',(6.192536146,1.069390921,4.231134137));
#152682=CARTESIAN_POINT('Ctrl Pts',(6.19484741387888,1.06873681508671,4.22775144824465));
#152683=CARTESIAN_POINT('Ctrl Pts',(6.19715868175776,1.06808270917341,4.22436875948929));
#152684=CARTESIAN_POINT('',(6.15478540133549,1.06939091791719,4.06135656166154));
#152685=CARTESIAN_POINT('Ctrl Pts',(6.11280841197604,1.06811592995216,3.89822207217745));
#152686=CARTESIAN_POINT('Ctrl Pts',(6.11492154498802,1.06875342547608,3.89490051308873));
#152687=CARTESIAN_POINT('Ctrl Pts',(6.117034678,1.069390921,3.891578954));
#152688=CARTESIAN_POINT('Ctrl Pts',(6.120412486,1.070409947,3.886269497));
#152689=CARTESIAN_POINT('Ctrl Pts',(6.123781072,1.071428571,3.880954185));
#152690=CARTESIAN_POINT('Ctrl Pts',(6.332363645,1.134501699,3.551830482));
#152691=CARTESIAN_POINT('Ctrl Pts',(6.50446896,1.198754474,3.202246641));
#152692=CARTESIAN_POINT('Ctrl Pts',(6.4524455879471,1.06811592995216,3.82308936021757));
#152693=CARTESIAN_POINT('Ctrl Pts',(6.45451772397355,1.06875342547608,3.81958342260879));
#152694=CARTESIAN_POINT('Ctrl Pts',(6.45658986,1.069390921,3.816077485));
#152695=CARTESIAN_POINT('Ctrl Pts',(6.45990213500001,1.070409947,3.810473302));
#152696=CARTESIAN_POINT('Ctrl Pts',(6.463204676,1.071428571,3.804863377));
#152697=CARTESIAN_POINT('Ctrl Pts',(6.667697735,1.134501699,3.457497292));
#152698=CARTESIAN_POINT('Ctrl Pts',(6.833781861,1.198754474,3.090214471));
#152699=CARTESIAN_POINT('',(6.45658986212243,1.06939091911146,3.81607747695018));
#152700=CARTESIAN_POINT('',(6.72713535380483,1.15903910586345,3.31596892777236));
#152701=CARTESIAN_POINT('Origin',(-0.174832111025703,1.33838404516078,-0.0543955737960117));
#152702=CARTESIAN_POINT('Ctrl Pts',(6.50237472517852,1.19797317335901,3.20649698852999));
#152703=CARTESIAN_POINT('Ctrl Pts',(6.53983233906171,1.19116565840804,3.22461146673117));
#152704=CARTESIAN_POINT('Ctrl Pts',(6.57731071417596,1.18452222611864,3.24280517092969));
#152705=CARTESIAN_POINT('Ctrl Pts',(6.65221682460398,1.17155461459956,3.27929303559281));
#152706=CARTESIAN_POINT('Ctrl Pts',(6.68968837315633,1.16522285272586,3.29760854664996));
#152707=CARTESIAN_POINT('Ctrl Pts',(6.72713535453218,1.15903910500762,3.31596892600066));
#152708=CARTESIAN_POINT('',(6.28681227798357,1.06939091820867,3.85382820484497));
#152709=CARTESIAN_POINT('Origin',(-5.68121938382404E-13,1.16011713400022,
-2.82326245715225E-13));
#152710=CARTESIAN_POINT('',(6.72424867213753,0.979367659153833,3.32181874799286));
#152711=CARTESIAN_POINT('Origin',(-0.174345382799326,0.946436314050401,
-0.080217914826296));
#152712=CARTESIAN_POINT('',(6.95732685417891,1.06939091992739,2.80100035617951));
#152713=CARTESIAN_POINT('Origin',(-0.150185083090411,0.803756637318066,
-0.105345803537276));
#152714=CARTESIAN_POINT('Origin',(-0.180332952476162,0.946509333178315,
-0.0514140178657779));
#152715=CARTESIAN_POINT('Ctrl Pts',(6.500301751,1.198733649,3.210697299));
#152716=CARTESIAN_POINT('Ctrl Pts',(6.675197676,1.134619049,2.856607148));
#152717=CARTESIAN_POINT('Ctrl Pts',(6.810596247,1.069390921,2.485614363));
#152718=CARTESIAN_POINT('Ctrl Pts',(6.81195402022849,1.06873681508671,2.48189405732976));
#152719=CARTESIAN_POINT('Ctrl Pts',(6.81331179345697,1.06808270917341,2.47817375165952));
#152720=CARTESIAN_POINT('Ctrl Pts',(6.611905843,1.198733649,3.540155522));
#152721=CARTESIAN_POINT('Ctrl Pts',(6.804748307,1.134619049,3.179985975));
#152722=CARTESIAN_POINT('Ctrl Pts',(6.95732686,1.069390921,2.80100035));
#152723=CARTESIAN_POINT('Ctrl Pts',(6.95885691362593,1.06873681508671,2.79719989234521));
#152724=CARTESIAN_POINT('Ctrl Pts',(6.96038696725186,1.06808270917341,2.79339943469041));
#152725=CARTESIAN_POINT('',(6.88396154655908,1.06939091791719,2.64330737457626));
#152726=CARTESIAN_POINT('Ctrl Pts',(6.80789686204117,1.06811592995401,2.49301069012391));
#152727=CARTESIAN_POINT('Ctrl Pts',(6.80924655452058,1.06875342547701,2.48931252656195));
#152728=CARTESIAN_POINT('Ctrl Pts',(6.810596247,1.069390921,2.485614363));
#152729=CARTESIAN_POINT('Ctrl Pts',(6.812753708,1.070409947,2.47970291));
#152730=CARTESIAN_POINT('Ctrl Pts',(6.814900903,1.071428571,2.47378772));
#152731=CARTESIAN_POINT('Ctrl Pts',(6.94785506400001,1.134501699,2.107519659));
#152732=CARTESIAN_POINT('Ctrl Pts',(7.04078646,1.198754474,1.729111338));
#152733=CARTESIAN_POINT('Ctrl Pts',(7.12344219883659,1.06811592995401,2.34662258803516));
#152734=CARTESIAN_POINT('Ctrl Pts',(7.12471221641829,1.06875342547701,2.34275316901758));
#152735=CARTESIAN_POINT('Ctrl Pts',(7.125982234,1.069390921,2.33888375));
#152736=CARTESIAN_POINT('Ctrl Pts',(7.128012336,1.070409947,2.332698548));
#152737=CARTESIAN_POINT('Ctrl Pts',(7.130031697,1.071428571,2.326509831));
#152738=CARTESIAN_POINT('Ctrl Pts',(7.255070382,1.134501699,1.94330501));
#152739=CARTESIAN_POINT('Ctrl Pts',(7.338316604,1.198754474,1.548905879));
#152740=CARTESIAN_POINT('',(7.12598223423462,1.06939091910945,2.33888374168009));
#152741=CARTESIAN_POINT('',(7.28269396775983,1.15903910589433,1.79230816855612));
#152742=CARTESIAN_POINT('Origin',(-0.182438073594617,1.33838404864279,-0.0155400990156312));
#152743=CARTESIAN_POINT('Ctrl Pts',(7.03965488635939,1.19797317331785,1.73371251352998));
#152744=CARTESIAN_POINT('Ctrl Pts',(7.08013084500336,1.19116565746261,1.74335120689549));
#152745=CARTESIAN_POINT('Ctrl Pts',(7.12064411118154,1.18452222427951,1.75306281109334));
#152746=CARTESIAN_POINT('Ctrl Pts',(7.20164275946683,1.17155461460936,1.77259500754028));
#152747=CARTESIAN_POINT('Ctrl Pts',(7.24217553752639,1.16522285275215,1.7824270368528));
#152748=CARTESIAN_POINT('Ctrl Pts',(7.28269396809338,1.15903910505169,1.79230816666107));
#152749=CARTESIAN_POINT('',(6.96828924612935,1.06939091820559,2.41224904023845));
#152750=CARTESIAN_POINT('Origin',(7.94937032866372E-13,1.16011713400011,
2.03287907341032E-13));
#152751=CARTESIAN_POINT('',(7.28113231366877,0.97936765913114,1.79864177447981));
#152752=CARTESIAN_POINT('Origin',(-0.187513717011382,0.946436304846853,
-0.0408633449838341));
#152753=CARTESIAN_POINT('',(7.396800698641,1.06939091992734,1.23989490826094));
#152754=CARTESIAN_POINT('Origin',(-0.169320101023622,0.803756621750654,
-0.0705975350748289));
#152755=CARTESIAN_POINT('Origin',(-0.187169459703335,0.946509334807441,
-0.0114457587835903));
#152756=CARTESIAN_POINT('Ctrl Pts',(7.03853332,1.198733649,1.738260252));
#152757=CARTESIAN_POINT('Ctrl Pts',(7.13322136,1.134619049,1.354851078));
#152758=CARTESIAN_POINT('Ctrl Pts',(7.185701905,1.069390921,0.963425207));
#152759=CARTESIAN_POINT('Ctrl Pts',(7.18622817849381,1.06873681508671,0.959499998892894));
#152760=CARTESIAN_POINT('Ctrl Pts',(7.18675445198762,1.06808270917341,0.955574790785788));
#152761=CARTESIAN_POINT('Ctrl Pts',(7.21835195,1.198733649,2.036024343));
#152762=CARTESIAN_POINT('Ctrl Pts',(7.329260058,1.134619049,1.642819931));
#152763=CARTESIAN_POINT('Ctrl Pts',(7.396800703,1.069390921,1.239894901));
#152764=CARTESIAN_POINT('Ctrl Pts',(7.39747799877158,1.06873681508671,1.23585437963571));
#152765=CARTESIAN_POINT('Ctrl Pts',(7.39815529454315,1.06808270917341,1.23181385827142));
#152766=CARTESIAN_POINT('',(7.29125130110721,1.06939091791719,1.10166007314573));
#152767=CARTESIAN_POINT('Ctrl Pts',(7.18465562199158,1.06811592995212,0.971228900272083));
#152768=CARTESIAN_POINT('Ctrl Pts',(7.1851787634958,1.06875342547606,0.967327053636041));
#152769=CARTESIAN_POINT('Ctrl Pts',(7.18570190500001,1.069390921,0.963425207));
#152770=CARTESIAN_POINT('Ctrl Pts',(7.186538138,1.070409947,0.95718817));
#152771=CARTESIAN_POINT('Ctrl Pts',(7.187363542,1.071428571,0.95094969));
#152772=CARTESIAN_POINT('Ctrl Pts',(7.238472502,1.134501699,0.564663559));
#152773=CARTESIAN_POINT('Ctrl Pts',(7.247884611,1.198754474,0.175124711));
#152774=CARTESIAN_POINT('Ctrl Pts',(7.46135457079931,1.06811592995212,0.760430350372509));
#152775=CARTESIAN_POINT('Ctrl Pts',(7.46176308489966,1.06875342547606,0.756378380186254));
#152776=CARTESIAN_POINT('Ctrl Pts',(7.462171599,1.069390921,0.75232641));
#152777=CARTESIAN_POINT('Ctrl Pts',(7.46282460200001,1.070409947,0.745849403));
#152778=CARTESIAN_POINT('Ctrl Pts',(7.463466361,1.071428571,0.739371272));
#152779=CARTESIAN_POINT('Ctrl Pts',(7.503204002,1.134501699,0.338245945));
#152780=CARTESIAN_POINT('Ctrl Pts',(7.499719818,1.198754474,-0.064827831));
#152781=CARTESIAN_POINT('Ctrl Pts',(7.24776860954439,1.19797317331415,0.179861568603665));
#152782=CARTESIAN_POINT('Ctrl Pts',(7.28937029396337,1.19116565793403,0.180573779781957));
#152783=CARTESIAN_POINT('Ctrl Pts',(7.33102408720557,1.18452222520096,0.181349177264534));
#152784=CARTESIAN_POINT('Ctrl Pts',(7.4143278828079,1.17155461459689,0.183012406879414));
#152785=CARTESIAN_POINT('Ctrl Pts',(7.45602662267977,1.16522285273111,0.183901219767036));
#152786=CARTESIAN_POINT('Ctrl Pts',(7.49772190567691,1.1590391050196,0.184841069551826));
#152787=CARTESIAN_POINT('',(7.32393675399974,1.06939091820872,0.857875791427671));
#152788=CARTESIAN_POINT('Ctrl Pts',(7.247650894,1.198733649,0.184544087));
#152789=CARTESIAN_POINT('Ctrl Pts',(7.257703542,1.134619049,-0.210256324));
#152790=CARTESIAN_POINT('Ctrl Pts',(7.224812129,1.069390921,-0.603812641));
#152791=CARTESIAN_POINT('Ctrl Pts',(7.22448229479504,1.06873681508671,-0.607759213162297));
#152792=CARTESIAN_POINT('Ctrl Pts',(7.22415246059009,1.06808270917341,-0.611705785324593));
#152793=CARTESIAN_POINT('Ctrl Pts',(7.487275942,1.198733649,0.436690929));
#152794=CARTESIAN_POINT('Ctrl Pts',(7.51106375400001,1.134619049,0.028837453));
#152795=CARTESIAN_POINT('Ctrl Pts',(7.490408365,1.069390921,-0.379186656));
#152796=CARTESIAN_POINT('Ctrl Pts',(7.49020123331463,1.06873681508671,-0.383278310791366));
#152797=CARTESIAN_POINT('Ctrl Pts',(7.48999410162926,1.06808270917341,-0.387369965582731));
#152798=CARTESIAN_POINT('',(7.35761024829061,1.06939091791719,-0.491499629180019));
#152799=CARTESIAN_POINT('Ctrl Pts',(7.2254678718203,1.06811592995217,-0.595966473717617));
#152800=CARTESIAN_POINT('Ctrl Pts',(7.22514000041015,1.06875342547609,-0.599889557358809));
#152801=CARTESIAN_POINT('Ctrl Pts',(7.224812129,1.069390921,-0.603812641000001));
#152802=CARTESIAN_POINT('Ctrl Pts',(7.224288032,1.070409947,-0.610083625));
#152803=CARTESIAN_POINT('Ctrl Pts',(7.22375305,1.071428571,-0.616353689));
#152804=CARTESIAN_POINT('Ctrl Pts',(7.190627011,1.134501699,-1.004595582));
#152805=CARTESIAN_POINT('Ctrl Pts',(7.116079733,1.198754474,-1.387050553));
#152806=CARTESIAN_POINT('Ctrl Pts',(7.45038229297622,1.06811592995217,-0.861318764735266));
#152807=CARTESIAN_POINT('Ctrl Pts',(7.44991020298811,1.06875342547609,-0.865363820867633));
#152808=CARTESIAN_POINT('Ctrl Pts',(7.449438113,1.069390921,-0.869408877000001));
#152809=CARTESIAN_POINT('Ctrl Pts',(7.448683485,1.070409947,-0.875874832));
#152810=CARTESIAN_POINT('Ctrl Pts',(7.447917633,1.071428571,-0.882339467));
#152811=CARTESIAN_POINT('Ctrl Pts',(7.400496141,1.134501699,-1.282629125));
#152812=CARTESIAN_POINT('Ctrl Pts',(7.310444469,1.198754474,-1.675530263));
#152813=CARTESIAN_POINT('',(7.44943810973505,1.06939091911148,-0.869408884642924));
#152814=CARTESIAN_POINT('',(7.36216470066823,1.15903910587719,-1.43126898914685));
#152815=CARTESIAN_POINT('Origin',(-0.172101427481555,1.33838407053768,0.0624999501092453));
#152816=CARTESIAN_POINT('Ctrl Pts',(7.11698472793918,1.1979731733218,-1.3823995036554));
#152817=CARTESIAN_POINT('Ctrl Pts',(7.15776689789494,1.19116565700939,-1.39064707706337));
#152818=CARTESIAN_POINT('Ctrl Pts',(7.19861354226323,1.18452222333549,-1.39884414344332));
#152819=CARTESIAN_POINT('Ctrl Pts',(7.28032727466069,1.17155461460988,-1.41512765056565));
#152820=CARTESIAN_POINT('Ctrl Pts',(7.32124218987634,1.16522285270705,-1.42322361423589));
#152821=CARTESIAN_POINT('Ctrl Pts',(7.36216470016111,1.15903910500744,-1.43126899105776));
#152822=CARTESIAN_POINT('',(7.33712511928289,1.06939091820865,-0.736610776103533));
#152823=CARTESIAN_POINT('Origin',(-1.46800974154537E-12,1.16011713399978,
2.62322715632868E-13));
#152824=CARTESIAN_POINT('',(7.36340679369018,0.979367659169459,-1.42486504209286));
#152825=CARTESIAN_POINT('Origin',(-0.18734085634547,0.94643629633262,0.0416483950848034));
#152826=CARTESIAN_POINT('',(7.23377285710191,1.06939091992737,-1.980537857564));
#152827=CARTESIAN_POINT('Origin',(-0.183313845503943,0.803756640188027,
0.00702306772492167));
#152828=CARTESIAN_POINT('Origin',(-0.174676264822841,0.946509290946531,
0.0682025193396724));
#152829=CARTESIAN_POINT('Ctrl Pts',(7.117876367,1.198733649,-1.377801155));
#152830=CARTESIAN_POINT('Ctrl Pts',(7.042823572,1.134619049,-1.765532373));
#152831=CARTESIAN_POINT('Ctrl Pts',(6.926098167,1.069390921,-2.14281688));
#152832=CARTESIAN_POINT('Ctrl Pts',(6.92492764777796,1.06873681508671,-2.14660027888924));
#152833=CARTESIAN_POINT('Ctrl Pts',(6.92375712855592,1.06808270917341,-2.15038367777849));
#152834=CARTESIAN_POINT('Ctrl Pts',(7.406103233,1.198733649,-1.183061667));
#152835=CARTESIAN_POINT('Ctrl Pts',(7.341658458,1.134619049,-1.586493433));
#152836=CARTESIAN_POINT('Ctrl Pts',(7.233772858,1.069390921,-1.980537866));
#152837=CARTESIAN_POINT('Ctrl Pts',(7.23269098410475,1.06873681508671,-1.98448933297642));
#152838=CARTESIAN_POINT('Ctrl Pts',(7.2316091102095,1.06808270917341,-1.98844079995283));
#152839=CARTESIAN_POINT('',(7.07993551791366,1.06939091791719,-2.06167735440915));
#152840=CARTESIAN_POINT('Ctrl Pts',(6.92842527283417,1.06811592995212,-2.13529511646555));
#152841=CARTESIAN_POINT('Ctrl Pts',(6.92726171991709,1.06875342547606,-2.13905599823277));
#152842=CARTESIAN_POINT('Ctrl Pts',(6.926098167,1.069390921,-2.14281688));
#152843=CARTESIAN_POINT('Ctrl Pts',(6.924238247,1.070409947,-2.148828587));
#152844=CARTESIAN_POINT('Ctrl Pts',(6.922367894,1.071428571,-2.154837056));
#152845=CARTESIAN_POINT('Ctrl Pts',(6.806555793,1.134501699,-2.52688095));
#152846=CARTESIAN_POINT('Ctrl Pts',(6.651534875,1.198754474,-2.884368874));
#152847=CARTESIAN_POINT('Ctrl Pts',(7.09103842230696,1.06811592995212,-2.44279357166386));
#152848=CARTESIAN_POINT('Ctrl Pts',(7.08970780165348,1.06875342547606,-2.44664257133193));
#152849=CARTESIAN_POINT('Ctrl Pts',(7.088377181,1.069390921,-2.450491571));
#152850=CARTESIAN_POINT('Ctrl Pts',(7.086250206,1.070409947,-2.456644133));
#152851=CARTESIAN_POINT('Ctrl Pts',(7.084112554,1.071428571,-2.462792993));
#152852=CARTESIAN_POINT('Ctrl Pts',(6.951749306,1.134501699,-2.843529882));
#152853=CARTESIAN_POINT('Ctrl Pts',(6.779340862,1.198754474,-3.207886762));
#152854=CARTESIAN_POINT('',(7.0883771760567,1.06939091911158,-2.45049157765598));
#152855=CARTESIAN_POINT('',(6.88236085655826,1.15903910585907,-2.98045450177495));
#152856=CARTESIAN_POINT('Origin',(-0.154642145265497,1.33838411158198,0.0980354607432685));
#152857=CARTESIAN_POINT('Ctrl Pts',(6.65341854975392,1.19797317333231,-2.88002111080759));
#152858=CARTESIAN_POINT('Ctrl Pts',(6.69147429362735,1.19116565295346,-2.89684283171955));
#152859=CARTESIAN_POINT('Ctrl Pts',(6.72960386502397,1.18452221510443,-2.91362908763632));
#152860=CARTESIAN_POINT('Ctrl Pts',(6.80590665471737,1.17155461461087,-2.94709791120943));
#152861=CARTESIAN_POINT('Ctrl Pts',(6.84412460899343,1.16522285272256,-2.96380009301572));
#152862=CARTESIAN_POINT('Ctrl Pts',(6.88236085568021,1.15903910499693,-2.98045450347072));
#152863=CARTESIAN_POINT('',(7.00723766864643,1.06939091820872,-2.29665424183409));
#152864=CARTESIAN_POINT('Origin',(-9.11163505756818E-13,1.16011713400011,
4.39969241594618E-13));
#152865=CARTESIAN_POINT('',(6.88495056955131,0.979367659115532,-2.97446728926621));
#152866=CARTESIAN_POINT('Origin',(-0.174007811960476,0.946436343448101,
0.0809474406507071));
#152867=CARTESIAN_POINT('',(6.63889417195209,1.0693909199274,-3.48928131855112));
#152868=CARTESIAN_POINT('Origin',(-0.177518215079709,0.803756643672089,
0.0462658936260202));
#152869=CARTESIAN_POINT('Origin',(-0.155930962436405,0.946509332563335,
0.104158238975147));
#152870=CARTESIAN_POINT('Ctrl Pts',(6.655277852,1.198733649,-2.875721945));
#152871=CARTESIAN_POINT('Ctrl Pts',(6.498628999,1.134619049,-3.238254091));
#152872=CARTESIAN_POINT('Ctrl Pts',(6.303527553,1.069390921,-3.581625384));
#152873=CARTESIAN_POINT('Ctrl Pts',(6.30157108094671,1.06873681508671,-3.58506870209134));
#152874=CARTESIAN_POINT('Ctrl Pts',(6.29961460889341,1.06808270917341,-3.58851202018267));
#152875=CARTESIAN_POINT('Ctrl Pts',(6.978629367,1.198733649,-2.747495615));
#152876=CARTESIAN_POINT('Ctrl Pts',(6.828965371,1.134619049,-3.127641648));
#152877=CARTESIAN_POINT('Ctrl Pts',(6.638894171,1.069390921,-3.489281327));
#152878=CARTESIAN_POINT('Ctrl Pts',(6.63698814211831,1.06873681508671,-3.49290783997482));
#152879=CARTESIAN_POINT('Ctrl Pts',(6.63508211323662,1.06808270917341,-3.49653435294964));
#152880=CARTESIAN_POINT('',(6.47121087128357,1.06939091791719,-3.53545333850757));
#152881=CARTESIAN_POINT('Ctrl Pts',(6.30741720870105,1.06811592995355,-3.57477973385255));
#152882=CARTESIAN_POINT('Ctrl Pts',(6.30547238085052,1.06875342547678,-3.57820255892628));
#152883=CARTESIAN_POINT('Ctrl Pts',(6.303527553,1.069390921,-3.581625384));
#152884=CARTESIAN_POINT('Ctrl Pts',(6.300418778,1.070409947,-3.587096713));
#152885=CARTESIAN_POINT('Ctrl Pts',(6.297300509,1.071428571,-3.592562637));
#152886=CARTESIAN_POINT('Ctrl Pts',(6.104217591,1.134501699,-3.931012172));
#152887=CARTESIAN_POINT('Ctrl Pts',(5.875971639,1.198754474,-4.246817313));
#152888=CARTESIAN_POINT('Ctrl Pts',(6.40012547593091,1.06811592995355,-3.91004606779373));
#152889=CARTESIAN_POINT('Ctrl Pts',(6.39799854296545,1.06875342547678,-3.91351903539686));
#152890=CARTESIAN_POINT('Ctrl Pts',(6.39587161,1.069390921,-3.916992003));
#152891=CARTESIAN_POINT('Ctrl Pts',(6.392471743,1.070409947,-3.922543484));
#152892=CARTESIAN_POINT('Ctrl Pts',(6.389062245,1.071428571,-3.928089055));
#152893=CARTESIAN_POINT('Ctrl Pts',(6.1779464,1.134501699,-4.271470342));
#152894=CARTESIAN_POINT('Ctrl Pts',(5.93124281,1.198754474,-4.59024604200001));
#152895=CARTESIAN_POINT('',(6.39587160367231,1.06939091911003,-3.9169920083545));
#152896=CARTESIAN_POINT('',(6.08074546794259,1.15903910585345,-4.39027727503094));
#152897=CARTESIAN_POINT('Origin',(-0.129951979063783,1.33838405798379,0.128986930953131));
#152898=CARTESIAN_POINT('Ctrl Pts',(5.87874591481904,1.19797317339007,-4.24297613254375));
#152899=CARTESIAN_POINT('Ctrl Pts',(5.91229590555161,1.19116562424506,-4.26758553472227));
#152900=CARTESIAN_POINT('Ctrl Pts',(5.94592563809149,1.18452215738926,-4.29217618263442));
#152901=CARTESIAN_POINT('Ctrl Pts',(6.01324940384929,1.17155461456642,-4.34126514960852));
#152902=CARTESIAN_POINT('Ctrl Pts',(6.04698336827264,1.16522285267214,-4.36579257419969));
#152903=CARTESIAN_POINT('Ctrl Pts',(6.0807454666896,1.15903910497335,-4.39027727653642));
#152904=CARTESIAN_POINT('',(6.34969957275281,1.06939091820635,-3.74930870831395));
#152905=CARTESIAN_POINT('Origin',(1.47885176327023E-13,1.16011713399978,
-5.85469173142172E-14));
#152906=CARTESIAN_POINT('',(6.08456170863479,0.979367659166524,-4.38498675147155));
#152907=CARTESIAN_POINT('Origin',(-0.152538369459255,0.946436363046565,
0.116461520105225));
#152908=CARTESIAN_POINT('',(5.73358817473831,1.06939091992739,-4.83486986295877));
#152909=CARTESIAN_POINT('Origin',(-0.163422130638148,0.803756623814009,
0.0833453740518564));
#152910=CARTESIAN_POINT('Origin',(-0.129894276848799,0.946509303917947,
0.135243500605047));
#152911=CARTESIAN_POINT('Ctrl Pts',(5.881485942,1.198733649,-4.239177174));
#152912=CARTESIAN_POINT('Ctrl Pts',(5.650565757,1.134619049,-4.559558646));
#152913=CARTESIAN_POINT('Ctrl Pts',(5.386210996,1.069390921,-4.852961066));
#152914=CARTESIAN_POINT('Ctrl Pts',(5.38356005356643,1.06873681508671,-4.85590329757679));
#152915=CARTESIAN_POINT('Ctrl Pts',(5.38090911113287,1.06808270917341,-4.85884552915358));
#152916=CARTESIAN_POINT('Ctrl Pts',(6.224842549,1.198733649,-4.183459721));
#152917=CARTESIAN_POINT('Ctrl Pts',(5.996957454,1.134619049,-4.522544817));
#152918=CARTESIAN_POINT('Ctrl Pts',(5.733588172,1.069390921,-4.834869871));
#152919=CARTESIAN_POINT('Ctrl Pts',(5.73094711192334,1.06873681508671,-4.83800185824163));
#152920=CARTESIAN_POINT('Ctrl Pts',(5.72830605184669,1.06808270917341,-4.84113384548325));
#152921=CARTESIAN_POINT('',(5.5598995967194,1.06939091791719,-4.84391545390054));
#152922=CARTESIAN_POINT('Ctrl Pts',(5.39148132667974,1.06811592995213,-4.84711162513904));
#152923=CARTESIAN_POINT('Ctrl Pts',(5.38884616133988,1.06875342547606,-4.85003634556952));
#152924=CARTESIAN_POINT('Ctrl Pts',(5.386210996,1.069390921,-4.852961066));
#152925=CARTESIAN_POINT('Ctrl Pts',(5.381998728,1.070409947,-4.857636183));
#152926=CARTESIAN_POINT('Ctrl Pts',(5.377778351,1.071428571,-4.862303981));
#152927=CARTESIAN_POINT('Ctrl Pts',(5.116452959,1.134501699,-5.15133363500001));
#152928=CARTESIAN_POINT('Ctrl Pts',(4.82565450100001,1.198754474,-5.410689294));
#152929=CARTESIAN_POINT('Ctrl Pts',(5.40994977202152,1.06811592995213,-5.19446915376555));
#152930=CARTESIAN_POINT('Ctrl Pts',(5.40712598101076,1.06875342547606,-5.19740369788277));
#152931=CARTESIAN_POINT('Ctrl Pts',(5.40430219,1.069390921,-5.200338242));
#152932=CARTESIAN_POINT('Ctrl Pts',(5.399788407,1.070409947,-5.205029062));
#152933=CARTESIAN_POINT('Ctrl Pts',(5.395266487,1.071428571,-5.209712039));
#152934=CARTESIAN_POINT('Ctrl Pts',(5.115269587,1.134501699,-5.499681596));
#152935=CARTESIAN_POINT('Ctrl Pts',(4.805806437,1.198754474,-5.757970518));
#152936=CARTESIAN_POINT('',(5.40430218280845,1.06939091911149,-5.20033824619054));
#152937=CARTESIAN_POINT('',(4.99480117958429,1.15903910589032,-5.59481556208076));
#152938=CARTESIAN_POINT('Origin',(-0.0991854125737524,1.3383839565782,0.153907115829031));
#152939=CARTESIAN_POINT('Ctrl Pts',(4.82918965631122,1.19797317332657,-5.40753430549404));
#152940=CARTESIAN_POINT('Ctrl Pts',(4.85666484372267,1.1911656561366,-5.43878046336018));
#152941=CARTESIAN_POINT('Ctrl Pts',(4.88422192477404,1.18452222157352,-5.47002543160182));
#152942=CARTESIAN_POINT('Ctrl Pts',(4.93941929418718,1.17155461463316,-5.53243965416407));
#152943=CARTESIAN_POINT('Ctrl Pts',(4.96709190597967,1.16522285273282,-5.56364544646066));
#152944=CARTESIAN_POINT('Ctrl Pts',(4.99480117805053,1.15903910502987,-5.59481556327352));
#152945=CARTESIAN_POINT('',(5.39525658128272,1.06939091820872,-5.02664966657652));
#152946=CARTESIAN_POINT('Origin',(6.0281640790194E-14,1.16011713399972,
1.37476835471162E-13));
#152947=CARTESIAN_POINT('',(4.99966550416853,0.979367659117338,-5.59046910769365));
#152948=CARTESIAN_POINT('Origin',(-0.123936256261242,0.946436354951502,
0.146529879828055));
#152949=CARTESIAN_POINT('',(4.56018596634018,1.06939091992731,-5.95438526676254));
#152950=CARTESIAN_POINT('Origin',(-0.141684595606068,0.803756645137163,
0.116527713010236));
#152951=CARTESIAN_POINT('Origin',(-0.0977841519629702,0.94650933355158,
0.160005103084018));
#152952=CARTESIAN_POINT('Ctrl Pts',(4.832682286,1.198733649,-5.404413189));
#152953=CARTESIAN_POINT('Ctrl Pts',(4.53828834,1.134619049,-5.667663307));
#152954=CARTESIAN_POINT('Ctrl Pts',(4.217041199,1.069390921,-5.897377682));
#152955=CARTESIAN_POINT('Ctrl Pts',(4.2138197413099,1.06873681508671,-5.89968125157441));
#152956=CARTESIAN_POINT('Ctrl Pts',(4.2105982836198,1.06808270917341,-5.90198482114881));
#152957=CARTESIAN_POINT('Ctrl Pts',(5.17998901100001,1.198733649,-5.423809901));
#152958=CARTESIAN_POINT('Ctrl Pts',(4.884538471,1.134619049,-5.705978816));
#152959=CARTESIAN_POINT('Ctrl Pts',(4.560185962,1.069390921,-5.954385274));
#152960=CARTESIAN_POINT('Ctrl Pts',(4.55693336376311,1.06873681508671,-5.95687628728));
#152961=CARTESIAN_POINT('Ctrl Pts',(4.55368076552623,1.06808270917341,-5.95936730056002));
#152962=CARTESIAN_POINT('',(4.38861359606052,1.06939091791719,-5.92588146647613));
#152963=CARTESIAN_POINT('Ctrl Pts',(4.22344576855884,1.06811592995244,-5.89279796219269));
#152964=CARTESIAN_POINT('Ctrl Pts',(4.22024348377942,1.06875342547622,-5.89508782209635));
#152965=CARTESIAN_POINT('Ctrl Pts',(4.217041199,1.069390921,-5.89737768200001));
#152966=CARTESIAN_POINT('Ctrl Pts',(4.2119224,1.070409947,-5.90103798500001));
#152967=CARTESIAN_POINT('Ctrl Pts',(4.206797255,1.071428571,-5.904689396));
#152968=CARTESIAN_POINT('Ctrl Pts',(3.889448673,1.134501699,-6.130784462));
#152969=CARTESIAN_POINT('Ctrl Pts',(3.549695121,1.198754474,-6.321563458));
#152970=CARTESIAN_POINT('Ctrl Pts',(4.16681083229441,1.06811592995244,-6.2360046363775));
#152971=CARTESIAN_POINT('Ctrl Pts',(4.1634222196472,1.06875342547622,-6.23826354068875));
#152972=CARTESIAN_POINT('Ctrl Pts',(4.160033607,1.069390921,-6.240522445));
#152973=CARTESIAN_POINT('Ctrl Pts',(4.154616966,1.070409947,-6.244133266));
#152974=CARTESIAN_POINT('Ctrl Pts',(4.149194064,1.071428571,-6.247734679));
#152975=CARTESIAN_POINT('Ctrl Pts',(3.813408453,1.134501699,-6.470733852));
#152976=CARTESIAN_POINT('Ctrl Pts',(3.455655896,1.198754474,-6.656458693));
#152977=CARTESIAN_POINT('',(4.16003359904353,1.06939091911123,-6.24052244736327));
#152978=CARTESIAN_POINT('',(3.67530553951482,1.15903910585863,-6.53774649177692));
#152979=CARTESIAN_POINT('Origin',(-0.0637810247764503,1.33838400211325,
0.171630786261117));
#152980=CARTESIAN_POINT('Ctrl Pts',(3.55382585549297,1.19797317334867,-6.31924218533958));
#152981=CARTESIAN_POINT('Ctrl Pts',(3.57394168117612,1.19116565846847,-6.35566416603344));
#152982=CARTESIAN_POINT('Ctrl Pts',(3.59413774078712,1.18452222623441,-6.39210258828997));
#152983=CARTESIAN_POINT('Ctrl Pts',(3.63462742819504,1.17155461460377,-6.46492342989095));
#152984=CARTESIAN_POINT('Ctrl Pts',(3.65494474674917,1.16522285272797,-6.50134844137981));
#152985=CARTESIAN_POINT('Ctrl Pts',(3.67530553778319,1.15903910500572,-6.53774649260067));
#152986=CARTESIAN_POINT('',(4.18853738885056,1.06939091820823,-6.06895007326536));
#152987=CARTESIAN_POINT('Origin',(-9.9031026434826E-13,1.16011713399994,
1.74730022117764E-12));
#152988=CARTESIAN_POINT('',(3.68099049779525,0.979367659150468,-6.53454734113609));
#152989=CARTESIAN_POINT('Origin',(-0.0895392482799334,0.946436331401545,
0.169746975250635));
#152990=CARTESIAN_POINT('',(3.1735545308418,1.06939091992736,-6.7954802328553));
#152991=CARTESIAN_POINT('Origin',(-0.113322216432054,0.803756648482305,
0.144261627842868));
#152992=CARTESIAN_POINT('Origin',(-0.0611017779390599,0.94650932016441,
0.177285241390716));
#152993=CARTESIAN_POINT('Ctrl Pts',(3.557907777,1.198733649,-6.31694485100001));
#152994=CARTESIAN_POINT('Ctrl Pts',(3.213805605,1.134619049,-6.510754331));
#152995=CARTESIAN_POINT('Ctrl Pts',(2.850687243,1.069390921,-6.666039472));
#152996=CARTESIAN_POINT('Ctrl Pts',(2.84704590183182,1.06873681508671,-6.6675966672176));
#152997=CARTESIAN_POINT('Ctrl Pts',(2.84340456066365,1.06808270917341,-6.6691538624352));
#152998=CARTESIAN_POINT('Ctrl Pts',(3.892924945,1.198733649,-6.410548758));
#152999=CARTESIAN_POINT('Ctrl Pts',(3.543723898,1.134619049,-6.622607587));
#153000=CARTESIAN_POINT('Ctrl Pts',(3.173554525,1.069390921,-6.795480239));
#153001=CARTESIAN_POINT('Ctrl Pts',(3.16984247648315,1.06873681508671,-6.7972138013049));
#153002=CARTESIAN_POINT('Ctrl Pts',(3.1661304279663,1.06808270917341,-6.79894736360979));
#153003=CARTESIAN_POINT('',(3.01212090167396,1.06939091791719,-6.73075984759063));
#153004=CARTESIAN_POINT('Ctrl Pts',(2.85792658132718,1.06811592995212,-6.66294361747869));
#153005=CARTESIAN_POINT('Ctrl Pts',(2.85430691216359,1.06875342547606,-6.66449154473935));
#153006=CARTESIAN_POINT('Ctrl Pts',(2.850687243,1.069390921,-6.666039472));
#153007=CARTESIAN_POINT('Ctrl Pts',(2.844901262,1.070409947,-6.66851380800001));
#153008=CARTESIAN_POINT('Ctrl Pts',(2.839110994,1.071428571,-6.670978097));
#153009=CARTESIAN_POINT('Ctrl Pts',(2.48057809,1.134501699,-6.823566622));
#153010=CARTESIAN_POINT('Ctrl Pts',(2.107755942,1.198754474,-6.93684834));
#153011=CARTESIAN_POINT('Ctrl Pts',(2.72883644918952,1.06811592995212,-6.98595147272629));
#153012=CARTESIAN_POINT('Ctrl Pts',(2.72504146259476,1.06875342547606,-6.98742911336314));
#153013=CARTESIAN_POINT('Ctrl Pts',(2.721246476,1.069390921,-6.988906754));
#153014=CARTESIAN_POINT('Ctrl Pts',(2.715180253,1.070409947,-6.991268738));
#153015=CARTESIAN_POINT('Ctrl Pts',(2.709109939,1.071428571,-6.993620188));
#153016=CARTESIAN_POINT('Ctrl Pts',(2.333236578,1.134501699,-7.139221784));
#153017=CARTESIAN_POINT('Ctrl Pts',(1.943922727,1.198754474,-7.243698257));
#153018=CARTESIAN_POINT('',(2.72124646772611,1.06939091911157,-6.98890675455456));
#153019=CARTESIAN_POINT('',(2.18395669755006,1.15903910587617,-7.17497966133097));
#153020=CARTESIAN_POINT('Origin',(-0.0253943220334973,1.33838395587535,
0.181329189256539));
#153021=CARTESIAN_POINT('Ctrl Pts',(2.11228910713819,1.19797317338517,-6.93546932305721));
#153022=CARTESIAN_POINT('Ctrl Pts',(2.1241050465527,1.19116562424527,-6.97536428671798));
#153023=CARTESIAN_POINT('Ctrl Pts',(2.13599581747036,1.18452215738752,-7.01529257794451));
#153024=CARTESIAN_POINT('Ctrl Pts',(2.15988442353831,1.17155461460947,-7.09511457081028));
#153025=CARTESIAN_POINT('Ctrl Pts',(2.17189643372923,1.16522285276294,-7.13505560849572));
#153026=CARTESIAN_POINT('Ctrl Pts',(2.18395669573087,1.15903910503581,-7.17497966175034));
#153027=CARTESIAN_POINT('',(2.78596684358495,1.06939091820872,-6.82747311949418));
#153028=CARTESIAN_POINT('Origin',(-1.41271543074861E-13,1.16011713400044,
2.67581096169422E-13));
#153029=CARTESIAN_POINT('',(2.1901964674615,0.979367659171838,-7.17307740322741));
#153030=CARTESIAN_POINT('Origin',(-0.050955182254146,0.946436337456487,
0.185026366150669));
#153031=CARTESIAN_POINT('',(1.63853121200223,1.06939091992734,-7.31882609525481));
#153032=CARTESIAN_POINT('Origin',(-0.0796607088836709,0.803756648666082,
0.165249406374038));
#153033=CARTESIAN_POINT('Origin',(-0.0215621339804298,0.946509307655302,
0.186275393095969));
#153034=CARTESIAN_POINT('Ctrl Pts',(2.116769455,1.198733649,-6.934103192));
#153035=CARTESIAN_POINT('Ctrl Pts',(1.739048891,1.134619049,-7.049409718));
#153036=CARTESIAN_POINT('Ctrl Pts',(1.35103832,1.069390921,-7.123004665));
#153037=CARTESIAN_POINT('Ctrl Pts',(1.34714736042944,1.06873681508671,-7.12374267314921));
#153038=CARTESIAN_POINT('Ctrl Pts',(1.34325640085888,1.06808270917341,-7.1244806812984));
#153039=CARTESIAN_POINT('Ctrl Pts',(2.423832035,1.198733649,-7.097537479));
#153040=CARTESIAN_POINT('Ctrl Pts',(2.037208734,1.134619049,-7.22957058800001));
#153041=CARTESIAN_POINT('Ctrl Pts',(1.638531205,1.069390921,-7.3188261));
#153042=CARTESIAN_POINT('Ctrl Pts',(1.6345332774615,1.06873681508671,-7.31972115187383));
#153043=CARTESIAN_POINT('Ctrl Pts',(1.630535349923,1.06808270917341,-7.32061620374768));
#153044=CARTESIAN_POINT('',(1.49478478146109,1.06939091791719,-7.22091537857491));
#153045=CARTESIAN_POINT('Ctrl Pts',(1.35877392497451,1.06811592995337,-7.12153743298077));
#153046=CARTESIAN_POINT('Ctrl Pts',(1.35490612248726,1.06875342547668,-7.12227104899038));
#153047=CARTESIAN_POINT('Ctrl Pts',(1.35103832,1.069390921,-7.123004665));
#153048=CARTESIAN_POINT('Ctrl Pts',(1.344855702,1.070409947,-7.124177338));
#153049=CARTESIAN_POINT('Ctrl Pts',(1.338671059,1.071428571,-7.125339276));
#153050=CARTESIAN_POINT('Ctrl Pts',(0.955718432,1.134501699,-7.19728639));
#153051=CARTESIAN_POINT('Ctrl Pts',(0.567260438,1.198754474,-7.227773903));
#153052=CARTESIAN_POINT('Ctrl Pts',(1.16326470617094,1.06811592995337,-7.40924298181097));
#153053=CARTESIAN_POINT('Ctrl Pts',(1.15924079508547,1.06875342547668,-7.40987026640548));
#153054=CARTESIAN_POINT('Ctrl Pts',(1.155216884,1.069390921,-7.410497551));
#153055=CARTESIAN_POINT('Ctrl Pts',(1.148784729,1.070409947,-7.411500255));
#153056=CARTESIAN_POINT('Ctrl Pts',(1.142350843,1.071428571,-7.412491791));
#153057=CARTESIAN_POINT('Ctrl Pts',(0.743965153,1.134501699,-7.47388764));
#153058=CARTESIAN_POINT('Ctrl Pts',(0.341293891,1.198754474,-7.492230541));
#153059=CARTESIAN_POINT('',(1.15521687581794,1.06939091911024,-7.41049754966549));
#153060=CARTESIAN_POINT('',(0.590488466701952,1.15903910589274,-7.47671875687175));
#153061=CARTESIAN_POINT('Origin',(0.0141798106748021,1.33838402878226,0.182548839069203));
#153062=CARTESIAN_POINT('Ctrl Pts',(0.571984068188111,1.19797317337619,
-7.22740162320938));
#153063=CARTESIAN_POINT('Ctrl Pts',(0.574947519443085,1.19116562425375,
-7.26890394257768));
#153064=CARTESIAN_POINT('Ctrl Pts',(0.577976888262406,1.18452215740707,
-7.31045489687104));
#153065=CARTESIAN_POINT('Ctrl Pts',(0.584147622817373,1.17155461463842,
-7.39354604020064));
#153066=CARTESIAN_POINT('Ctrl Pts',(0.587292656358846,1.16522285274723,
-7.43513550608413));
#153067=CARTESIAN_POINT('Ctrl Pts',(0.590488464750283,1.15903910503688,
-7.47671875689447));
#153068=CARTESIAN_POINT('',(1.25312758504849,1.06939091820667,-7.26675111092324));
#153069=CARTESIAN_POINT('Origin',(1.5748036555352E-14,1.16011713400006,
7.30318583386236E-13));
#153070=CARTESIAN_POINT('',(0.596991284787135,0.979367659177192,-7.47620233853123));
#153071=CARTESIAN_POINT('Origin',(-0.00998869212352212,0.946436346326042,
0.191654495969603));
#153072=CARTESIAN_POINT('',(0.0268919958833657,1.06939091992737,-7.49995178487649));
#153073=CARTESIAN_POINT('Origin',(-0.042274564920128,0.803756675780424,
0.178510930582303));
#153074=CARTESIAN_POINT('Origin',(0.0189856731973442,0.946509307003066,
0.186555619158163));
#153075=CARTESIAN_POINT('Ctrl Pts',(0.576653346,1.198733649,-7.227030574));
#153076=CARTESIAN_POINT('Ctrl Pts',(0.182976184,1.134619049,-7.258442542));
#153077=CARTESIAN_POINT('Ctrl Pts',(-0.211783654,1.069390921,-7.246906077));
#153078=CARTESIAN_POINT('Ctrl Pts',(-0.215742295038516,1.06873681508671,
-7.24679038963925));
#153079=CARTESIAN_POINT('Ctrl Pts',(-0.219700936077032,1.06808270917341,
-7.24667470227851));
#153080=CARTESIAN_POINT('Ctrl Pts',(0.841403432,1.198733649,-7.452653237));
#153081=CARTESIAN_POINT('Ctrl Pts',(0.435435954,1.134619049,-7.498486904));
#153082=CARTESIAN_POINT('Ctrl Pts',(0.026891988,1.069390921,-7.499951788));
#153083=CARTESIAN_POINT('Ctrl Pts',(0.0227951200966198,1.06873681508671,
-7.49996647781735));
#153084=CARTESIAN_POINT('Ctrl Pts',(0.0186982521932396,1.06808270917341,
-7.49998116763471));
#153085=CARTESIAN_POINT('',(-0.0924458136384814,1.06939091791719,-7.37342893274275));
#153086=CARTESIAN_POINT('Ctrl Pts',(-0.203913492723738,1.06811592995213,
-7.24713607501221));
#153087=CARTESIAN_POINT('Ctrl Pts',(-0.207848573361869,1.06875342547606,
-7.24702107600611));
#153088=CARTESIAN_POINT('Ctrl Pts',(-0.211783654,1.069390921,-7.246906077));
#153089=CARTESIAN_POINT('Ctrl Pts',(-0.218073815,1.070409947,-7.246722253));
#153090=CARTESIAN_POINT('Ctrl Pts',(-0.224363648,1.071428571,-7.24652751));
#153091=CARTESIAN_POINT('Ctrl Pts',(-0.613829558,1.134501699,-7.234469046));
#153092=CARTESIAN_POINT('Ctrl Pts',(-0.999759533999999,1.198754474,-7.180736792));
#153093=CARTESIAN_POINT('Ctrl Pts',(-0.45670000052831,1.06811592995213,
-7.48608652399922));
#153094=CARTESIAN_POINT('Ctrl Pts',(-0.460764682764155,1.06875342547606,
-7.48583412099961));
#153095=CARTESIAN_POINT('Ctrl Pts',(-0.464829365,1.069390921,-7.485581718));
#153096=CARTESIAN_POINT('Ctrl Pts',(-0.471326692,1.070409947,-7.485178256));
#153097=CARTESIAN_POINT('Ctrl Pts',(-0.477823308,1.071428571,-7.484763516));
#153098=CARTESIAN_POINT('Ctrl Pts',(-0.880093255,1.134501699,-7.459082817));
#153099=CARTESIAN_POINT('Ctrl Pts',(-1.277293469,1.198754474,-7.39043445200001));
#153100=CARTESIAN_POINT('',(-0.464829372799176,1.06939091911153,-7.48558171513683));
#153101=CARTESIAN_POINT('',(-1.03059034795361,1.15903910584036,-7.42885479283027));
#153102=CARTESIAN_POINT('Origin',(0.0530909045809279,1.33838406702624,0.175232705328355));
#153103=CARTESIAN_POINT('Ctrl Pts',(-0.995066310316853,1.19797317334389,
-7.18138865679072));
#153104=CARTESIAN_POINT('Ctrl Pts',(-1.0010939147494,1.19116562419481,-7.22255772936614));
#153105=CARTESIAN_POINT('Ctrl Pts',(-1.00706759778314,1.18452215732646,
-7.2637884701795));
#153106=CARTESIAN_POINT('Ctrl Pts',(-1.0189032710843,1.17155461456224,-7.34626351406299));
#153107=CARTESIAN_POINT('Ctrl Pts',(-1.02477227239017,1.16522285266749,
-7.3875567305792));
#153108=CARTESIAN_POINT('Ctrl Pts',(-1.0305903498677,1.15903910495932,-7.42885479242869));
#153109=CARTESIAN_POINT('',(-0.338306526670948,1.06939091820872,-7.3662438967114));
#153110=CARTESIAN_POINT('Origin',(-1.29291109068896E-13,1.16011713399978,
-6.56159154788227E-13));
#153111=CARTESIAN_POINT('',(-1.02412854774879,0.979367659155358,-7.42974836164533));
#153112=CARTESIAN_POINT('Origin',(0.0314449104851384,0.946436323522522,
0.189321198650079));
#153113=CARTESIAN_POINT('',(-1.58600466060697,1.06939091992739,-7.33038806365574));
#153114=CARTESIAN_POINT('Origin',(-0.0029116071295629,0.803756661929236,
0.183425348603111));
#153115=CARTESIAN_POINT('Origin',(0.0586457268839945,0.946509308198984,
0.178112571944439));
#153116=CARTESIAN_POINT('Ctrl Pts',(-0.990426433,1.198733649,-7.182030039));
#153117=CARTESIAN_POINT('Ctrl Pts',(-1.381652286,1.134619049,-7.12807866));
#153118=CARTESIAN_POINT('Ctrl Pts',(-1.764702859,1.069390921,-7.03195021400001));
#153119=CARTESIAN_POINT('Ctrl Pts',(-1.76854407984401,1.06873681508671,
-7.03098624052886));
#153120=CARTESIAN_POINT('Ctrl Pts',(-1.77238530068803,1.06808270917341,
-7.03002226705771));
#153121=CARTESIAN_POINT('Ctrl Pts',(-0.780368259,1.198733649,-7.459291212));
#153122=CARTESIAN_POINT('Ctrl Pts',(-1.186697327,1.134619049,-7.416782306));
#153123=CARTESIAN_POINT('Ctrl Pts',(-1.586004669,1.069390921,-7.330388065));
#153124=CARTESIAN_POINT('Ctrl Pts',(-1.59000891228632,1.06873681508671,
-7.3295217058748));
#153125=CARTESIAN_POINT('Ctrl Pts',(-1.59401315557265,1.06808270917341,
-7.3286553467496));
#153126=CARTESIAN_POINT('',(-1.67535374514333,1.06939091791719,-7.18116914389923));
#153127=CARTESIAN_POINT('Ctrl Pts',(-1.75706614025095,1.06811592995213,
-7.03386668559918));
#153128=CARTESIAN_POINT('Ctrl Pts',(-1.76088449962548,1.06875342547606,
-7.03290844979959));
#153129=CARTESIAN_POINT('Ctrl Pts',(-1.764702859,1.069390921,-7.031950214));
#153130=CARTESIAN_POINT('Ctrl Pts',(-1.770806443,1.070409947,-7.03041849));
#153131=CARTESIAN_POINT('Ctrl Pts',(-1.776907359,1.071428571,-7.028876172));
#153132=CARTESIAN_POINT('Ctrl Pts',(-2.154675559,1.134501699,-6.93337597));
#153133=CARTESIAN_POINT('Ctrl Pts',(-2.52003186,1.198754474,-6.79793640900001));
#153134=CARTESIAN_POINT('Ctrl Pts',(-2.05530992479782,1.06811592995213,
-7.21288898031393));
#153135=CARTESIAN_POINT('Ctrl Pts',(-2.05922531739891,1.06875342547606,
-7.21176869215696));
#153136=CARTESIAN_POINT('Ctrl Pts',(-2.06314071,1.069390921,-7.210648404));
#153137=CARTESIAN_POINT('Ctrl Pts',(-2.0693994,1.070409947,-7.208857642));
#153138=CARTESIAN_POINT('Ctrl Pts',(-2.075654973,1.071428571,-7.207056017));
#153139=CARTESIAN_POINT('Ctrl Pts',(-2.46299948,1.134501699,-7.095499572));
#153140=CARTESIAN_POINT('Ctrl Pts',(-2.836156005,1.198754474,-6.943069863));
#153141=CARTESIAN_POINT('',(-2.06314071700248,1.06939091911153,-7.21064839952851));
#153142=CARTESIAN_POINT('',(-2.60347990315653,1.15903910587584,-7.03362583537486));
#153143=CARTESIAN_POINT('Origin',(0.0895195164046692,1.33838403536281,0.159722890325232));
#153144=CARTESIAN_POINT('Ctrl Pts',(-2.51558849334323,1.19797317341412,
-6.79958193777258));
#153145=CARTESIAN_POINT('Ctrl Pts',(-2.53032530942631,1.19116562429394,
-6.83849274352607));
#153146=CARTESIAN_POINT('Ctrl Pts',(-2.54502272157404,1.18452215744368,
-6.87747536725597));
#153147=CARTESIAN_POINT('Ctrl Pts',(-2.57431138011397,1.17155461460349,
-6.9554778711486));
#153148=CARTESIAN_POINT('Ctrl Pts',(-2.58891998821519,1.16522285277055,
-6.99454401305868));
#153149=CARTESIAN_POINT('Ctrl Pts',(-2.60347990485454,1.15903910504116,
-7.0336258346102));
#153150=CARTESIAN_POINT('',(-1.91392180109997,1.06939091820872,-7.12129930453859));
#153151=CARTESIAN_POINT('Origin',(-4.17634676841416E-13,1.16011713399994,
-1.19002030452009E-12));
#153152=CARTESIAN_POINT('',(-2.59736126722514,0.979367659142584,-7.0358876089964));
#153153=CARTESIAN_POINT('Origin',(0.0714082026105445,0.946436336876394,
0.178135238070495));
#153154=CARTESIAN_POINT('',(-3.12474150253183,1.06939091992737,-6.8180635444769));
#153155=CARTESIAN_POINT('Origin',(0.0365874470695776,0.803756633914609,
0.179762794930365));
#153156=CARTESIAN_POINT('Origin',(0.0955636390219455,0.946509331580637,
0.161341518403026));
#153157=CARTESIAN_POINT('Ctrl Pts',(-2.511194972,1.198733649,-6.80120576200001));
#153158=CARTESIAN_POINT('Ctrl Pts',(-2.881676231,1.134619049,-6.66441374200001));
#153159=CARTESIAN_POINT('Ctrl Pts',(-3.23510652,1.069390921,-6.488188176));
#153160=CARTESIAN_POINT('Ctrl Pts',(-3.23865070943269,1.06873681508671,
-6.48642099076369));
#153161=CARTESIAN_POINT('Ctrl Pts',(-3.24219489886538,1.06808270917341,
-6.48465380552737));
#153162=CARTESIAN_POINT('Ctrl Pts',(-2.365650799,1.198733649,-7.11714102));
#153163=CARTESIAN_POINT('Ctrl Pts',(-2.75334196,1.134619049,-6.98827721));
#153164=CARTESIAN_POINT('Ctrl Pts',(-3.124741511,1.069390921,-6.818063544));
#153165=CARTESIAN_POINT('Ctrl Pts',(-3.12846589570875,1.06873681508671,
-6.8163566459352));
#153166=CARTESIAN_POINT('Ctrl Pts',(-3.1321902804175,1.06808270917341,-6.81464974787039));
#153167=CARTESIAN_POINT('',(-3.17992399802989,1.06939091791719,-6.65312586835001));
#153168=CARTESIAN_POINT('Ctrl Pts',(-3.22806032850427,1.06811592995213,
-6.49170151124601));
#153169=CARTESIAN_POINT('Ctrl Pts',(-3.23158342425213,1.06875342547606,
-6.48994484362301));
#153170=CARTESIAN_POINT('Ctrl Pts',(-3.23510652,1.069390921,-6.488188176));
#153171=CARTESIAN_POINT('Ctrl Pts',(-3.24073813,1.070409947,-6.485380172));
#153172=CARTESIAN_POINT('Ctrl Pts',(-3.246364857,1.071428571,-6.482562396));
#153173=CARTESIAN_POINT('Ctrl Pts',(-3.594771326,1.134501699,-6.308085939));
#153174=CARTESIAN_POINT('Ctrl Pts',(-3.922470298,1.198754474,-6.097272075));
#153175=CARTESIAN_POINT('Ctrl Pts',(-3.55781583914299,1.06811592995213,
-6.6024247660727));
#153176=CARTESIAN_POINT('Ctrl Pts',(-3.5613988635715,1.06875342547606,-6.60048897553635));
#153177=CARTESIAN_POINT('Ctrl Pts',(-3.564981888,1.069390921,-6.598553185));
#153178=CARTESIAN_POINT('Ctrl Pts',(-3.570709293,1.070409947,-6.595458856));
#153179=CARTESIAN_POINT('Ctrl Pts',(-3.576431317,1.071428571,-6.592354589));
#153180=CARTESIAN_POINT('Ctrl Pts',(-3.930738587,1.134501699,-6.400138652));
#153181=CARTESIAN_POINT('Ctrl Pts',(-4.262403038,1.198754474,-6.17105504300001));
#153182=CARTESIAN_POINT('',(-3.56498189383506,1.06939091911155,-6.59855317909549));
#153183=CARTESIAN_POINT('',(-4.05463363206377,1.15903910590348,-6.30951235096862));
#153184=CARTESIAN_POINT('Origin',(0.121762300074483,1.33838403875015,0.136744607366341));
#153185=CARTESIAN_POINT('Ctrl Pts',(-3.91848455494606,1.19797317343746,
-6.09983432463178));
#153186=CARTESIAN_POINT('Ctrl Pts',(-3.94124150543094,1.19116562430746,
-6.13466743758724));
#153187=CARTESIAN_POINT('Ctrl Pts',(-3.96397541200388,1.18452215745755,
-6.1695791600814));
#153188=CARTESIAN_POINT('Ctrl Pts',(-4.00934755051591,1.17155461463885,
-6.23946181284915));
#153189=CARTESIAN_POINT('Ctrl Pts',(-4.03201268338122,1.16522285276633,
-6.27447419137526));
#153190=CARTESIAN_POINT('Ctrl Pts',(-4.05463363359707,1.15903910506087,
-6.30951234983));
#153191=CARTESIAN_POINT('',(-3.40004421925281,1.06939091820872,-6.54337067257439));
#153192=CARTESIAN_POINT('Origin',(3.70580302555545E-13,1.16011713399972,
5.26922255827955E-13));
#153193=CARTESIAN_POINT('',(-4.04914426134537,0.979367659186683,-6.31303657114383));
#153194=CARTESIAN_POINT('Origin',(0.108032464833622,0.946436291803525,0.158619752436514));
#153195=CARTESIAN_POINT('',(-4.51736890386031,1.06939091992732,-5.98693395125204));
#153196=CARTESIAN_POINT('Origin',(0.0743757745959278,0.80375664599575,0.1676948622839));
#153197=CARTESIAN_POINT('Origin',(0.128012932444943,0.946509301500725,0.137025874713763));
#153198=CARTESIAN_POINT('Ctrl Pts',(-3.914542826,1.198733649,-6.102364662));
#153199=CARTESIAN_POINT('Ctrl Pts',(-4.246956198,1.134619049,-5.889128244));
#153200=CARTESIAN_POINT('Ctrl Pts',(-4.554240196,1.069390921,-5.641045669));
#153201=CARTESIAN_POINT('Ctrl Pts',(-4.55732163166763,1.06873681508671,
-5.63855790361001));
#153202=CARTESIAN_POINT('Ctrl Pts',(-4.56040306733527,1.06808270917341,
-5.63607013822001));
#153203=CARTESIAN_POINT('Ctrl Pts',(-3.840318136,1.198733649,-6.442201224));
#153204=CARTESIAN_POINT('Ctrl Pts',(-4.191243384,1.134619049,-6.233008039));
#153205=CARTESIAN_POINT('Ctrl Pts',(-4.517368912,1.069390921,-5.98693394900001));
#153206=CARTESIAN_POINT('Ctrl Pts',(-4.52063929002373,1.06873681508671,
-5.98446632464357));
#153207=CARTESIAN_POINT('Ctrl Pts',(-4.52390966804747,1.06808270917341,
-5.98199870028714));
#153208=CARTESIAN_POINT('',(-4.53580453873334,1.06939091791719,-5.81398982091035));
#153209=CARTESIAN_POINT('Ctrl Pts',(-4.5481140040602,1.06811592995212,-5.64599158717323));
#153210=CARTESIAN_POINT('Ctrl Pts',(-4.5511771000301,1.06875342547606,-5.64351862808662));
#153211=CARTESIAN_POINT('Ctrl Pts',(-4.554240196,1.069390921,-5.64104566900001));
#153212=CARTESIAN_POINT('Ctrl Pts',(-4.559136504,1.070409947,-5.637092685));
#153213=CARTESIAN_POINT('Ctrl Pts',(-4.564025943,1.071428571,-5.633131207));
#153214=CARTESIAN_POINT('Ctrl Pts',(-4.866779581,1.134501699,-5.387836821));
#153215=CARTESIAN_POINT('Ctrl Pts',(-5.141498385,1.198754474,-5.111506076));
#153216=CARTESIAN_POINT('Ctrl Pts',(-4.89396224110399,1.06811592995212,
-5.68323850498272));
#153217=CARTESIAN_POINT('Ctrl Pts',(-4.897045358552,1.06875342547606,-5.68057772849136));
#153218=CARTESIAN_POINT('Ctrl Pts',(-4.900128476,1.069390921,-5.677916952));
#153219=CARTESIAN_POINT('Ctrl Pts',(-4.905056788,1.070409947,-5.673663745));
#153220=CARTESIAN_POINT('Ctrl Pts',(-4.909977709,1.071428571,-5.669401988));
#153221=CARTESIAN_POINT('Ctrl Pts',(-5.214680727,1.134501699,-5.405514363));
#153222=CARTESIAN_POINT('Ctrl Pts',(-5.489344843,1.198754474,-5.110488548));
#153223=CARTESIAN_POINT('',(-4.90012848048504,1.06939091911153,-5.67791694500488));
#153224=CARTESIAN_POINT('',(-5.31619719772624,1.15903910677738,-5.29037308240282));
#153225=CARTESIAN_POINT('Origin',(0.148311690093998,1.33838494836903,0.107372169549576));
#153226=CARTESIAN_POINT('Ctrl Pts',(-5.13815663368765,1.19797317323022,
-5.11486523948492));
#153227=CARTESIAN_POINT('Ctrl Pts',(-5.16786948413822,1.19116565731859,
-5.14399175972748));
#153228=CARTESIAN_POINT('Ctrl Pts',(-5.19757671253684,1.1845222240275,-5.1731999885154));
#153229=CARTESIAN_POINT('Ctrl Pts',(-5.25691108503454,1.17155461463184,
-5.23169545535011));
#153230=CARTESIAN_POINT('Ctrl Pts',(-5.28657294587277,1.16522285281417,
-5.26101693007331));
#153231=CARTESIAN_POINT('Ctrl Pts',(-5.31619719935021,1.15903910507514,
-5.29037308040545));
#153232=CARTESIAN_POINT('',(-4.72718434919243,1.06939091820872,-5.65948129948078));
#153233=CARTESIAN_POINT('Ctrl Pts',(-5.134851007,1.198733649,-5.118183773));
#153234=CARTESIAN_POINT('Ctrl Pts',(-5.413653213,1.134619049,-4.838473655));
#153235=CARTESIAN_POINT('Ctrl Pts',(-5.660422662,1.069390921,-4.530134136));
#153236=CARTESIAN_POINT('Ctrl Pts',(-5.66289725939779,1.06873681508671,
-4.52704211559617));
#153237=CARTESIAN_POINT('Ctrl Pts',(-5.66537185679557,1.06808270917341,
-4.52395009519234));
#153238=CARTESIAN_POINT('Ctrl Pts',(-5.135416465,1.198733649,-5.46603126000001));
#153239=CARTESIAN_POINT('Ctrl Pts',(-5.433166924,1.134619049,-5.18629033999999));
#153240=CARTESIAN_POINT('Ctrl Pts',(-5.698769164,1.069390921,-4.87586197700001));
#153241=CARTESIAN_POINT('Ctrl Pts',(-5.70143261611943,1.06873681508671,
-4.87274900972471));
#153242=CARTESIAN_POINT('Ctrl Pts',(-5.70409606823886,1.06808270917341,
-4.86963604244942));
#153243=CARTESIAN_POINT('',(-5.69876914857299,1.06939091993135,-4.8758619666544));
#153244=CARTESIAN_POINT('Origin',(0.15447204525214,0.946510515245744,0.106299044358358));
#153245=CARTESIAN_POINT('',(-5.67959590065063,1.06939091791719,-4.70299807141377));
#153246=CARTESIAN_POINT('Origin',(-2.07299455379228E-13,1.160117134,-1.76941794549634E-13));
#153247=CARTESIAN_POINT('',(-5.3115937688696,0.979367660225015,-5.29499496096233));
#153248=CARTESIAN_POINT('Origin',(0.139605180174829,0.946436327905003,0.131687433615584));
#153249=CARTESIAN_POINT('Origin',(0.108681843188683,0.803757173971954,0.147781049594621));
#153250=CARTESIAN_POINT('Ctrl Pts',(-5.65550292364228,1.06811592995212,
-4.53628137163686));
#153251=CARTESIAN_POINT('Ctrl Pts',(-5.65796279282114,1.06875342547606,
-4.53320775381843));
#153252=CARTESIAN_POINT('Ctrl Pts',(-5.660422662,1.069390921,-4.530134136));
#153253=CARTESIAN_POINT('Ctrl Pts',(-5.664354722,1.070409947,-4.525221009));
#153254=CARTESIAN_POINT('Ctrl Pts',(-5.668278248,1.071428571,-4.520301063));
#153255=CARTESIAN_POINT('Ctrl Pts',(-5.911222633,1.134501699,-4.215658441));
#153256=CARTESIAN_POINT('Ctrl Pts',(-6.120115721,1.198754474,-3.886731733));
#153257=CARTESIAN_POINT('Ctrl Pts',(-6.00127240686537,1.06811592995212,
-4.49831033178267));
#153258=CARTESIAN_POINT('Ctrl Pts',(-6.00371145443268,1.06875342547606,
-4.49504898289134));
#153259=CARTESIAN_POINT('Ctrl Pts',(-6.006150502,1.069390921,-4.491787634));
#153260=CARTESIAN_POINT('Ctrl Pts',(-6.010049279,1.070409947,-4.486574422));
#153261=CARTESIAN_POINT('Ctrl Pts',(-6.013939,1.071428571,-4.48135445));
#153262=CARTESIAN_POINT('Ctrl Pts',(-6.254790191,1.134501699,-4.158134229));
#153263=CARTESIAN_POINT('Ctrl Pts',(-6.459610984,1.198754474,-3.810961288));
#153264=CARTESIAN_POINT('',(-6.0061505046738,1.0693909191116,-4.4917876261598));
#153265=CARTESIAN_POINT('',(-5.83328659251519,1.06939091820872,-4.51096087140242));
#153266=CARTESIAN_POINT('',(-6.32918129250909,1.15903910586461,-4.02386184692367));
#153267=CARTESIAN_POINT('Origin',(0.167926042615231,1.3383840767741,0.0729793754949004));
#153268=CARTESIAN_POINT('Ctrl Pts',(-6.11757421903209,1.19797317328605,
-3.89073073857305));
#153269=CARTESIAN_POINT('Ctrl Pts',(-6.15285373554259,1.1911656583077,-3.91278890943602));
#153270=CARTESIAN_POINT('Ctrl Pts',(-6.188145325728,1.18452222597648,-3.93492808663254));
#153271=CARTESIAN_POINT('Ctrl Pts',(-6.25866730043927,1.17155461461106,
-3.97930083247413));
#153272=CARTESIAN_POINT('Ctrl Pts',(-6.29393893410434,1.16522285272675,
-4.0015603643175));
#153273=CARTESIAN_POINT('Ctrl Pts',(-6.32918129341782,1.15903910500407,
-4.02386184524901));
#153274=CARTESIAN_POINT('Origin',(-6.17127876578749E-13,1.16011713399983,
-4.562322741819E-13));
#153275=CARTESIAN_POINT('',(-6.61370129654141,1.06939091992739,-3.53680012252872));
#153276=CARTESIAN_POINT('Origin',(0.173717228195296,0.946509319216001,0.0706101781319868));
#153277=CARTESIAN_POINT('',(-6.32567905567461,0.979367659158276,-4.02936527022592));
#153278=CARTESIAN_POINT('Origin',(0.164650191334943,0.946436337767066,0.0985976552067486));
#153279=CARTESIAN_POINT('Origin',(0.137914834916094,0.803756629624046,0.120966140186841));
#153280=CARTESIAN_POINT('Ctrl Pts',(-6.115059263,1.198733649,-3.894682299));
#153281=CARTESIAN_POINT('Ctrl Pts',(-6.327213821,1.134619049,-3.561577415));
#153282=CARTESIAN_POINT('Ctrl Pts',(-6.501930055,1.069390921,-3.207398566));
#153283=CARTESIAN_POINT('Ctrl Pts',(-6.50368210469561,1.06873681508671,
-3.20384687002776));
#153284=CARTESIAN_POINT('Ctrl Pts',(-6.50543415439122,1.06808270917341,
-3.20029517405553));
#153285=CARTESIAN_POINT('Ctrl Pts',(-6.190388428,1.198733649,-4.234275748));
#153286=CARTESIAN_POINT('Ctrl Pts',(-6.42104161800001,1.134619049,-3.897067468));
#153287=CARTESIAN_POINT('Ctrl Pts',(-6.61370130300001,1.069390921,-3.536800117));
#153288=CARTESIAN_POINT('Ctrl Pts',(-6.61563328913966,1.06873681508671,
-3.53318736569346));
#153289=CARTESIAN_POINT('Ctrl Pts',(-6.61756527527932,1.06808270917341,
-3.52957461438691));
#153290=CARTESIAN_POINT('',(-6.55781567014536,1.06939091791719,-3.37209935871988));
#153291=CARTESIAN_POINT('Ctrl Pts',(-6.49844681077687,1.06811592995212,
-3.21445968164217));
#153292=CARTESIAN_POINT('Ctrl Pts',(-6.50018843288844,1.06875342547606,
-3.21092912382109));
#153293=CARTESIAN_POINT('Ctrl Pts',(-6.501930055,1.069390921,-3.207398566));
#153294=CARTESIAN_POINT('Ctrl Pts',(-6.504714009,1.070409947,-3.201755028));
#153295=CARTESIAN_POINT('Ctrl Pts',(-6.507488162,1.071428571,-3.196106666));
#153296=CARTESIAN_POINT('Ctrl Pts',(-6.679263483,1.134501699,-2.846360558));
#153297=CARTESIAN_POINT('Ctrl Pts',(-6.81256324800001,1.198754474,-2.480218134));
#153298=CARTESIAN_POINT('Ctrl Pts',(-6.82796974558505,1.06811592995212,
-3.10304616523142));
#153299=CARTESIAN_POINT('Ctrl Pts',(-6.82965067579253,1.06875342547606,
-3.09933674161571));
#153300=CARTESIAN_POINT('Ctrl Pts',(-6.831331606,1.069390921,-3.095627318));
#153301=CARTESIAN_POINT('Ctrl Pts',(-6.834018545,1.070409947,-3.089697866));
#153302=CARTESIAN_POINT('Ctrl Pts',(-6.836695187,1.071428571,-3.08376376));
#153303=CARTESIAN_POINT('Ctrl Pts',(-7.002432618,1.134501699,-2.716324361));
#153304=CARTESIAN_POINT('Ctrl Pts',(-7.127832894,1.198754474,-2.333237714));
#153305=CARTESIAN_POINT('',(-6.83133160687962,1.06939091911161,-3.09562730976832));
#153306=CARTESIAN_POINT('',(-7.04621990368853,1.15903910588547,-2.56919930445691));
#153307=CARTESIAN_POINT('Origin',(0.179688433322887,1.3383840144886,0.0351740334676576));
#153308=CARTESIAN_POINT('Ctrl Pts',(-6.81094083279843,1.19797317334171,
-2.48466999264094));
#153309=CARTESIAN_POINT('Ctrl Pts',(-6.85013758504179,1.19116562421767,
-2.49862847261659));
#153310=CARTESIAN_POINT('Ctrl Pts',(-6.88936356467505,1.18452215736906,
-2.5126634787143));
#153311=CARTESIAN_POINT('Ctrl Pts',(-6.96777518862747,1.17155461462058,
-2.54083852552382));
#153312=CARTESIAN_POINT('Ctrl Pts',(-7.00700733256815,1.16522285272643,
-2.55499528336012));
#153313=CARTESIAN_POINT('Ctrl Pts',(-7.04621990422763,1.15903910502355,
-2.56919930259339));
#153314=CARTESIAN_POINT('',(-6.6666308378463,1.06939091820872,-3.15151292645983));
#153315=CARTESIAN_POINT('Origin',(9.32413868337534E-14,1.16011713400033,
1.08637057683048E-13));
#153316=CARTESIAN_POINT('',(-7.04398262080491,0.979367659166783,-2.57532693793603));
#153317=CARTESIAN_POINT('Origin',(0.181996628548818,0.946436318537255,0.0608976861711508));
#153318=CARTESIAN_POINT('',(-7.21938411488094,1.06939091992739,-2.03236142178664));
#153319=CARTESIAN_POINT('Origin',(0.160694476192415,0.803756681254556,0.0884903519069058));
#153320=CARTESIAN_POINT('Origin',(0.184834718443735,0.946509311812307,0.0316152163446676));
#153321=CARTESIAN_POINT('Ctrl Pts',(-6.80933414400001,1.198733649,-2.489069809));
#153322=CARTESIAN_POINT('Ctrl Pts',(-6.944920943,1.134619049,-2.118145774));
#153323=CARTESIAN_POINT('Ctrl Pts',(-7.039414425,1.069390921,-1.734688604));
#153324=CARTESIAN_POINT('Ctrl Pts',(-7.04036200309612,1.06873681508671,
-1.73084330581221));
#153325=CARTESIAN_POINT('Ctrl Pts',(-7.04130958119224,1.06808270917341,
-1.72699800762441));
#153326=CARTESIAN_POINT('Ctrl Pts',(-6.955904708,1.198733649,-2.804530209));
#153327=CARTESIAN_POINT('Ctrl Pts',(-7.108675543,1.134619049,-2.425622053));
#153328=CARTESIAN_POINT('Ctrl Pts',(-7.21938412,1.069390921,-2.032361415));
#153329=CARTESIAN_POINT('Ctrl Pts',(-7.22049430263268,1.06873681508671,
-2.02841780789876));
#153330=CARTESIAN_POINT('Ctrl Pts',(-7.22160448526537,1.06808270917341,
-2.02447420079752));
#153331=CARTESIAN_POINT('',(-7.12939926755414,1.06939091791719,-1.88352502822078));
#153332=CARTESIAN_POINT('Ctrl Pts',(-7.03753054804731,1.06811592995241,
-1.7423334291813));
#153333=CARTESIAN_POINT('Ctrl Pts',(-7.03847248652365,1.0687534254762,-1.73851101659065));
#153334=CARTESIAN_POINT('Ctrl Pts',(-7.039414425,1.069390921,-1.734688604));
#153335=CARTESIAN_POINT('Ctrl Pts',(-7.040920098,1.070409947,-1.728578541));
#153336=CARTESIAN_POINT('Ctrl Pts',(-7.042415162,1.071428571,-1.722465874));
#153337=CARTESIAN_POINT('Ctrl Pts',(-7.134989397,1.134501699,-1.343970018));
#153338=CARTESIAN_POINT('Ctrl Pts',(-7.186462889,1.198754474,-0.957732292));
#153339=CARTESIAN_POINT('Ctrl Pts',(-7.33539880555853,1.06811592995241,
-1.56268700810849));
#153340=CARTESIAN_POINT('Ctrl Pts',(-7.33624302077927,1.0687534254762,-1.55870295855425));
#153341=CARTESIAN_POINT('Ctrl Pts',(-7.337087236,1.069390921,-1.554718909));
#153342=CARTESIAN_POINT('Ctrl Pts',(-7.33843670000001,1.070409947,-1.548350472));
#153343=CARTESIAN_POINT('Ctrl Pts',(-7.339775105,1.071428571,-1.541979703));
#153344=CARTESIAN_POINT('Ctrl Pts',(-7.422649079,1.134501699,-1.147502184));
#153345=CARTESIAN_POINT('Ctrl Pts',(-7.462765261,1.198754474,-0.746414538));
#153346=CARTESIAN_POINT('',(-7.33708723535121,1.06939091911119,-1.55471890071167));
#153347=CARTESIAN_POINT('',(-7.43378510362113,1.15903910586694,-0.994403858029308));
#153348=CARTESIAN_POINT('Origin',(0.183048793396375,1.33838406389971,-0.00427602568615876));
#153349=CARTESIAN_POINT('Ctrl Pts',(-7.18583542313158,1.19797317327582,
-0.962428840202223));
#153350=CARTESIAN_POINT('Ctrl Pts',(-7.22711623435964,1.19116565769764,
-0.967634809917467));
#153351=CARTESIAN_POINT('Ctrl Pts',(-7.26844201747691,1.18452222476187,
-0.972909229448894));
#153352=CARTESIAN_POINT('Ctrl Pts',(-7.35107765327792,1.17155461459036,
-0.983569433385695));
#153353=CARTESIAN_POINT('Ctrl Pts',(-7.39243585582729,1.16522285272814,
-0.988961462780946));
#153354=CARTESIAN_POINT('Ctrl Pts',(-7.43378510374658,1.15903910501563,
-0.994403856108894));
#153355=CARTESIAN_POINT('',(-7.18825083433454,1.06939091820823,-1.64470373974097));
#153356=CARTESIAN_POINT('Origin',(-9.86623976961809E-13,1.16011713399994,
-1.70219741080224E-13));
#153357=CARTESIAN_POINT('',(-7.43291738723043,0.97936765919445,-1.0008691806923));
#153358=CARTESIAN_POINT('Origin',(0.190832825435658,0.946436294533378,0.0203500377589748));
#153359=CARTESIAN_POINT('',(-7.4874965564513,1.06939091992734,-0.432891760688444));
#153360=CARTESIAN_POINT('Origin',(0.175960374723034,0.803756653729906,0.0518769504748556));
#153361=CARTESIAN_POINT('Origin',(0.187309731526595,0.946509314557843,-0.00885792245696237));
#153362=CARTESIAN_POINT('Ctrl Pts',(-7.185212128,1.198733649,-0.967071182));
#153363=CARTESIAN_POINT('Ctrl Pts',(-7.23789128,1.134619049,-0.575671991));
#153364=CARTESIAN_POINT('Ctrl Pts',(-7.2477436,1.069390921,-0.180866531));
#153365=CARTESIAN_POINT('Ctrl Pts',(-7.24784239879999,1.06873681508671,
-0.176907432465295));
#153366=CARTESIAN_POINT('Ctrl Pts',(-7.24794119759997,1.06808270917341,
-0.17294833393059));
#153367=CARTESIAN_POINT('Ctrl Pts',(-7.39617061500001,1.198733649,-1.243647954));
#153368=CARTESIAN_POINT('Ctrl Pts',(-7.4639157,1.134619049,-0.840757247));
#153369=CARTESIAN_POINT('Ctrl Pts',(-7.48749656,1.069390921,-0.432891753));
#153370=CARTESIAN_POINT('Ctrl Pts',(-7.48773302822988,1.06873681508671,
-0.428801688795589));
#153371=CARTESIAN_POINT('Ctrl Pts',(-7.48796949645976,1.06808270917341,
-0.424711624591177));
#153372=CARTESIAN_POINT('',(-7.36762007919418,1.06939091791717,-0.306879161346403));
#153373=CARTESIAN_POINT('Ctrl Pts',(-7.2475471775637,1.06811592995236,-0.188737601887027));
#153374=CARTESIAN_POINT('Ctrl Pts',(-7.24764538878185,1.06875342547618,
-0.184802066443513));
#153375=CARTESIAN_POINT('Ctrl Pts',(-7.2477436,1.069390921,-0.180866531));
#153376=CARTESIAN_POINT('Ctrl Pts',(-7.247900589,1.070409947,-0.174575643));
#153377=CARTESIAN_POINT('Ctrl Pts',(-7.248046656,1.071428571,-0.168284491));
#153378=CARTESIAN_POINT('Ctrl Pts',(-7.257091136,1.134501699,0.221263065));
#153379=CARTESIAN_POINT('Ctrl Pts',(-7.224331513,1.198754474,0.609536047));
#153380=CARTESIAN_POINT('Ctrl Pts',(-7.49983277261797,1.06811592995236,
0.0507416564256056));
#153381=CARTESIAN_POINT('Ctrl Pts',(-7.49980079730899,1.06875342547618,
0.0548140422128028));
#153382=CARTESIAN_POINT('Ctrl Pts',(-7.499768822,1.069390921,0.058886428));
#153383=CARTESIAN_POINT('Ctrl Pts',(-7.49971771,1.070409947,0.065396069));
#153384=CARTESIAN_POINT('Ctrl Pts',(-7.499655298,1.071428571,0.071905611));
#153385=CARTESIAN_POINT('Ctrl Pts',(-7.495790718,1.134501699,0.474975919));
#153386=CARTESIAN_POINT('Ctrl Pts',(-7.44874701800001,1.198754474,0.875310152000001));
#153387=CARTESIAN_POINT('',(-7.49976881957978,1.06939091911126,0.0588864359523553));
#153388=CARTESIAN_POINT('',(-7.47375477398927,1.15903910588506,0.626888807520051));
#153389=CARTESIAN_POINT('Origin',(0.177849996470257,1.33838404543367,-0.0435261314210013));
#153390=CARTESIAN_POINT('Ctrl Pts',(-7.22472833593332,1.19797317330152,
0.604814415005951));
#153391=CARTESIAN_POINT('Ctrl Pts',(-7.26616317337376,1.19116565457661,
0.608604313924491));
#153392=CARTESIAN_POINT('Ctrl Pts',(-7.30765664821257,1.18452221845763,
0.612337031058701));
#153393=CARTESIAN_POINT('Ctrl Pts',(-7.39065189683772,1.17155461462232,
0.619690272251385));
#153394=CARTESIAN_POINT('Ctrl Pts',(-7.43220229451985,1.16522285275759,
0.623315096548411));
#153395=CARTESIAN_POINT('Ctrl Pts',(-7.47375477370222,1.15903910504407,
0.626888809402448));
#153396=CARTESIAN_POINT('',(-7.37375621114219,1.06939091820832,-0.0609900343090774));
#153397=CARTESIAN_POINT('Origin',(-1.4658413372004E-13,1.16011713400011,
-1.77097648611929E-13));
#153398=CARTESIAN_POINT('',(-7.47429719740142,0.97936765915432,0.620388107456751));
#153399=CARTESIAN_POINT('Origin',(0.190745673161867,0.946436329317841,-0.0211491355141363));
#153400=CARTESIAN_POINT('',(-7.40550198016269,1.06939091992728,1.18681943978567));
#153401=CARTESIAN_POINT('Origin',(0.182998526930598,0.803756652297692,0.0128378233106978));
#153402=CARTESIAN_POINT('Origin',(0.181026394733831,0.946509328684528,-0.048916885303092));
#153403=CARTESIAN_POINT('Ctrl Pts',(-7.225117579,1.198733649,0.600146619));
#153404=CARTESIAN_POINT('Ctrl Pts',(-7.19242586500001,1.134619049,0.993719575));
#153405=CARTESIAN_POINT('Ctrl Pts',(-7.11717634000001,1.069390921,1.381412661));
#153406=CARTESIAN_POINT('Ctrl Pts',(-7.11642173978711,1.06873681508671,
1.38530043683952));
#153407=CARTESIAN_POINT('Ctrl Pts',(-7.11566713957423,1.06808270917341,
1.38918821267904));
#153408=CARTESIAN_POINT('Ctrl Pts',(-7.490599804,1.198733649,0.375385897));
#153409=CARTESIAN_POINT('Ctrl Pts',(-7.470151454,1.134619049,0.783420434));
#153410=CARTESIAN_POINT('Ctrl Pts',(-7.405501982,1.069390921,1.186819448));
#153411=CARTESIAN_POINT('Ctrl Pts',(-7.40485367883351,1.06873681508671,
1.1908647224631));
#153412=CARTESIAN_POINT('Ctrl Pts',(-7.40420537566703,1.06808270917341,
1.19490999692619));
#153413=CARTESIAN_POINT('',(-7.26133916437191,1.06939091791719,1.28411603543277));
#153414=CARTESIAN_POINT('Ctrl Pts',(-7.11867655828793,1.06811592995212,
1.37368338701899));
#153415=CARTESIAN_POINT('Ctrl Pts',(-7.11792644914396,1.06875342547606,
1.3775480240095));
#153416=CARTESIAN_POINT('Ctrl Pts',(-7.11717634,1.069390921,1.381412661));
#153417=CARTESIAN_POINT('Ctrl Pts',(-7.115977303,1.070409947,1.387590219));
#153418=CARTESIAN_POINT('Ctrl Pts',(-7.114767544,1.071428571,1.393765687));
#153419=CARTESIAN_POINT('Ctrl Pts',(-7.03985936,1.134501699,1.776150134));
#153420=CARTESIAN_POINT('Ctrl Pts',(-6.92439842400001,1.198754474,2.148303159));
#153421=CARTESIAN_POINT('Ctrl Pts',(-7.31358289534331,1.06811592995212,
1.66179769895285));
#153422=CARTESIAN_POINT('Ctrl Pts',(-7.31267622467166,1.06875342547606,
1.66576800047642));
#153423=CARTESIAN_POINT('Ctrl Pts',(-7.311769554,1.069390921,1.669738302));
#153424=CARTESIAN_POINT('Ctrl Pts',(-7.310320256,1.070409947,1.676084763));
#153425=CARTESIAN_POINT('Ctrl Pts',(-7.308859943,1.071428571,1.682428699));
#153426=CARTESIAN_POINT('Ctrl Pts',(-7.218437514,1.134501699,2.075244676));
#153427=CARTESIAN_POINT('Ctrl Pts',(-7.086433643,1.198754474,2.456106313));
#153428=CARTESIAN_POINT('',(-7.3117695495949,1.06939091911166,1.66973830899131));
#153429=CARTESIAN_POINT('',(-7.16425997754007,1.15903910587629,2.2188688494947));
#153430=CARTESIAN_POINT('Origin',(0.16433513636284,1.33838399167333,-0.0807409994602218));
#153431=CARTESIAN_POINT('Ctrl Pts',(-6.92580098057473,1.19797317334101,
2.14377722136203));
#153432=CARTESIAN_POINT('Ctrl Pts',(-6.9654525554008,1.19116562422871,2.15638583603037));
#153433=CARTESIAN_POINT('Ctrl Pts',(-7.0051737095645,1.18452215739093,2.16895121642368));
#153434=CARTESIAN_POINT('Ctrl Pts',(-7.08464747190185,1.17155461458958,
2.19397395012068));
#153435=CARTESIAN_POINT('Ctrl Pts',(-7.12444721430514,1.16522285272146,
2.20644613523128));
#153436=CARTESIAN_POINT('Ctrl Pts',(-7.16425997685052,1.15903910502031,
2.21886885127851));
#153437=CARTESIAN_POINT('',(-7.21447294344383,1.06939091820872,1.52557549831721));
#153438=CARTESIAN_POINT('Origin',(1.20303073058992E-12,1.16011713400017,
-3.39246859770714E-13));
#153439=CARTESIAN_POINT('',(-7.16618717794668,0.979367659170003,2.21263673771568));
#153440=CARTESIAN_POINT('Origin',(0.181740147034324,0.946436360213773,-0.0616594867204892));
#153441=CARTESIAN_POINT('',(-6.97723436100213,1.06939091992733,2.7510362805412));
#153442=CARTESIAN_POINT('Origin',(0.181479818422117,0.803756624957982,-0.0268015869709309));
#153443=CARTESIAN_POINT('Origin',(0.166278516225549,0.94650930964704,-0.0866886107508608));
#153444=CARTESIAN_POINT('Ctrl Pts',(-6.927184563,1.198733649,2.139302231));
#153445=CARTESIAN_POINT('Ctrl Pts',(-6.810650611,1.134619049,2.516645918));
#153446=CARTESIAN_POINT('Ctrl Pts',(-6.653817825,1.069390921,2.879098531));
#153447=CARTESIAN_POINT('Ctrl Pts',(-6.65224511003996,1.06873681508671,
2.88273319605511));
#153448=CARTESIAN_POINT('Ctrl Pts',(-6.65067239507993,1.06808270917341,
2.88636786111022));
#153449=CARTESIAN_POINT('Ctrl Pts',(-7.234776872,1.198733649,1.976867121));
#153450=CARTESIAN_POINT('Ctrl Pts',(-7.127091228,1.134619049,2.370966246));
#153451=CARTESIAN_POINT('Ctrl Pts',(-6.977234361,1.069390921,2.751036289));
#153452=CARTESIAN_POINT('Ctrl Pts',(-6.97573160036808,1.06873681508671,
2.75484762116934));
#153453=CARTESIAN_POINT('Ctrl Pts',(-6.97422883973616,1.06808270917341,
2.75865895333867));
#153454=CARTESIAN_POINT('',(-6.81552610039196,1.06939091791719,2.8150673921034));
#153455=CARTESIAN_POINT('Ctrl Pts',(-6.65694453501886,1.06811592995212,
2.87187246525374));
#153456=CARTESIAN_POINT('Ctrl Pts',(-6.65538118000943,1.06875342547606,
2.87548549812687));
#153457=CARTESIAN_POINT('Ctrl Pts',(-6.653817825,1.069390921,2.879098531));
#153458=CARTESIAN_POINT('Ctrl Pts',(-6.651318828,1.070409947,2.884873904));
#153459=CARTESIAN_POINT('Ctrl Pts',(-6.64880981,1.071428571,2.890644931));
#153460=CARTESIAN_POINT('Ctrl Pts',(-6.49345158400001,1.134501699,3.247986396));
#153461=CARTESIAN_POINT('Ctrl Pts',(-6.300688161,1.198754474,3.586618002));
#153462=CARTESIAN_POINT('Ctrl Pts',(-6.78535800869692,1.06811592995212,
3.19514992667576));
#153463=CARTESIAN_POINT('Ctrl Pts',(-6.78361903784846,1.06875342547606,
3.19883249733788));
#153464=CARTESIAN_POINT('Ctrl Pts',(-6.78188006700001,1.069390921,3.202515068));
#153465=CARTESIAN_POINT('Ctrl Pts',(-6.779100351,1.070409947,3.208401596));
#153466=CARTESIAN_POINT('Ctrl Pts',(-6.776310422,1.071428571,3.21428329));
#153467=CARTESIAN_POINT('Ctrl Pts',(-6.603558194,1.134501699,3.578477299));
#153468=CARTESIAN_POINT('Ctrl Pts',(-6.392766507,1.198754474,3.922057672));
#153469=CARTESIAN_POINT('',(-6.78188006127793,1.06939091911161,3.20251507397874));
#153470=CARTESIAN_POINT('',(-6.51977234700602,1.15903910587942,3.70709705022766));
#153471=CARTESIAN_POINT('Origin',(0.143136145802599,1.3383839765348,-0.11418051460323));
#153472=CARTESIAN_POINT('Ctrl Pts',(-6.30303086913351,1.19797317342552,
3.58249938691693));
#153473=CARTESIAN_POINT('Ctrl Pts',(-6.33904493282402,1.19116562428146,
3.60333713566231));
#153474=CARTESIAN_POINT('Ctrl Pts',(-6.37513624316441,1.18452215742029,
3.62414761846004));
#153475=CARTESIAN_POINT('Ctrl Pts',(-6.44737280500721,1.17155461459444,
3.66566984427696));
#153476=CARTESIAN_POINT('Ctrl Pts',(-6.48356090047984,1.16522285270483,
3.68640620487469));
#153477=CARTESIAN_POINT('Ctrl Pts',(-6.51977234593288,1.15903910501135,
3.70709705184634));
#153478=CARTESIAN_POINT('',(-6.71784893891174,1.06939091820871,3.0408068151596));
#153479=CARTESIAN_POINT('Origin',(4.87023615880489E-13,1.16011713399989,
-2.53703308361608E-13));
#153480=CARTESIAN_POINT('',(-6.5229942104888,0.979367659169073,3.70142493227494));
#153481=CARTESIAN_POINT('Origin',(0.16423608862457,0.946436316923738,-0.0992866306007983));
#153482=CARTESIAN_POINT('',(-6.22271901884537,1.06939091992734,4.18661772371598));
#153483=CARTESIAN_POINT('Origin',(0.171475441864284,0.803756611867204,-0.0651878064944689));
#153484=CARTESIAN_POINT('Origin',(0.143755515321106,0.946509288269899,-0.120406833011424));
#153485=CARTESIAN_POINT('Ctrl Pts',(-6.305344095,1.198733649,3.578426449));
#153486=CARTESIAN_POINT('Ctrl Pts',(-6.110416904,1.134619049,3.921896695));
#153487=CARTESIAN_POINT('Ctrl Pts',(-5.879334183,1.069390921,4.242160954));
#153488=CARTESIAN_POINT('Ctrl Pts',(-5.87701689168871,1.06873681508671,
4.24537255537584));
#153489=CARTESIAN_POINT('Ctrl Pts',(-5.87469960037743,1.06808270917341,
4.24858415675168));
#153490=CARTESIAN_POINT('Ctrl Pts',(-6.64066381400001,1.198733649,3.485912235));
#153491=CARTESIAN_POINT('Ctrl Pts',(-6.450776138,1.134619049,3.847648312));
#153492=CARTESIAN_POINT('Ctrl Pts',(-6.222719017,1.069390921,4.186617732));
#153493=CARTESIAN_POINT('Ctrl Pts',(-6.22043206632414,1.06873681508671,
4.19001690822728));
#153494=CARTESIAN_POINT('Ctrl Pts',(-6.21814511564828,1.06808270917341,
4.19341608445456));
#153495=CARTESIAN_POINT('',(-6.05102661106638,1.06939091791719,4.21438932711088));
#153496=CARTESIAN_POINT('Ctrl Pts',(-5.88394118241394,1.06811592995282,
4.23577597926674));
#153497=CARTESIAN_POINT('Ctrl Pts',(-5.88163768270697,1.06875342547641,
4.23896846663337));
#153498=CARTESIAN_POINT('Ctrl Pts',(-5.879334183,1.069390921,4.242160954));
#153499=CARTESIAN_POINT('Ctrl Pts',(-5.875652077,1.070409947,4.247264092));
#153500=CARTESIAN_POINT('Ctrl Pts',(-5.871961118,1.071428571,4.25236083));
#153501=CARTESIAN_POINT('Ctrl Pts',(-5.643417229,1.134501699,4.567950425));
#153502=CARTESIAN_POINT('Ctrl Pts',(-5.382364723,1.198754474,4.857226574));
#153503=CARTESIAN_POINT('Ctrl Pts',(-5.93985732264725,1.06811592995282,
4.57910049459051));
#153504=CARTESIAN_POINT('Ctrl Pts',(-5.93736736432363,1.06875342547641,
4.58232314179525));
#153505=CARTESIAN_POINT('Ctrl Pts',(-5.934877406,1.069390921,4.585545789));
#153506=CARTESIAN_POINT('Ctrl Pts',(-5.930897249,1.070409947,4.590697137));
#153507=CARTESIAN_POINT('Ctrl Pts',(-5.926908156,1.071428571,4.595841568));
#153508=CARTESIAN_POINT('Ctrl Pts',(-5.679903833,1.134501699,4.9143843));
#153509=CARTESIAN_POINT('Ctrl Pts',(-5.400180715,1.198754474,5.204617973));
#153510=CARTESIAN_POINT('',(-5.93487739907329,1.06939091911089,4.58554579351939));
#153511=CARTESIAN_POINT('',(-5.57042740808656,1.15903910589183,5.02198551255723));
#153512=CARTESIAN_POINT('Origin',(0.115244261096626,1.33838401607545,-0.142281081303194));
#153513=CARTESIAN_POINT('Ctrl Pts',(-5.38553804049224,1.19797317340481,
4.85370786275825));
#153514=CARTESIAN_POINT('Ctrl Pts',(-5.41623061527284,1.1911656242694,4.88180039563952));
#153515=CARTESIAN_POINT('Ctrl Pts',(-5.44700449210093,1.18452215741908,
4.90988290574779));
#153516=CARTESIAN_POINT('Ctrl Pts',(-5.50862615186155,1.17155461463078,
4.96596309029382));
#153517=CARTESIAN_POINT('Ctrl Pts',(-5.53951048516166,1.16522285274509,
4.99399401705785));
#153518=CARTESIAN_POINT('Ctrl Pts',(-5.57042740670401,1.15903910503806,
5.02198551389566));
#153519=CARTESIAN_POINT('',(-5.90710578420689,1.06939091820756,4.41385338527538));
#153520=CARTESIAN_POINT('Origin',(3.86843335142828E-13,1.16011713399978,
-3.00107161343988E-13));
#153521=CARTESIAN_POINT('',(-5.57479328396129,0.979367659167658,5.01713861087021));
#153522=CARTESIAN_POINT('Origin',(0.139052551745913,0.946436336407711,-0.132271185697479));
#153523=CARTESIAN_POINT('',(-5.17723625158196,1.06939091992736,5.42643757430719));
#153524=CARTESIAN_POINT('Origin',(0.153452966466637,0.803756635048499,-0.10052588202717));
#153525=CARTESIAN_POINT('Origin',(0.114510670055927,0.946509351282626,-0.14849495020988));
#153526=CARTESIAN_POINT('Ctrl Pts',(-5.388672745,1.198733649,4.850227423));
#153527=CARTESIAN_POINT('Ctrl Pts',(-5.124466893,1.134619049,5.143763941));
#153528=CARTESIAN_POINT('Ctrl Pts',(-4.829939409,1.069390921,5.40686464600001));
#153529=CARTESIAN_POINT('Ctrl Pts',(-4.82698589531168,1.06873681508671,
5.40950301279372));
#153530=CARTESIAN_POINT('Ctrl Pts',(-4.82403238162336,1.06808270917341,
5.41214137958745));
#153531=CARTESIAN_POINT('Ctrl Pts',(-5.736040696,1.198733649,4.831959968));
#153532=CARTESIAN_POINT('Ctrl Pts',(-5.472829926,1.134619049,5.144418618));
#153533=CARTESIAN_POINT('Ctrl Pts',(-5.17723624800001,1.069390921,5.426437582));
#153534=CARTESIAN_POINT('Ctrl Pts',(-5.17427204254692,1.06873681508671,
5.42926566058618));
#153535=CARTESIAN_POINT('Ctrl Pts',(-5.17130783709384,1.06808270917341,
5.43209373917236));
#153536=CARTESIAN_POINT('',(-5.00358784272335,1.06939091791719,5.4166511008613));
#153537=CARTESIAN_POINT('Ctrl Pts',(-4.83581127987199,1.06811592995214,
5.40161931776984));
#153538=CARTESIAN_POINT('Ctrl Pts',(-4.832875344436,1.06875342547607,5.40424198188491));
#153539=CARTESIAN_POINT('Ctrl Pts',(-4.829939409,1.069390921,5.406864646));
#153540=CARTESIAN_POINT('Ctrl Pts',(-4.82524636499999,1.070409947,5.411056931));
#153541=CARTESIAN_POINT('Ctrl Pts',(-4.82054605,1.071428571,5.415241063));
#153542=CARTESIAN_POINT('Ctrl Pts',(-4.529502956,1.134501699,5.674322168));
#153543=CARTESIAN_POINT('Ctrl Pts',(-4.212367892,1.198754474,5.90071663));
#153544=CARTESIAN_POINT('Ctrl Pts',(-4.81661550888194,1.06811592995214,
5.74893741316851));
#153545=CARTESIAN_POINT('Ctrl Pts',(-4.81349099094096,1.06875342547607,
5.75154944908425));
#153546=CARTESIAN_POINT('Ctrl Pts',(-4.810366473,1.069390921,5.754161485));
#153547=CARTESIAN_POINT('Ctrl Pts',(-4.805371983,1.070409947,5.758336781));
#153548=CARTESIAN_POINT('Ctrl Pts',(-4.800370252,1.071428571,5.762503401));
#153549=CARTESIAN_POINT('Ctrl Pts',(-4.490663482,1.134501699,6.020500154));
#153550=CARTESIAN_POINT('Ctrl Pts',(-4.155088474,1.198754474,6.243816123));
#153551=CARTESIAN_POINT('',(-4.81036646532958,1.06939091911155,5.75416148814387));
#153552=CARTESIAN_POINT('',(-4.36061547464227,1.1590391058868,6.10205151390795));
#153553=CARTESIAN_POINT('Origin',(0.0819636971075782,1.33838395772576,-0.163728735462429));
#153554=CARTESIAN_POINT('Ctrl Pts',(-4.21622343834094,1.19797317332506,
5.89796235369778));
#153555=CARTESIAN_POINT('Ctrl Pts',(-4.24015925230638,1.19116565867653,
5.93199592258888));
#153556=CARTESIAN_POINT('Ctrl Pts',(-4.26417660734966,1.18452222668692,
5.96603716173334));
#153557=CARTESIAN_POINT('Ctrl Pts',(-4.3123022622184,1.17155461461324,6.03405342148723));
#153558=CARTESIAN_POINT('Ctrl Pts',(-4.33643871619161,1.16522285278025,
6.06806821925712));
#153559=CARTESIAN_POINT('Ctrl Pts',(-4.36061547307682,1.15903910505355,
6.10205151487003));
#153560=CARTESIAN_POINT('',(-4.82015292799143,1.06939091820868,5.58051307673611));
#153561=CARTESIAN_POINT('Origin',(-3.27429056090622E-13,1.16011713400039,
3.59521440396193E-13));
#153562=CARTESIAN_POINT('',(-4.36592121873627,0.979367659175133,6.09825646507156));
#153563=CARTESIAN_POINT('Origin',(0.10736725186915,0.946436344476906,-0.159071021017346));
#153564=CARTESIAN_POINT('',(-3.88967167115354,1.06939091992738,6.41252323525665));
#153565=CARTESIAN_POINT('Origin',(0.128255209084623,0.803756677600229,-0.131163488073143));
#153566=CARTESIAN_POINT('Origin',(0.0799114619989633,0.946509291999864,
-0.169639663453076));
#153567=CARTESIAN_POINT('Ctrl Pts',(-4.220033046,1.198733649,5.895237153));
#153568=CARTESIAN_POINT('Ctrl Pts',(-3.898902506,1.134619049,6.125114502));
#153569=CARTESIAN_POINT('Ctrl Pts',(-3.554702037,1.069390921,6.318749356));
#153570=CARTESIAN_POINT('Ctrl Pts',(-3.55125040395404,1.06873681508671,
6.32069112110816));
#153571=CARTESIAN_POINT('Ctrl Pts',(-3.54779877090807,1.06808270917341,
6.32263288621632));
#153572=CARTESIAN_POINT('Ctrl Pts',(-4.563206691,1.198733649,5.95207062200001));
#153573=CARTESIAN_POINT('Ctrl Pts',(-4.238980268,1.134619049,6.200641628));
#153574=CARTESIAN_POINT('Ctrl Pts',(-3.889671666,1.069390921,6.41252324200001));
#153575=CARTESIAN_POINT('Ctrl Pts',(-3.88616880873369,1.06873681508671,
6.4146479851267));
#153576=CARTESIAN_POINT('Ctrl Pts',(-3.88266595146739,1.06808270917341,
6.4167727282534));
#153577=CARTESIAN_POINT('',(-3.72218686821525,1.06939091791719,6.36563628922607));
#153578=CARTESIAN_POINT('Ctrl Pts',(-3.56156421782437,1.06811592995212,
6.31488893800863));
#153579=CARTESIAN_POINT('Ctrl Pts',(-3.55813312741219,1.06875342547606,
6.31681914700431));
#153580=CARTESIAN_POINT('Ctrl Pts',(-3.554702037,1.069390921,6.318749356));
#153581=CARTESIAN_POINT('Ctrl Pts',(-3.549217496,1.070409947,6.321834763));
#153582=CARTESIAN_POINT('Ctrl Pts',(-3.543727607,1.071428571,6.324910643));
#153583=CARTESIAN_POINT('Ctrl Pts',(-3.20379416,1.134501699,6.515368914));
#153584=CARTESIAN_POINT('Ctrl Pts',(-2.84540542,1.198754474,6.668295734));
#153585=CARTESIAN_POINT('Ctrl Pts',(-3.46815410914429,1.06811592995212,
6.64996040604056));
#153586=CARTESIAN_POINT('Ctrl Pts',(-3.46454113007215,1.06875342547606,
6.65183969552028));
#153587=CARTESIAN_POINT('Ctrl Pts',(-3.460928151,1.069390921,6.65371898500001));
#153588=CARTESIAN_POINT('Ctrl Pts',(-3.455152864,1.070409947,6.656722998));
#153589=CARTESIAN_POINT('Ctrl Pts',(-3.44937237,1.071428571,6.65971698));
#153590=CARTESIAN_POINT('Ctrl Pts',(-3.091444697,1.134501699,6.845104111));
#153591=CARTESIAN_POINT('Ctrl Pts',(-2.715708914,1.198754474,6.99106037));
#153592=CARTESIAN_POINT('',(-3.46092814283713,1.06939091911156,6.65371898649407));
#153593=CARTESIAN_POINT('',(-2.94690600790438,1.15903910589172,6.89679236883628));
#153594=CARTESIAN_POINT('Origin',(0.0448505823939493,1.33838402075146,-0.177520621225209));
#153595=CARTESIAN_POINT('Ctrl Pts',(-2.84976291363965,1.19797317337202,
6.6664346795221));
#153596=CARTESIAN_POINT('Ctrl Pts',(-2.8658229917059,1.19116562423472,6.70481824954385));
#153597=CARTESIAN_POINT('Ctrl Pts',(-2.88196106597728,1.18452215738225,
6.74322686101663));
#153598=CARTESIAN_POINT('Ctrl Pts',(-2.91433991138458,1.17155461462031,
6.81999812139951));
#153599=CARTESIAN_POINT('Ctrl Pts',(-2.93059989247976,1.16522285275017,
6.85840629648366));
#153600=CARTESIAN_POINT('Ctrl Pts',(-2.94690600609201,1.15903910504532,
6.89679236946981));
#153601=CARTESIAN_POINT('',(-3.50781507888034,1.06939091820872,6.48623417867685));
#153602=CARTESIAN_POINT('Origin',(8.12934788929631E-13,1.16011713400022,
-1.6531914726059E-12));
#153603=CARTESIAN_POINT('',(-2.95290353040653,0.979367659136253,6.89422662374214));
#153604=CARTESIAN_POINT('Origin',(0.070661430224247,0.946436330066777,-0.17843267214666));
#153605=CARTESIAN_POINT('',(-2.42023036541204,1.06939091992729,7.09876643752802));
#153606=CARTESIAN_POINT('Origin',(0.0970604625441626,0.803756636778403,
-0.155668159303939));
#153607=CARTESIAN_POINT('Origin',(0.0415756801104716,0.946509325067864,
-0.182852213635061));
#153608=CARTESIAN_POINT('Ctrl Pts',(-2.854069293,1.198733649,6.664592146));
#153609=CARTESIAN_POINT('Ctrl Pts',(-2.491029771,1.134619049,6.820061517));
#153610=CARTESIAN_POINT('Ctrl Pts',(-2.113250748,1.069390921,6.93517637));
#153611=CARTESIAN_POINT('Ctrl Pts',(-2.10946239011761,1.06873681508671,
6.93633073864991));
#153612=CARTESIAN_POINT('Ctrl Pts',(-2.10567403223522,1.06808270917341,
6.93748510729981));
#153613=CARTESIAN_POINT('Ctrl Pts',(-3.177002213,1.198733649,6.79386907));
#153614=CARTESIAN_POINT('Ctrl Pts',(-2.806920605,1.134619049,6.966929527));
#153615=CARTESIAN_POINT('Ctrl Pts',(-2.420230359,1.069390921,7.098766443));
#153616=CARTESIAN_POINT('Ctrl Pts',(-2.41635263961303,1.06873681508671,
7.10008850004794));
#153617=CARTESIAN_POINT('Ctrl Pts',(-2.41247492022606,1.06808270917341,
7.10141055709586));
#153618=CARTESIAN_POINT('',(-2.26674057192556,1.06939091791719,7.01697140054787));
#153619=CARTESIAN_POINT('Ctrl Pts',(-2.12078237087665,1.06811592995269,
6.93288137335275));
#153620=CARTESIAN_POINT('Ctrl Pts',(-2.11701655943833,1.06875342547634,
6.93402887167638));
#153621=CARTESIAN_POINT('Ctrl Pts',(-2.113250748,1.069390921,6.93517637));
#153622=CARTESIAN_POINT('Ctrl Pts',(-2.107231161,1.070409947,6.937010627));
#153623=CARTESIAN_POINT('Ctrl Pts',(-2.1012084,1.071428571,6.938834431));
#153624=CARTESIAN_POINT('Ctrl Pts',(-1.728279509,1.134501699,7.05176425));
#153625=CARTESIAN_POINT('Ctrl Pts',(-1.345394953,1.198754474,7.124072741));
#153626=CARTESIAN_POINT('Ctrl Pts',(-1.95752567888414,1.06811592995269,
7.24003864400401));
#153627=CARTESIAN_POINT('Ctrl Pts',(-1.95359317694207,1.06875342547634,
7.241097312502));
#153628=CARTESIAN_POINT('Ctrl Pts',(-1.949660675,1.069390921,7.24215598100001));
#153629=CARTESIAN_POINT('Ctrl Pts',(-1.943374636,1.070409947,7.243848245));
#153630=CARTESIAN_POINT('Ctrl Pts',(-1.93708567,1.071428571,7.245529595));
#153631=CARTESIAN_POINT('Ctrl Pts',(-1.547673393,1.134501699,7.349638609));
#153632=CARTESIAN_POINT('Ctrl Pts',(-1.149345823,1.198754474,7.411410404));
#153633=CARTESIAN_POINT('',(-1.94966066671809,1.06939091911095,7.24215598060968));
#153634=CARTESIAN_POINT('',(-1.39540249131301,1.15903910584932,7.36904687769396));
#153635=CARTESIAN_POINT('Origin',(0.0056402997146246,1.33838410971113,-0.183011834889248));
#153636=CARTESIAN_POINT('Ctrl Pts',(-1.35005064267087,1.19797317333044,
7.12319192941442));
#153637=CARTESIAN_POINT('Ctrl Pts',(-1.35748387767238,1.19116565562259,
7.16413036591661));
#153638=CARTESIAN_POINT('Ctrl Pts',(-1.36498789721534,1.18452222053175,
7.20511000403772));
#153639=CARTESIAN_POINT('Ctrl Pts',(-1.38010626517507,1.17155461459164,
7.28704728882415));
#153640=CARTESIAN_POINT('Ctrl Pts',(-1.38772947465277,1.16522285271402,
7.3280529174482));
#153641=CARTESIAN_POINT('Ctrl Pts',(-1.39540248941714,1.1590391049902,7.36904687791923));
#153642=CARTESIAN_POINT('',(-2.03145569497042,1.06939091820777,7.08866618023702));
#153643=CARTESIAN_POINT('Origin',(-3.19080699362484E-13,1.16011713400028,
1.66403349433075E-12));
#153644=CARTESIAN_POINT('',(-1.40181135465005,0.979367659141008,7.36783040844139));
#153645=CARTESIAN_POINT('Origin',(0.0306516470017276,0.946436331022197,
-0.189451099218505));
#153646=CARTESIAN_POINT('',(-0.837621778443209,1.06939091992729,7.45307921003506));
#153647=CARTESIAN_POINT('Origin',(0.061327216830241,0.80375661447446,-0.172894016761331));
#153648=CARTESIAN_POINT('Origin',(0.00129586030556517,0.946509335692072,
-0.187514887539498));
#153649=CARTESIAN_POINT('Ctrl Pts',(-1.354652431,1.198733649,7.122318217));
#153650=CARTESIAN_POINT('Ctrl Pts',(-0.966679253,1.134619049,7.196110035));
#153651=CARTESIAN_POINT('Ctrl Pts',(-0.572986203,1.069390921,7.227322244));
#153652=CARTESIAN_POINT('Ctrl Pts',(-0.569038259682857,1.06873681508671,
7.22763523919241));
#153653=CARTESIAN_POINT('Ctrl Pts',(-0.565090316365714,1.06808270917341,
7.22794823438482));
#153654=CARTESIAN_POINT('Ctrl Pts',(-1.642244642,1.198733649,7.317993751));
#153655=CARTESIAN_POINT('Ctrl Pts',(-1.243612454,1.134619049,7.407451544));
#153656=CARTESIAN_POINT('Ctrl Pts',(-0.837621771000001,1.069390921,7.453079214));
#153657=CARTESIAN_POINT('Ctrl Pts',(-0.833550507349874,1.06873681508671,
7.45353676704762));
#153658=CARTESIAN_POINT('Ctrl Pts',(-0.829479243699748,1.06808270917341,
7.45399432009523));
#153659=CARTESIAN_POINT('',(-0.705304006274312,1.06939091791719,7.34020072714797));
#153660=CARTESIAN_POINT('Origin',(1.09775469964157E-14,1.16011713400033,
-2.83193607453214E-13));
#153661=CARTESIAN_POINT('',(0.214827962323003,0.979367659150024,7.49692263181167));
#153662=CARTESIAN_POINT('',(-0.347229223939931,1.06939091911043,7.49195780996947));
#153663=CARTESIAN_POINT('Origin',(-0.010791358648808,0.94643631321699,-0.19161089903692));
#153664=CARTESIAN_POINT('Origin',(0.0227263342227098,0.803756637030686,
-0.182035181962791));
#153665=CARTESIAN_POINT('Origin',(-0.0338336897090269,1.33838403136748,
-0.179945622470713));
#153666=CARTESIAN_POINT('Ctrl Pts',(-0.580835096610768,1.06811592995312,
7.22669998041471));
#153667=CARTESIAN_POINT('Ctrl Pts',(-0.576910649805384,1.06875342547656,
7.22701111220736));
#153668=CARTESIAN_POINT('Ctrl Pts',(-0.572986203,1.069390921,7.227322244));
#153669=CARTESIAN_POINT('Ctrl Pts',(-0.56671304,1.070409947,7.227819583));
#153670=CARTESIAN_POINT('Ctrl Pts',(-0.560439023,1.071428571,7.228306033));
#153671=CARTESIAN_POINT('Ctrl Pts',(-0.17195243,1.134501699,7.258426928));
#153672=CARTESIAN_POINT('Ctrl Pts',(0.217524687,1.198754474,7.246736025));
#153673=CARTESIAN_POINT('Ctrl Pts',(-0.355365520528548,1.06811592995312,
7.49158071955915));
#153674=CARTESIAN_POINT('Ctrl Pts',(-0.351297376264274,1.06875342547656,
7.49176926577957));
#153675=CARTESIAN_POINT('Ctrl Pts',(-0.347229232,1.069390921,7.49195781200001));
#153676=CARTESIAN_POINT('Ctrl Pts',(-0.340726371,1.070409947,7.4922592));
#153677=CARTESIAN_POINT('Ctrl Pts',(-0.334222997,1.071428571,7.492549298));
#153678=CARTESIAN_POINT('Ctrl Pts',(0.068465398,1.134501699,7.510512173));
#153679=CARTESIAN_POINT('Ctrl Pts',(0.470759401,1.198754474,7.485211125));
#153680=CARTESIAN_POINT('',(-0.460107700334207,1.06939091820706,7.35964002907317));
#153681=CARTESIAN_POINT('Ctrl Pts',(-1.14050351955613,4.81939092100001,
7.43209880004169));
#153682=CARTESIAN_POINT('Ctrl Pts',(-0.737770323522325,4.754503495,7.49390080806282));
#153683=CARTESIAN_POINT('Ctrl Pts',(-0.330717067503511,4.689276009,7.51182182120226));
#153684=CARTESIAN_POINT('Ctrl Pts',(-1.155216884,4.81939092100001,7.410497551));
#153685=CARTESIAN_POINT('Ctrl Pts',(-0.753654224,4.754503495,7.473096852));
#153686=CARTESIAN_POINT('Ctrl Pts',(-0.347678495,4.689276009,7.491936977));
#153687=CARTESIAN_POINT('Ctrl Pts',(-1.35103832,4.81939092100001,7.123004665));
#153688=CARTESIAN_POINT('Ctrl Pts',(-0.965054425,4.754503495,7.196215207));
#153689=CARTESIAN_POINT('Ctrl Pts',(-0.573419596,4.689276009,7.227287871));
#153690=CARTESIAN_POINT('',(-0.598342121129821,4.73201976879592,7.49397863771111));
#153691=CARTESIAN_POINT('Ctrl Pts',(-0.59831258994097,4.73200270359627,
7.49384481755901));
#153692=CARTESIAN_POINT('Ctrl Pts',(-0.59482195673254,4.72506033663315,
7.44720105427947));
#153693=CARTESIAN_POINT('Ctrl Pts',(-0.59130988361317,4.71792582707077,
7.40055371361005));
#153694=CARTESIAN_POINT('Ctrl Pts',(-0.584568150926036,4.70392125170665,
7.31160013884204));
#153695=CARTESIAN_POINT('Ctrl Pts',(-0.581337570868995,4.69707707070605,
7.26922871111862));
#153696=CARTESIAN_POINT('Ctrl Pts',(-0.578090315740495,4.69005394718278,
7.22691577275115));
#153697=CARTESIAN_POINT('',(-1.2089559129046,4.8193909197054,7.33160125315675));
#153698=CARTESIAN_POINT('Ctrl Pts',(-0.598394674877038,4.73205099219874,
7.49409641631189));
#153699=CARTESIAN_POINT('Ctrl Pts',(-0.701560839128794,4.74662633022798,
7.47123699178965));
#153700=CARTESIAN_POINT('Ctrl Pts',(-0.804232364139554,4.76121922702359,
7.44620705502926));
#153701=CARTESIAN_POINT('Ctrl Pts',(-1.00781309835978,4.79033919834542,
7.39200028864064));
#153702=CARTESIAN_POINT('Ctrl Pts',(-1.10870789696985,4.80486306066967,
7.36285585215043));
#153703=CARTESIAN_POINT('Ctrl Pts',(-1.20895590732316,4.81939092104741,
7.33160125063828));
#153704=CARTESIAN_POINT('',(-1.27957088547711,4.81939091791758,7.22792874414045));
#153705=CARTESIAN_POINT('Ctrl Pts',(-2.4530261316489,4.689268254,7.10774157717197));
#153706=CARTESIAN_POINT('Ctrl Pts',(-2.06279664085677,4.754934719,7.24241770931939));
#153707=CARTESIAN_POINT('Ctrl Pts',(-1.66016901775353,4.819390921,7.33356436923981));
#153708=CARTESIAN_POINT('Ctrl Pts',(-2.429904911,4.689268254,7.09546067));
#153709=CARTESIAN_POINT('Ctrl Pts',(-2.040349667,4.754934719,7.2288674));
#153710=CARTESIAN_POINT('Ctrl Pts',(-1.638531205,4.819390921,7.3188261));
#153711=CARTESIAN_POINT('Ctrl Pts',(-2.122702584,4.689268254,6.932289213));
#153712=CARTESIAN_POINT('Ctrl Pts',(-1.742105785,4.754934719,7.04882990900001));
#153713=CARTESIAN_POINT('Ctrl Pts',(-1.35103832,4.819390921,7.123004665));
#153714=CARTESIAN_POINT('',(-1.55963490183381,4.81939091971443,7.26508708152735));
#153715=CARTESIAN_POINT('',(-1.45491314490615,4.81939091820872,7.19375744735644));
#153716=CARTESIAN_POINT('',(-2.19533721229327,4.7320198238682,7.19014807039892));
#153717=CARTESIAN_POINT('Ctrl Pts',(-1.55963490663822,4.81939092085753,
7.26508707759447));
#153718=CARTESIAN_POINT('Ctrl Pts',(-1.66575655822878,4.80491309558304,
7.25711305448626));
#153719=CARTESIAN_POINT('Ctrl Pts',(-1.77169575683013,4.79041128761736,
7.24690770166126));
#153720=CARTESIAN_POINT('Ctrl Pts',(-1.9836880211467,4.76128647698349,7.22198419719515));
#153721=CARTESIAN_POINT('Ctrl Pts',(-2.08971531443295,4.74666639459473,
7.20724269142357));
#153722=CARTESIAN_POINT('Ctrl Pts',(-2.19539471642952,4.73203683304299,
7.19027205457454));
#153723=CARTESIAN_POINT('Ctrl Pts',(-2.1181481514051,4.6900539473732,6.93368216908028));
#153724=CARTESIAN_POINT('Ctrl Pts',(-2.13041551437734,4.69707706864944,
6.97430777773428));
#153725=CARTESIAN_POINT('Ctrl Pts',(-2.14267916587992,4.70392124758685,
7.0149940936479));
#153726=CARTESIAN_POINT('Ctrl Pts',(-2.1683857367939,4.71792585997149,7.10041893384059));
#153727=CARTESIAN_POINT('Ctrl Pts',(-2.18184357645508,4.72506040970981,
7.14522095253068));
#153728=CARTESIAN_POINT('Ctrl Pts',(-2.19527970815702,4.7320028146934,7.1900240862233));
#153729=CARTESIAN_POINT('Origin',(3.04010289164935E-13,4.93907429999964,
-7.64145691167784E-13));
#153730=CARTESIAN_POINT('',(-2.12995512140554,4.93794662027152,6.99495645510371));
#153731=CARTESIAN_POINT('Ctrl Pts',(-2.12995512205003,4.93794661929206,
6.99495645593132));
#153732=CARTESIAN_POINT('Ctrl Pts',(-2.03687773364896,4.91814186452076,
7.04400094768946));
#153733=CARTESIAN_POINT('Ctrl Pts',(-1.94277951412653,4.89834552796937,
7.09105849203187));
#153734=CARTESIAN_POINT('Ctrl Pts',(-1.80030894915214,4.86872423033274,
7.15854536088304));
#153735=CARTESIAN_POINT('Ctrl Pts',(-1.75268628190587,4.85888055797279,
7.1804867625023));
#153736=CARTESIAN_POINT('Ctrl Pts',(-1.65233933152185,4.83826147072025,
7.22542971669909));
#153737=CARTESIAN_POINT('Ctrl Pts',(-1.60370556157199,4.82833849617245,
7.24647476580251));
#153738=CARTESIAN_POINT('Ctrl Pts',(-1.55963490097094,4.81939092004434,
7.26508707964281));
#153739=CARTESIAN_POINT('',(-2.75676874468984,4.81939091962397,6.90030270497095));
#153740=CARTESIAN_POINT('Ctrl Pts',(-2.75676874432946,4.8193909198592,6.90030270293695));
#153741=CARTESIAN_POINT('Ctrl Pts',(-2.70856221741575,4.82837891575066,
6.90988314681471));
#153742=CARTESIAN_POINT('Ctrl Pts',(-2.65658740037599,4.83808521854872,
6.91969511781252));
#153743=CARTESIAN_POINT('Ctrl Pts',(-2.54838669927649,4.85839508142698,
6.9386041878068));
#153744=CARTESIAN_POINT('Ctrl Pts',(-2.49640727554015,4.86818863447598,
6.94706881560552));
#153745=CARTESIAN_POINT('Ctrl Pts',(-2.33982942837266,4.89780165988493,
6.97071017729041));
#153746=CARTESIAN_POINT('Ctrl Pts',(-2.23501398669613,4.91777478488708,
6.9840524371011));
#153747=CARTESIAN_POINT('Ctrl Pts',(-2.12995512148023,4.93794662119409,
6.99495645411656));
#153748=CARTESIAN_POINT('Ctrl Pts',(-2.19541375170991,4.7320509931869,7.19025143703924));
#153749=CARTESIAN_POINT('Ctrl Pts',(-2.29125384788963,4.74662633122123,
7.14574877728955));
#153750=CARTESIAN_POINT('Ctrl Pts',(-2.38614427324306,4.76121922802501,
7.09923268348006));
#153751=CARTESIAN_POINT('Ctrl Pts',(-2.57331254432414,4.79033919837692,
7.00252940413573));
#153752=CARTESIAN_POINT('Ctrl Pts',(-2.66558328619014,4.80486306068117,
6.95237694925337));
#153753=CARTESIAN_POINT('Ctrl Pts',(-2.75676873810498,4.81939092102955,
6.90030270416342));
#153754=CARTESIAN_POINT('Ctrl Pts',(-2.7115207327671,4.819390921,7.01316591404527));
#153755=CARTESIAN_POINT('Ctrl Pts',(-2.33148881985781,4.754503495,7.16009875803589));
#153756=CARTESIAN_POINT('Ctrl Pts',(-1.93780473105558,4.689276009,7.2651052049765));
#153757=CARTESIAN_POINT('Ctrl Pts',(-2.721246476,4.819390921,6.988906754));
#153758=CARTESIAN_POINT('Ctrl Pts',(-2.342529127,4.754503495,7.13636662));
#153759=CARTESIAN_POINT('Ctrl Pts',(-1.950094955,4.689276009,7.242039054));
#153760=CARTESIAN_POINT('Ctrl Pts',(-2.850687243,4.819390921,6.666039472));
#153761=CARTESIAN_POINT('Ctrl Pts',(-2.48946554,4.754503495,6.82051352));
#153762=CARTESIAN_POINT('Ctrl Pts',(-2.11366662,4.689276009,6.93504963400001));
#153763=CARTESIAN_POINT('',(-2.80344625281137,4.81939091791756,6.78387387063942));
#153764=CARTESIAN_POINT('Ctrl Pts',(-3.92363007934769,4.689268254,6.41423842243658));
#153765=CARTESIAN_POINT('Ctrl Pts',(-3.57147532391773,4.754934719,6.62965370569363));
#153766=CARTESIAN_POINT('Ctrl Pts',(-3.19785474998995,4.819390921,6.80522244558559));
#153767=CARTESIAN_POINT('Ctrl Pts',(-3.898409388,4.689268254,6.407215015));
#153768=CARTESIAN_POINT('Ctrl Pts',(-3.546640232,4.754934719,6.621245631));
#153769=CARTESIAN_POINT('Ctrl Pts',(-3.173554525,4.819390921,6.79548023900001));
#153770=CARTESIAN_POINT('Ctrl Pts',(-3.563312241,4.689268254,6.313897835));
#153771=CARTESIAN_POINT('Ctrl Pts',(-3.216666389,4.754934719,6.509530936));
#153772=CARTESIAN_POINT('Ctrl Pts',(-2.850687243,4.819390921,6.666039472));
#153773=CARTESIAN_POINT('',(-3.08495047229094,4.81939091970353,6.75995798154528));
#153774=CARTESIAN_POINT('',(-2.96734328929225,4.81939091820873,6.71280807683697));
#153775=CARTESIAN_POINT('',(-3.6896807437116,4.73201982384953,6.55011379745764));
#153776=CARTESIAN_POINT('Ctrl Pts',(-3.08495047608777,4.81939092086118,
6.75995797672338));
#153777=CARTESIAN_POINT('Ctrl Pts',(-3.18687688266884,4.80491309566292,
6.72935736384145));
#153778=CARTESIAN_POINT('Ctrl Pts',(-3.28814543198366,4.79041128777397,
6.69661681053702));
#153779=CARTESIAN_POINT('Ctrl Pts',(-3.48982361922147,4.76128647699335,
6.62670393305435));
#153780=CARTESIAN_POINT('Ctrl Pts',(-3.59020306534355,4.7466663945943,6.58951434159313));
#153781=CARTESIAN_POINT('Ctrl Pts',(-3.68976355640026,4.73203683302006,
6.55022252125281));
#153782=CARTESIAN_POINT('Ctrl Pts',(-3.55916373230487,4.69005394749471,
6.31623729329977));
#153783=CARTESIAN_POINT('Ctrl Pts',(-3.57987759641344,4.69707706879228,
6.35327597766147));
#153784=CARTESIAN_POINT('Ctrl Pts',(-3.60060088539638,4.70392124755126,
6.39037474666884));
#153785=CARTESIAN_POINT('Ctrl Pts',(-3.64407026673631,4.7179258599679,6.46827624894677));
#153786=CARTESIAN_POINT('Ctrl Pts',(-3.66684457924855,4.72506040969475,
6.50913778352832));
#153787=CARTESIAN_POINT('Ctrl Pts',(-3.68959793102294,4.732002814679,6.55000507366246));
#153788=CARTESIAN_POINT('Origin',(-3.79904441238921E-13,4.93907429999982,
6.90853624307763E-13));
#153789=CARTESIAN_POINT('',(-3.58386682213069,4.937946620308,6.3735408705598));
#153790=CARTESIAN_POINT('Ctrl Pts',(-3.58386682305503,4.93794661918659,
6.37354087132658));
#153791=CARTESIAN_POINT('Ctrl Pts',(-3.5035086482658,4.9181418644276,6.44144761724973));
#153792=CARTESIAN_POINT('Ctrl Pts',(-3.42172637389743,4.8983455278665,6.50763331800492));
#153793=CARTESIAN_POINT('Ctrl Pts',(-3.29709437357307,4.86872423024352,
6.60416934135374));
#153794=CARTESIAN_POINT('Ctrl Pts',(-3.25530185067192,4.85888055790257,
6.63583523087271));
#153795=CARTESIAN_POINT('Ctrl Pts',(-3.16696236313074,4.83826147072462,
6.70129907166331));
#153796=CARTESIAN_POINT('Ctrl Pts',(-3.1239896871397,4.82833849618614,6.73230692215565));
#153797=CARTESIAN_POINT('Ctrl Pts',(-3.08495047108381,4.81939092001171,
6.75995797994071));
#153798=CARTESIAN_POINT('',(-4.17567813333125,4.81939091958503,6.14635367162492));
#153799=CARTESIAN_POINT('Ctrl Pts',(-4.1756781326346,4.8193909197402,6.14635366996372));
#153800=CARTESIAN_POINT('Ctrl Pts',(-4.13065827124356,4.82837889487366,
6.16607305606045));
#153801=CARTESIAN_POINT('Ctrl Pts',(-4.08200792740075,4.83808518697421,
6.18682866311168));
#153802=CARTESIAN_POINT('Ctrl Pts',(-3.98040163242939,4.8583950812381,6.22855566656678));
#153803=CARTESIAN_POINT('Ctrl Pts',(-3.93145710281929,4.86818863440753,
6.24799643597097));
#153804=CARTESIAN_POINT('Ctrl Pts',(-3.7836221517757,4.89780165995966,6.30474468485385));
#153805=CARTESIAN_POINT('Ctrl Pts',(-3.68412542814874,4.91777478500429,
6.34030723174283));
#153806=CARTESIAN_POINT('Ctrl Pts',(-3.58386682196884,4.93794662138014,
6.3735408694208));
#153807=CARTESIAN_POINT('Ctrl Pts',(-3.68977771447632,4.73205099318326,
6.5501982937046));
#153808=CARTESIAN_POINT('Ctrl Pts',(-3.77381036623843,4.74662633125715,
6.48613329363275));
#153809=CARTESIAN_POINT('Ctrl Pts',(-3.85648272115148,4.76121922808381,
6.42030608363322));
#153810=CARTESIAN_POINT('Ctrl Pts',(-4.01848676156039,4.79033919950061,
6.2856280226034));
#153811=CARTESIAN_POINT('Ctrl Pts',(-4.09781896633792,4.80486306124649,
6.21681262465362));
#153812=CARTESIAN_POINT('Ctrl Pts',(-4.17567812688072,4.81939092105904,
6.14635367227836));
#153813=CARTESIAN_POINT('Ctrl Pts',(-4.15575024852906,4.819390921,6.26630518683826));
#153814=CARTESIAN_POINT('Ctrl Pts',(-3.81618948817902,4.754503495,6.49149844966127));
#153815=CARTESIAN_POINT('Ctrl Pts',(-3.45428279729009,4.689276009,6.67868034729526));
#153816=CARTESIAN_POINT('Ctrl Pts',(-4.160033607,4.819390921,6.240522445));
#153817=CARTESIAN_POINT('Ctrl Pts',(-3.821869971,4.754503495,6.465947816));
#153818=CARTESIAN_POINT('Ctrl Pts',(-3.461327142,4.689276009,6.65351143500001));
#153819=CARTESIAN_POINT('Ctrl Pts',(-4.217041199,4.819390921,5.897377682));
#153820=CARTESIAN_POINT('Ctrl Pts',(-3.897472013,4.754503495,6.125892201));
#153821=CARTESIAN_POINT('Ctrl Pts',(-3.555080941,4.689276009,6.31853618300001));
#153822=CARTESIAN_POINT('',(-4.19623558931448,4.8193909179172,6.02261259398131));
#153823=CARTESIAN_POINT('Ctrl Pts',(-5.21076944541101,4.689268254,5.42081260694443));
#153824=CARTESIAN_POINT('Ctrl Pts',(-4.91315579169461,4.754934719,5.70689446397799));
#153825=CARTESIAN_POINT('Ctrl Pts',(-4.5860123475086,4.819390921,5.95867588311505));
#153826=CARTESIAN_POINT('Ctrl Pts',(-5.184628575,4.689268254,5.419375106));
#153827=CARTESIAN_POINT('Ctrl Pts',(-4.88709384300001,4.754934719,5.704021776));
#153828=CARTESIAN_POINT('Ctrl Pts',(-4.56018596200001,4.819390921,5.954385274));
#153829=CARTESIAN_POINT('Ctrl Pts',(-4.837305378,4.689268254,5.400275611));
#153830=CARTESIAN_POINT('Ctrl Pts',(-4.540819247,4.754934719,5.66585353));
#153831=CARTESIAN_POINT('Ctrl Pts',(-4.217041199,4.819390921,5.897377682));
#153832=CARTESIAN_POINT('',(-4.4660171875858,4.81939091972219,5.93874075956449));
#153833=CARTESIAN_POINT('',(-4.34102375947002,4.81939091820872,5.91797526136406));
#153834=CARTESIAN_POINT('',(-5.01149890497033,4.73201982381453,5.60380348299995));
#153835=CARTESIAN_POINT('Ctrl Pts',(-4.46601719029875,4.81939092087189,
5.93874075396268));
#153836=CARTESIAN_POINT('Ctrl Pts',(-4.55898238578439,4.80491309584948,
5.8869444025433));
#153837=CARTESIAN_POINT('Ctrl Pts',(-4.6508450803644,4.7904112881491,5.83319956134153));
#153838=CARTESIAN_POINT('Ctrl Pts',(-4.83277894394465,4.76128647699006,
5.72156635797227));
#153839=CARTESIAN_POINT('Ctrl Pts',(-4.9228169116799,4.74666639456854,5.66366762468992));
#153840=CARTESIAN_POINT('Ctrl Pts',(-5.01160315398706,4.73203683297963,
5.60389186259176));
#153841=CARTESIAN_POINT('Ctrl Pts',(-4.83375677298044,4.69005394733486,
5.40345218008686));
#153842=CARTESIAN_POINT('Ctrl Pts',(-4.86194858047605,4.69707706858877,
5.43517205187568));
#153843=CARTESIAN_POINT('Ctrl Pts',(-4.89016250998706,4.70392124754382,
5.46694857865637));
#153844=CARTESIAN_POINT('Ctrl Pts',(-4.94936212146285,4.71792585991507,
5.53368415494247));
#153845=CARTESIAN_POINT('Ctrl Pts',(-4.98038800542991,4.72506040965708,
5.56869456572523));
#153846=CARTESIAN_POINT('Ctrl Pts',(-5.01139465595361,4.73200281464944,
5.60371510340813));
#153847=CARTESIAN_POINT('Origin',(-2.94902990916057E-13,4.93907429999893,
3.00107161343988E-13));
#153848=CARTESIAN_POINT('',(-4.8702008953712,4.93794662022304,5.45410559738563));
#153849=CARTESIAN_POINT('Ctrl Pts',(-4.87020089618387,4.93794661936938,
5.45410559780442));
#153850=CARTESIAN_POINT('Ctrl Pts',(-4.80631939369209,4.9181418645925,5.5376993542193));
#153851=CARTESIAN_POINT('Ctrl Pts',(-4.74067711244161,4.89834552799912,
5.61991844185732));
#153852=CARTESIAN_POINT('Ctrl Pts',(-4.63971133011318,4.86872423032248,
5.74098970296878));
#153853=CARTESIAN_POINT('Ctrl Pts',(-4.60570312327546,4.85888055796491,
5.78089941874312));
#153854=CARTESIAN_POINT('Ctrl Pts',(-4.53350175443041,4.83826147078614,
5.86382312992339));
#153855=CARTESIAN_POINT('Ctrl Pts',(-4.4981995269382,4.82833849624498,5.90334388922536));
#153856=CARTESIAN_POINT('Ctrl Pts',(-4.46601718601022,4.81939092005081,
5.93874075821506));
#153857=CARTESIAN_POINT('',(-5.39933745356238,4.81939091961611,5.10500797198601));
#153858=CARTESIAN_POINT('Ctrl Pts',(-5.39933745241095,4.81939091983647,
5.1050079703367));
#153859=CARTESIAN_POINT('Ctrl Pts',(-5.35960920618647,4.8283788969602,5.1339442744892));
#153860=CARTESIAN_POINT('Ctrl Pts',(-5.31655812254176,4.83808518899225,
5.16467301236654));
#153861=CARTESIAN_POINT('Ctrl Pts',(-5.22629740734351,4.85839508126596,
5.22726680555861));
#153862=CARTESIAN_POINT('Ctrl Pts',(-5.18267636485299,4.86818863432646,
5.25677468734867));
#153863=CARTESIAN_POINT('Ctrl Pts',(-5.05049690960121,4.89780165970237,
5.34397633774945));
#153864=CARTESIAN_POINT('Ctrl Pts',(-4.96097126074703,4.91777478468387,
5.40009630635383));
#153865=CARTESIAN_POINT('Ctrl Pts',(-4.8702008950791,4.9379466210003,5.45410559660442));
#153866=CARTESIAN_POINT('Ctrl Pts',(-5.01161177283213,4.7320509931675,5.60386515788382));
#153867=CARTESIAN_POINT('Ctrl Pts',(-5.07990770656187,4.74662633121997,
5.52323342585211));
#153868=CARTESIAN_POINT('Ctrl Pts',(-5.14649632337388,4.76121922804003,
5.44117310698807));
#153869=CARTESIAN_POINT('Ctrl Pts',(-5.27576099365539,4.7903391986696,5.27481766892534));
#153870=CARTESIAN_POINT('Ctrl Pts',(-5.33844518102469,4.80486306082872,
5.19055705554994));
#153871=CARTESIAN_POINT('Ctrl Pts',(-5.39933744725787,4.81939092103739,
5.10500797403888));
#153872=CARTESIAN_POINT('Ctrl Pts',(-5.40566150139869,4.819390921,5.22643899328157));
#153873=CARTESIAN_POINT('Ctrl Pts',(-5.12244937875261,4.754503495,5.51936288912698));
#153874=CARTESIAN_POINT('Ctrl Pts',(-4.80924243929241,4.689276009,5.77996781809004));
#153875=CARTESIAN_POINT('Ctrl Pts',(-5.40430219,4.819390921,5.200338242));
#153876=CARTESIAN_POINT('Ctrl Pts',(-5.122504424,4.754503495,5.493188479));
#153877=CARTESIAN_POINT('Ctrl Pts',(-4.810711519,4.689276009,5.75387301500001));
#153878=CARTESIAN_POINT('Ctrl Pts',(-5.386210996,4.819390921,4.852961066));
#153879=CARTESIAN_POINT('Ctrl Pts',(-5.123237026,4.754503495,5.144830971));
#153880=CARTESIAN_POINT('Ctrl Pts',(-4.830263629,4.689276009,5.406575004));
#153881=CARTESIAN_POINT('',(-5.39281361407602,4.8193909179172,4.97974064683932));
#153882=CARTESIAN_POINT('Ctrl Pts',(-6.25425902407638,4.689268254,4.17391561840196));
#153883=CARTESIAN_POINT('Ctrl Pts',(-6.02510255533609,4.754934719,4.51728717839333));
#153884=CARTESIAN_POINT('Ctrl Pts',(-5.75973310559946,4.819390921,4.83350825853756));
#153885=CARTESIAN_POINT('Ctrl Pts',(-6.22842029200001,4.689268254,4.17813124));
#153886=CARTESIAN_POINT('Ctrl Pts',(-5.999032377,4.754934719,4.520084201));
#153887=CARTESIAN_POINT('Ctrl Pts',(-5.733588172,4.819390921,4.83486987100001));
#153888=CARTESIAN_POINT('Ctrl Pts',(-5.885111492,4.689268254,4.234142502));
#153889=CARTESIAN_POINT('Ctrl Pts',(-5.652648444,4.754934719,4.557247111));
#153890=CARTESIAN_POINT('Ctrl Pts',(-5.38621099600001,4.819390921,4.852961066));
#153891=CARTESIAN_POINT('',(-5.63825790329601,4.81939091975338,4.83983461973514));
#153892=CARTESIAN_POINT('',(-5.51172278325784,4.81939091820872,4.84642449989799));
#153893=CARTESIAN_POINT('',(-6.09898494735702,4.73201982388842,4.39546554549127));
#153894=CARTESIAN_POINT('Ctrl Pts',(-5.63825790479694,4.81939092085883,
4.83983461349765));
#153895=CARTESIAN_POINT('Ctrl Pts',(-5.71791494255591,4.80491309559872,
4.76926446177373));
#153896=CARTESIAN_POINT('Ctrl Pts',(-5.79607638747738,4.79041128765872,
4.69702837984562));
#153897=CARTESIAN_POINT('Ctrl Pts',(-5.94975889685249,4.76128647703165,
4.54889469853867));
#153898=CARTESIAN_POINT('Ctrl Pts',(-6.02524531066462,4.74666639463682,
4.47299410396976));
#153899=CARTESIAN_POINT('Ctrl Pts',(-6.0991057579877,4.73203683307021,4.39552944845035));
#153900=CARTESIAN_POINT('Ctrl Pts',(-5.88232872025789,4.69005394749199,
4.23800765046643));
#153901=CARTESIAN_POINT('Ctrl Pts',(-5.91668025408089,4.6970770688052,4.26292552406789));
#153902=CARTESIAN_POINT('Ctrl Pts',(-5.9510655707326,4.70392124759191,4.28789397167456));
#153903=CARTESIAN_POINT('Ctrl Pts',(-6.02322730468982,4.71792586000582,
4.34034314051077));
#153904=CARTESIAN_POINT('Ctrl Pts',(-6.06105402409859,4.72506040973061,
4.36786537913626));
#153905=CARTESIAN_POINT('Ctrl Pts',(-6.09886413672633,4.73200281470664,
4.39540164253219));
#153906=CARTESIAN_POINT('Origin',(9.65807295250087E-13,4.93907430000018,
-7.16874476447416E-13));
#153907=CARTESIAN_POINT('',(-5.92880978559005,4.93794662022799,4.27964240970281));
#153908=CARTESIAN_POINT('Ctrl Pts',(-5.92880978656371,4.93794661928743,
4.27964240996096));
#153909=CARTESIAN_POINT('Ctrl Pts',(-5.88439198483936,4.91814186452631,
4.37501442529949));
#153910=CARTESIAN_POINT('Ctrl Pts',(-5.83795905720867,4.89834552796916,
4.46942242625393));
#153911=CARTESIAN_POINT('Ctrl Pts',(-5.76538054119186,4.86872423034047,
4.60936776698835));
#153912=CARTESIAN_POINT('Ctrl Pts',(-5.74074683651474,4.85888055798814,
4.65565517495367));
#153913=CARTESIAN_POINT('Ctrl Pts',(-5.68805964221968,4.83826147079414,
4.75216133594935));
#153914=CARTESIAN_POINT('Ctrl Pts',(-5.66207855629228,4.82833849628135,
4.79834705710259));
#153915=CARTESIAN_POINT('Ctrl Pts',(-5.63825790129655,4.81939092014492,
4.83983461867157));
#153916=CARTESIAN_POINT('',(-6.3705297556276,4.81939091962137,3.8249577731703));
#153917=CARTESIAN_POINT('Ctrl Pts',(-6.37052975403151,4.8193909198275,3.82495777170694));
#153918=CARTESIAN_POINT('Ctrl Pts',(-6.33795068445817,4.82837892242052,
3.86175807299039));
#153919=CARTESIAN_POINT('Ctrl Pts',(-6.30251183084649,4.83808522931985,
3.9010231472222));
#153920=CARTESIAN_POINT('Ctrl Pts',(-6.22781732456498,4.85839508129715,
3.98155675809144));
#153921=CARTESIAN_POINT('Ctrl Pts',(-6.19155944002768,4.86818863439397,
4.01975199682512));
#153922=CARTESIAN_POINT('Ctrl Pts',(-6.08121604392898,4.89780165982673,
4.13332959701782));
#153923=CARTESIAN_POINT('Ctrl Pts',(-6.00584758923612,4.91777478480989,
4.20738288023703));
#153924=CARTESIAN_POINT('Ctrl Pts',(-5.92880978508571,4.93794662109296,
4.27964240892365));
#153925=CARTESIAN_POINT('Ctrl Pts',(-6.09910843466592,4.73205099318423,
4.3955015153301));
#153926=CARTESIAN_POINT('Ctrl Pts',(-6.14847420848262,4.74662633121565,
4.30207330148139));
#153927=CARTESIAN_POINT('Ctrl Pts',(-6.19586547756303,4.76121922801461,
4.20761692303707));
#153928=CARTESIAN_POINT('Ctrl Pts',(-6.28634650922938,4.79033919837924,
4.01736270113525));
#153929=CARTESIAN_POINT('Ctrl Pts',(-6.32945163452773,4.80486306068784,
3.92159680566657));
#153930=CARTESIAN_POINT('Ctrl Pts',(-6.37052975011586,4.81939092102897,
3.82495777589447));
#153931=CARTESIAN_POINT('Ctrl Pts',(-6.40281003136325,4.819390921,3.94219032100099));
#153932=CARTESIAN_POINT('Ctrl Pts',(-6.18918922906761,4.754503495,4.28914805360017));
#153933=CARTESIAN_POINT('Ctrl Pts',(-5.93932724980595,4.689276009,4.61099041838498));
#153934=CARTESIAN_POINT('Ctrl Pts',(-6.39587161000001,4.819390921,3.916992003));
#153935=CARTESIAN_POINT('Ctrl Pts',(-6.18361626300001,4.754503495,4.263573754));
#153936=CARTESIAN_POINT('Ctrl Pts',(-5.935152372,4.689276009,4.585189889));
#153937=CARTESIAN_POINT('Ctrl Pts',(-6.303527553,4.819390921,3.581625384));
#153938=CARTESIAN_POINT('Ctrl Pts',(-6.10944517000001,4.754503495,3.923203163));
#153939=CARTESIAN_POINT('Ctrl Pts',(-5.87958855800001,4.689276009,4.241808386));
#153940=CARTESIAN_POINT('',(-6.3372296677262,4.8193909179172,3.70402156085939));
#153941=CARTESIAN_POINT('Ctrl Pts',(-7.00530640168829,4.689268254,2.7318509758169));
#153942=CARTESIAN_POINT('Ctrl Pts',(-6.85532221866109,4.754934719,3.11645656668847));
#153943=CARTESIAN_POINT('Ctrl Pts',(-6.6641351438977,4.819390921,3.48233116048104));
#153944=CARTESIAN_POINT('Ctrl Pts',(-6.980977999,4.689268254,2.741522602));
#153945=CARTESIAN_POINT('Ctrl Pts',(-6.830462824,4.754934719,3.124792514));
#153946=CARTESIAN_POINT('Ctrl Pts',(-6.638894171,4.819390921,3.489281327));
#153947=CARTESIAN_POINT('Ctrl Pts',(-6.657736333,4.689268254,2.870025595));
#153948=CARTESIAN_POINT('Ctrl Pts',(-6.500166082,4.754934719,3.235548881));
#153949=CARTESIAN_POINT('Ctrl Pts',(-6.303527553,4.819390921,3.581625384));
#153950=CARTESIAN_POINT('',(-6.54685994546402,4.81939091973621,3.51462319233795));
#153951=CARTESIAN_POINT('',(-6.4246997757989,4.81939091820872,3.54826031502617));
#153952=CARTESIAN_POINT('',(-6.90128923179587,4.73201982380202,2.98160052488795));
#153953=CARTESIAN_POINT('Ctrl Pts',(-6.54685994559511,4.81939092086963,
3.51462318600688));
#153954=CARTESIAN_POINT('Ctrl Pts',(-6.60948414861081,4.80491309580405,
3.42857901797942));
#153955=CARTESIAN_POINT('Ctrl Pts',(-6.67028959924742,4.79041128806021,
3.34122937663874));
#153956=CARTESIAN_POINT('Ctrl Pts',(-6.78853473591051,4.76128647699977,
3.16352177942524));
#153957=CARTESIAN_POINT('Ctrl Pts',(-6.84593993515113,4.74666639457268,
3.07316835092304));
#153958=CARTESIAN_POINT('Ctrl Pts',(-6.90142095522026,4.73203683297701,
2.98163696307265));
#153959=CARTESIAN_POINT('Ctrl Pts',(-6.65584951415727,4.69005394750498,
2.8743985919351));
#153960=CARTESIAN_POINT('Ctrl Pts',(-6.69475453450432,4.69707706882282,
2.89134933526787));
#153961=CARTESIAN_POINT('Ctrl Pts',(-6.73370341955243,4.70392124757204,
2.90834220782314));
#153962=CARTESIAN_POINT('Ctrl Pts',(-6.8154530731439,4.71792585996462,2.94405250474992));
#153963=CARTESIAN_POINT('Ctrl Pts',(-6.85831189257049,4.72506040967098,
2.96279966231256));
#153964=CARTESIAN_POINT('Ctrl Pts',(-6.90115750837148,4.73200281462704,
2.98156408670324));
#153965=CARTESIAN_POINT('Origin',(8.59555482346508E-13,4.93907430000018,
-3.81856005149395E-13));
#153966=CARTESIAN_POINT('',(-6.71019411999318,4.93794662023874,2.90506789946243));
#153967=CARTESIAN_POINT('Ctrl Pts',(-6.71019412117,4.93794661913889,2.90506789951248));
#153968=CARTESIAN_POINT('Ctrl Pts',(-6.68731694705018,4.91814186443027,
3.00775868445496));
#153969=CARTESIAN_POINT('Ctrl Pts',(-6.6622645250126,4.89834552787458,3.10994118563057));
#153970=CARTESIAN_POINT('Ctrl Pts',(-6.6214669659314,4.86872423024708,3.26221691745863));
#153971=CARTESIAN_POINT('Ctrl Pts',(-6.60735960808125,4.85888055790125,
3.31271766979899));
#153972=CARTESIAN_POINT('Ctrl Pts',(-6.57665018314621,4.83826147076628,
3.41829375935451));
#153973=CARTESIAN_POINT('Ctrl Pts',(-6.56120508540271,4.8283384962618,3.46898484943721));
#153974=CARTESIAN_POINT('Ctrl Pts',(-6.54685994339077,4.81939092009245,
3.51462319175612));
#153975=CARTESIAN_POINT('',(-7.04384316624177,4.81939091957173,2.36605679960635));
#153976=CARTESIAN_POINT('Ctrl Pts',(-7.04384316473025,4.81939091970471,
2.36605679873706));
#153977=CARTESIAN_POINT('Ctrl Pts',(-7.01993684385504,4.82837888959944,
2.40900009757574));
#153978=CARTESIAN_POINT('Ctrl Pts',(-6.99376741163948,4.83808517752402,
2.45496540987332));
#153979=CARTESIAN_POINT('Ctrl Pts',(-6.93813142560118,4.85839508118821,
2.54967354160683));
#153980=CARTESIAN_POINT('Ctrl Pts',(-6.91093207744687,4.86818863432016,
2.59477017043889));
#153981=CARTESIAN_POINT('Ctrl Pts',(-6.82758427512232,4.89780165984243,
2.72941295820832));
#153982=CARTESIAN_POINT('Ctrl Pts',(-6.76989715978556,4.91777478488697,
2.817936906831));
#153983=CARTESIAN_POINT('Ctrl Pts',(-6.71019411921342,4.93794662126058,
2.90506789869156));
#153984=CARTESIAN_POINT('Ctrl Pts',(-6.90141756449681,4.73205099312077,
2.98160910759462));
#153985=CARTESIAN_POINT('Ctrl Pts',(-6.9295448897165,4.74662633118373,2.87975301121524));
#153986=CARTESIAN_POINT('Ctrl Pts',(-6.95552284802293,4.76121922801361,
2.77731724830936));
#153987=CARTESIAN_POINT('Ctrl Pts',(-7.00298945097549,4.79033919925393,
2.57206031116946));
#153988=CARTESIAN_POINT('Ctrl Pts',(-7.02449996483583,4.80486306112818,
2.46926704446389));
#153989=CARTESIAN_POINT('Ctrl Pts',(-7.04384316156922,4.81939092105299,
2.36605680391327));
#153990=CARTESIAN_POINT('Ctrl Pts',(-7.10057027935825,4.819390921,2.47360921065799));
#153991=CARTESIAN_POINT('Ctrl Pts',(-6.96652946959742,4.754503495,2.85837742253879));
#153992=CARTESIAN_POINT('Ctrl Pts',(-6.79169571959383,4.689276009,3.22640823087936));
#153993=CARTESIAN_POINT('Ctrl Pts',(-7.088377181,4.819390921,2.450491571));
#153994=CARTESIAN_POINT('Ctrl Pts',(-6.955589078,4.754503495,2.834599059));
#153995=CARTESIAN_POINT('Ctrl Pts',(-6.78207209700001,4.689276009,3.202108379));
#153996=CARTESIAN_POINT('Ctrl Pts',(-6.926098167,4.819390921,2.14281688));
#153997=CARTESIAN_POINT('Ctrl Pts',(-6.809982448,4.754503495,2.518130736));
#153998=CARTESIAN_POINT('Ctrl Pts',(-6.653990461,4.689276009,2.878699522));
#153999=CARTESIAN_POINT('',(-6.98532390492156,4.8193909179172,2.25510654365763));
#154000=CARTESIAN_POINT('Ctrl Pts',(-7.42879343763473,4.689268254,1.16204801642745));
#154001=CARTESIAN_POINT('Ctrl Pts',(-7.36499463477628,4.754934719,1.56990390823356));
#154002=CARTESIAN_POINT('Ctrl Pts',(-7.25692963095346,4.819390921,1.96832412729405));
#154003=CARTESIAN_POINT('Ctrl Pts',(-7.407112933,4.689268254,1.176723413));
#154004=CARTESIAN_POINT('Ctrl Pts',(-7.342508421,4.754934719,1.583389001));
#154005=CARTESIAN_POINT('Ctrl Pts',(-7.233772858,4.819390921,1.980537866));
#154006=CARTESIAN_POINT('Ctrl Pts',(-7.119052823,4.689268254,1.371709481));
#154007=CARTESIAN_POINT('Ctrl Pts',(-7.043743179,4.754934719,1.762559983));
#154008=CARTESIAN_POINT('Ctrl Pts',(-6.926098167,4.819390921,2.14281688));
#154009=CARTESIAN_POINT('',(-7.14933809287314,4.81939091974536,2.02507189097459));
#154010=CARTESIAN_POINT('',(-7.03726494732171,4.81939091820872,2.08418342172407));
#154011=CARTESIAN_POINT('',(-7.38089690198285,4.73201982388821,1.42831917721988));
#154012=CARTESIAN_POINT('Ctrl Pts',(-7.14933809165179,4.81939092087443,
2.02507188465993));
#154013=CARTESIAN_POINT('Ctrl Pts',(-7.19200122269096,4.80491309589017,
1.9275770295049));
#154014=CARTESIAN_POINT('Ctrl Pts',(-7.2326074846078,4.79041128825026,1.82919820034297));
#154015=CARTESIAN_POINT('Ctrl Pts',(-7.30988623568892,4.76128647706763,
1.63022609776993));
#154016=CARTESIAN_POINT('Ctrl Pts',(-7.34652601697845,4.74666639465519,
1.52964466117206));
#154017=CARTESIAN_POINT('Ctrl Pts',(-7.3810333788971,4.73203683306954,1.42832644690564));
#154018=CARTESIAN_POINT('Ctrl Pts',(-7.11815018181255,4.69005394745638,
1.37638584987177));
#154019=CARTESIAN_POINT('Ctrl Pts',(-7.15978953282356,4.69707706872065,
1.38457686486532));
#154020=CARTESIAN_POINT('Ctrl Pts',(-7.2014807805252,4.70392124759223,1.39279959468546));
#154021=CARTESIAN_POINT('Ctrl Pts',(-7.28899583059621,4.71792585998154,
1.41010124566418));
#154022=CARTESIAN_POINT('Ctrl Pts',(-7.33488271934859,4.72506040971655,
1.41919672582886));
#154023=CARTESIAN_POINT('Ctrl Pts',(-7.38076042506859,4.73200281470688,
1.42831190753412));
#154024=CARTESIAN_POINT('Origin',(-2.94902990916057E-14,4.93907430000053,
-4.98732999343332E-14));
#154025=CARTESIAN_POINT('',(-7.17781723584371,4.93794662022731,1.39465564117819));
#154026=CARTESIAN_POINT('Ctrl Pts',(-7.17781723670216,4.93794661941343,
1.39465564102716));
#154027=CARTESIAN_POINT('Ctrl Pts',(-7.17755040150417,4.91814186461323,
1.49986348894002));
#154028=CARTESIAN_POINT('Ctrl Pts',(-7.17504990843411,4.89834552801126,
1.60504255047927));
#154029=CARTESIAN_POINT('Ctrl Pts',(-7.16794095468464,4.86872423033395,
1.76252842994329));
#154030=CARTESIAN_POINT('Ctrl Pts',(-7.16501958796713,4.85888055797704,
1.81488116780166));
#154031=CARTESIAN_POINT('Ctrl Pts',(-7.157723870727,4.83826147080119,1.9245905659777));
#154032=CARTESIAN_POINT('Ctrl Pts',(-7.15353695671268,4.8283384962796,1.9774167661419));
#154033=CARTESIAN_POINT('Ctrl Pts',(-7.14933809068473,4.81939092011745,
2.02507189085163));
#154034=CARTESIAN_POINT('',(-7.38779429945998,4.81939091967051,0.796521640787532));
#154035=CARTESIAN_POINT('Ctrl Pts',(-7.38779429716093,4.8193909199705,0.796521640040918));
#154036=CARTESIAN_POINT('Ctrl Pts',(-7.37367837789995,4.82837892375171,
0.843600292298873));
#154037=CARTESIAN_POINT('Ctrl Pts',(-7.35800192287268,4.83808523015355,
0.894116694457562));
#154038=CARTESIAN_POINT('Ctrl Pts',(-7.3240262118831,4.85839508130368,0.998570424941728));
#154039=CARTESIAN_POINT('Ctrl Pts',(-7.30715721170585,4.86818863432921,
1.04845977495898));
#154040=CARTESIAN_POINT('Ctrl Pts',(-7.2547022543451,4.89780165967758,1.19787200213601));
#154041=CARTESIAN_POINT('Ctrl Pts',(-7.21739386403372,4.91777478464996,
1.29672733440014));
#154042=CARTESIAN_POINT('Ctrl Pts',(-7.17781723517334,4.93794662096607,
1.3946556407551));
#154043=CARTESIAN_POINT('Ctrl Pts',(-7.38102407937051,4.73205099318476,
1.42829997158409));
#154044=CARTESIAN_POINT('Ctrl Pts',(-7.38659775345975,4.74662633124308,
1.32277867077803));
#154045=CARTESIAN_POINT('Ctrl Pts',(-7.38994770048621,4.76121922805999,
1.21715330607263));
#154046=CARTESIAN_POINT('Ctrl Pts',(-7.39218038646568,4.79033919864747,
1.00649125024579));
#154047=CARTESIAN_POINT('Ctrl Pts',(-7.39109048280139,4.80486306081453,
0.901477106205701));
#154048=CARTESIAN_POINT('Ctrl Pts',(-7.38779429544083,4.81939092103713,
0.796521646044604));
#154049=CARTESIAN_POINT('Ctrl Pts',(-7.46631575272062,4.819390921,0.88936488343584));
#154050=CARTESIAN_POINT('Ctrl Pts',(-7.41812253464388,4.754503495,1.2939522410014));
#154051=CARTESIAN_POINT('Ctrl Pts',(-7.32649204551892,4.689276009,1.69096278051253));
#154052=CARTESIAN_POINT('Ctrl Pts',(-7.44943811300001,4.819390921,0.869408877));
#154053=CARTESIAN_POINT('Ctrl Pts',(-7.40232627800001,4.754503495,1.273081663));
#154054=CARTESIAN_POINT('Ctrl Pts',(-7.311869668,4.689276009,1.66929984));
#154055=CARTESIAN_POINT('Ctrl Pts',(-7.224812129,4.819390921,0.603812641));
#154056=CARTESIAN_POINT('Ctrl Pts',(-7.192092516,4.754503495,0.995313314));
#154057=CARTESIAN_POINT('Ctrl Pts',(-7.117259166,4.689276009,1.380985869));
#154058=CARTESIAN_POINT('',(-7.30679216083989,4.81939091791748,0.700745251315236));
#154059=CARTESIAN_POINT('Ctrl Pts',(-7.5049183491183,4.689268254,-0.462091015612824));
#154060=CARTESIAN_POINT('Ctrl Pts',(-7.53028808736866,4.754934719,-0.0500557111030223));
#154061=CARTESIAN_POINT('Ctrl Pts',(-7.51039815272873,4.819390921,0.362280445934188));
#154062=CARTESIAN_POINT('Ctrl Pts',(-7.48689949900001,4.689268254,-0.443098054));
#154063=CARTESIAN_POINT('Ctrl Pts',(-7.511226485,4.754934719,-0.032052021));
#154064=CARTESIAN_POINT('Ctrl Pts',(-7.49040836500001,4.819390921,0.379186656));
#154065=CARTESIAN_POINT('Ctrl Pts',(-7.247490315,4.689268254,-0.190746244));
#154066=CARTESIAN_POINT('Ctrl Pts',(-7.257962673,4.754934719,0.207155738));
#154067=CARTESIAN_POINT('Ctrl Pts',(-7.224812129,4.819390921,0.603812641));
#154068=CARTESIAN_POINT('',(-7.41752113704197,4.81939091971279,0.440830478443873));
#154069=CARTESIAN_POINT('',(-7.32077543098668,4.81939091820872,0.522652428364941));
#154070=CARTESIAN_POINT('',(-7.51538203638646,4.73201982383859,-0.191748787497206));
#154071=CARTESIAN_POINT('Ctrl Pts',(-7.41752113453922,4.81939092085595,
0.440830472769329));
#154072=CARTESIAN_POINT('Ctrl Pts',(-7.43822831383812,4.80491309553719,
0.336443678595771));
#154073=CARTESIAN_POINT('Ctrl Pts',(-7.45673668403369,4.79041128752491,
0.231635743075057));
#154074=CARTESIAN_POINT('Ctrl Pts',(-7.48943557967304,4.76128647694917,
0.0207028550013527));
#154075=CARTESIAN_POINT('Ctrl Pts',(-7.50359670749935,4.74666639456738,
-0.0854035131269754));
#154076=CARTESIAN_POINT('Ctrl Pts',(-7.51551688532758,4.73203683301208,
-0.191771026338893));
#154077=CARTESIAN_POINT('Ctrl Pts',(-7.24761405796477,4.69005394746672,
-0.185985164613402));
#154078=CARTESIAN_POINT('Ctrl Pts',(-7.2900407301435,4.69707706869655,-0.186936880614835));
#154079=CARTESIAN_POINT('Ctrl Pts',(-7.33252490370272,4.70392124758181,
-0.187868779482321));
#154080=CARTESIAN_POINT('Ctrl Pts',(-7.4217132440767,4.71792585994043,-0.189784780218647));
#154081=CARTESIAN_POINT('Ctrl Pts',(-7.46848258230995,4.72506040967391,
-0.190766271932785));
#154082=CARTESIAN_POINT('Ctrl Pts',(-7.51524718744534,4.7320028146651,-0.19172654865552));
#154083=CARTESIAN_POINT('Origin',(5.52075746229619E-13,4.93907429999911,
4.82198916212928E-14));
#154084=CARTESIAN_POINT('',(-7.30981359479562,4.93794662022752,-0.180969163073113));
#154085=CARTESIAN_POINT('Ctrl Pts',(-7.30981359571788,4.93794661929613,
-0.180969163453093));
#154086=CARTESIAN_POINT('Ctrl Pts',(-7.33216957627644,4.91814186456599,
-0.0781636550505026));
#154087=CARTESIAN_POINT('Ctrl Pts',(-7.35233793245503,4.8983455280094,0.025093910417717));
#154088=CARTESIAN_POINT('Ctrl Pts',(-7.37924999091234,4.86872423035244,
0.180426072259296));
#154089=CARTESIAN_POINT('Ctrl Pts',(-7.38765121524058,4.85888055798396,
0.232182839687074));
#154090=CARTESIAN_POINT('Ctrl Pts',(-7.40411034549692,4.83826147074226,
0.340895656795059));
#154091=CARTESIAN_POINT('Ctrl Pts',(-7.41137739073122,4.82833849619623,
0.393386872495712));
#154092=CARTESIAN_POINT('Ctrl Pts',(-7.4175211349983,4.81939092004165,0.440830478770539));
#154093=CARTESIAN_POINT('',(-7.38630038196097,4.81939091969751,-0.810257984855973));
#154094=CARTESIAN_POINT('Ctrl Pts',(-7.38630037963555,4.81939091994588,
-0.810257985075426));
#154095=CARTESIAN_POINT('Ctrl Pts',(-7.38263500614926,4.82837891042957,
-0.761245578091695));
#154096=CARTESIAN_POINT('Ctrl Pts',(-7.37818459619328,4.83808521117728,
-0.708540272239645));
#154097=CARTESIAN_POINT('Ctrl Pts',(-7.3674576729076,4.85839508126324,-0.599224736206719));
#154098=CARTESIAN_POINT('Ctrl Pts',(-7.36170779607613,4.8681886343682,-0.546875434589808));
#154099=CARTESIAN_POINT('Ctrl Pts',(-7.34259841866334,4.89780165980116,
-0.389680116429263));
#154100=CARTESIAN_POINT('Ctrl Pts',(-7.32741325205991,4.91777478478915,
-0.285115765756162));
#154101=CARTESIAN_POINT('Ctrl Pts',(-7.30981359392888,4.93794662108625,
-0.180969163385907));
#154102=CARTESIAN_POINT('Ctrl Pts',(-7.51550211177187,4.73205099316266,
-0.19179488355814));
#154103=CARTESIAN_POINT('Ctrl Pts',(-7.49826151596717,4.74662633122546,
-0.296047330203138));
#154104=CARTESIAN_POINT('Ctrl Pts',(-7.47882681194459,4.76121922804102,
-0.399923372205497));
#154105=CARTESIAN_POINT('Ctrl Pts',(-7.43572118392055,4.7903391987379,-0.606140228564144));
#154106=CARTESIAN_POINT('Ctrl Pts',(-7.41208182486807,4.80486306086146,
-0.708464902909228));
#154107=CARTESIAN_POINT('Ctrl Pts',(-7.38630037914515,4.81939092103882,
-0.810257979522875));
#154108=CARTESIAN_POINT('Ctrl Pts',(-7.48294460067957,4.819390921,-0.736465157357116));
#154109=CARTESIAN_POINT('Ctrl Pts',(-7.52285243445693,4.754503495,-0.330976710562069));
#154110=CARTESIAN_POINT('Ctrl Pts',(-7.51870974654472,4.689276009,0.0764497902556042));
#154111=CARTESIAN_POINT('Ctrl Pts',(-7.462171599,4.819390921,-0.75232641));
#154112=CARTESIAN_POINT('Ctrl Pts',(-7.502938928,4.754503495,-0.347963618));
#154113=CARTESIAN_POINT('Ctrl Pts',(-7.49977234,4.689276009,0.058436696));
#154114=CARTESIAN_POINT('Ctrl Pts',(-7.185701905,4.819390921,-0.963425207));
#154115=CARTESIAN_POINT('Ctrl Pts',(-7.237908331,4.754503495,-0.574043853));
#154116=CARTESIAN_POINT('Ctrl Pts',(-7.247732742,4.689276009,-0.181301149));
#154117=CARTESIAN_POINT('',(-7.28559392484569,4.81939091791749,-0.887152541784059));
#154118=CARTESIAN_POINT('Ctrl Pts',(-7.23012161980515,4.689268254,-2.0646231853681));
#154119=CARTESIAN_POINT('Ctrl Pts',(-7.34347363819581,4.754934719,-1.66767478139762));
#154120=CARTESIAN_POINT('Ctrl Pts',(-7.41268880490121,4.819390921,-1.26070306624057));
#154121=CARTESIAN_POINT('Ctrl Pts',(-7.21660696600001,4.689268254,-2.042200749));
#154122=CARTESIAN_POINT('Ctrl Pts',(-7.328727947,4.754934719,-1.645994327));
#154123=CARTESIAN_POINT('Ctrl Pts',(-7.396800703,4.819390921,-1.239894901));
#154124=CARTESIAN_POINT('Ctrl Pts',(-7.037043215,4.689268254,-1.744282886));
#154125=CARTESIAN_POINT('Ctrl Pts',(-7.13280789900001,4.754934719,-1.357934879));
#154126=CARTESIAN_POINT('Ctrl Pts',(-7.18570190500001,4.819390921,-0.963425207));
#154127=CARTESIAN_POINT('',(-7.3388691369478,4.81939091972585,-1.16402367686312));
#154128=CARTESIAN_POINT('',(-7.26197459231862,4.81939091820873,-1.06331721224712));
#154129=CARTESIAN_POINT('',(-7.29845625953015,4.73201982380467,-1.80285079211797));
#154130=CARTESIAN_POINT('Ctrl Pts',(-7.33886913323993,4.81939092085855,
-1.16402368197451));
#154131=CARTESIAN_POINT('Ctrl Pts',(-7.33665211510866,4.80491309559566,
-1.27042140196416));
#154132=CARTESIAN_POINT('Ctrl Pts',(-7.33219716189816,4.79041128764499,
-1.37675773825831));
#154133=CARTESIAN_POINT('Ctrl Pts',(-7.31878723969319,4.7612864769747,-1.58978842933262));
#154134=CARTESIAN_POINT('Ctrl Pts',(-7.30980755554305,4.74666639456651,
-1.69645831361357));
#154135=CARTESIAN_POINT('Ctrl Pts',(-7.29858317508326,4.73203683298043,
-1.80290149954302));
#154136=CARTESIAN_POINT('Ctrl Pts',(-7.03818755575372,4.69005394737967,
-1.73965971898629));
#154137=CARTESIAN_POINT('Ctrl Pts',(-7.07941772512982,4.69707706861374,
-1.74970966487086));
#154138=CARTESIAN_POINT('Ctrl Pts',(-7.12070831179316,4.70392124752775,
-1.75975261806698));
#154139=CARTESIAN_POINT('Ctrl Pts',(-7.20739959490221,4.71792585989463,
-1.78079668068838));
#154140=CARTESIAN_POINT('Ctrl Pts',(-7.25286450035518,4.72506040963286,
-1.79180925094483));
#154141=CARTESIAN_POINT('Ctrl Pts',(-7.29832934397703,4.7320028146289,-1.80280008469291));
#154142=CARTESIAN_POINT('Origin',(-8.8037216405823E-13,4.93907430000053,
-2.65304271607203E-13));
#154143=CARTESIAN_POINT('',(-7.10001119460225,4.93794662021071,-1.74813205033564));
#154144=CARTESIAN_POINT('Ctrl Pts',(-7.10001119554104,4.93794661914312,
-1.74813205098826));
#154145=CARTESIAN_POINT('Ctrl Pts',(-7.14394465112064,4.91814186436947,
-1.65253595326797));
#154146=CARTESIAN_POINT('Ctrl Pts',(-7.18583880662247,4.89834552781747,
-1.55602809274632));
#154147=CARTESIAN_POINT('Ctrl Pts',(-7.24551349920576,4.86872423023617,
-1.41011280770722));
#154148=CARTESIAN_POINT('Ctrl Pts',(-7.26484448257846,4.85888055791847,
-1.36137209975618));
#154149=CARTESIAN_POINT('Ctrl Pts',(-7.30428884953336,4.8382614707778,-1.2587391545377));
#154150=CARTESIAN_POINT('Ctrl Pts',(-7.32267005503197,4.82833849625316,
-1.20903735410299));
#154151=CARTESIAN_POINT('Ctrl Pts',(-7.33886913496549,4.81939092007772,
-1.16402367607981));
#154152=CARTESIAN_POINT('',(-7.03943126753197,4.81939091962378,-2.37915084878438));
#154153=CARTESIAN_POINT('Ctrl Pts',(-7.03943126550706,4.81939091985741,
-2.37915084853802));
#154154=CARTESIAN_POINT('Ctrl Pts',(-7.04638780382853,4.82837890877908,
-2.33049638615935));
#154155=CARTESIAN_POINT('Ctrl Pts',(-7.05337152460824,4.83808520858237,
-2.27806659884981));
#154156=CARTESIAN_POINT('Ctrl Pts',(-7.06639500140624,4.85839508132424,
-2.16900081368179));
#154157=CARTESIAN_POINT('Ctrl Pts',(-7.07203310589037,4.86818863440908,
-2.1166393562294));
#154158=CARTESIAN_POINT('Ctrl Pts',(-7.08716284183417,4.89780165986177,
-1.95901122594177));
#154159=CARTESIAN_POINT('Ctrl Pts',(-7.09481094048261,4.91777478488203,
-1.85362716958633));
#154160=CARTESIAN_POINT('Ctrl Pts',(-7.10001119355224,4.93794662119754,
-1.74813205047258));
#154161=CARTESIAN_POINT('Ctrl Pts',(-7.29856361833912,4.73205099311978,
-1.80292162311842));
#154162=CARTESIAN_POINT('Ctrl Pts',(-7.25931490371634,4.74662633119835,
-1.9010304870377));
#154163=CARTESIAN_POINT('Ctrl Pts',(-7.21800429377516,4.76121922803141,
-1.99830007803845));
#154164=CARTESIAN_POINT('Ctrl Pts',(-7.13157592253394,4.79033919889737,
-2.190429264016));
#154165=CARTESIAN_POINT('Ctrl Pts',(-7.08649245851456,4.80486306093905,
-2.28527988030872));
#154166=CARTESIAN_POINT('Ctrl Pts',(-7.03943126641627,4.81939092104429,
-2.37915084214098));
#154167=CARTESIAN_POINT('Ctrl Pts',(-7.1496792742943,4.819390921,-2.32785890618325));
#154168=CARTESIAN_POINT('Ctrl Pts',(-7.27582211625994,4.754503495,-1.94042955853822));
#154169=CARTESIAN_POINT('Ctrl Pts',(-7.35936093581297,4.689276009,-1.54163790783283));
#154170=CARTESIAN_POINT('Ctrl Pts',(-7.125982234,4.819390921,-2.33888375));
#154171=CARTESIAN_POINT('Ctrl Pts',(-7.25272249400001,4.754503495,-1.952738506));
#154172=CARTESIAN_POINT('Ctrl Pts',(-7.33699399300001,4.689276009,-1.555158883));
#154173=CARTESIAN_POINT('Ctrl Pts',(-6.810596247,4.819390921,-2.485614363));
#154174=CARTESIAN_POINT('Ctrl Pts',(-6.945287596,4.754503495,-2.116559367));
#154175=CARTESIAN_POINT('Ctrl Pts',(-7.03931039,4.689276009,-1.735110727));
#154176=CARTESIAN_POINT('',(-6.92454921546238,4.8193909179172,-2.43259874169278));
#154177=CARTESIAN_POINT('Ctrl Pts',(-6.61725243872918,4.689268254,-3.57061587074017));
#154178=CARTESIAN_POINT('Ctrl Pts',(-6.81328652345985,4.754934719,-3.20731523249149));
#154179=CARTESIAN_POINT('Ctrl Pts',(-6.96837036658216,4.819390921,-2.82473750445019));
#154180=CARTESIAN_POINT('Ctrl Pts',(-6.608873911,4.689268254,-3.545812407));
#154181=CARTESIAN_POINT('Ctrl Pts',(-6.803546235,4.754934719,-3.182971767));
#154182=CARTESIAN_POINT('Ctrl Pts',(-6.95732686000001,4.819390921,-2.80100035));
#154183=CARTESIAN_POINT('Ctrl Pts',(-6.49755179600001,4.689268254,-3.216258799));
#154184=CARTESIAN_POINT('Ctrl Pts',(-6.674130955,4.754934719,-2.85952997));
#154185=CARTESIAN_POINT('Ctrl Pts',(-6.810596247,4.819390921,-2.485614363));
#154186=CARTESIAN_POINT('',(-6.9170597724146,4.81939091969098,-2.71444937933755));
#154187=CARTESIAN_POINT('',(-6.86361189254967,4.81939091820872,-2.59956732185072));
#154188=CARTESIAN_POINT('',(-6.74026277951148,4.73201982385666,-3.32965349748354));
#154189=CARTESIAN_POINT('Ctrl Pts',(-6.91705976785379,4.81939092086901,
-2.71444938335613));
#154190=CARTESIAN_POINT('Ctrl Pts',(-6.89202221803927,4.80491309582878,
-2.81788298886713));
#154191=CARTESIAN_POINT('Ctrl Pts',(-6.86481225063187,4.79041128809892,
-2.92077555594569));
#154192=CARTESIAN_POINT('Ctrl Pts',(-6.80592054268088,4.761286477031,-3.12594297386103));
#154193=CARTESIAN_POINT('Ctrl Pts',(-6.77421992653286,4.74666639461734,
-3.22818860897718));
#154194=CARTESIAN_POINT('Ctrl Pts',(-6.74037582725774,4.73203683303548,
-3.32973030246518));
#154195=CARTESIAN_POINT('Ctrl Pts',(-6.4996632263326,4.69005394725939,-3.2119897183158));
#154196=CARTESIAN_POINT('Ctrl Pts',(-6.5377690158468,4.69707706853122,-3.23066796984932));
#154197=CARTESIAN_POINT('Ctrl Pts',(-6.57593531352748,4.70392124749675,
-3.24935238012372));
#154198=CARTESIAN_POINT('Ctrl Pts',(-6.65607595110484,4.71792585990761,
-3.28854050765078));
#154199=CARTESIAN_POINT('Ctrl Pts',(-6.6981105352828,4.72506040966862,-3.30906922090527));
#154200=CARTESIAN_POINT('Ctrl Pts',(-6.74014973176521,4.73200281467784,
-3.32957669250189));
#154201=CARTESIAN_POINT('Origin',(3.63424568217141E-13,4.93907430000018,
1.19479079407903E-13));
#154202=CARTESIAN_POINT('',(-6.55822016129101,4.93794662025088,-3.233554227833));
#154203=CARTESIAN_POINT('Ctrl Pts',(-6.55822016187665,4.93794661944576,
-3.23355422846586));
#154204=CARTESIAN_POINT('Ctrl Pts',(-6.62167681304073,4.91814186463008,
-3.14963750850499));
#154205=CARTESIAN_POINT('Ctrl Pts',(-6.68333784388084,4.89834552804239,
-3.06439195297611));
#154206=CARTESIAN_POINT('Ctrl Pts',(-6.77298484869264,4.86872423034124,
-2.93471638075813));
#154207=CARTESIAN_POINT('Ctrl Pts',(-6.80234169603496,4.85888055795474,
-2.89127079325353));
#154208=CARTESIAN_POINT('Ctrl Pts',(-6.86292692531123,4.83826147067629,
-2.79951672185459));
#154209=CARTESIAN_POINT('Ctrl Pts',(-6.89156280638917,4.8283384961102,-2.75492833775227));
#154210=CARTESIAN_POINT('Ctrl Pts',(-6.91705977081307,4.8193909199736,-2.7144493782663));
#154211=CARTESIAN_POINT('',(-6.36340617132589,4.81939091960603,-3.83679726201069));
#154212=CARTESIAN_POINT('Ctrl Pts',(-6.36340616948724,4.81939091980664,
-3.83679726136057));
#154213=CARTESIAN_POINT('Ctrl Pts',(-6.3806593570124,4.8283789174746,-3.7907757165676));
#154214=CARTESIAN_POINT('Ctrl Pts',(-6.39875066126507,4.83808522135753,
-3.74107298389996));
#154215=CARTESIAN_POINT('Ctrl Pts',(-6.4349155533591,4.85839508125963,-3.63735682436214));
#154216=CARTESIAN_POINT('Ctrl Pts',(-6.45167800761775,4.86818863433314,
-3.5874315745783));
#154217=CARTESIAN_POINT('Ctrl Pts',(-6.50033940714799,4.89780165972296,
-3.43674114880472));
#154218=CARTESIAN_POINT('Ctrl Pts',(-6.53046315438364,4.91777478469678,
-3.33546502858284));
#154219=CARTESIAN_POINT('Ctrl Pts',(-6.5582201605052,4.93794662098598,-3.23355422776447));
#154220=CARTESIAN_POINT('Ctrl Pts',(-6.74035240177763,4.73205099316135,
-3.32974575144665));
#154221=CARTESIAN_POINT('Ctrl Pts',(-6.68093079468288,4.74662633123018,
-3.41712357109346));
#154222=CARTESIAN_POINT('Ctrl Pts',(-6.61967591711042,4.76121922805284,
-3.50323849301328));
#154223=CARTESIAN_POINT('Ctrl Pts',(-6.49396609790326,4.79033919882502,
-3.67229625980263));
#154224=CARTESIAN_POINT('Ctrl Pts',(-6.42954658131606,4.80486306090825,
-3.7552377095359));
#154225=CARTESIAN_POINT('Ctrl Pts',(-6.363406171612,4.81939092104128,-3.83679725544552));
#154226=CARTESIAN_POINT('Ctrl Pts',(-6.48210289236304,4.819390921,-3.81040455899514));
#154227=CARTESIAN_POINT('Ctrl Pts',(-6.68858244194038,4.754503495,-3.45915007679625));
#154228=CARTESIAN_POINT('Ctrl Pts',(-6.8558965873045,4.689276009,-3.08764033017328));
#154229=CARTESIAN_POINT('Ctrl Pts',(-6.45658986,4.819390921,-3.816077485));
#154230=CARTESIAN_POINT('Ctrl Pts',(-6.66337681600001,4.754503495,-3.466205512));
#154231=CARTESIAN_POINT('Ctrl Pts',(-6.831145961,4.689276009,-3.096036961));
#154232=CARTESIAN_POINT('Ctrl Pts',(-6.117034678,4.819390921,-3.891578954));
#154233=CARTESIAN_POINT('Ctrl Pts',(-6.327912933,4.754503495,-3.560106917));
#154234=CARTESIAN_POINT('Ctrl Pts',(-6.501737708,4.689276009,-3.207788456));
#154235=CARTESIAN_POINT('',(-6.24095952935368,4.8193909179172,-3.86402377588778));
#154236=CARTESIAN_POINT('Ctrl Pts',(-5.69496788889646,4.689268254,-4.90965052517024));
#154237=CARTESIAN_POINT('Ctrl Pts',(-5.96451770339228,4.754934719,-4.59698518770047));
#154238=CARTESIAN_POINT('Ctrl Pts',(-6.19821867492906,4.819390921,-4.25669035731628));
#154239=CARTESIAN_POINT('Ctrl Pts',(-5.69211725800001,4.689268254,-4.883625817));
#154240=CARTESIAN_POINT('Ctrl Pts',(-5.960238263,4.754934719,-4.571116985));
#154241=CARTESIAN_POINT('Ctrl Pts',(-6.192536146,4.819390921,-4.231134137));
#154242=CARTESIAN_POINT('Ctrl Pts',(-5.654242076,4.689268254,-4.537846025));
#154243=CARTESIAN_POINT('Ctrl Pts',(-5.903379066,4.754934719,-4.227416618));
#154244=CARTESIAN_POINT('Ctrl Pts',(-6.117034678,4.819390921,-3.891578954));
#154245=CARTESIAN_POINT('',(-6.17181638077985,4.81939091971653,-4.13795044575052));
#154246=CARTESIAN_POINT('',(-6.14431432941737,4.81939091820872,-4.01426455256242));
#154247=CARTESIAN_POINT('',(-5.86690210342724,4.73201982384263,-4.70076530568075));
#154248=CARTESIAN_POINT('Ctrl Pts',(-6.17181637537512,4.81939092084589,
-4.13795044869547));
#154249=CARTESIAN_POINT('Ctrl Pts',(-6.12512902047052,4.80491309537189,
-4.23358350371706));
#154250=CARTESIAN_POINT('Ctrl Pts',(-6.07643634486721,4.79041128718496,
-4.32822116392062));
#154251=CARTESIAN_POINT('Ctrl Pts',(-5.97481656514734,4.76128647695001,
-4.51593189974137));
#154252=CARTESIAN_POINT('Ctrl Pts',(-5.92187730276754,4.74666639456897,
-4.60897239303821));
#154253=CARTESIAN_POINT('Ctrl Pts',(-5.86699599736058,4.73203683301616,
-4.70086461697002));
#154254=CARTESIAN_POINT('Ctrl Pts',(-5.65722186833484,4.6900539472246,-4.53413064874397));
#154255=CARTESIAN_POINT('Ctrl Pts',(-5.6904214938143,4.69707706850835,-4.56056383126527));
#154256=CARTESIAN_POINT('Ctrl Pts',(-5.72367888888419,4.70392124749352,
-4.58701603615188));
#154257=CARTESIAN_POINT('Ctrl Pts',(-5.79352159389577,4.71792585990658,
-4.64251583503509));
#154258=CARTESIAN_POINT('Ctrl Pts',(-5.83016036631121,4.72506040966537,
-4.67160079145656));
#154259=CARTESIAN_POINT('Ctrl Pts',(-5.8668082094939,4.73200281466911,-4.70066599439149));
#154260=CARTESIAN_POINT('Origin',(5.00901403688303E-13,4.93907429999947,
4.46257614195034E-13));
#154261=CARTESIAN_POINT('',(-5.70977404307001,4.93794662017026,-4.56777900150209));
#154262=CARTESIAN_POINT('Ctrl Pts',(-5.70977404358148,4.93794661922554,
-4.56777900237504));
#154263=CARTESIAN_POINT('Ctrl Pts',(-5.78978672754553,4.9181418644839,-4.49946551303395));
#154264=CARTESIAN_POINT('Ctrl Pts',(-5.86833143216554,4.89834552793919,
-4.42946825032602));
#154265=CARTESIAN_POINT('Ctrl Pts',(-5.98375895432666,4.86872423033756,
-4.32209587730957));
#154266=CARTESIAN_POINT('Ctrl Pts',(-6.02176897178718,4.85888055800352,
-4.28597687805401));
#154267=CARTESIAN_POINT('Ctrl Pts',(-6.1006621650845,4.83826147078189,-4.20939199933421));
#154268=CARTESIAN_POINT('Ctrl Pts',(-6.13821373977607,4.82833849622781,
-4.17200193476362));
#154269=CARTESIAN_POINT('Ctrl Pts',(-6.17181637932586,4.81939092005262,
-4.13795044422738));
#154270=CARTESIAN_POINT('',(-5.38983527523063,4.81939091970597,-5.1150393000287));
#154271=CARTESIAN_POINT('Ctrl Pts',(-5.38983527319774,4.81939091997457,
-5.11503929876886));
#154272=CARTESIAN_POINT('Ctrl Pts',(-5.4165784094306,4.82837893202885,-5.07380256711433));
#154273=CARTESIAN_POINT('Ctrl Pts',(-5.44493138418316,4.83808524390011,
-5.02915091937289));
#154274=CARTESIAN_POINT('Ctrl Pts',(-5.50254660586824,4.85839508130118,
-4.93563407236016));
#154275=CARTESIAN_POINT('Ctrl Pts',(-5.52964961625224,4.86818863439001,
-4.89047947924477));
#154276=CARTESIAN_POINT('Ctrl Pts',(-5.6095673266254,4.89780165979951,-4.75377287414642));
#154277=CARTESIAN_POINT('Ctrl Pts',(-5.66076286351395,4.91777664866465,
-4.66133161615084));
#154278=CARTESIAN_POINT('Ctrl Pts',(-5.70977860043483,4.93794849692008,
-4.56777030045401));
#154279=CARTESIAN_POINT('Ctrl Pts',(-5.86696979846174,4.73205099316642,
-4.70087466896192));
#154280=CARTESIAN_POINT('Ctrl Pts',(-5.79015378711476,4.74662633121483,
-4.7734357548079));
#154281=CARTESIAN_POINT('Ctrl Pts',(-5.71181885180552,4.76121922803017,
-4.84436936979641));
#154282=CARTESIAN_POINT('Ctrl Pts',(-5.55270563680197,4.79033919858816,
-4.98245076390519));
#154283=CARTESIAN_POINT('Ctrl Pts',(-5.47196225209423,4.80486306078942,
-5.04960479741087));
#154284=CARTESIAN_POINT('Ctrl Pts',(-5.38983527625753,4.8193909210351,-5.11503929400405));
#154285=CARTESIAN_POINT('Ctrl Pts',(-5.51143058358818,4.819390921,-5.11477993069985));
#154286=CARTESIAN_POINT('Ctrl Pts',(-5.7885920867199,4.754503495,-4.81612458249205));
#154287=CARTESIAN_POINT('Ctrl Pts',(-6.0318581341366,4.689276009,-4.4892681216581));
#154288=CARTESIAN_POINT('Ctrl Pts',(-5.48529452,4.819390921,-5.114835679));
#154289=CARTESIAN_POINT('Ctrl Pts',(-5.762459044,4.754503495,-4.817596601));
#154290=CARTESIAN_POINT('Ctrl Pts',(-6.005881136,4.689276009,-4.492147791));
#154291=CARTESIAN_POINT('Ctrl Pts',(-5.137447365,4.819390921,-5.115577638));
#154292=CARTESIAN_POINT('Ctrl Pts',(-5.414652094,4.754503495,-4.837187824));
#154293=CARTESIAN_POINT('Ctrl Pts',(-5.66015099700001,4.689276009,-4.530473562));
#154294=CARTESIAN_POINT('',(-5.2643984710689,4.81939091791741,-5.11530686482257));
#154295=CARTESIAN_POINT('Ctrl Pts',(-4.50639296980373,4.689268254,-6.01911537846736));
#154296=CARTESIAN_POINT('Ctrl Pts',(-4.83685466449597,4.754934719,-5.771705224826));
#154297=CARTESIAN_POINT('Ctrl Pts',(-5.13824516666925,4.819390921,-5.48960509895427));
#154298=CARTESIAN_POINT('Ctrl Pts',(-4.509203528,4.689268254,-5.993086312));
#154299=CARTESIAN_POINT('Ctrl Pts',(-4.838236174,4.754934719,-5.745521853));
#154300=CARTESIAN_POINT('Ctrl Pts',(-5.138189324,4.819390921,-5.46342479300001));
#154301=CARTESIAN_POINT('Ctrl Pts',(-4.54654628,4.689268254,-5.647248615));
#154302=CARTESIAN_POINT('Ctrl Pts',(-4.85659173300001,4.754934719,-5.397633963));
#154303=CARTESIAN_POINT('Ctrl Pts',(-5.137447365,4.819390921,-5.11557763800001));
#154304=CARTESIAN_POINT('',(-5.13798571439769,4.81939091970502,-5.3679655482769));
#154305=CARTESIAN_POINT('',(-5.13771545634754,4.81939091820872,-5.24125923432883));
#154306=CARTESIAN_POINT('',(-4.71921160543078,4.73201982384171,-5.85207455297479));
#154307=CARTESIAN_POINT('Ctrl Pts',(-5.13798570851046,4.81939092085927,
-5.36796555001529));
#154308=CARTESIAN_POINT('Ctrl Pts',(-5.07183159928317,4.80491309562667,
-5.45132635462913));
#154309=CARTESIAN_POINT('Ctrl Pts',(-5.00393303326813,4.79041128770499,
-5.53328395155443));
#154310=CARTESIAN_POINT('Ctrl Pts',(-4.86433680581298,4.76128647699594,
-5.69476086848324));
#154311=CARTESIAN_POINT('Ctrl Pts',(-4.79263427810061,4.74666639459734,
-5.77424575029438));
#154312=CARTESIAN_POINT('Ctrl Pts',(-4.71928195522053,4.73203683302225,
-5.85219172679468));
#154313=CARTESIAN_POINT('Ctrl Pts',(-4.55025510313446,4.69005394736987,
-5.64426066962907));
#154314=CARTESIAN_POINT('Ctrl Pts',(-4.57699618710132,4.69707706863428,
-5.67721279719471));
#154315=CARTESIAN_POINT('Ctrl Pts',(-4.60378960046422,4.70392124753795,
-5.71019592079278));
#154316=CARTESIAN_POINT('Ctrl Pts',(-4.66006860578606,4.71792585992939,
-5.77941228229491));
#154317=CARTESIAN_POINT('Ctrl Pts',(-4.68959837815049,4.72506040966796,
-5.81569350156484));
#154318=CARTESIAN_POINT('Ctrl Pts',(-4.71914125564104,4.73200281466116,
-5.8519573791549));
#154319=CARTESIAN_POINT('Origin',(-1.53089346754953E-13,4.93907429999875,
-2.01661604082304E-13));
#154320=CARTESIAN_POINT('',(-4.5943452367228,4.93794662024679,-5.68841950581731));
#154321=CARTESIAN_POINT('Ctrl Pts',(-4.59434523707343,4.93794661918462,
-5.68841950689947));
#154322=CARTESIAN_POINT('Ctrl Pts',(-4.68717264971606,4.91814186448087,
-5.63890351089828));
#154323=CARTESIAN_POINT('Ctrl Pts',(-4.77892836507603,4.89834552794767,
-5.58742753507463));
#154324=CARTESIAN_POINT('Ctrl Pts',(-4.91473914215364,4.86872423031433,
-5.5073789738014));
#154325=CARTESIAN_POINT('Ctrl Pts',(-4.9596250237364,4.85888055795239,-5.48027544686202));
#154326=CARTESIAN_POINT('Ctrl Pts',(-5.05313722302055,4.8382614706992,-5.42244078465439));
#154327=CARTESIAN_POINT('Ctrl Pts',(-5.0978486212441,4.82833849615031,-5.39399735769675));
#154328=CARTESIAN_POINT('Ctrl Pts',(-5.13798571334812,4.81939092001646,
-5.36796554655156));
#154329=CARTESIAN_POINT('',(-4.16424167158184,4.81939091970267,-6.15410778547649));
#154330=CARTESIAN_POINT('Ctrl Pts',(-4.16424166989983,4.81939091995633,
-6.15410778383816));
#154331=CARTESIAN_POINT('Ctrl Pts',(-4.19922416010835,4.82837891178309,
-6.11958420957116));
#154332=CARTESIAN_POINT('Ctrl Pts',(-4.23651301091994,4.83808521293132,
-6.08207158245674));
#154333=CARTESIAN_POINT('Ctrl Pts',(-4.31288469475123,4.85839508127127,
-6.00312655673912));
#154334=CARTESIAN_POINT('Ctrl Pts',(-4.3490609546311,4.86818863438469,-5.96485399891931));
#154335=CARTESIAN_POINT('Ctrl Pts',(-4.45649811260519,4.89780165987256,
-5.84852346342451));
#154336=CARTESIAN_POINT('Ctrl Pts',(-4.52636242450352,4.91777478489387,
-5.76925637902194));
#154337=CARTESIAN_POINT('Ctrl Pts',(-4.59434523579166,4.9379466212469,-5.6884195052838));
#154338=CARTESIAN_POINT('Ctrl Pts',(-4.71925420797629,4.7320509931407,-5.8521959118125));
#154339=CARTESIAN_POINT('Ctrl Pts',(-4.62863562367905,4.746626331206,-5.90654738803205));
#154340=CARTESIAN_POINT('Ctrl Pts',(-4.53688348514562,4.76121922803168,
-5.95898291901078));
#154341=CARTESIAN_POINT('Ctrl Pts',(-4.35180682815207,4.79033919897972,
-6.05963141031581));
#154342=CARTESIAN_POINT('Ctrl Pts',(-4.25851504799658,4.80486306098252,
-6.10785797814731));
#154343=CARTESIAN_POINT('Ctrl Pts',(-4.16424167386614,4.81939092104639,
-6.15410777983815));
#154344=CARTESIAN_POINT('Ctrl Pts',(-4.28304990569923,4.819390921,-6.17999387708313));
#154345=CARTESIAN_POINT('Ctrl Pts',(-4.61793359871535,4.754503495,-5.94790245508186));
#154346=CARTESIAN_POINT('Ctrl Pts',(-4.92577669870553,4.689276009,-5.68098272644485));
#154347=CARTESIAN_POINT('Ctrl Pts',(-4.257512905,4.819390921,-6.17442984100001));
#154348=CARTESIAN_POINT('Ctrl Pts',(-4.592095092,4.754503495,-5.943722227));
#154349=CARTESIAN_POINT('Ctrl Pts',(-4.899787985,4.689276009,-5.67821078400001));
#154350=CARTESIAN_POINT('Ctrl Pts',(-3.917638724,4.819390921,-6.100377597));
#154351=CARTESIAN_POINT('Ctrl Pts',(-4.248208141,4.754503495,-5.88808720500001));
#154352=CARTESIAN_POINT('Ctrl Pts',(-4.553901916,4.689276009,-5.64131875900001));
#154353=CARTESIAN_POINT('',(-4.04043957907225,4.81939091791743,-6.1271336267888));
#154354=CARTESIAN_POINT('Ctrl Pts',(-3.10710412312025,4.689268254,-6.84713308652525));
#154355=CARTESIAN_POINT('Ctrl Pts',(-3.48302567743148,4.754934719,-6.67654674054884));
#154356=CARTESIAN_POINT('Ctrl Pts',(-3.8380130251523,4.819390921,-6.4658320075701));
#154357=CARTESIAN_POINT('Ctrl Pts',(-3.115444452,4.689268254,-6.822316752));
#154358=CARTESIAN_POINT('Ctrl Pts',(-3.490003539,4.754934719,-6.651272505));
#154359=CARTESIAN_POINT('Ctrl Pts',(-3.84358648,4.819390921,-6.440251778));
#154360=CARTESIAN_POINT('Ctrl Pts',(-3.226259034,4.689268254,-6.492592136));
#154361=CARTESIAN_POINT('Ctrl Pts',(-3.582715568,4.754934719,-6.315463943));
#154362=CARTESIAN_POINT('Ctrl Pts',(-3.917638724,4.819390921,-6.100377597));
#154363=CARTESIAN_POINT('',(-3.86390854667387,4.81939091970075,-6.34698054757804));
#154364=CARTESIAN_POINT('',(-3.89088271932647,4.81939091820872,-6.22317845909021));
#154365=CARTESIAN_POINT('',(-3.35085601772043,4.73201982388317,-6.72974729825321));
#154366=CARTESIAN_POINT('Ctrl Pts',(-3.86390854051543,4.81939092087177,
-6.34698054805234));
#154367=CARTESIAN_POINT('Ctrl Pts',(-3.78138097004906,4.8049130958697,-6.41417124432607));
#154368=CARTESIAN_POINT('Ctrl Pts',(-3.69745137556109,4.79041128819257,
-6.47961653253445));
#154369=CARTESIAN_POINT('Ctrl Pts',(-3.52640606383257,4.76128647705211,
-6.60730914834069));
#154370=CARTESIAN_POINT('Ctrl Pts',(-3.43929300122602,4.74666639464369,
-6.66952179391214));
#154371=CARTESIAN_POINT('Ctrl Pts',(-3.35089953388808,4.73203683306755,
-6.72987685571895));
#154372=CARTESIAN_POINT('Ctrl Pts',(-3.23052346702925,4.69005394743846,
-6.49047133482806));
#154373=CARTESIAN_POINT('Ctrl Pts',(-3.24955562586843,4.69707706873026,
-6.5284016026402));
#154374=CARTESIAN_POINT('Ctrl Pts',(-3.26863222727741,4.70392124758219,
-6.56637339066714));
#154375=CARTESIAN_POINT('Ctrl Pts',(-3.30871598892618,4.71792585998442,
-6.64606983462008));
#154376=CARTESIAN_POINT('Ctrl Pts',(-3.32975598189518,4.7250604097162,-6.68785084722996));
#154377=CARTESIAN_POINT('Ctrl Pts',(-3.35081250155278,4.73200281469878,
-6.72961774078747));
#154378=CARTESIAN_POINT('Origin',(-4.77048955893622E-15,4.93907430000053,
7.80625564189564E-15));
#154379=CARTESIAN_POINT('',(-3.26408995174312,4.93794662025481,-6.54307583749208));
#154380=CARTESIAN_POINT('Ctrl Pts',(-3.26408995181825,4.93794661952797,
-6.54307583826685));
#154381=CARTESIAN_POINT('Ctrl Pts',(-3.36539158685823,4.9181418646899,-6.51467264853357));
#154382=CARTESIAN_POINT('Ctrl Pts',(-3.46606791803756,4.89834552807624,
-6.48412491890387));
#154383=CARTESIAN_POINT('Ctrl Pts',(-3.61591158944693,4.86872423035731,
-6.43514315094611));
#154384=CARTESIAN_POINT('Ctrl Pts',(-3.66557452130607,4.85888055797118,
-6.41832242708623));
#154385=CARTESIAN_POINT('Ctrl Pts',(-3.76933320020153,4.83826147070826,
-6.38194226575869));
#154386=CARTESIAN_POINT('Ctrl Pts',(-3.81911376685812,4.82833849615013,
-6.36377545925099));
#154387=CARTESIAN_POINT('Ctrl Pts',(-3.86390854603416,4.81939092000138,
-6.34698054571165));
#154388=CARTESIAN_POINT('',(-2.74393275536061,4.81939091966315,-6.90541703078901));
#154389=CARTESIAN_POINT('Ctrl Pts',(-2.74393275405512,4.81939091994474,
-6.90541702881319));
#154390=CARTESIAN_POINT('Ctrl Pts',(-2.78551901199698,4.82837892998224,
-6.8792207421115));
#154391=CARTESIAN_POINT('Ctrl Pts',(-2.83000021338486,4.83808524130702,
-6.85060111088975));
#154392=CARTESIAN_POINT('Ctrl Pts',(-2.92155708880109,4.85839508127528,
-6.78991951522507));
#154393=CARTESIAN_POINT('Ctrl Pts',(-2.9651150362015,4.86818863433114,-6.76031857521332));
#154394=CARTESIAN_POINT('Ctrl Pts',(-3.09504799913575,4.89780165970208,
-6.66980359646244));
#154395=CARTESIAN_POINT('Ctrl Pts',(-3.18031900209256,4.91777478466184,
-6.60740849449519));
#154396=CARTESIAN_POINT('Ctrl Pts',(-3.2640899512144,4.93794662092021,-6.54307583701224));
#154397=CARTESIAN_POINT('Ctrl Pts',(-3.35087153571166,4.7320509931687,-6.72987497807152));
#154398=CARTESIAN_POINT('Ctrl Pts',(-3.25068760284654,4.74662633121048,
-6.7634754300197));
#154399=CARTESIAN_POINT('Ctrl Pts',(-3.14980848920595,4.76121922802042,
-6.79496104980241));
#154400=CARTESIAN_POINT('Ctrl Pts',(-2.94742237247686,4.79033919877432,
-6.85347042449631));
#154401=CARTESIAN_POINT('Ctrl Pts',(-2.8459444151631,4.80486306087506,-6.88051450712535));
#154402=CARTESIAN_POINT('Ctrl Pts',(-2.74393275928622,4.81939092104137,
-6.90541702555452));
#154403=CARTESIAN_POINT('Ctrl Pts',(-2.85439857559013,4.819390921,-6.95623817828906));
#154404=CARTESIAN_POINT('Ctrl Pts',(-3.23134566830383,4.754503495,-6.80156301980523));
#154405=CARTESIAN_POINT('Ctrl Pts',(-3.58937141931755,4.689276009,-6.6070608921574));
#154406=CARTESIAN_POINT('Ctrl Pts',(-2.830654719,4.819390921,-6.945314526));
#154407=CARTESIAN_POINT('Ctrl Pts',(-3.207009877,4.754503495,-6.791926008));
#154408=CARTESIAN_POINT('Ctrl Pts',(-3.564586193,4.689276009,-6.598766951));
#154409=CARTESIAN_POINT('Ctrl Pts',(-2.51464565,4.819390921,-6.79993068));
#154410=CARTESIAN_POINT('Ctrl Pts',(-2.883122697,4.754503495,-6.663666173));
#154411=CARTESIAN_POINT('Ctrl Pts',(-3.234717443,4.689276009,-6.488382161));
#154412=CARTESIAN_POINT('',(-2.62997704800503,4.81939091791719,-6.85299031890594));
#154413=CARTESIAN_POINT('Ctrl Pts',(-1.5625305423085,4.689268254,-7.35498646080462));
#154414=CARTESIAN_POINT('Ctrl Pts',(-1.96633428062159,4.754934719,-7.26920035157733));
#154415=CARTESIAN_POINT('Ctrl Pts',(-2.35831966042307,4.819390921,-7.13972379752685));
#154416=CARTESIAN_POINT('Ctrl Pts',(-1.576010657,4.689268254,-7.332543243));
#154417=CARTESIAN_POINT('Ctrl Pts',(-1.978582217,4.754934719,-7.246017048));
#154418=CARTESIAN_POINT('Ctrl Pts',(-2.369261804,4.819390921,-7.115939748));
#154419=CARTESIAN_POINT('Ctrl Pts',(-1.755115501,4.689268254,-7.034349265));
#154420=CARTESIAN_POINT('Ctrl Pts',(-2.141315605,4.754934719,-6.937989849));
#154421=CARTESIAN_POINT('Ctrl Pts',(-2.51464565,4.819390921,-6.79993068000001));
#154422=CARTESIAN_POINT('',(-2.40915930973851,4.81939091976617,-7.02921779085296));
#154423=CARTESIAN_POINT('',(-2.46211663093204,4.81939091820872,-6.91410877610072));
#154424=CARTESIAN_POINT('',(-1.82581812686482,4.73201982382574,-7.29274453948536));
#154425=CARTESIAN_POINT('Ctrl Pts',(-2.40915930329185,4.81939092085653,
-7.02921778994019));
#154426=CARTESIAN_POINT('Ctrl Pts',(-2.31411716591817,4.80491309552321,
-7.07709661798109));
#154427=CARTESIAN_POINT('Ctrl Pts',(-2.21808099413988,4.7904112875162,-7.12296945072462));
#154428=CARTESIAN_POINT('Ctrl Pts',(-2.02358449302411,4.76128647696444,
-7.21090699632491));
#154429=CARTESIAN_POINT('Ctrl Pts',(-1.92513420577956,4.74666639456743,
-7.25293841133325));
#154430=CARTESIAN_POINT('Ctrl Pts',(-1.8258327745597,4.73203683300157,-7.2928804226923));
#154431=CARTESIAN_POINT('Ctrl Pts',(-1.75973614394115,4.69005394753977,
-7.03319477416654));
#154432=CARTESIAN_POINT('Ctrl Pts',(-1.77016945516759,4.69707706885708,
-7.0743296052304));
#154433=CARTESIAN_POINT('Ctrl Pts',(-1.78063724402955,4.7039212475672,-7.11551453859287));
#154434=CARTESIAN_POINT('Ctrl Pts',(-1.80265148994025,4.71792585997664,
-7.20196454805052));
#154435=CARTESIAN_POINT('Ctrl Pts',(-1.814217896818,4.72506040968594,-7.24729172026223));
#154436=CARTESIAN_POINT('Ctrl Pts',(-1.82580347916994,4.73200281464992,
-7.29260865627842));
#154437=CARTESIAN_POINT('Origin',(6.25584653524136E-14,4.93907430000036,
6.55291793050239E-13));
#154438=CARTESIAN_POINT('',(-1.7812094499623,4.93794662024309,-7.09178521416007));
#154439=CARTESIAN_POINT('Ctrl Pts',(-1.78120944984785,4.93794661935037,
-7.09178521510926));
#154440=CARTESIAN_POINT('Ctrl Pts',(-1.88624855505386,4.91814186459227,
-7.08582293318277));
#154441=CARTESIAN_POINT('Ctrl Pts',(-1.99113798834326,4.89834552802905,
-7.07763182769846));
#154442=CARTESIAN_POINT('Ctrl Pts',(-2.14800803001082,4.86872423039614,
-7.06200718622492));
#154443=CARTESIAN_POINT('Ctrl Pts',(-2.20012582844497,4.85888055804361,
-7.05625578385709));
#154444=CARTESIAN_POINT('Ctrl Pts',(-2.30927934629833,4.83826147084028,
-7.04303121932758));
#154445=CARTESIAN_POINT('Ctrl Pts',(-2.36180139727908,4.82833849632546,
-7.03599049297186));
#154446=CARTESIAN_POINT('Ctrl Pts',(-2.40915930948499,4.81939092018277,
-7.02921778852983));
#154447=CARTESIAN_POINT('',(-1.19532059297275,4.81939091961768,-7.33383665019445));
#154448=CARTESIAN_POINT('Ctrl Pts',(-1.19532059224552,4.81939091984225,
-7.33383664829511));
#154449=CARTESIAN_POINT('Ctrl Pts',(-1.24156587632055,4.82837890505971,
-7.3171926799642));
#154450=CARTESIAN_POINT('Ctrl Pts',(-1.29115944652801,4.83808520204432,
-7.29880433204201));
#154451=CARTESIAN_POINT('Ctrl Pts',(-1.393620720796,4.85839508137039,-7.25922338349757));
#154452=CARTESIAN_POINT('Ctrl Pts',(-1.44252363468209,4.86818863443235,
-7.23967816813496));
#154453=CARTESIAN_POINT('Ctrl Pts',(-1.58887688197419,4.89780165982057,
-7.1792111255017));
#154454=CARTESIAN_POINT('Ctrl Pts',(-1.68556739885766,4.91777478478944,
-7.13660553136001));
#154455=CARTESIAN_POINT('Ctrl Pts',(-1.78120944944539,4.93794662107547,
-7.09178521343167));
#154456=CARTESIAN_POINT('Ctrl Pts',(-1.82580583459438,4.73205099314127,
-7.29287257012552));
#154457=CARTESIAN_POINT('Ctrl Pts',(-1.72074104247871,4.74662633119089,
-7.30415087801442));
#154458=CARTESIAN_POINT('Ctrl Pts',(-1.61545194892915,4.76121922800212,
-7.31321435402907));
#154459=CARTESIAN_POINT('Ctrl Pts',(-1.40521972391614,4.79033919836613,
-7.32684877926749));
#154460=CARTESIAN_POINT('Ctrl Pts',(-1.30030058497591,4.80486306067414,
-7.33144582527584));
#154461=CARTESIAN_POINT('Ctrl Pts',(-1.19532059816352,4.81939092102958,
-7.33383664612755));
#154462=CARTESIAN_POINT('Ctrl Pts',(-1.29227873911615,4.819390921,-7.40721651375988));
#154463=CARTESIAN_POINT('Ctrl Pts',(-1.6936636054524,4.754503495,-7.33719005668571));
#154464=CARTESIAN_POINT('Ctrl Pts',(-2.08513112145502,4.689276009,-7.22420023456691));
#154465=CARTESIAN_POINT('Ctrl Pts',(-1.271438263,4.819390921,-7.391444023));
#154466=CARTESIAN_POINT('Ctrl Pts',(-1.671968444,4.754503495,-7.32254687700001));
#154467=CARTESIAN_POINT('Ctrl Pts',(-2.062708312,4.689276009,-7.21077211));
#154468=CARTESIAN_POINT('Ctrl Pts',(-0.994070541,4.819390921,-7.181526562));
#154469=CARTESIAN_POINT('Ctrl Pts',(-1.38322564,4.754503495,-7.127659516));
#154470=CARTESIAN_POINT('Ctrl Pts',(-1.764281177,4.689276009,-7.03205602400001));
#154471=CARTESIAN_POINT('',(-1.09428701315445,4.81939091791739,-7.25737241764825));
#154472=CARTESIAN_POINT('Ctrl Pts',(0.0551052307094634,4.689268254,-7.5189288428372));
#154473=CARTESIAN_POINT('Ctrl Pts',(-0.35769927843588,4.754934719,-7.5219542327515));
#154474=CARTESIAN_POINT('Ctrl Pts',(-0.768353889884251,4.819390921,-7.47977003953121));
#154475=CARTESIAN_POINT('Ctrl Pts',(0.037115645,4.689268254,-7.499908161));
#154476=CARTESIAN_POINT('Ctrl Pts',(-0.37464459,4.754934719,-7.501945886));
#154477=CARTESIAN_POINT('Ctrl Pts',(-0.78415308,4.819390921,-7.458894285));
#154478=CARTESIAN_POINT('Ctrl Pts',(-0.201904718,4.689268254,-7.24718804));
#154479=CARTESIAN_POINT('Ctrl Pts',(-0.599790104,4.754934719,-7.23610306));
#154480=CARTESIAN_POINT('Ctrl Pts',(-0.994070541000001,4.819390921,-7.18152656200001));
#154481=CARTESIAN_POINT('',(-0.918224705199005,4.81939091820872,-7.28174305106958));
#154482=CARTESIAN_POINT('Ctrl Pts',(-0.206665514464669,4.6900539473239,
-7.24705384062151));
#154483=CARTESIAN_POINT('Ctrl Pts',(-0.208012127751941,4.69707706859336,
-7.28946981548055));
#154484=CARTESIAN_POINT('Ctrl Pts',(-0.209381642204492,4.70392124749239,
-7.33194213439115));
#154485=CARTESIAN_POINT('Ctrl Pts',(-0.212297010587137,4.71792585990076,
-7.42110340287249));
#154486=CARTESIAN_POINT('Ctrl Pts',(-0.213848999159561,4.72506040965179,
-7.4678572868583));
#154487=CARTESIAN_POINT('Ctrl Pts',(-0.215421915432243,4.73200281465868,
-7.51460529612207));
#154488=CARTESIAN_POINT('Ctrl Pts',(0.33026661393265,4.819390921,-7.51184163683667));
#154489=CARTESIAN_POINT('Ctrl Pts',(-0.0767877158185115,4.754503495,-7.52973824160898));
#154490=CARTESIAN_POINT('Ctrl Pts',(-0.483392409605453,4.689276009,-7.50354400259746));
#154491=CARTESIAN_POINT('Ctrl Pts',(0.347229232,4.819390921,-7.491957812));
#154492=CARTESIAN_POINT('Ctrl Pts',(-0.0587476260000001,4.754503495,-7.510773593));
#154493=CARTESIAN_POINT('Ctrl Pts',(-0.464380483,4.689276009,-7.485609579));
#154494=CARTESIAN_POINT('Ctrl Pts',(0.572986203,4.819390921,-7.227322244));
#154495=CARTESIAN_POINT('Ctrl Pts',(0.181349511,4.754503495,-7.25837142200001));
#154496=CARTESIAN_POINT('Ctrl Pts',(-0.211349085,4.689276009,-7.24691876300001));
#154497=CARTESIAN_POINT('',(0.490593424731472,4.8193909179172,-7.32390426471178));
#154498=CARTESIAN_POINT('Ctrl Pts',(1.67016434457945,4.689268254,-7.33129446975108));
#154499=CARTESIAN_POINT('Ctrl Pts',(1.26766134467495,4.754934719,-7.4229898936172));
#154500=CARTESIAN_POINT('Ctrl Pts',(0.857539254896607,4.819390921,-7.47007054607416));
#154501=CARTESIAN_POINT('Ctrl Pts',(1.648506461,4.689268254,-7.31658571));
#154502=CARTESIAN_POINT('Ctrl Pts',(1.246811002,4.754934719,-7.407092072));
#154503=CARTESIAN_POINT('Ctrl Pts',(0.837621771,4.819390921,-7.453079214));
#154504=CARTESIAN_POINT('Ctrl Pts',(1.360746905,4.689268254,-7.121156357));
#154505=CARTESIAN_POINT('Ctrl Pts',(0.969780916,4.754934719,-7.195864134));
#154506=CARTESIAN_POINT('Ctrl Pts',(0.572986203,4.819390921,-7.227322244));
#154507=CARTESIAN_POINT('',(0.764998170628619,4.81939091971407,-7.39112502452024));
#154508=CARTESIAN_POINT('',(0.668602387742703,4.81939091820872,-7.30889111458854));
#154509=CARTESIAN_POINT('',(1.40507629994002,4.73201982382458,-7.38535681886841));
#154510=CARTESIAN_POINT('Ctrl Pts',(0.764998175836196,4.81939092085866,
-7.39112502113075));
#154511=CARTESIAN_POINT('Ctrl Pts',(0.871359881258293,4.80491309562033,
-7.39467151086817));
#154512=CARTESIAN_POINT('Ctrl Pts',(0.977781452401426,4.79041128768559,
-7.3959800244164));
#154513=CARTESIAN_POINT('Ctrl Pts',(1.19122571432888,4.7612864770025,-7.39412301811676));
#154514=CARTESIAN_POINT('Ctrl Pts',(1.29822530834739,4.7466663945937,-7.39093149455899));
#154515=CARTESIAN_POINT('Ctrl Pts',(1.4051200618959,4.73203683300444,-7.38548629353271));
#154516=CARTESIAN_POINT('Ctrl Pts',(1.35606856510726,4.69005394731185,-7.12204872604118));
#154517=CARTESIAN_POINT('Ctrl Pts',(1.36387161560206,4.69707706857266,-7.16376252089336));
#154518=CARTESIAN_POINT('Ctrl Pts',(1.3716644127257,4.70392124750565,-7.20553626584865));
#154519=CARTESIAN_POINT('Ctrl Pts',(1.38798424111399,4.71792585989974,-7.29323971123585));
#154520=CARTESIAN_POINT('Ctrl Pts',(1.39651924019486,4.72506040964578,-7.33923414698756));
#154521=CARTESIAN_POINT('Ctrl Pts',(1.40503253798415,4.73200281464471,-7.3852273442041));
#154522=CARTESIAN_POINT('Origin',(1.3389896830196E-14,4.93907429999875,
-4.15032591627451E-13));
#154523=CARTESIAN_POINT('',(1.361181406915,4.93794662024243,-7.18424037779173));
#154524=CARTESIAN_POINT('Ctrl Pts',(1.36118140755056,4.93794661911314,-7.18424037882069));
#154525=CARTESIAN_POINT('Ctrl Pts',(1.26334700045149,4.91814186435326,-7.22293393378318));
#154526=CARTESIAN_POINT('Ctrl Pts',(1.16471257319447,4.89834552781051,-7.25954181764329));
#154527=CARTESIAN_POINT('Ctrl Pts',(1.0157805627591,4.86872423021828,-7.31122929788308));
#154528=CARTESIAN_POINT('Ctrl Pts',(0.966064778855809,4.85888055788355,
-7.32789316199559));
#154529=CARTESIAN_POINT('Ctrl Pts',(0.861446878623905,4.838261470707,-7.36172324479444));
#154530=CARTESIAN_POINT('Ctrl Pts',(0.810822831831353,4.82833849618497,
-7.37738669142729));
#154531=CARTESIAN_POINT('Ctrl Pts',(0.764998169975832,4.81939092004315,
-7.39112502255717));
#154532=CARTESIAN_POINT('',(1.9945544934734,4.81939091960363,-7.15791196534276));
#154533=CARTESIAN_POINT('Ctrl Pts',(1.99455449333891,4.81939091980167,-7.15791196340296));
#154534=CARTESIAN_POINT('Ctrl Pts',(1.94559476297443,4.82837890968501,-7.1622242001431));
#154535=CARTESIAN_POINT('Ctrl Pts',(1.89286378000787,4.83808520897093,-7.16635918701156));
#154536=CARTESIAN_POINT('Ctrl Pts',(1.78325287452173,4.85839508130526,-7.17345886106996));
#154537=CARTESIAN_POINT('Ctrl Pts',(1.73066296862473,4.86818863442145,-7.17625390465097));
#154538=CARTESIAN_POINT('Ctrl Pts',(1.5724469059283,4.89780165990501,-7.18282763662407));
#154539=CARTESIAN_POINT('Ctrl Pts',(1.46680334461262,4.91777478493161,-7.18475914088505));
#154540=CARTESIAN_POINT('Ctrl Pts',(1.36118140712162,4.93794662129573,-7.18424037668054));
#154541=CARTESIAN_POINT('Ctrl Pts',(1.40514121474242,4.73205099312586,-7.38546785495625));
#154542=CARTESIAN_POINT('Ctrl Pts',(1.50523107615726,4.74662633118788,-7.35158820878161));
#154543=CARTESIAN_POINT('Ctrl Pts',(1.60459452427703,4.76121922800804,-7.31560425391225));
#154544=CARTESIAN_POINT('Ctrl Pts',(1.80112107278766,4.79033919867926,-7.23970430222656));
#154545=CARTESIAN_POINT('Ctrl Pts',(1.89827335282728,4.80486306083143,-7.19982206555386));
#154546=CARTESIAN_POINT('Ctrl Pts',(1.99455448709657,4.81939092103824,-7.15791196385871));
#154547=CARTESIAN_POINT('Ctrl Pts',(1.93736906818931,4.819390921,-7.26522139449432));
#154548=CARTESIAN_POINT('Ctrl Pts',(1.54367868338508,4.754503495,-7.37020423461234));
#154549=CARTESIAN_POINT('Ctrl Pts',(1.14094919361909,4.689276009,-7.43203039289954));
#154550=CARTESIAN_POINT('Ctrl Pts',(1.949660675,4.819390921,-7.242155981));
#154551=CARTESIAN_POINT('Ctrl Pts',(1.557220167,4.754503495,-7.34780488300001));
#154552=CARTESIAN_POINT('Ctrl Pts',(1.155661261,4.689276009,-7.410428264));
#154553=CARTESIAN_POINT('Ctrl Pts',(2.113250748,4.819390921,-6.93517637));
#154554=CARTESIAN_POINT('Ctrl Pts',(1.73744496,4.754503495,-7.04968994800001));
#154555=CARTESIAN_POINT('Ctrl Pts',(1.351465456,4.689276009,-7.122923636));
#154556=CARTESIAN_POINT('',(2.05354654700379,4.81939091791738,-7.04721236860803));
#154557=CARTESIAN_POINT('Ctrl Pts',(3.20712842978384,4.689268254,-6.80085691434977));
#154558=CARTESIAN_POINT('Ctrl Pts',(2.83374753197936,4.754934719,-6.97693479805095));
#154559=CARTESIAN_POINT('Ctrl Pts',(2.44333481731984,4.819390921,-7.11107885687941));
#154560=CARTESIAN_POINT('Ctrl Pts',(3.182814947,4.689268254,-6.79114784200001));
#154561=CARTESIAN_POINT('Ctrl Pts',(2.809967097,4.754934719,-6.965890866));
#154562=CARTESIAN_POINT('Ctrl Pts',(2.420230359,4.819390921,-7.098766443));
#154563=CARTESIAN_POINT('Ctrl Pts',(2.859771516,4.689268254,-6.662147317));
#154564=CARTESIAN_POINT('Ctrl Pts',(2.494006057,4.754934719,-6.819154599));
#154565=CARTESIAN_POINT('Ctrl Pts',(2.113250748,4.819390921,-6.93517637));
#154566=CARTESIAN_POINT('',(2.33598633845085,4.81939091972229,-7.0538726353531));
#154567=CARTESIAN_POINT('',(2.22416637565606,4.81939091820872,-6.99428355248962));
#154568=CARTESIAN_POINT('',(2.95985980325624,4.73201982382998,-6.91064140985388));
#154569=CARTESIAN_POINT('Ctrl Pts',(2.33598634279356,4.81939092086852,-7.05387263091369));
#154570=CARTESIAN_POINT('Ctrl Pts',(2.44062375986601,4.80491309579386,-7.03447158329896));
#154571=CARTESIAN_POINT('Ctrl Pts',(2.54483854424275,4.79041128804214,-7.0128720128882));
#154572=CARTESIAN_POINT('Ctrl Pts',(2.75289339897587,4.76128647701724,-6.96517421484957));
#154573=CARTESIAN_POINT('Ctrl Pts',(2.85670531885606,4.74666639459917,-6.93905555747064));
#154574=CARTESIAN_POINT('Ctrl Pts',(2.95993037533596,4.73203683300646,-6.91075844994129));
#154575=CARTESIAN_POINT('Ctrl Pts',(2.85539438564915,4.69005394748178,-6.66402452836791));
#154576=CARTESIAN_POINT('Ctrl Pts',(2.87198223804774,4.69707706875983,-6.70308565294994));
#154577=CARTESIAN_POINT('Ctrl Pts',(2.88857296395198,4.70392124756544,-6.74220752936085));
#154578=CARTESIAN_POINT('Ctrl Pts',(2.92336489211045,4.71792585995299,-6.82435223648));
#154579=CARTESIAN_POINT('Ctrl Pts',(2.94158779172578,4.72506040967516,-6.86743657534881));
#154580=CARTESIAN_POINT('Ctrl Pts',(2.95978923117651,4.73200281465349,-6.91052436976648));
#154581=CARTESIAN_POINT('Origin',(6.13658429626796E-14,4.93907429999947,
-3.72098185597025E-13));
#154582=CARTESIAN_POINT('',(2.87375706009855,4.93794662024794,-6.72366306323252));
#154583=CARTESIAN_POINT('Ctrl Pts',(2.87375706070915,4.9379466194289,-6.72366306386225));
#154584=CARTESIAN_POINT('Ctrl Pts',(2.78652793794651,4.91814186461107,-6.78248349077825));
#154585=CARTESIAN_POINT('Ctrl Pts',(2.69806914139962,4.89834552800437,-6.83943898910689));
#154586=CARTESIAN_POINT('Ctrl Pts',(2.56373035855149,4.86872423031914,-6.92193402490032));
#154587=CARTESIAN_POINT('Ctrl Pts',(2.51875914010647,4.85888055795341,-6.94889572116907));
#154588=CARTESIAN_POINT('Ctrl Pts',(2.42385961591318,4.83826147075346,-7.00442463156618));
#154589=CARTESIAN_POINT('Ctrl Pts',(2.3777863091507,4.82833849621868,-7.03060454918325));
#154590=CARTESIAN_POINT('Ctrl Pts',(2.33598633738469,4.81939092005231,-7.0538726335647));
#154591=CARTESIAN_POINT('',(3.4866624037102,4.8193909195952,-6.56179370394099));
#154592=CARTESIAN_POINT('Ctrl Pts',(3.48666240317772,4.8193909197725,-6.56179370213862));
#154593=CARTESIAN_POINT('Ctrl Pts',(3.43977429249229,4.82837891588597,-6.57653002753051));
#154594=CARTESIAN_POINT('Ctrl Pts',(3.38916501125661,4.83808521941846,-6.59190394743572));
#154595=CARTESIAN_POINT('Ctrl Pts',(3.28364302290187,4.85839508118745,-6.62240072374302));
#154596=CARTESIAN_POINT('Ctrl Pts',(3.23288349162489,4.86818863429477,-6.63643569594599));
#154597=CARTESIAN_POINT('Ctrl Pts',(3.07977959098872,4.89780165972668,-6.67686751425433));
#154598=CARTESIAN_POINT('Ctrl Pts',(2.97702113403897,4.91777478470248,-6.70146410384215));
#154599=CARTESIAN_POINT('Ctrl Pts',(2.87375706007209,4.93794662099952,-6.72366306242647));
#154600=CARTESIAN_POINT('Ctrl Pts',(2.95994706988585,4.73205099314337,-6.91073589519746));
#154601=CARTESIAN_POINT('Ctrl Pts',(3.05041376349921,4.74662633121276,-6.8561319747512));
#154602=CARTESIAN_POINT('Ctrl Pts',(3.13971866278778,4.76121922803844,-6.79962910056749));
#154603=CARTESIAN_POINT('Ctrl Pts',(3.31533428564133,4.79033919902709,-6.68325624768655));
#154604=CARTESIAN_POINT('Ctrl Pts',(3.40164169634223,4.80486306101155,-6.62342156777488));
#154605=CARTESIAN_POINT('Ctrl Pts',(3.4866623972128,4.81939092104663,-6.56179370386531));
#154606=CARTESIAN_POINT('Ctrl Pts',(3.45388229713187,4.819390921,-6.67888747440437));
#154607=CARTESIAN_POINT('Ctrl Pts',(3.09196438218115,4.754503495,-6.86604766914545));
#154608=CARTESIAN_POINT('Ctrl Pts',(2.71194128065134,4.689276009,-7.01300330203434));
#154609=CARTESIAN_POINT('Ctrl Pts',(3.460928151,4.819390921,-6.653718985));
#154610=CARTESIAN_POINT('Ctrl Pts',(3.100374075,4.754503495,-6.841260983));
#154611=CARTESIAN_POINT('Ctrl Pts',(2.721665569,4.689276009,-6.988743559));
#154612=CARTESIAN_POINT('Ctrl Pts',(3.554702037,4.819390921,-6.318749356));
#154613=CARTESIAN_POINT('Ctrl Pts',(3.212299413,4.754503495,-6.511372807));
#154614=CARTESIAN_POINT('Ctrl Pts',(2.851086974,4.689276009,-6.665868515));
#154615=CARTESIAN_POINT('',(3.52082035429869,4.81939091791742,-6.43977814068551));
#154616=CARTESIAN_POINT('Ctrl Pts',(4.59413075429447,4.689268254,-5.95241884841558));
#154617=CARTESIAN_POINT('Ctrl Pts',(4.26733083418468,4.754934719,-6.20464598542213));
#154618=CARTESIAN_POINT('Ctrl Pts',(3.91488275966786,4.819390921,-6.41958102282211));
#154619=CARTESIAN_POINT('Ctrl Pts',(4.568298544,4.689268254,-5.948163449));
#154620=CARTESIAN_POINT('Ctrl Pts',(4.241732254,4.754934719,-6.198972345));
#154621=CARTESIAN_POINT('Ctrl Pts',(3.889671666,4.819390921,-6.412523242));
#154622=CARTESIAN_POINT('Ctrl Pts',(4.225076389,4.689268254,-5.891623674));
#154623=CARTESIAN_POINT('Ctrl Pts',(3.901614248,4.754934719,-6.123588974));
#154624=CARTESIAN_POINT('Ctrl Pts',(3.554702037,4.819390921,-6.318749356));
#154625=CARTESIAN_POINT('',(3.79774638263754,4.81939091972637,-6.38678900096167));
#154626=CARTESIAN_POINT('',(3.67573081612178,4.81939091820872,-6.35263106417826));
#154627=CARTESIAN_POINT('',(4.37624355193186,4.73201982384556,-6.11279208909231));
#154628=CARTESIAN_POINT('Ctrl Pts',(3.79774638599498,4.81939092085526,-6.38678899563233));
#154629=CARTESIAN_POINT('Ctrl Pts',(3.89576678816968,4.80491309551935,-6.34534758150289));
#154630=CARTESIAN_POINT('Ctrl Pts',(3.99290182116961,4.79041128749769,-6.30184989818854));
#154631=CARTESIAN_POINT('Ctrl Pts',(4.18583884888006,4.76128647695171,-6.21054160612787));
#154632=CARTESIAN_POINT('Ctrl Pts',(4.2816089641817,4.74666639456629,-6.1627170944889));
#154633=CARTESIAN_POINT('Ctrl Pts',(4.37633763423928,4.73203683302124,-6.11289122193341));
#154634=CARTESIAN_POINT('Ctrl Pts',(4.22120513800341,4.69005394745124,-5.8943979506271));
#154635=CARTESIAN_POINT('Ctrl Pts',(4.24580216290519,4.69707706874209,-5.92897994972898));
#154636=CARTESIAN_POINT('Ctrl Pts',(4.27041505393711,4.70392124756459,-5.96362066268045));
#154637=CARTESIAN_POINT('Ctrl Pts',(4.32205225002897,4.71792585996443,-6.03636563588632));
#154638=CARTESIAN_POINT('Ctrl Pts',(4.34911096763941,4.72506040969101,-6.0745253020366));
#154639=CARTESIAN_POINT('Ctrl Pts',(4.37614946962444,4.73200281466989,-6.1126929562512));
#154640=CARTESIAN_POINT('Origin',(1.6978606021123E-13,4.93907429999947,
-5.68121938382404E-14));
#154641=CARTESIAN_POINT('',(4.2519590248966,4.93794662024346,-5.94869473742009));
#154642=CARTESIAN_POINT('Ctrl Pts',(4.25195902576348,4.9379466192731,-5.94869473799322));
#154643=CARTESIAN_POINT('Ctrl Pts',(4.1794139247583,4.9181418644975,-6.02489165867405));
#154644=CARTESIAN_POINT('Ctrl Pts',(4.1052669945485,4.89834552794473,-6.09953159527505));
#154645=CARTESIAN_POINT('Ctrl Pts',(3.99180297237013,4.86872423032577,-6.20897680991753));
#154646=CARTESIAN_POINT('Ctrl Pts',(3.95367912386868,4.85888055797775,-6.24497563923672));
#154647=CARTESIAN_POINT('Ctrl Pts',(3.87293537213586,4.83826147073724,-6.31960690711586));
#154648=CARTESIAN_POINT('Ctrl Pts',(3.83356714218467,4.82833849620036,-6.35507915179506));
#154649=CARTESIAN_POINT('Ctrl Pts',(3.79774638116995,4.81939092007985,-6.38678899940356));
#154650=CARTESIAN_POINT('',(4.81573785503565,4.8193909195985,-5.65885326212327));
#154651=CARTESIAN_POINT('Ctrl Pts',(4.81573785412003,4.81939091978043,-5.65885326046163));
#154652=CARTESIAN_POINT('Ctrl Pts',(4.77311389288525,4.82837890454499,-5.68332458283608));
#154653=CARTESIAN_POINT('Ctrl Pts',(4.72699279340066,4.83808520180399,-5.70921855673414));
#154654=CARTESIAN_POINT('Ctrl Pts',(4.63049367195276,4.85839508124016,-5.7616864892933));
#154655=CARTESIAN_POINT('Ctrl Pts',(4.58393797450878,4.86818863433821,-5.7863051303968));
#154656=CARTESIAN_POINT('Ctrl Pts',(4.44310520378661,4.89780165977954,-5.85870448813445));
#154657=CARTESIAN_POINT('Ctrl Pts',(4.3480367221006,4.91777478478945,-5.90481605383178));
#154658=CARTESIAN_POINT('Ctrl Pts',(4.25195902465804,4.9379466211439,-5.9486947364838));
#154659=CARTESIAN_POINT('Ctrl Pts',(4.37634908987473,4.7320509931612,-6.11286560566984));
#154660=CARTESIAN_POINT('Ctrl Pts',(4.45296249357072,4.74662633122668,-6.04009062964906));
#154661=CARTESIAN_POINT('Ctrl Pts',(4.52803304613346,4.76121922804461,-5.96571084781629));
#154662=CARTESIAN_POINT('Ctrl Pts',(4.67452614959537,4.7903391989875,-5.81430656012054));
#154663=CARTESIAN_POINT('Ctrl Pts',(4.74595305356124,4.80486306098948,-5.7373172396589));
#154664=CARTESIAN_POINT('Ctrl Pts',(4.81573784867121,4.8193909210453,-5.65885326343773));
#154665=CARTESIAN_POINT('Ctrl Pts',(4.80889582853022,4.819390921,-5.7802561994388));
#154666=CARTESIAN_POINT('Ctrl Pts',(4.4956732629108,4.754503495,-6.04084234557442));
#154667=CARTESIAN_POINT('Ctrl Pts',(4.15612600775738,4.689276009,-6.26605597125353));
#154668=CARTESIAN_POINT('Ctrl Pts',(4.810366473,4.819390921,-5.754161485));
#154669=CARTESIAN_POINT('Ctrl Pts',(4.498557937,4.754503495,-6.014827323));
#154670=CARTESIAN_POINT('Ctrl Pts',(4.16040782,4.689276009,-6.240272973));
#154671=CARTESIAN_POINT('Ctrl Pts',(4.829939409,4.819390921,-5.406864646));
#154672=CARTESIAN_POINT('Ctrl Pts',(4.536950317,4.754503495,-5.66859111));
#154673=CARTESIAN_POINT('Ctrl Pts',(4.217394834,4.689276009,-5.89712479200001));
#154674=CARTESIAN_POINT('',(4.82279603852955,4.81939091791738,-5.53361490783684));
#154675=CARTESIAN_POINT('Ctrl Pts',(5.76631663010193,4.689268254,-4.82565229291977));
#154676=CARTESIAN_POINT('Ctrl Pts',(5.50137849007381,4.754934719,-5.1422348217962));
#154677=CARTESIAN_POINT('Ctrl Pts',(5.20337513502365,4.819390921,-5.42791071594587));
#154678=CARTESIAN_POINT('Ctrl Pts',(5.74017357700001,4.689268254,-4.827049544));
#154679=CARTESIAN_POINT('Ctrl Pts',(5.475158725,4.754934719,-5.142196766));
#154680=CARTESIAN_POINT('Ctrl Pts',(5.177236248,4.819390921,-5.426437582));
#154681=CARTESIAN_POINT('Ctrl Pts',(5.392821385,4.689268254,-4.845614255));
#154682=CARTESIAN_POINT('Ctrl Pts',(5.126787292,4.754934719,-5.141691134));
#154683=CARTESIAN_POINT('Ctrl Pts',(4.829939409,4.819390921,-5.406864646));
#154684=CARTESIAN_POINT('',(5.08192802541004,4.81939091972029,-5.42106621189636));
#154685=CARTESIAN_POINT('',(4.95542216813492,4.81939091820872,-5.41393660870127));
#154686=CARTESIAN_POINT('',(5.58799901600127,4.73201982386544,-5.02911540404799));
#154687=CARTESIAN_POINT('Ctrl Pts',(5.08192802756682,4.81939092086455,-5.4210662059747));
#154688=CARTESIAN_POINT('Ctrl Pts',(5.16874808717188,4.80491309572286,-5.35952218075136));
#154689=CARTESIAN_POINT('Ctrl Pts',(5.25426143996334,4.79041128789788,-5.29616028910016));
#154690=CARTESIAN_POINT('Ctrl Pts',(5.42305912547235,4.76128647702865,-5.16551097479791));
#154691=CARTESIAN_POINT('Ctrl Pts',(5.50630933252438,4.74666639462265,-5.09821682969789));
#154692=CARTESIAN_POINT('Ctrl Pts',(5.58811220930506,4.73203683304752,-5.02919199433367));
#154693=CARTESIAN_POINT('Ctrl Pts',(5.38963703028743,4.69005394753149,-4.84915587539731));
#154694=CARTESIAN_POINT('Ctrl Pts',(5.42109309802439,4.69707706884286,-4.87764173344675));
#154695=CARTESIAN_POINT('Ctrl Pts',(5.45257728229003,4.7039212475901,-4.906181521479));
#154696=CARTESIAN_POINT('Ctrl Pts',(5.51864524839433,4.71792585999831,-4.96612528693495));
#154697=CARTESIAN_POINT('Ctrl Pts',(5.55327454843862,4.72506040971483,-4.99757597681861));
#154698=CARTESIAN_POINT('Ctrl Pts',(5.58788582269747,4.73200281468336,-5.02903881376231));
#154699=CARTESIAN_POINT('Origin',(2.52402265754625E-13,4.93907430000018,
-1.57859836313889E-13));
#154700=CARTESIAN_POINT('',(5.43134411168424,4.93794662030685,-4.89557205727329));
#154701=CARTESIAN_POINT('Ctrl Pts',(5.43134411273164,4.93794661925887,-4.89557205767653));
#154702=CARTESIAN_POINT('Ctrl Pts',(5.37687516145781,4.9181418644691,-4.98558258899984));
#154703=CARTESIAN_POINT('Ctrl Pts',(5.32050712531743,4.89834552788478,-5.07441688360505));
#154704=CARTESIAN_POINT('Ctrl Pts',(5.23322331493081,4.86872423024933,-5.20569474071468));
#154705=CARTESIAN_POINT('Ctrl Pts',(5.2037294650359,4.85888055790566,-5.24904743786462));
#154706=CARTESIAN_POINT('Ctrl Pts',(5.14091697406473,4.83826147074124,-5.33929138771099));
#154707=CARTESIAN_POINT('Ctrl Pts',(5.11009463552047,4.82833849622207,-5.38239731671222));
#154708=CARTESIAN_POINT('Ctrl Pts',(5.08192802368369,4.81939092006014,-5.42106621071751));
#154709=CARTESIAN_POINT('',(5.91963475744616,4.81939091962027,-4.49131113040391));
#154710=CARTESIAN_POINT('Ctrl Pts',(5.9196347561068,4.81939091985038,-4.49131112886811));
#154711=CARTESIAN_POINT('Ctrl Pts',(5.88326785870452,4.82837892128484,-4.52437328388305));
#154712=CARTESIAN_POINT('Ctrl Pts',(5.84379145345502,4.83808522668422,-4.5595765661234));
#154713=CARTESIAN_POINT('Ctrl Pts',(5.76082758369809,4.85839508134986,-4.63156219823851));
#154714=CARTESIAN_POINT('Ctrl Pts',(5.72065261291011,4.86818863441021,-4.66561336776986));
#154715=CARTESIAN_POINT('Ctrl Pts',(5.59867615593021,4.89780165987564,-4.76659495141481));
#154716=CARTESIAN_POINT('Ctrl Pts',(5.51574294592142,4.91777478493435,-4.83206536780779));
#154717=CARTESIAN_POINT('Ctrl Pts',(5.43134411120292,4.93794662130489,-4.89557205631661));
#154718=CARTESIAN_POINT('Ctrl Pts',(5.58811789039565,4.73205099315931,-5.02916451435992));
#154719=CARTESIAN_POINT('Ctrl Pts',(5.64729564669879,4.74662633121721,-4.94162135968071));
#154720=CARTESIAN_POINT('Ctrl Pts',(5.70462163705322,4.76121922803165,-4.85284258604163));
#154721=CARTESIAN_POINT('Ctrl Pts',(5.81514236548186,4.79033919860815,-4.67348636165991));
#154722=CARTESIAN_POINT('Ctrl Pts',(5.86834892079121,4.80486306079293,-4.58294233458863));
#154723=CARTESIAN_POINT('Ctrl Pts',(5.91963475136461,4.81939092103644,-4.49131113315614));
#154724=CARTESIAN_POINT('Ctrl Pts',(5.93905073662225,4.819390921,-4.61134656846007));
#154725=CARTESIAN_POINT('Ctrl Pts',(5.68916945885119,4.754503495,-4.9331739483148));
#154726=CARTESIAN_POINT('Ctrl Pts',(5.40597490160482,4.689276009,-5.22611482698729));
#154727=CARTESIAN_POINT('Ctrl Pts',(5.934877406,4.819390921,-4.585545789));
#154728=CARTESIAN_POINT('Ctrl Pts',(5.68639423,4.754503495,-4.907147023));
#154729=CARTESIAN_POINT('Ctrl Pts',(5.404614025,4.689276009,-5.200014158));
#154730=CARTESIAN_POINT('Ctrl Pts',(5.879334183,4.819390921,-4.242160954));
#154731=CARTESIAN_POINT('Ctrl Pts',(5.649458466,4.754503495,-4.560752393));
#154732=CARTESIAN_POINT('Ctrl Pts',(5.386501999,4.689276009,-4.852638067));
#154733=CARTESIAN_POINT('',(5.89960538046836,4.8193909179172,-4.36748347900853));
#154734=CARTESIAN_POINT('Ctrl Pts',(6.66887594922512,4.689268254,-3.47324360036106));
#154735=CARTESIAN_POINT('Ctrl Pts',(6.47818780120644,4.754934719,-3.83937847364755));
#154736=CARTESIAN_POINT('Ctrl Pts',(6.24856347140929,4.819390921,-4.18243733692546));
#154737=CARTESIAN_POINT('Ctrl Pts',(6.643644474,4.689268254,-3.480228168));
#154738=CARTESIAN_POINT('Ctrl Pts',(6.452572859,4.754934719,-3.844977782));
#154739=CARTESIAN_POINT('Ctrl Pts',(6.222719017,4.819390921,-4.186617732));
#154740=CARTESIAN_POINT('Ctrl Pts',(6.308404047,4.689268254,-3.573029299));
#154741=CARTESIAN_POINT('Ctrl Pts',(6.112237461,4.754934719,-3.919373532));
#154742=CARTESIAN_POINT('Ctrl Pts',(5.879334183,4.819390921,-4.242160954));
#154743=CARTESIAN_POINT('',(6.12848436209898,4.81939091971738,-4.20186039183531));
#154744=CARTESIAN_POINT('',(6.00340348775815,4.81939091820872,-4.22209249434916));
#154745=CARTESIAN_POINT('',(6.53846585632056,4.73201982386532,-3.71028287274101));
#154746=CARTESIAN_POINT('Ctrl Pts',(6.12848436286711,4.81939092087191,-4.2018603856999));
#154747=CARTESIAN_POINT('Ctrl Pts',(6.20004447082737,4.80491309586707,-4.12309147994593));
#154748=CARTESIAN_POINT('Ctrl Pts',(6.26993763454746,4.79041128819051,-4.04282811188466));
#154749=CARTESIAN_POINT('Ctrl Pts',(6.40670318462008,4.76128647705193,-3.87894679171586));
#154750=CARTESIAN_POINT('Ctrl Pts',(6.47354079612634,4.74666639463727,-3.79532961265998));
#154751=CARTESIAN_POINT('Ctrl Pts',(6.53859286789724,4.73203683304325,-3.71033333914916));
#154752=CARTESIAN_POINT('Ctrl Pts',(6.30605548406717,4.69005394743836,-3.57717266011216));
#154753=CARTESIAN_POINT('Ctrl Pts',(6.3428997435947,4.69707706869056,-3.59823040999787));
#154754=CARTESIAN_POINT('Ctrl Pts',(6.37978305655066,4.70392124755452,-3.61933478523539));
#154755=CARTESIAN_POINT('Ctrl Pts',(6.4571925278355,4.71792585994776,-3.66367443923128));
#154756=CARTESIAN_POINT('Ctrl Pts',(6.49777318281428,4.72506040968754,-3.68694555374012));
#154757=CARTESIAN_POINT('Ctrl Pts',(6.53833884474388,4.7320028146874,-3.71023240633286));
#154758=CARTESIAN_POINT('Origin',(5.41233724504764E-13,4.93907429999964,
-3.14201789586299E-13));
#154759=CARTESIAN_POINT('',(6.35676558561064,4.9379466202581,-3.61353786721423));
#154760=CARTESIAN_POINT('Ctrl Pts',(6.35676558641561,4.93794661949784,-3.61353786733658));
#154761=CARTESIAN_POINT('Ctrl Pts',(6.3229196923951,4.91814186467107,-3.71315321718136));
#154762=CARTESIAN_POINT('Ctrl Pts',(6.28696625694172,4.8983455280375,-3.8120280771608));
#154763=CARTESIAN_POINT('Ctrl Pts',(6.22994395212096,4.86872423032536,-3.95900017046747));
#154764=CARTESIAN_POINT('Ctrl Pts',(6.21045920039375,4.85888055795967,-4.00767961165742));
#154765=CARTESIAN_POINT('Ctrl Pts',(6.16851501210557,4.83826147076072,-4.10931653712138));
#154766=CARTESIAN_POINT('Ctrl Pts',(6.14767978318993,4.82833849621905,-4.15804056525908));
#154767=CARTESIAN_POINT('Ctrl Pts',(6.12848436019905,4.81939092003673,-4.20186039106825));
#154768=CARTESIAN_POINT('',(6.74673611732405,4.81939091966401,-3.11376028273081));
#154769=CARTESIAN_POINT('Ctrl Pts',(6.74673611541487,4.81939091994905,-3.11376028131458));
#154770=CARTESIAN_POINT('Ctrl Pts',(6.71832675655188,4.82837894707265,-3.15386739304371));
#154771=CARTESIAN_POINT('Ctrl Pts',(6.68734090682483,4.83808526753276,-3.19673395510896));
#154772=CARTESIAN_POINT('Ctrl Pts',(6.62179160131477,4.85839508125913,-3.28487120529323));
#154773=CARTESIAN_POINT('Ctrl Pts',(6.58987589384118,4.86818863433174,-3.32676270870871));
#154774=CARTESIAN_POINT('Ctrl Pts',(6.49245923422682,4.89780165972544,-3.45160473170117));
#154775=CARTESIAN_POINT('Ctrl Pts',(6.42553916100857,4.91777478469304,-3.5333726746681));
#154776=CARTESIAN_POINT('Ctrl Pts',(6.3567655851381,4.93794662095604,-3.61353786663321));
#154777=CARTESIAN_POINT('Ctrl Pts',(6.53859250876927,4.73205099317319,-3.71030528036639));
#154778=CARTESIAN_POINT('Ctrl Pts',(6.57756753156013,4.74662633124687,-3.61208736757819));
#154779=CARTESIAN_POINT('Ctrl Pts',(6.6144684601147,4.7612192280688,-3.51306079885455));
#154780=CARTESIAN_POINT('Ctrl Pts',(6.68384898913673,4.79033919873798,-3.31413913287888));
#154781=CARTESIAN_POINT('Ctrl Pts',(6.71634731529611,4.80486306086017,-3.21427413852161));
#154782=CARTESIAN_POINT('Ctrl Pts',(6.74673611187852,4.81939092103915,-3.11376028637559));
#154783=CARTESIAN_POINT('Ctrl Pts',(6.79150223242666,4.819390921,-3.22681549701117));
#154784=CARTESIAN_POINT('Ctrl Pts',(6.61664641316176,4.754503495,-3.59483582030978));
#154785=CARTESIAN_POINT('Ctrl Pts',(6.40304641741186,4.689276009,-3.94180636280658));
#154786=CARTESIAN_POINT('Ctrl Pts',(6.781880067,4.819390921,-3.202515068));
#154787=CARTESIAN_POINT('Ctrl Pts',(6.60834104800001,4.754503495,-3.570013982));
#154788=CARTESIAN_POINT('Ctrl Pts',(6.396106485,4.689276009,-3.916608461));
#154789=CARTESIAN_POINT('Ctrl Pts',(6.65381782500001,4.819390921,-2.879098531));
#154790=CARTESIAN_POINT('Ctrl Pts',(6.497804216,4.754503495,-3.239657963));
#154791=CARTESIAN_POINT('Ctrl Pts',(6.303742317,4.689276009,-3.58124738));
#154792=CARTESIAN_POINT('',(6.70055573136945,4.81939091791743,-2.99713337640664));
#154793=CARTESIAN_POINT('Ctrl Pts',(7.25960604149006,4.689268254,-1.95842989642778));
#154794=CARTESIAN_POINT('Ctrl Pts',(7.15208425107236,4.754934719,-2.35699705509661));
#154795=CARTESIAN_POINT('Ctrl Pts',(7.0015759247285,4.819390921,-2.74139783555722));
#154796=CARTESIAN_POINT('Ctrl Pts',(7.23646594,4.689268254,-1.97067519));
#154797=CARTESIAN_POINT('Ctrl Pts',(7.128271858,4.754934719,-2.36797191));
#154798=CARTESIAN_POINT('Ctrl Pts',(6.977234361,4.819390921,-2.751036289));
#154799=CARTESIAN_POINT('Ctrl Pts',(6.929012748,4.689268254,-2.133373465));
#154800=CARTESIAN_POINT('Ctrl Pts',(6.811886199,4.754934719,-2.513790379));
#154801=CARTESIAN_POINT('Ctrl Pts',(6.653817825,4.819390921,-2.879098531));
#154802=CARTESIAN_POINT('',(6.88847958175789,4.81939091976399,-2.78618024947188));
#154803=CARTESIAN_POINT('',(6.77067233276658,4.81939091820872,-2.83282802776268));
#154804=CARTESIAN_POINT('',(7.18320130066625,4.73201982383894,-2.21796163729291));
#154805=CARTESIAN_POINT('Ctrl Pts',(6.88847958119671,4.81939092085773,-2.78618024299713));
#154806=CARTESIAN_POINT('Ctrl Pts',(6.94143366829728,4.80491309556365,-2.69386960074661));
#154807=CARTESIAN_POINT('Ctrl Pts',(6.99243851802072,4.79041128758828,-2.60045777954763));
#154808=CARTESIAN_POINT('Ctrl Pts',(7.09077692407315,4.7612864769949,-2.41100736677257));
#154809=CARTESIAN_POINT('Ctrl Pts',(7.13807668749975,4.74666639459136,-2.31497700028956));
#154810=CARTESIAN_POINT('Ctrl Pts',(7.18333619157649,4.73203683301509,-2.21798362007685));
#154811=CARTESIAN_POINT('Ctrl Pts',(6.92760979322192,4.69005394737233,-2.13792482796009));
#154812=CARTESIAN_POINT('Ctrl Pts',(6.96811944820875,4.69707706867108,-2.15056983262706));
#154813=CARTESIAN_POINT('Ctrl Pts',(7.00867726644626,4.70392124753095,-2.16325197718333));
#154814=CARTESIAN_POINT('Ctrl Pts',(7.09380866214356,4.71792585994454,-2.18991424646924));
#154815=CARTESIAN_POINT('Ctrl Pts',(7.13844316561336,4.72506040967912,-2.20391765390694));
#154816=CARTESIAN_POINT('Ctrl Pts',(7.18306640975602,4.73200281466279,-2.21793965450897));
#154817=CARTESIAN_POINT('Origin',(6.57026516526216E-13,4.93907430000125,
-1.80844922370582E-13));
#154818=CARTESIAN_POINT('',(6.98495176460664,4.93794662022521,-2.16253866434672));
#154819=CARTESIAN_POINT('Ctrl Pts',(6.98495285287821,4.93794846925664,-2.16252889722076));
#154820=CARTESIAN_POINT('Ctrl Pts',(6.97331261263774,4.91814371449703,-2.26709116209391));
#154821=CARTESIAN_POINT('Ctrl Pts',(6.95945383338078,4.89834552799468,-2.37139307551936));
#154822=CARTESIAN_POINT('Ctrl Pts',(6.935359333946,4.86872423037574,-2.52718715267149));
#154823=CARTESIAN_POINT('Ctrl Pts',(6.92679476578634,4.85888055803537,-2.57891714116587));
#154824=CARTESIAN_POINT('Ctrl Pts',(6.90768014386894,4.83826147081477,-2.68719461261355));
#154825=CARTESIAN_POINT('Ctrl Pts',(6.89780625681373,4.82833849629522,-2.73925845828388));
#154826=CARTESIAN_POINT('Ctrl Pts',(6.88847957946565,4.8193909201761,-2.78618024909484));
#154827=CARTESIAN_POINT('',(7.25836759455823,4.81939091960755,-1.59061346457017));
#154828=CARTESIAN_POINT('Ctrl Pts',(7.25836759274682,4.81939091981385,-1.59061346376413));
#154829=CARTESIAN_POINT('Ctrl Pts',(7.2392443413621,4.82837891576264,-1.63588989669372));
#154830=CARTESIAN_POINT('Ctrl Pts',(7.21819800562684,4.83808521910493,-1.68441523451707));
#154831=CARTESIAN_POINT('Ctrl Pts',(7.17312800219686,4.85839508139569,-1.78458328712413));
#154832=CARTESIAN_POINT('Ctrl Pts',(7.1509639011611,4.86818863447246,-1.83235632410635));
#154833=CARTESIAN_POINT('Ctrl Pts',(7.08266213355276,4.89780165987253,-1.9752213120985));
#154834=CARTESIAN_POINT('Ctrl Pts',(7.03488430515766,4.91777478482829,-2.0694634035917));
#154835=CARTESIAN_POINT('Ctrl Pts',(6.98495176389734,4.93794662106943,-2.16253866378324));
#154836=CARTESIAN_POINT('Ctrl Pts',(7.18332980902812,4.73205099315307,-2.21795629449247));
#154837=CARTESIAN_POINT('Ctrl Pts',(7.20027966947563,4.74662633120077,-2.11365618425764));
#154838=CARTESIAN_POINT('Ctrl Pts',(7.21503008972912,4.7612192280067,-2.0090121929705));
#154839=CARTESIAN_POINT('Ctrl Pts',(7.24002626209827,4.79033919833949,-1.79982644475022));
#154840=CARTESIAN_POINT('Ctrl Pts',(7.25029677383234,4.80486306066114,-1.69531005772086));
#154841=CARTESIAN_POINT('Ctrl Pts',(7.25836759025581,4.81939092102856,-1.59061346945665));
#154842=CARTESIAN_POINT('Ctrl Pts',(7.32639063248861,4.819390921,-1.69140211925593));
#154843=CARTESIAN_POINT('Ctrl Pts',(7.23473633580764,4.754503495,-2.08840716336033));
#154844=CARTESIAN_POINT('Ctrl Pts',(7.10071859964245,4.689276009,-2.47318341352876));
#154845=CARTESIAN_POINT('Ctrl Pts',(7.311769554,4.819390921,-1.669738302));
#154846=CARTESIAN_POINT('Ctrl Pts',(7.221289184,4.754503495,-2.065951054));
#154847=CARTESIAN_POINT('Ctrl Pts',(7.08852411500001,4.689276009,-2.450066505));
#154848=CARTESIAN_POINT('Ctrl Pts',(7.11717634000001,4.819390921,-1.381412661));
#154849=CARTESIAN_POINT('Ctrl Pts',(7.04231986300001,4.754503495,-1.767080728));
#154850=CARTESIAN_POINT('Ctrl Pts',(6.926226651,4.689276009,-2.142401545));
#154851=CARTESIAN_POINT('',(7.18819554290371,4.81939091791719,-1.48664064912483));
#154852=CARTESIAN_POINT('Ctrl Pts',(7.51088502287621,4.689268254,-0.352042186526741));
#154853=CARTESIAN_POINT('Ctrl Pts',(7.49155719048726,4.754934719,-0.764405074307319));
#154854=CARTESIAN_POINT('Ctrl Pts',(7.42720247132914,4.819390921,-1.17217361937048));
#154855=CARTESIAN_POINT('Ctrl Pts',(7.4909183,4.689268254,-0.36897563));
#154856=CARTESIAN_POINT('Ctrl Pts',(7.470660787,4.754934719,-0.780242304));
#154857=CARTESIAN_POINT('Ctrl Pts',(7.405501982,4.819390921,-1.186819448));
#154858=CARTESIAN_POINT('Ctrl Pts',(7.22562851299999,4.689268254,-0.593963458000001));
#154859=CARTESIAN_POINT('Ctrl Pts',(7.193018709,4.754934719,-0.990665182));
#154860=CARTESIAN_POINT('Ctrl Pts',(7.11717634,4.819390921,-1.381412661));
#154861=CARTESIAN_POINT('',(7.22135206436877,4.81939091820872,-1.31110367082324));
#154862=CARTESIAN_POINT('Ctrl Pts',(7.2252367670457,4.69005394743003,-0.598710006737396));
#154863=CARTESIAN_POINT('Ctrl Pts',(7.26751763097446,4.69707706870792,-0.6023509997094));
#154864=CARTESIAN_POINT('Ctrl Pts',(7.30985351641467,4.7039212475935,-0.606017910678717));
#154865=CARTESIAN_POINT('Ctrl Pts',(7.39872618716097,4.71792585997227,-0.613756097271705));
#154866=CARTESIAN_POINT('Ctrl Pts',(7.44532747948944,4.72506040969926,-0.617837014015916));
#154867=CARTESIAN_POINT('Ctrl Pts',(7.49192177268656,4.73200281467246,-0.62193850969841));
#154868=CARTESIAN_POINT('Ctrl Pts',(7.51870514809341,4.819390921,-0.076900657597555));
#154869=CARTESIAN_POINT('Ctrl Pts',(7.51453802865909,4.754503495,-0.484326909943372));
#154870=CARTESIAN_POINT('Ctrl Pts',(7.46636907136083,4.689276009,-0.888917156273409));
#154871=CARTESIAN_POINT('Ctrl Pts',(7.499768822,4.819390921,-0.058886428));
#154872=CARTESIAN_POINT('Ctrl Pts',(7.496577864,4.754503495,-0.465286552));
#154873=CARTESIAN_POINT('Ctrl Pts',(7.449490235,4.689276009,-0.868962162));
#154874=CARTESIAN_POINT('Ctrl Pts',(7.2477436,4.819390921,0.180866531));
#154875=CARTESIAN_POINT('Ctrl Pts',(7.25754446000001,4.754503495,-0.211876761));
#154876=CARTESIAN_POINT('Ctrl Pts',(7.22484832400001,4.689276009,-0.603379396));
#154877=CARTESIAN_POINT('',(7.33880352304753,4.81939091791719,0.0942407518356453));
#154878=CARTESIAN_POINT('Ctrl Pts',(7.41096336896773,4.689268254,1.27080662387004));
#154879=CARTESIAN_POINT('Ctrl Pts',(7.48073324162791,4.754934719,0.86392963883171));
#154880=CARTESIAN_POINT('Ctrl Pts',(7.50554128344012,4.819390921,0.451860133748774));
#154881=CARTESIAN_POINT('Ctrl Pts',(7.39510364700001,4.689268254,1.24997682));
#154882=CARTESIAN_POINT('Ctrl Pts',(7.463729921,4.754934719,0.843970566));
#154883=CARTESIAN_POINT('Ctrl Pts',(7.48749656,4.819390921,0.432891753));
#154884=CARTESIAN_POINT('Ctrl Pts',(7.18438192,4.689268254,0.97321962));
#154885=CARTESIAN_POINT('Ctrl Pts',(7.23781366,4.754934719,0.578782418));
#154886=CARTESIAN_POINT('Ctrl Pts',(7.2477436,4.819390921,0.180866531));
#154887=CARTESIAN_POINT('',(7.42170146897581,4.81939091973662,0.363728793212368));
#154888=CARTESIAN_POINT('',(7.33436939906887,4.81939091820872,0.271926436703321));
#154889=CARTESIAN_POINT('',(7.4505948541799,4.73201982386191,1.00318047675999));
#154890=CARTESIAN_POINT('Ctrl Pts',(7.42170146582378,4.81939092087145,0.363728798718234));
#154891=CARTESIAN_POINT('Ctrl Pts',(7.43100106085642,4.80491309582812,0.469742510757373));
#154892=CARTESIAN_POINT('Ctrl Pts',(7.43806920306258,4.79041128812343,0.575937162154928));
#154893=CARTESIAN_POINT('Ctrl Pts',(7.44777055976193,4.76128647702322,0.789168928915151));
#154894=CARTESIAN_POINT('Ctrl Pts',(7.45037655808387,4.74666639461449,0.896184384460626));
#154895=CARTESIAN_POINT('Ctrl Pts',(7.45072650818383,4.7320368330397,1.00321716493418));
#154896=CARTESIAN_POINT('Ctrl Pts',(7.18501969993772,4.69005394736277,0.968499828836364));
#154897=CARTESIAN_POINT('Ctrl Pts',(7.22709476672504,4.69707706864331,0.974033096195835));
#154898=CARTESIAN_POINT('Ctrl Pts',(7.26922914014701,4.70392124752637,0.979552879507885));
#154899=CARTESIAN_POINT('Ctrl Pts',(7.35768749876934,4.71792585994092,0.991100604633074));
#154900=CARTESIAN_POINT('Ctrl Pts',(7.40407655527288,4.72506040968585,0.997132997816654));
#154901=CARTESIAN_POINT('Ctrl Pts',(7.45046320017597,4.73200281468412,1.00314378858579));
#154902=CARTESIAN_POINT('Origin',(9.94430232603705E-13,4.9390743,9.72800399262619E-14));
#154903=CARTESIAN_POINT('',(7.24739694618749,4.93794662020714,0.970238183641761));
#154904=CARTESIAN_POINT('Ctrl Pts',(7.24739694729143,4.93794661905671,0.970238184238935));
#154905=CARTESIAN_POINT('Ctrl Pts',(7.28073710674728,4.91814186433868,0.870452432924917));
#154906=CARTESIAN_POINT('Ctrl Pts',(7.31195134176256,4.89834552778171,0.769980750653622));
#154907=CARTESIAN_POINT('Ctrl Pts',(7.35550000134278,4.86872423018959,0.618468858201964));
#154908=CARTESIAN_POINT('Ctrl Pts',(7.36944786817102,4.85888055785931,0.567923823437499));
#154909=CARTESIAN_POINT('Ctrl Pts',(7.39756443723973,4.83826147072286,0.461627830901946));
#154910=CARTESIAN_POINT('Ctrl Pts',(7.41046418140696,4.82833849622491,0.41023002688005));
#154911=CARTESIAN_POINT('Ctrl Pts',(7.4217014669009,4.81939092009302,0.363728792642376));
#154912=CARTESIAN_POINT('',(7.25539727428587,4.81939091962013,1.60410776566287));
#154913=CARTESIAN_POINT('Ctrl Pts',(7.25539727225668,4.81939091984757,1.6041077656361));
#154914=CARTESIAN_POINT('Ctrl Pts',(7.25705256066902,4.82837891800305,1.55498633038954));
#154915=CARTESIAN_POINT('Ctrl Pts',(7.25832668383295,4.83808522200181,1.50210879657953));
#154916=CARTESIAN_POINT('Ctrl Pts',(7.25948173003012,4.85839508137762,1.39227434661416));
#154917=CARTESIAN_POINT('Ctrl Pts',(7.25942551431641,4.86818863450141,1.33961024775736));
#154918=CARTESIAN_POINT('Ctrl Pts',(7.25742400178274,4.89780104726198,1.18127360416032));
#154919=CARTESIAN_POINT('Ctrl Pts',(7.2536330114369,4.9177754105084,1.07567386289559));
#154920=CARTESIAN_POINT('Ctrl Pts',(7.24739694504265,4.93794662132742,0.9702381839238));
#154921=CARTESIAN_POINT('Ctrl Pts',(7.45070924183244,4.73205099316992,1.00323928500142));
#154922=CARTESIAN_POINT('Ctrl Pts',(7.4222980389261,4.74662633124793,1.10501656302923));
#154923=CARTESIAN_POINT('Ctrl Pts',(7.39174628626538,4.76121922807228,1.20618241809027));
#154924=CARTESIAN_POINT('Ctrl Pts',(7.32659738124921,4.79033919874295,1.40652988402164));
#154925=CARTESIAN_POINT('Ctrl Pts',(7.29203335377851,4.80486306086565,1.50569886250131));
#154926=CARTESIAN_POINT('Ctrl Pts',(7.2553972724486,4.81939092103895,1.60410775924929));
#154927=CARTESIAN_POINT('Ctrl Pts',(7.35945336807604,4.819390921,1.54119659248567));
#154928=CARTESIAN_POINT('Ctrl Pts',(7.44296827404257,4.754503495,1.14239993157747));
#154929=CARTESIAN_POINT('Ctrl Pts',(7.48290042445847,4.689276009,0.736913879334189));
#154930=CARTESIAN_POINT('Ctrl Pts',(7.337087236,4.819390921,1.554718909));
#154931=CARTESIAN_POINT('Ctrl Pts',(7.421334894,4.754503495,1.157134232));
#154932=CARTESIAN_POINT('Ctrl Pts',(7.462126472,4.689276009,0.752773886));
#154933=CARTESIAN_POINT('Ctrl Pts',(7.039414425,4.819390921,1.734688604));
#154934=CARTESIAN_POINT('Ctrl Pts',(7.133414344,4.754503495,1.353234327));
#154935=CARTESIAN_POINT('Ctrl Pts',(7.185644119,4.689276009,0.963856104));
#154936=CARTESIAN_POINT('',(7.14805379311779,4.81939091791745,1.6690064577682));
#154937=CARTESIAN_POINT('Ctrl Pts',(6.9645133045181,4.689268254,2.83423392936511));
#154938=CARTESIAN_POINT('Ctrl Pts',(7.12011852097099,4.754934719,2.45186796138366));
#154939=CARTESIAN_POINT('Ctrl Pts',(7.23292932676832,4.819390921,2.05476540792949));
#154940=CARTESIAN_POINT('Ctrl Pts',(6.953502166,4.689268254,2.810481743));
#154941=CARTESIAN_POINT('Ctrl Pts',(7.107803339,4.754934719,2.428720309));
#154942=CARTESIAN_POINT('Ctrl Pts',(7.21938412,4.819390921,2.032361415));
#154943=CARTESIAN_POINT('Ctrl Pts',(6.807201613,4.689268254,2.49489603));
#154944=CARTESIAN_POINT('Ctrl Pts',(6.94417648700001,4.754934719,2.121166795));
#154945=CARTESIAN_POINT('Ctrl Pts',(7.039414425,4.819390921,1.734688604));
#154946=CARTESIAN_POINT('',(7.16999527406823,4.81939091970922,1.95067144827473));
#154947=CARTESIAN_POINT('',(7.10443977264433,4.81939091820872,1.8422415662143));
#154948=CARTESIAN_POINT('',(7.06074993823213,4.73201982385919,2.58138433013341));
#154949=CARTESIAN_POINT('Ctrl Pts',(7.16999526991829,4.81939092084721,1.95067145274065));
#154950=CARTESIAN_POINT('Ctrl Pts',(7.15628763084189,4.80491309538955,2.05620576419138));
#154951=CARTESIAN_POINT('Ctrl Pts',(7.14036181216804,4.79041128722461,2.16143708857166));
#154952=CARTESIAN_POINT('Ctrl Pts',(7.10399783077811,4.76128647693571,2.3717691141358));
#154953=CARTESIAN_POINT('Ctrl Pts',(7.08353774277662,4.74666639456533,2.47684282010996));
#154954=CARTESIAN_POINT('Ctrl Pts',(7.0608706273649,4.73203683303586,2.58144846228725));
#154955=CARTESIAN_POINT('Ctrl Pts',(6.80883909823081,4.69005394741873,2.49042368960527));
#154956=CARTESIAN_POINT('Ctrl Pts',(6.84874098442337,4.69707706872806,2.50487248769431));
#154957=CARTESIAN_POINT('Ctrl Pts',(6.88870368909124,4.70392124757714,2.51932086608864));
#154958=CARTESIAN_POINT('Ctrl Pts',(6.97261152078471,4.71792585998271,2.54961454381537));
#154959=CARTESIAN_POINT('Ctrl Pts',(7.01661924063605,4.72506040971095,2.56547817877681));
#154960=CARTESIAN_POINT('Ctrl Pts',(7.06062924909937,4.73200281468252,2.58132019797957));
#154961=CARTESIAN_POINT('Origin',(1.04300248993106E-12,4.93907430000018,
3.03468188078693E-13));
#154962=CARTESIAN_POINT('',(6.86938430310311,4.93794662027974,2.50553066717595));
#154963=CARTESIAN_POINT('Ctrl Pts',(6.86938430382193,4.93794661939022,2.50553066780109));
#154964=CARTESIAN_POINT('Ctrl Pts',(6.92339597581209,4.91814186465082,2.41524500063482));
#154965=CARTESIAN_POINT('Ctrl Pts',(6.97547888113087,4.89834552808515,2.32383242836538));
#154966=CARTESIAN_POINT('Ctrl Pts',(7.05057997558024,4.86872423042573,2.18522447423273));
#154967=CARTESIAN_POINT('Ctrl Pts',(7.07506743745908,4.8588805580645,2.13885953332533));
#154968=CARTESIAN_POINT('Ctrl Pts',(7.12537715336372,4.83826147078332,2.04109291284144));
#154969=CARTESIAN_POINT('Ctrl Pts',(7.14902431737564,4.82833849620866,1.99366982439162));
#154970=CARTESIAN_POINT('Ctrl Pts',(7.16999527224034,4.81939092003057,1.95067144731637));
#154971=CARTESIAN_POINT('',(6.74093436535114,4.81939091956886,3.12630056326878));
#154972=CARTESIAN_POINT('Ctrl Pts',(6.74093436364107,4.81939091970027,3.1263005628563));
#154973=CARTESIAN_POINT('Ctrl Pts',(6.75311058856627,4.82837890461987,3.07868347282228));
#154974=CARTESIAN_POINT('Ctrl Pts',(6.76572202560481,4.83808520173977,3.02731611672858));
#154975=CARTESIAN_POINT('Ctrl Pts',(6.79046125202133,4.85839508123233,2.92029772999924));
#154976=CARTESIAN_POINT('Ctrl Pts',(6.80172757514065,4.86818863438586,2.86885280366468));
#154977=CARTESIAN_POINT('Ctrl Pts',(6.83381121865547,4.8978016598734,2.71378450832141));
#154978=CARTESIAN_POINT('Ctrl Pts',(6.85280850453319,4.91777478484511,2.60984512293696));
#154979=CARTESIAN_POINT('Ctrl Pts',(6.86938430221194,4.93794662111043,2.50553066719498));
#154980=CARTESIAN_POINT('Ctrl Pts',(7.06084900952567,4.73205099317129,2.58146635344278));
#154981=CARTESIAN_POINT('Ctrl Pts',(7.01122293851196,4.74662633122357,2.67475656650648));
#154982=CARTESIAN_POINT('Ctrl Pts',(6.95963780046243,4.76121922803318,2.76698949640077));
#154983=CARTESIAN_POINT('Ctrl Pts',(6.85294325765045,4.79033919870283,2.94864786124386));
#154984=CARTESIAN_POINT('Ctrl Pts',(6.79786891886765,4.80486306085235,3.03806808008998));
#154985=CARTESIAN_POINT('Ctrl Pts',(6.74093436486265,4.81939092103708,3.12630055704499));
#154986=CARTESIAN_POINT('Ctrl Pts',(6.85608172884453,4.819390921,3.08722920296354));
#154987=CARTESIAN_POINT('Ctrl Pts',(7.0233735958105,4.754503495,2.71570942253431));
#154988=CARTESIAN_POINT('Ctrl Pts',(7.14953966970884,4.689276009,2.32828764003355));
#154989=CARTESIAN_POINT('Ctrl Pts',(6.831331606,4.819390921,3.095627318));
#154990=CARTESIAN_POINT('Ctrl Pts',(6.999078553,4.754503495,2.725448706));
#154991=CARTESIAN_POINT('Ctrl Pts',(7.12584196800001,4.689276009,2.339311063));
#154992=CARTESIAN_POINT('Ctrl Pts',(6.501930055,4.819390921,3.207398566));
#154993=CARTESIAN_POINT('Ctrl Pts',(6.675733702,4.754503495,2.855069682));
#154994=CARTESIAN_POINT('Ctrl Pts',(6.81044718200001,4.689276009,2.486022764));
#154995=CARTESIAN_POINT('',(6.62214921468494,4.81939091791719,3.16660628438882));
#154996=CARTESIAN_POINT('Ctrl Pts',(6.19241033836026,4.689268254,4.26513560605128));
#154997=CARTESIAN_POINT('Ctrl Pts',(6.4265749708741,4.754934719,3.92515966456883));
#154998=CARTESIAN_POINT('Ctrl Pts',(6.62211363423336,4.819390921,3.56159213646275));
#154999=CARTESIAN_POINT('Ctrl Pts',(6.186762652,4.689268254,4.239571663));
#155000=CARTESIAN_POINT('Ctrl Pts',(6.419523772,4.754934719,3.899905791));
#155001=CARTESIAN_POINT('Ctrl Pts',(6.61370130300001,4.819390921,3.536800117));
#155002=CARTESIAN_POINT('Ctrl Pts',(6.111724124,4.689268254,3.899913875));
#155003=CARTESIAN_POINT('Ctrl Pts',(6.32583734,4.754934719,3.564367771));
#155004=CARTESIAN_POINT('Ctrl Pts',(6.501930055,4.819390921,3.207398566));
#155005=CARTESIAN_POINT('',(6.58302806924343,4.8193909197456,3.44640287397763));
#155006=CARTESIAN_POINT('',(6.542314438764,4.81939091820872,3.32641552756463));
#155007=CARTESIAN_POINT('',(6.3407522023859,4.73201982388303,4.03888552173727));
#155008=CARTESIAN_POINT('Ctrl Pts',(6.5830280640492,4.81939092085899,3.44640287763249));
#155009=CARTESIAN_POINT('Ctrl Pts',(6.54695414499058,4.80491309561722,3.54652311704798));
#155010=CARTESIAN_POINT('Ctrl Pts',(6.50877903958484,4.79041128768656,3.64587060988582));
#155011=CARTESIAN_POINT('Ctrl Pts',(6.42805005867109,4.76128647704054,3.8434680110759));
#155012=CARTESIAN_POINT('Ctrl Pts',(6.38548057524206,4.74666639463987,3.94168683827164));
#155013=CARTESIAN_POINT('Ctrl Pts',(6.34085628336632,4.7320368330631,4.03897409908925));
#155014=CARTESIAN_POINT('Ctrl Pts',(6.11428474712324,4.69005394750855,3.89589810638951));
#155015=CARTESIAN_POINT('Ctrl Pts',(6.15014768491915,4.69707706880471,3.91858682551975));
#155016=CARTESIAN_POINT('Ctrl Pts',(6.18607010944633,4.70392124763845,3.94128820901256));
#155017=CARTESIAN_POINT('Ctrl Pts',(6.26150397730438,4.71792586002178,3.98891134089339));
#155018=CARTESIAN_POINT('Ctrl Pts',(6.30107260842563,4.72506040973843,4.01386445183326));
#155019=CARTESIAN_POINT('Ctrl Pts',(6.34064812140549,4.73200281470297,4.03879694438529));
#155020=CARTESIAN_POINT('Origin',(1.01047642475649E-13,4.93907430000125,
1.22731685925359E-13));
#155021=CARTESIAN_POINT('',(6.17016688530534,4.93794662024516,3.92366731972341));
#155022=CARTESIAN_POINT('Ctrl Pts',(6.17016688596748,4.93794661920754,3.92366732061585));
#155023=CARTESIAN_POINT('Ctrl Pts',(6.24232454472163,4.91814186446448,3.84710339503515));
#155024=CARTESIAN_POINT('Ctrl Pts',(6.31284078157814,4.89834552790831,3.7690242829255));
#155025=CARTESIAN_POINT('Ctrl Pts',(6.41598266705498,4.86872423030126,3.64980142099868));
#155026=CARTESIAN_POINT('Ctrl Pts',(6.44986471740306,4.85888055796827,3.6097845471039));
#155027=CARTESIAN_POINT('Ctrl Pts',(6.52001515335497,4.83826147078904,3.52511875777889));
#155028=CARTESIAN_POINT('Ctrl Pts',(6.55330402191576,4.82833849627079,3.48388783610231));
#155029=CARTESIAN_POINT('Ctrl Pts',(6.58302806754595,4.81939092012227,3.44640287254168));
#155030=CARTESIAN_POINT('',(5.91127285763218,4.81939091960316,4.50231102143997));
#155031=CARTESIAN_POINT('Ctrl Pts',(5.91127285587575,4.81939091979814,4.5023110205943));
#155032=CARTESIAN_POINT('Ctrl Pts',(5.93340068110552,4.82837890717549,4.45842470701994));
#155033=CARTESIAN_POINT('Ctrl Pts',(5.9567597358703,4.83808520599485,4.4109693698699));
#155034=CARTESIAN_POINT('Ctrl Pts',(6.0039263530434,4.85839508132317,4.31177123615426));
#155035=CARTESIAN_POINT('Ctrl Pts',(6.02598841424333,4.86818863446027,4.26395099008268));
#155036=CARTESIAN_POINT('Ctrl Pts',(6.09065705974093,4.89780165993548,4.11940514025462));
#155037=CARTESIAN_POINT('Ctrl Pts',(6.13155409507273,4.91777478492038,4.02197965479997));
#155038=CARTESIAN_POINT('Ctrl Pts',(6.17016688427914,4.93794662122005,3.92366731952039));
#155039=CARTESIAN_POINT('Ctrl Pts',(6.34083132488251,4.73205099318433,4.03898692477078));
#155040=CARTESIAN_POINT('Ctrl Pts',(6.27231084572381,4.74662633121309,4.11942792610098));
#155041=CARTESIAN_POINT('Ctrl Pts',(6.20210438604712,4.7612192280144,4.19841522144427));
#155042=CARTESIAN_POINT('Ctrl Pts',(6.05885312475774,4.79033919848783,4.35289034064804));
#155043=CARTESIAN_POINT('Ctrl Pts',(5.98584368919382,4.80486306074136,4.42838061007477));
#155044=CARTESIAN_POINT('Ctrl Pts',(5.91127285856016,4.81939092103213,4.50231101503326));
#155045=CARTESIAN_POINT('Ctrl Pts',(6.03212732728657,4.819390921,4.48890640701289));
#155046=CARTESIAN_POINT('Ctrl Pts',(6.27537377440064,4.754503495,4.16203535965215));
#155047=CARTESIAN_POINT('Ctrl Pts',(6.48187438570106,4.689276009,3.81079325888398));
#155048=CARTESIAN_POINT('Ctrl Pts',(6.006150502,4.819390921,4.491787634));
#155049=CARTESIAN_POINT('Ctrl Pts',(6.249553078,4.754503495,4.166324228));
#155050=CARTESIAN_POINT('Ctrl Pts',(6.456361013,4.689276009,3.816464655));
#155051=CARTESIAN_POINT('Ctrl Pts',(5.660422662,4.819390921,4.530134136));
#155052=CARTESIAN_POINT('Ctrl Pts',(5.905903171,4.754503495,4.223405152));
#155053=CARTESIAN_POINT('Ctrl Pts',(6.116801304,4.689276009,3.891945762));
#155054=CARTESIAN_POINT('',(5.7866002991413,4.81939091791719,4.51613912119474));
#155055=CARTESIAN_POINT('Ctrl Pts',(5.13075714752225,4.689268254,5.49660428171978));
#155056=CARTESIAN_POINT('Ctrl Pts',(5.43253191840415,4.754934719,5.21491526319109));
#155057=CARTESIAN_POINT('Ctrl Pts',(5.70165526825467,4.819390921,4.90188277526916));
#155058=CARTESIAN_POINT('Ctrl Pts',(5.130736993,4.689268254,5.47042392400001));
#155059=CARTESIAN_POINT('Ctrl Pts',(5.431074409,4.754934719,5.188736012));
#155060=CARTESIAN_POINT('Ctrl Pts',(5.698769164,4.819390921,4.875861977));
#155061=CARTESIAN_POINT('Ctrl Pts',(5.130469208,4.689268254,5.12257608100001));
#155062=CARTESIAN_POINT('Ctrl Pts',(5.41170907,4.754934719,4.840902871));
#155063=CARTESIAN_POINT('Ctrl Pts',(5.660422662,4.819390921,4.530134136));
#155064=CARTESIAN_POINT('',(5.68824578838242,4.81939091971947,4.78098433171713));
#155065=CARTESIAN_POINT('',(5.67427775255105,4.81939091820873,4.6550499957781));
#155066=CARTESIAN_POINT('',(5.32426794103522,4.73201982384579,5.30753291487205));
#155067=CARTESIAN_POINT('Ctrl Pts',(5.68824578258985,4.81939092086497,4.78098433419026));
#155068=CARTESIAN_POINT('Ctrl Pts',(5.63149236024124,4.80491309574013,4.87100899105073));
#155069=CARTESIAN_POINT('Ctrl Pts',(5.5728529938489,4.79041128793007,4.95982727479803));
#155070=CARTESIAN_POINT('Ctrl Pts',(5.45153381034727,4.76128647704277,5.1354506154349));
#155071=CARTESIAN_POINT('Ctrl Pts',(5.38884543321955,4.74666639462687,5.22222196051445));
#155072=CARTESIAN_POINT('Ctrl Pts',(5.32435054716052,4.7320368330288,5.30764179564587));
#155073=CARTESIAN_POINT('Ctrl Pts',(5.13383323629967,4.69005394740914,5.11920465603329));
#155074=CARTESIAN_POINT('Ctrl Pts',(5.16398031443929,4.69707706865119,5.14907239726348));
#155075=CARTESIAN_POINT('Ctrl Pts',(5.19418276648921,4.70392124753492,5.17896529492946));
#155076=CARTESIAN_POINT('Ctrl Pts',(5.25761546681946,4.71792585991741,5.24169107654769));
#155077=CARTESIAN_POINT('Ctrl Pts',(5.29089482417904,4.72506040965878,5.274566883803));
#155078=CARTESIAN_POINT('Ctrl Pts',(5.32418533490993,4.73200281466277,5.30742403409823));
#155079=CARTESIAN_POINT('Origin',(-4.33680868994202E-13,4.93907430000142,
-5.08707659330199E-13));
#155080=CARTESIAN_POINT('',(5.18243932173717,4.93794662023057,5.15833764936207));
#155081=CARTESIAN_POINT('Ctrl Pts',(5.18243932225554,4.93794661907332,5.15833765050919));
#155082=CARTESIAN_POINT('Ctrl Pts',(5.26936895578191,4.91814186434841,5.09907551064492));
#155083=CARTESIAN_POINT('Ctrl Pts',(5.35502126333883,4.89834552778627,5.03798075123464));
#155084=CARTESIAN_POINT('Ctrl Pts',(5.48138113989073,4.86872423019759,4.94371771012989));
#155085=CARTESIAN_POINT('Ctrl Pts',(5.52307349170308,4.85888055787091,4.91192004780149));
#155086=CARTESIAN_POINT('Ctrl Pts',(5.60978449120292,4.83826147075238,4.84431396785914));
#155087=CARTESIAN_POINT('Ctrl Pts',(5.65115851388493,4.8283384962394,4.81120312496045));
#155088=CARTESIAN_POINT('Ctrl Pts',(5.6882457871148,4.81939092005774,4.78098433006123));
#155089=CARTESIAN_POINT('',(4.80520680109334,4.81939091959657,5.66779841993978));
#155090=CARTESIAN_POINT('Ctrl Pts',(4.80520679962465,4.81939091977378,5.66779841878496));
#155091=CARTESIAN_POINT('Ctrl Pts',(4.83625148209303,4.82837888943184,5.62969505090097));
#155092=CARTESIAN_POINT('Ctrl Pts',(4.86926588559444,4.83808517869205,5.58837073655554));
#155093=CARTESIAN_POINT('Ctrl Pts',(4.93665453039515,4.8583950812876,5.50163111211332));
#155094=CARTESIAN_POINT('Ctrl Pts',(4.96848073234918,4.86818863446822,5.45967156764961));
#155095=CARTESIAN_POINT('Ctrl Pts',(5.06270859626848,4.89780104727634,5.3324095996632));
#155096=CARTESIAN_POINT('Ctrl Pts',(5.12359685564863,4.91777541052763,5.24604816832737));
#155097=CARTESIAN_POINT('Ctrl Pts',(5.18243932064061,4.93794662136248,5.15833764888674));
#155098=CARTESIAN_POINT('Ctrl Pts',(5.32432341505984,4.73205099313603,5.3076489561436));
#155099=CARTESIAN_POINT('Ctrl Pts',(5.2401124691097,4.74662633120553,5.3714794139907));
#155100=CARTESIAN_POINT('Ctrl Pts',(5.15456746375139,4.76121922803258,5.43352771672791));
#155101=CARTESIAN_POINT('Ctrl Pts',(4.98145774809673,4.79033919935161,5.55359651013127));
#155102=CARTESIAN_POINT('Ctrl Pts',(4.89392705868379,4.80486306117032,5.61162698657165));
#155103=CARTESIAN_POINT('Ctrl Pts',(4.80520680348237,4.81939092105607,5.66779841383323));
#155104=CARTESIAN_POINT('Ctrl Pts',(4.92611735566809,4.819390921,5.68068733594333));
#155105=CARTESIAN_POINT('Ctrl Pts',(5.23394444927887,4.754503495,5.41374914837397));
#155106=CARTESIAN_POINT('Ctrl Pts',(5.51112386023993,4.689276009,5.11511042105134));
#155107=CARTESIAN_POINT('Ctrl Pts',(4.900128476,4.819390921,5.677916952));
#155108=CARTESIAN_POINT('Ctrl Pts',(5.207805447,4.754503495,5.412387059));
#155109=CARTESIAN_POINT('Ctrl Pts',(5.48498779400001,4.689276009,5.115164602));
#155110=CARTESIAN_POINT('Ctrl Pts',(4.554240196,4.819390921,5.641045669));
#155111=CARTESIAN_POINT('Ctrl Pts',(4.859919172,4.754503495,5.394258892));
#155112=CARTESIAN_POINT('Ctrl Pts',(5.13714059500001,4.689276009,5.11588570100001));
#155113=CARTESIAN_POINT('',(4.68047638465216,4.8193909179172,5.65450231179019));
#155114=CARTESIAN_POINT('Ctrl Pts',(3.82919545430357,4.689268254,6.47105785099436));
#155115=CARTESIAN_POINT('Ctrl Pts',(4.18446971154184,4.754934719,6.26082722012167));
#155116=CARTESIAN_POINT('Ctrl Pts',(4.51459383830672,4.819390921,6.01296682235049));
#155117=CARTESIAN_POINT('Ctrl Pts',(3.834803774,4.689268254,6.44548524300001));
#155118=CARTESIAN_POINT('Ctrl Pts',(4.188674043,4.754934719,6.234946704));
#155119=CARTESIAN_POINT('Ctrl Pts',(4.517368912,4.819390921,5.98693394900001));
#155120=CARTESIAN_POINT('Ctrl Pts',(3.909319254,4.689268254,6.105712323));
#155121=CARTESIAN_POINT('Ctrl Pts',(4.244535298,4.754934719,5.891082733));
#155122=CARTESIAN_POINT('Ctrl Pts',(4.554240196,4.819390921,5.64104566900001));
#155123=CARTESIAN_POINT('',(4.5274874560285,4.81939091970524,5.89201227629259));
#155124=CARTESIAN_POINT('',(4.54091814475076,4.81939091820872,5.76601949987998));
#155125=CARTESIAN_POINT('',(4.0588268284519,4.73201982389532,6.32800596761535));
#155126=CARTESIAN_POINT('Ctrl Pts',(4.52748745002682,4.8193909208755,5.89201227736476));
#155127=CARTESIAN_POINT('Ctrl Pts',(4.45270825217731,4.80491309595357,5.96773189845441));
#155128=CARTESIAN_POINT('Ctrl Pts',(4.37634653726941,4.79041128835246,6.04186792862038));
#155129=CARTESIAN_POINT('Ctrl Pts',(4.22010990001682,4.76128647707316,6.18730525675326));
#155130=CARTESIAN_POINT('Ctrl Pts',(4.14023386809453,4.74666639465908,6.2585717879563));
#155131=CARTESIAN_POINT('Ctrl Pts',(4.05888409709935,4.7320368330706,6.3281300607384));
#155132=CARTESIAN_POINT('Ctrl Pts',(3.91332938999963,4.69005394748938,6.10314288784437));
#155133=CARTESIAN_POINT('Ctrl Pts',(3.93635096493821,4.69707706879331,6.13879306848366));
#155134=CARTESIAN_POINT('Ctrl Pts',(3.95942121082128,4.70392124759608,6.17447972053153));
#155135=CARTESIAN_POINT('Ctrl Pts',(4.00788670113755,4.71792586001038,6.24937516349814));
#155136=CARTESIAN_POINT('Ctrl Pts',(4.03332067884046,4.72506040973901,6.28863643055456));
#155137=CARTESIAN_POINT('Ctrl Pts',(4.05876955980445,4.73200281472003,6.3278818744923));
#155138=CARTESIAN_POINT('Origin',(1.51571463713474E-13,4.93907430000036,
2.61509564003504E-13));
#155139=CARTESIAN_POINT('',(3.95238665404255,4.93794662023081,6.15180984471564));
#155140=CARTESIAN_POINT('Ctrl Pts',(3.95238665422766,4.93794661938177,6.15180984560589));
#155141=CARTESIAN_POINT('Ctrl Pts',(4.05002352969431,4.91814186458453,6.11262052322142));
#155142=CARTESIAN_POINT('Ctrl Pts',(4.14680690131411,4.89834552798455,6.07136683959648));
#155143=CARTESIAN_POINT('Ctrl Pts',(4.29047632194858,4.86872423028554,6.00647125421571));
#155144=CARTESIAN_POINT('Ctrl Pts',(4.33802948738522,4.85888055790745,5.98437962672833));
#155145=CARTESIAN_POINT('Ctrl Pts',(4.43724654087929,4.83826147070269,5.93699444105603));
#155146=CARTESIAN_POINT('Ctrl Pts',(4.48477111437587,4.82833849616324,5.91355190316687));
#155147=CARTESIAN_POINT('Ctrl Pts',(4.52748745518786,4.81939092000006,5.89201227450301));
#155148=CARTESIAN_POINT('',(3.4744546152313,4.81939091970674,6.56826586411545));
#155149=CARTESIAN_POINT('Ctrl Pts',(3.47445461370284,4.81939091997752,6.56826586226773));
#155150=CARTESIAN_POINT('Ctrl Pts',(3.51296474936782,4.82837892459898,6.537726893308));
#155151=CARTESIAN_POINT('Ctrl Pts',(3.55409086076293,4.83808523213118,6.504465780003));
#155152=CARTESIAN_POINT('Ctrl Pts',(3.63855022943076,4.85839508128673,6.43424083121638));
#155153=CARTESIAN_POINT('Ctrl Pts',(3.67865241365108,4.86818863433627,6.40010397069764));
#155154=CARTESIAN_POINT('Ctrl Pts',(3.79803731333291,4.89780165972223,6.29607137019479));
#155155=CARTESIAN_POINT('Ctrl Pts',(3.8760623568951,4.91777478470677,6.22482261377889));
#155156=CARTESIAN_POINT('Ctrl Pts',(3.95238665336921,4.93794662100664,6.1518098442261));
#155157=CARTESIAN_POINT('Ctrl Pts',(4.05885606001792,4.73205099321256,6.32813122119888));
#155158=CARTESIAN_POINT('Ctrl Pts',(3.96289225747811,4.74662633126892,6.37236649436752));
#155159=CARTESIAN_POINT('Ctrl Pts',(3.86600869576448,4.76121922808055,6.41457449488229));
#155160=CARTESIAN_POINT('Ctrl Pts',(3.67113495261786,4.79033919859532,6.49462267289275));
#155161=CARTESIAN_POINT('Ctrl Pts',(3.5731758422539,4.80486306079332,6.53247991950132));
#155162=CARTESIAN_POINT('Ctrl Pts',(3.47445461813372,4.81939092103448,6.56826585872816));
#155163=CARTESIAN_POINT('Ctrl Pts',(3.58976761215825,4.819390921,6.60684564007593));
#155164=CARTESIAN_POINT('Ctrl Pts',(3.94778169971128,4.754503495,6.41232204349741));
#155165=CARTESIAN_POINT('Ctrl Pts',(4.2826793086101,4.689276009,6.18025070349683));
#155166=CARTESIAN_POINT('Ctrl Pts',(3.564981888,4.819390921,6.598553185));
#155167=CARTESIAN_POINT('Ctrl Pts',(3.922546621,4.754503495,6.405372686));
#155168=CARTESIAN_POINT('Ctrl Pts',(4.257142641,4.689276009,6.174685136));
#155169=CARTESIAN_POINT('Ctrl Pts',(3.23510652,4.819390921,6.48818817600001));
#155170=CARTESIAN_POINT('Ctrl Pts',(3.586690754,4.754503495,6.31288308));
#155171=CARTESIAN_POINT('Ctrl Pts',(3.917272901,4.689276009,6.100612512));
#155172=CARTESIAN_POINT('',(3.35549859635726,4.8193909179172,6.52846725931102));
#155173=CARTESIAN_POINT('Ctrl Pts',(2.34858483786858,4.689268254,7.14293194666788));
#155174=CARTESIAN_POINT('Ctrl Pts',(2.74074635153136,4.754934719,7.01398985508504));
#155175=CARTESIAN_POINT('Ctrl Pts',(3.11643501878727,4.819390921,6.84289122444231));
#155176=CARTESIAN_POINT('Ctrl Pts',(2.359559393,4.689268254,7.119162835));
#155177=CARTESIAN_POINT('Ctrl Pts',(2.750415934,4.754934719,6.98961821800001));
#155178=CARTESIAN_POINT('Ctrl Pts',(3.124741511,4.819390921,6.818063544));
#155179=CARTESIAN_POINT('Ctrl Pts',(2.505373877,4.689268254,6.803352243));
#155180=CARTESIAN_POINT('Ctrl Pts',(2.878891773,4.754934719,6.665802114));
#155181=CARTESIAN_POINT('Ctrl Pts',(3.23510652,4.819390921,6.488188176));
#155182=CARTESIAN_POINT('',(3.15502884264767,4.81939091970705,6.72753627497528));
#155183=CARTESIAN_POINT('',(3.19523025164699,4.81939091820872,6.60737634111682));
#155184=CARTESIAN_POINT('',(2.60359948408427,4.73201982384173,7.05258849478579));
#155185=CARTESIAN_POINT('Ctrl Pts',(3.15502883653014,4.81939092085369,6.72753627472605));
#155186=CARTESIAN_POINT('Ctrl Pts',(3.0657204519689,4.80491309551931,6.78541029771323));
#155187=CARTESIAN_POINT('Ctrl Pts',(2.9752069736963,4.79041128748405,6.84139755873418));
#155188=CARTESIAN_POINT('Ctrl Pts',(2.79135834054187,4.76128647696698,6.94984838141895));
#155189=CARTESIAN_POINT('Ctrl Pts',(2.69802956840313,4.74666639457685,7.0022777548983));
#155190=CARTESIAN_POINT('Ctrl Pts',(2.60362873745907,4.73203683301562,7.05272199775456));
#155191=CARTESIAN_POINT('Ctrl Pts',(2.50984261070199,4.69005394735047,6.80170493940382));
#155192=CARTESIAN_POINT('Ctrl Pts',(2.52466221878368,4.69707706866363,6.84147059689012));
#155193=CARTESIAN_POINT('Ctrl Pts',(2.5395215197407,4.70392124749718,6.88128233602919));
#155194=CARTESIAN_POINT('Ctrl Pts',(2.57075360727919,4.71792585993317,6.96484541325419));
#155195=CARTESIAN_POINT('Ctrl Pts',(2.587152940809,4.72506040967556,7.00865632725573));
#155196=CARTESIAN_POINT('Ctrl Pts',(2.60357023070946,4.73200281466784,7.05245499181701));
#155197=CARTESIAN_POINT('Origin',(2.7527893159407E-13,4.93907429999929,
6.93022028652734E-13));
#155198=CARTESIAN_POINT('',(2.5375247805209,4.93794662024614,6.85763024787807));
#155199=CARTESIAN_POINT('Ctrl Pts',(2.53751508663611,4.9379484691976,6.85763186342078));
#155200=CARTESIAN_POINT('Ctrl Pts',(2.64129381194683,4.91814371445961,6.84034780770094));
#155201=CARTESIAN_POINT('Ctrl Pts',(2.74469245836587,4.89834552797129,6.82086256179474));
#155202=CARTESIAN_POINT('Ctrl Pts',(2.89895360012165,4.86872423033738,6.78836887775632));
#155203=CARTESIAN_POINT('Ctrl Pts',(2.95014404579079,4.85888055797823,6.77701626516097));
#155204=CARTESIAN_POINT('Ctrl Pts',(3.0572278742593,4.83826147071546,6.75206765238496));
#155205=CARTESIAN_POINT('Ctrl Pts',(3.10868080240164,4.82833849616026,6.73938956646646));
#155206=CARTESIAN_POINT('Ctrl Pts',(3.15502884219955,4.81939092002354,6.72753627298416));
#155207=CARTESIAN_POINT('',(1.98124079272459,4.81939091960563,7.16160849615506));
#155208=CARTESIAN_POINT('Ctrl Pts',(1.98124079184273,4.81939091980114,7.16160849442862));
#155209=CARTESIAN_POINT('Ctrl Pts',(2.02541538625655,4.82837889211582,7.14006213131342));
#155210=CARTESIAN_POINT('Ctrl Pts',(2.07273008306626,4.83808518301028,7.11641958361174));
#155211=CARTESIAN_POINT('Ctrl Pts',(2.17031136292566,4.85839508131333,7.0659926007449));
#155212=CARTESIAN_POINT('Ctrl Pts',(2.21681439661171,4.86818863443092,7.04127462508136));
#155213=CARTESIAN_POINT('Ctrl Pts',(2.35577207790842,4.89780165988963,6.9653384732215));
#155214=CARTESIAN_POINT('Ctrl Pts',(2.44728931581958,4.91777478487672,6.91252855109724));
#155215=CARTESIAN_POINT('Ctrl Pts',(2.53752477986336,4.9379466211697,6.85763024713663));
#155216=CARTESIAN_POINT('Ctrl Pts',(2.60360110640195,4.73205099316428,7.05271710393411));
#155217=CARTESIAN_POINT('Ctrl Pts',(2.50037160818322,4.74662633122825,7.07528880007722));
#155218=CARTESIAN_POINT('Ctrl Pts',(2.39667965795009,4.76121922804818,7.09568289904169));
#155219=CARTESIAN_POINT('Ctrl Pts',(2.18915396030579,4.79033919892996,7.13196750112894));
#155220=CARTESIAN_POINT('Ctrl Pts',(2.08534689191287,4.80486306096256,7.14788135295602));
#155221=CARTESIAN_POINT('Ctrl Pts',(1.98124079742037,4.81939092104364,7.16160849159641));
#155222=CARTESIAN_POINT('Ctrl Pts',(2.08556432488194,4.819390921,7.22407518407912));
#155223=CARTESIAN_POINT('Ctrl Pts',(2.47702506393543,4.754503495,7.1110618872917));
#155224=CARTESIAN_POINT('Ctrl Pts',(2.85398143190021,4.689276009,6.95640933332439));
#155225=CARTESIAN_POINT('Ctrl Pts',(2.06314071,4.819390921,7.210648404));
#155226=CARTESIAN_POINT('Ctrl Pts',(2.453873874,4.754503495,7.098850206));
#155227=CARTESIAN_POINT('Ctrl Pts',(2.83023823,4.689276009,6.945484257));
#155228=CARTESIAN_POINT('Ctrl Pts',(1.764702859,4.819390921,7.031950214));
#155229=CARTESIAN_POINT('Ctrl Pts',(2.145752663,4.754503495,6.936323872));
#155230=CARTESIAN_POINT('Ctrl Pts',(2.51423788,4.689276009,6.800081461));
#155231=CARTESIAN_POINT('',(1.87253223753566,4.8193909179172,7.09651615128198));
#155232=CARTESIAN_POINT('Ctrl Pts',(0.758157004557344,4.689268254,7.48081048409299));
#155233=CARTESIAN_POINT('Ctrl Pts',(1.16886873855041,4.754934719,7.4391861192906));
#155234=CARTESIAN_POINT('Ctrl Pts',(1.57255516057675,4.819390921,7.35284963772685));
#155235=CARTESIAN_POINT('Ctrl Pts',(0.773984637,4.689268254,7.45995628600001));
#155236=CARTESIAN_POINT('Ctrl Pts',(1.183551433,4.754934719,7.417462952));
#155237=CARTESIAN_POINT('Ctrl Pts',(1.586004669,4.819390921,7.330388065));
#155238=CARTESIAN_POINT('Ctrl Pts',(0.984280001000001,4.689268254,7.182874973));
#155239=CARTESIAN_POINT('Ctrl Pts',(1.378634468,4.754934719,7.128835996));
#155240=CARTESIAN_POINT('Ctrl Pts',(1.764702859,4.819390921,7.03195021400001));
#155241=CARTESIAN_POINT('',(1.63504458650614,4.81939091971965,7.24848815472403));
#155242=CARTESIAN_POINT('',(1.70013694327804,4.81939091820872,7.13977960720693));
#155243=CARTESIAN_POINT('',(1.0266307218224,4.732019823845,7.44739982217204));
#155244=CARTESIAN_POINT('Ctrl Pts',(1.6350445805021,4.81939092087202,7.24848815316613));
#155245=CARTESIAN_POINT('Ctrl Pts',(1.53538297452666,4.80491309586785,7.28581045002857));
#155246=CARTESIAN_POINT('Ctrl Pts',(1.43495004754048,4.79041128818367,7.32103103698584));
#155247=CARTESIAN_POINT('Ctrl Pts',(1.2320859680399,4.76128647702923,7.38742431950823));
#155248=CARTESIAN_POINT('Ctrl Pts',(1.12966840519222,4.74666639460951,7.41856499618032));
#155249=CARTESIAN_POINT('Ctrl Pts',(1.02663059207865,4.73203683301885,7.44753649252512));
#155250=CARTESIAN_POINT('Ctrl Pts',(0.988998379597802,4.69005394744881,
7.18222682902306));
#155251=CARTESIAN_POINT('Ctrl Pts',(0.994923072737245,4.69707706871718,
7.22424856495182));
#155252=CARTESIAN_POINT('Ctrl Pts',(1.00087662460663,4.703921247592,7.26632383850002));
#155253=CARTESIAN_POINT('Ctrl Pts',(1.01341493203483,4.71792585996633,7.35464723268727));
#155254=CARTESIAN_POINT('Ctrl Pts',(1.02001280689968,4.72506040969293,7.40095924373872));
#155255=CARTESIAN_POINT('Ctrl Pts',(1.02663085156615,4.73200281467114,7.44726315181896));
#155256=CARTESIAN_POINT('Origin',(1.85940672581264E-14,4.93907429999982,
-2.15105711021124E-13));
#155257=CARTESIAN_POINT('',(1.0040110691062,4.93794662027172,7.2427954824852));
#155258=CARTESIAN_POINT('Ctrl Pts',(1.00401106883361,4.93794661914717,7.24279548365829));
#155259=CARTESIAN_POINT('Ctrl Pts',(1.10907906612687,4.91814186439149,7.24822487784654));
#155260=CARTESIAN_POINT('Ctrl Pts',(1.21423924707293,4.89834552782296,7.2514223315788));
#155261=CARTESIAN_POINT('Ctrl Pts',(1.37187903032445,4.86872423019335,7.252849917406));
#155262=CARTESIAN_POINT('Ctrl Pts',(1.42431314780498,4.85888055784907,7.25276715523505));
#155263=CARTESIAN_POINT('Ctrl Pts',(1.53425662938434,4.83826147072032,7.25142168492364));
#155264=CARTESIAN_POINT('Ctrl Pts',(1.58723203015921,4.82833849621078,7.25010086423123));
#155265=CARTESIAN_POINT('Ctrl Pts',(1.63504458649721,4.8193909200433,7.24848815266336));
#155266=CARTESIAN_POINT('',(0.395386352630777,4.81939091962198,7.42008227473765));
#155267=CARTESIAN_POINT('Ctrl Pts',(0.39538635210853,4.81939091985495,7.42008227275818));
#155268=CARTESIAN_POINT('Ctrl Pts',(0.443160188367102,4.82837892523183,
7.40853584051378));
#155269=CARTESIAN_POINT('Ctrl Pts',(0.494451219908121,4.83808523378702,
7.39561727616033));
#155270=CARTESIAN_POINT('Ctrl Pts',(0.600591149699864,4.85839508140899,
7.36734640934662));
#155271=CARTESIAN_POINT('Ctrl Pts',(0.651320602397542,4.86818863451005,
7.35320310385632));
#155272=CARTESIAN_POINT('Ctrl Pts',(0.803353558541045,4.89780165997746,
7.30891409091188));
#155273=CARTESIAN_POINT('Ctrl Pts',(0.904083746722127,4.91777478499841,
7.27701233627068));
#155274=CARTESIAN_POINT('Ctrl Pts',(1.00401106855046,4.93794662133483,7.24279548148896));
#155275=CARTESIAN_POINT('Ctrl Pts',(1.02660465904708,4.73205099316698,7.44752577325948));
#155276=CARTESIAN_POINT('Ctrl Pts',(0.920936361614114,4.74662633123541,
7.44737846502169));
#155277=CARTESIAN_POINT('Ctrl Pts',(0.81528454305873,4.76121922805836,7.44500505710333));
#155278=CARTESIAN_POINT('Ctrl Pts',(0.604810566195762,4.79033919861928,
7.43582945489426));
#155279=CARTESIAN_POINT('Ctrl Pts',(0.500009440448111,4.80486306080291,
7.42905579852791));
#155280=CARTESIAN_POINT('Ctrl Pts',(0.395386358326975,4.81939092103597,
7.42008227124413));
#155281=CARTESIAN_POINT('Ctrl Pts',(0.483842367355651,4.819390921,7.50351500170055));
#155282=CARTESIAN_POINT('Ctrl Pts',(0.890445490471756,4.754503495,7.47729638044081));
#155283=CARTESIAN_POINT('Ctrl Pts',(1.29183455551508,4.689276009,7.40729399359796));
#155284=CARTESIAN_POINT('Ctrl Pts',(0.464829365,4.819390921,7.485581718));
#155285=CARTESIAN_POINT('Ctrl Pts',(0.870460713,4.754503495,7.46039338));
#155286=CARTESIAN_POINT('Ctrl Pts',(1.270995025,4.689276009,7.391520253));
#155287=CARTESIAN_POINT('Ctrl Pts',(0.211783654,4.819390921,7.246906077));
#155288=CARTESIAN_POINT('Ctrl Pts',(0.604481562,4.754503495,7.23542986900001));
#155289=CARTESIAN_POINT('Ctrl Pts',(0.993639891,4.689276009,7.18158616));
#155290=CARTESIAN_POINT('',(0.304135795242029,4.8193909179172,7.33401370379861));
#155291=CARTESIAN_POINT('Origin',(7.74696333558783E-14,4.93907430000071,
1.65666091955785E-13));
#155292=CARTESIAN_POINT('',(0.0386074640004457,4.81939091973237,7.43050878427183));
#155293=CARTESIAN_POINT('Ctrl Pts',(0.0386074583560088,4.81939092087357,
7.43050878143317));
#155294=CARTESIAN_POINT('Ctrl Pts',(-0.0667473027758887,4.80491309622522,
7.44553420406776));
#155295=CARTESIAN_POINT('Ctrl Pts',(-0.172403546298225,4.79041128890658,
7.45834124249127));
#155296=CARTESIAN_POINT('Ctrl Pts',(-0.384797367802654,4.76128647803856,
7.47957250648728));
#155297=CARTESIAN_POINT('Ctrl Pts',(-0.491514790303439,4.74666639559778,
7.4879683829733));
#155298=CARTESIAN_POINT('Ctrl Pts',(-0.598371652318673,4.73203683399558,
7.49411245786321));
#155299=CARTESIAN_POINT('',(-0.576449089007819,4.93794662013209,7.28929565003906));
#155300=CARTESIAN_POINT('Ctrl Pts',(-0.576449089233835,4.93794661980761,
7.28929565063075));
#155301=CARTESIAN_POINT('Ctrl Pts',(-0.47500468183286,4.91814186494119,
7.317184622455));
#155302=CARTESIAN_POINT('Ctrl Pts',(-0.372990444739158,4.89834552828498,
7.34291365205627));
#155303=CARTESIAN_POINT('Ctrl Pts',(-0.219342958828865,4.86872420722662,
7.37819578327224));
#155304=CARTESIAN_POINT('Ctrl Pts',(-0.168116808705067,4.8588805115865,
7.3893867665824));
#155305=CARTESIAN_POINT('Ctrl Pts',(-0.0604545170709904,4.83826142650624,
7.41170734373942));
#155306=CARTESIAN_POINT('Ctrl Pts',(-0.00843383585907548,4.8283384752577,
7.421805523601));
#155307=CARTESIAN_POINT('Ctrl Pts',(0.0386074644507542,4.8193909200799,
7.43050878219518));
#155308=CARTESIAN_POINT('Ctrl Pts',(-1.20895591300036,4.81939091996494,
7.33160125079922));
#155309=CARTESIAN_POINT('Ctrl Pts',(-1.15981566191495,4.82837914487869,
7.33059470553182));
#155310=CARTESIAN_POINT('Ctrl Pts',(-1.1069453862108,4.83808569120533,7.32900417473453));
#155311=CARTESIAN_POINT('Ctrl Pts',(-0.997209430183357,4.8583955671125,
7.32421114410252));
#155312=CARTESIAN_POINT('Ctrl Pts',(-0.944626917499339,4.86818887849713,
7.32130389107535));
#155313=CARTESIAN_POINT('Ctrl Pts',(-0.786632152526621,4.89780104677615,
7.31073322814866));
#155314=CARTESIAN_POINT('Ctrl Pts',(-0.681392523108954,4.91777540990695,
7.30123074296795));
#155315=CARTESIAN_POINT('Ctrl Pts',(-0.576449089121962,4.93794662060687,
7.28929564983784));
#155316=CARTESIAN_POINT('Ctrl Pts',(-0.867721406319706,4.689268254,7.46889463457454));
#155317=CARTESIAN_POINT('Ctrl Pts',(-0.457663876072064,4.754934719,7.51653430751444));
#155318=CARTESIAN_POINT('Ctrl Pts',(-0.0448556267016637,4.819390921,7.51899697287651));
#155319=CARTESIAN_POINT('Ctrl Pts',(-0.847780781,4.689268254,7.451930471));
#155320=CARTESIAN_POINT('Ctrl Pts',(-0.438654618,4.754934719,7.498475363));
#155321=CARTESIAN_POINT('Ctrl Pts',(-0.026891988,4.819390921,7.499951788));
#155322=CARTESIAN_POINT('Ctrl Pts',(-0.582837713,4.689268254,7.226534453));
#155323=CARTESIAN_POINT('Ctrl Pts',(-0.186086252,4.754934719,7.258533431));
#155324=CARTESIAN_POINT('Ctrl Pts',(0.211783654,4.819390921,7.246906077));
#155325=CARTESIAN_POINT('',(0.124676045108029,4.81939091820872,7.33925823720938));
#155326=CARTESIAN_POINT('Ctrl Pts',(-0.037115645,0.939268254,7.499908161));
#155327=CARTESIAN_POINT('Ctrl Pts',(0.37464459,1.004934719,7.501945886));
#155328=CARTESIAN_POINT('Ctrl Pts',(0.78415308,1.069390921,7.458894285));
#155329=CARTESIAN_POINT('Ctrl Pts',(0.201904718,0.939268254,7.24718804));
#155330=CARTESIAN_POINT('Ctrl Pts',(0.599790104,1.004934719,7.23610306));
#155331=CARTESIAN_POINT('Ctrl Pts',(0.994070541000001,1.069390921,7.18152656200001));
#155332=CARTESIAN_POINT('',(0.206665520798754,0.940053947693287,7.24705384020318));
#155333=CARTESIAN_POINT('Origin',(0.0171543106145804,0.803719061399266,
-0.190604237663627));
#155334=CARTESIAN_POINT('Ctrl Pts',(0.20666551447053,0.940053947354557,
7.24705384080662));
#155335=CARTESIAN_POINT('Ctrl Pts',(0.20798572187948,0.946939351516512,
7.28863807645421));
#155336=CARTESIAN_POINT('Ctrl Pts',(0.209327926431948,0.953652683633494,
7.33027599541269));
#155337=CARTESIAN_POINT('Ctrl Pts',(0.212049360335663,0.96674613250779,
7.41355144745307));
#155338=CARTESIAN_POINT('Ctrl Pts',(0.213430188150455,0.973133921158012,
7.45523782159286));
#155339=CARTESIAN_POINT('Ctrl Pts',(0.214827964027396,0.979367659147288,
7.49692263175492));
#155340=CARTESIAN_POINT('Ctrl Pts',(1.271438263,1.069390921,7.391444023));
#155341=CARTESIAN_POINT('Ctrl Pts',(1.671968444,1.004503495,7.32254687700001));
#155342=CARTESIAN_POINT('Ctrl Pts',(2.062708312,0.939276009000001,7.21077211));
#155343=CARTESIAN_POINT('Ctrl Pts',(0.994070541,1.069390921,7.181526562));
#155344=CARTESIAN_POINT('Ctrl Pts',(1.38322564,1.004503495,7.127659516));
#155345=CARTESIAN_POINT('Ctrl Pts',(1.764281177,0.939276009000001,7.03205602400001));
#155346=CARTESIAN_POINT('',(1.75973614927377,0.940053948104567,7.03319478739377));
#155347=CARTESIAN_POINT('Origin',(-0.0472960242995052,0.946431379382763,
-0.193309116276293));
#155348=CARTESIAN_POINT('Ctrl Pts',(1.82142216389955,0.979367659138093,
7.27546708476632));
#155349=CARTESIAN_POINT('Ctrl Pts',(1.81109607941231,0.973133929663875,
7.23505737799103));
#155350=CARTESIAN_POINT('Ctrl Pts',(1.80078618995315,0.966746137351372,
7.19464242018625));
#155351=CARTESIAN_POINT('Ctrl Pts',(1.7802265873758,0.953652667115658,7.11389879786013));
#155352=CARTESIAN_POINT('Ctrl Pts',(1.76996485896721,0.946939346100155,
7.07352295524683));
#155353=CARTESIAN_POINT('Ctrl Pts',(1.75973614734533,0.940053949831287,
7.03319478758808));
#155354=CARTESIAN_POINT('Ctrl Pts',(1.576010657,0.939268254,7.332543243));
#155355=CARTESIAN_POINT('Ctrl Pts',(1.978582217,1.004934719,7.246017048));
#155356=CARTESIAN_POINT('Ctrl Pts',(2.369261804,1.069390921,7.115939748));
#155357=CARTESIAN_POINT('Ctrl Pts',(1.755115501,0.939268254,7.034349265));
#155358=CARTESIAN_POINT('Ctrl Pts',(2.141315605,1.004934719,6.937989849));
#155359=CARTESIAN_POINT('Ctrl Pts',(2.51464565,1.069390921,6.79993068000001));
#155360=CARTESIAN_POINT('Origin',(-0.0242212355237648,0.803718937193291,
-0.189835864139434));
#155361=CARTESIAN_POINT('Ctrl Pts',(2.830654719,1.069390921,6.945314526));
#155362=CARTESIAN_POINT('Ctrl Pts',(3.207009877,1.004503495,6.79192600800001));
#155363=CARTESIAN_POINT('Ctrl Pts',(3.564586193,0.939276009000001,6.598766951));
#155364=CARTESIAN_POINT('Ctrl Pts',(2.51464565,1.069390921,6.79993068));
#155365=CARTESIAN_POINT('Ctrl Pts',(2.883122697,1.004503495,6.663666173));
#155366=CARTESIAN_POINT('Ctrl Pts',(3.234717443,0.939276009000001,6.488382161));
#155367=CARTESIAN_POINT('',(3.23052347474322,0.940053947055572,6.49047134645543));
#155368=CARTESIAN_POINT('Origin',(-0.0877460033529154,0.946431378272004,
-0.178622367929185));
#155369=CARTESIAN_POINT('Ctrl Pts',(3.34284868775709,0.979367659169516,
6.71381878287936));
#155370=CARTESIAN_POINT('Ctrl Pts',(3.32407710461605,0.973133921631213,
6.6765735873877));
#155371=CARTESIAN_POINT('Ctrl Pts',(3.30532024644803,0.966746133471279,
6.6393198563039));
#155372=CARTESIAN_POINT('Ctrl Pts',(3.26788383502628,0.953652667121443,
6.56488370404856));
#155373=CARTESIAN_POINT('Ctrl Pts',(3.24918240690816,0.946939345899294,
6.52765779341606));
#155374=CARTESIAN_POINT('Ctrl Pts',(3.23052347304827,0.940053949659564,
6.49047134682375));
#155375=CARTESIAN_POINT('Ctrl Pts',(3.115444452,0.939268254,6.822316752));
#155376=CARTESIAN_POINT('Ctrl Pts',(3.490003539,1.004934719,6.651272505));
#155377=CARTESIAN_POINT('Ctrl Pts',(3.84358648,1.069390921,6.440251778));
#155378=CARTESIAN_POINT('Ctrl Pts',(3.226259034,0.939268254,6.492592136));
#155379=CARTESIAN_POINT('Ctrl Pts',(3.582715568,1.004934719,6.315463943));
#155380=CARTESIAN_POINT('Ctrl Pts',(3.917638724,1.069390921,6.100377597));
#155381=CARTESIAN_POINT('Origin',(-0.0644639989330614,0.803719114066693,
-0.180190601896159));
#155382=CARTESIAN_POINT('Ctrl Pts',(4.257512905,1.069390921,6.174429841));
#155383=CARTESIAN_POINT('Ctrl Pts',(4.592095092,1.004503495,5.94372222700001));
#155384=CARTESIAN_POINT('Ctrl Pts',(4.899787985,0.939276009000001,5.67821078400001));
#155385=CARTESIAN_POINT('Ctrl Pts',(3.917638724,1.069390921,6.100377597));
#155386=CARTESIAN_POINT('Ctrl Pts',(4.248208141,1.004503495,5.888087205));
#155387=CARTESIAN_POINT('Ctrl Pts',(4.553901916,0.939276009000001,5.64131875900001));
#155388=CARTESIAN_POINT('',(4.55025511321812,0.940053947070528,5.64426067931356));
#155389=CARTESIAN_POINT('Origin',(-0.124093184552952,0.946431366950847,
-0.15558361214484));
#155390=CARTESIAN_POINT('Ctrl Pts',(4.70796732248974,0.979367659143468,
5.83823977670622));
#155391=CARTESIAN_POINT('Ctrl Pts',(4.68162799240347,0.973133921597488,
5.80590068860478));
#155392=CARTESIAN_POINT('Ctrl Pts',(4.65530120807522,0.966746133420276,
5.77355009899131));
#155393=CARTESIAN_POINT('Ctrl Pts',(4.60273846663385,0.953652667081854,
5.70890194445239));
#155394=CARTESIAN_POINT('Ctrl Pts',(4.57647179682449,0.946939345811367,
5.67656660889873));
#155395=CARTESIAN_POINT('Ctrl Pts',(4.55025511161339,0.940053949596736,
5.6442606800774));
#155396=CARTESIAN_POINT('Ctrl Pts',(4.509203528,0.939268254,5.993086312));
#155397=CARTESIAN_POINT('Ctrl Pts',(4.838236174,1.004934719,5.745521853));
#155398=CARTESIAN_POINT('Ctrl Pts',(5.138189324,1.069390921,5.46342479300001));
#155399=CARTESIAN_POINT('Ctrl Pts',(4.54654628,0.939268254,5.647248615));
#155400=CARTESIAN_POINT('Ctrl Pts',(4.85659173300001,1.004934719,5.397633963));
#155401=CARTESIAN_POINT('Ctrl Pts',(5.137447365,1.069390921,5.11557763800001));
#155402=CARTESIAN_POINT('Origin',(-0.101692449550215,0.80371912530934,-0.162119920180928));
#155403=CARTESIAN_POINT('Ctrl Pts',(5.48529452,1.069390921,5.114835679));
#155404=CARTESIAN_POINT('Ctrl Pts',(5.762459044,1.004503495,4.817596601));
#155405=CARTESIAN_POINT('Ctrl Pts',(6.005881136,0.939276009000001,4.492147791));
#155406=CARTESIAN_POINT('Ctrl Pts',(5.137447365,1.069390921,5.115577638));
#155407=CARTESIAN_POINT('Ctrl Pts',(5.414652094,1.004503495,4.837187824));
#155408=CARTESIAN_POINT('Ctrl Pts',(5.660150997,0.939276009000001,4.530473562));
#155409=CARTESIAN_POINT('',(5.65722188060532,0.940053948044077,4.53413065603272));
#155410=CARTESIAN_POINT('Origin',(-0.154637863350217,0.946431349422814,
-0.125269808525206));
#155411=CARTESIAN_POINT('Ctrl Pts',(5.8529466375557,0.979367659130068,4.68967116711043));
#155412=CARTESIAN_POINT('Ctrl Pts',(5.82027120160593,0.973133929826048,
4.66375036058833));
#155413=CARTESIAN_POINT('Ctrl Pts',(5.78760547892972,0.9667461373603,4.63781557159902));
#155414=CARTESIAN_POINT('Ctrl Pts',(5.72237416328795,0.953652667030445,
4.58597827493679));
#155415=CARTESIAN_POINT('Ctrl Pts',(5.68977045243928,0.94693934575306,4.56004547916225));
#155416=CARTESIAN_POINT('Ctrl Pts',(5.65722187920481,0.940053949524057,
4.53413065739852));
#155417=CARTESIAN_POINT('Ctrl Pts',(5.69211725800001,0.939268254,4.883625817));
#155418=CARTESIAN_POINT('Ctrl Pts',(5.960238263,1.004934719,4.571116985));
#155419=CARTESIAN_POINT('Ctrl Pts',(6.192536146,1.069390921,4.231134137));
#155420=CARTESIAN_POINT('Ctrl Pts',(5.654242076,0.939268254,4.537846025));
#155421=CARTESIAN_POINT('Ctrl Pts',(5.903379066,1.004934719,4.227416618));
#155422=CARTESIAN_POINT('Ctrl Pts',(6.117034678,1.069390921,3.891578954));
#155423=CARTESIAN_POINT('Origin',(-0.134165992850455,0.803718955617848,
-0.136468870569669));
#155424=CARTESIAN_POINT('Ctrl Pts',(6.45658986,1.069390921,3.816077485));
#155425=CARTESIAN_POINT('Ctrl Pts',(6.66337681600001,1.004503495,3.466205512));
#155426=CARTESIAN_POINT('Ctrl Pts',(6.831145961,0.939276009000001,3.096036961));
#155427=CARTESIAN_POINT('Ctrl Pts',(6.117034678,1.069390921,3.891578954));
#155428=CARTESIAN_POINT('Ctrl Pts',(6.327912933,1.004503495,3.560106917));
#155429=CARTESIAN_POINT('Ctrl Pts',(6.501737708,0.939276009000001,3.207788456));
#155430=CARTESIAN_POINT('',(6.49966323932527,0.940053947076377,3.21198972307322));
#155431=CARTESIAN_POINT('Origin',(-0.177951791258012,0.946431387463854,
-0.0890984797086419));
#155432=CARTESIAN_POINT('Ctrl Pts',(6.72424867288718,0.979367659151059,
3.32181874645751));
#155433=CARTESIAN_POINT('Ctrl Pts',(6.68676491361813,0.973133921588396,
3.30352818266222));
#155434=CARTESIAN_POINT('Ctrl Pts',(6.64928771115034,0.96674613337873,3.28522191245718));
#155435=CARTESIAN_POINT('Ctrl Pts',(6.57443800366579,0.953652667026606,
3.2486193585997));
#155436=CARTESIAN_POINT('Ctrl Pts',(6.53702176458215,0.946939345686209,
3.23030169093364));
#155437=CARTESIAN_POINT('Ctrl Pts',(6.49966323833265,0.940053949471073,
3.21198972419785));
#155438=CARTESIAN_POINT('Ctrl Pts',(6.608873911,0.939268254,3.545812407));
#155439=CARTESIAN_POINT('Ctrl Pts',(6.803546235,1.004934719,3.182971767));
#155440=CARTESIAN_POINT('Ctrl Pts',(6.95732686000001,1.069390921,2.80100035));
#155441=CARTESIAN_POINT('Ctrl Pts',(6.49755179600001,0.939268254,3.216258799));
#155442=CARTESIAN_POINT('Ctrl Pts',(6.674130955,1.004934719,2.85952997));
#155443=CARTESIAN_POINT('Ctrl Pts',(6.810596247,1.069390921,2.485614363));
#155444=CARTESIAN_POINT('Origin',(-0.160366188329994,0.80371906941477,-0.104436620283826));
#155445=CARTESIAN_POINT('Ctrl Pts',(7.125982234,1.069390921,2.33888375));
#155446=CARTESIAN_POINT('Ctrl Pts',(7.252722494,1.004503495,1.952738506));
#155447=CARTESIAN_POINT('Ctrl Pts',(7.33699399300001,0.939276009000001,
1.555158883));
#155448=CARTESIAN_POINT('Ctrl Pts',(6.810596247,1.069390921,2.485614363));
#155449=CARTESIAN_POINT('Ctrl Pts',(6.945287596,1.004503495,2.116559367));
#155450=CARTESIAN_POINT('Ctrl Pts',(7.03931039,0.939276009000001,1.735110727));
#155451=CARTESIAN_POINT('',(7.03818757051311,0.940053948728594,1.73965971993727));
#155452=CARTESIAN_POINT('Origin',(-0.192944911291157,0.946431408256025,
-0.0487610407518779));
#155453=CARTESIAN_POINT('Ctrl Pts',(7.2811323139677,0.9793676591109,1.79864177274421));
#155454=CARTESIAN_POINT('Ctrl Pts',(7.24059302186394,0.973133928980762,
1.78883674406157));
#155455=CARTESIAN_POINT('Ctrl Pts',(7.20005668258872,0.966746136965024,
1.77901494874504));
#155456=CARTESIAN_POINT('Ctrl Pts',(7.11908843034966,0.953652667076533,
1.75935861156909));
#155457=CARTESIAN_POINT('Ctrl Pts',(7.078609206097,0.946939345946012,1.74951258654573));
#155458=CARTESIAN_POINT('Ctrl Pts',(7.03818756973805,0.94005394976175,1.73965972239499));
#155459=CARTESIAN_POINT('Ctrl Pts',(7.21660696600001,0.939268254,2.042200749));
#155460=CARTESIAN_POINT('Ctrl Pts',(7.328727947,1.004934719,1.645994327));
#155461=CARTESIAN_POINT('Ctrl Pts',(7.396800703,1.069390921,1.239894901));
#155462=CARTESIAN_POINT('Ctrl Pts',(7.037043215,0.939268254,1.744282886));
#155463=CARTESIAN_POINT('Ctrl Pts',(7.13280789900001,1.004934719,1.357934879));
#155464=CARTESIAN_POINT('Ctrl Pts',(7.18570190500001,1.069390921,0.963425207));
#155465=CARTESIAN_POINT('Origin',(-0.17906743711432,0.803719095684063,-0.0675208998158564));
#155466=CARTESIAN_POINT('Ctrl Pts',(7.462171599,1.069390921,0.75232641));
#155467=CARTESIAN_POINT('Ctrl Pts',(7.502938928,1.004503495,0.347963618));
#155468=CARTESIAN_POINT('Ctrl Pts',(7.49977234,0.939276009000001,-0.058436696));
#155469=CARTESIAN_POINT('Ctrl Pts',(7.185701905,1.069390921,0.963425207));
#155470=CARTESIAN_POINT('Ctrl Pts',(7.237908331,1.004503495,0.574043853));
#155471=CARTESIAN_POINT('Ctrl Pts',(7.247732742,0.939276009000001,0.181301149));
#155472=CARTESIAN_POINT('',(7.2476140724582,0.94005394809245,0.185985162743354));
#155473=CARTESIAN_POINT('Origin',(-0.198915958460675,0.946431400007768,
-0.00614357805642111));
#155474=CARTESIAN_POINT('Ctrl Pts',(7.49755829989574,0.979367659085542,
0.191362308830966));
#155475=CARTESIAN_POINT('Ctrl Pts',(7.45585900341291,0.973133929072959,
0.190501265756741));
#155476=CARTESIAN_POINT('Ctrl Pts',(7.41415898547609,0.966746137041716,
0.18962321328262));
#155477=CARTESIAN_POINT('Ctrl Pts',(7.3308581944993,0.953652667140489,0.187832211268411));
#155478=CARTESIAN_POINT('Ctrl Pts',(7.28920874762298,0.946939345996497,
0.186918217560852));
#155479=CARTESIAN_POINT('Ctrl Pts',(7.2476140721247,0.940053949810692,0.185985164931034));
#155480=CARTESIAN_POINT('Ctrl Pts',(7.48689949900001,0.939268254,0.443098054));
#155481=CARTESIAN_POINT('Ctrl Pts',(7.511226485,1.004934719,0.032052021));
#155482=CARTESIAN_POINT('Ctrl Pts',(7.49040836500001,1.069390921,-0.379186656));
#155483=CARTESIAN_POINT('Ctrl Pts',(7.247490315,0.939268254,0.190746244));
#155484=CARTESIAN_POINT('Ctrl Pts',(7.257962673,1.004934719,-0.207155738));
#155485=CARTESIAN_POINT('Ctrl Pts',(7.224812129,1.069390921,-0.603812641));
#155486=CARTESIAN_POINT('Origin',(-0.189396225307447,0.803718964998261,
-0.0274481071492917));
#155487=CARTESIAN_POINT('Ctrl Pts',(7.449438113,1.069390921,-0.869408877000001));
#155488=CARTESIAN_POINT('Ctrl Pts',(7.402326278,1.004503495,-1.273081663));
#155489=CARTESIAN_POINT('Ctrl Pts',(7.311869668,0.939276009000001,-1.66929984));
#155490=CARTESIAN_POINT('Ctrl Pts',(7.224812129,1.069390921,-0.603812640999999));
#155491=CARTESIAN_POINT('Ctrl Pts',(7.192092516,1.004503495,-0.995313314));
#155492=CARTESIAN_POINT('Ctrl Pts',(7.117259166,0.939276009000001,-1.380985869));
#155493=CARTESIAN_POINT('',(7.11815019522468,0.940053947080983,-1.37638585417308));
#155494=CARTESIAN_POINT('Origin',(-0.195586225751974,0.946431364602441,
0.0367611360511885));
#155495=CARTESIAN_POINT('Ctrl Pts',(7.36340679335851,0.979367659166656,
-1.42486504376531));
#155496=CARTESIAN_POINT('Ctrl Pts',(7.32249725512431,0.973133921633095,
-1.41674183026556));
#155497=CARTESIAN_POINT('Ctrl Pts',(7.28158343164316,0.966746133459874,
-1.40863508849938));
#155498=CARTESIAN_POINT('Ctrl Pts',(7.19984517687634,0.95365266713448,-1.39247701472651));
#155499=CARTESIAN_POINT('Ctrl Pts',(7.15897298894388,0.946939345913326,
-1.38441623981205));
#155500=CARTESIAN_POINT('Ctrl Pts',(7.11815019511434,0.940053949699928,
-1.37638585248842));
#155501=CARTESIAN_POINT('Ctrl Pts',(7.407112933,0.939268254,-1.176723413));
#155502=CARTESIAN_POINT('Ctrl Pts',(7.342508421,1.004934719,-1.583389001));
#155503=CARTESIAN_POINT('Ctrl Pts',(7.233772858,1.069390921,-1.980537866));
#155504=CARTESIAN_POINT('Ctrl Pts',(7.119052823,0.939268254,-1.371709481));
#155505=CARTESIAN_POINT('Ctrl Pts',(7.043743179,1.004934719,-1.762559983));
#155506=CARTESIAN_POINT('Ctrl Pts',(6.926098167,1.069390921,-2.14281688));
#155507=CARTESIAN_POINT('Origin',(-0.19086840065011,0.80371912887615,0.0139081448841));
#155508=CARTESIAN_POINT('Ctrl Pts',(7.08837718100001,1.069390921,-2.450491571));
#155509=CARTESIAN_POINT('Ctrl Pts',(6.955589078,1.004503495,-2.834599059));
#155510=CARTESIAN_POINT('Ctrl Pts',(6.78207209700001,0.939276009000001,
-3.202108379));
#155511=CARTESIAN_POINT('Ctrl Pts',(6.926098167,1.069390921,-2.14281688));
#155512=CARTESIAN_POINT('Ctrl Pts',(6.809982448,1.004503495,-2.518130736));
#155513=CARTESIAN_POINT('Ctrl Pts',(6.653990461,0.939276009000001,-2.878699522));
#155514=CARTESIAN_POINT('',(6.65584952602707,0.940053947074734,-2.87439859900565));
#155515=CARTESIAN_POINT('Origin',(-0.183110903818539,0.946431324714851,
0.0779469181040487));
#155516=CARTESIAN_POINT('Ctrl Pts',(6.88495056874341,0.979367659097039,
-2.97446729084826));
#155517=CARTESIAN_POINT('Ctrl Pts',(6.84674376983869,0.973133929140185,
-2.95773967239493));
#155518=CARTESIAN_POINT('Ctrl Pts',(6.80852917359771,0.966746137080596,
-2.94102718811594));
#155519=CARTESIAN_POINT('Ctrl Pts',(6.73217540049579,0.953652667102936,
-2.90767556313915));
#155520=CARTESIAN_POINT('Ctrl Pts',(6.69399161031049,0.946939345963208,
-2.89101693261409));
#155521=CARTESIAN_POINT('Ctrl Pts',(6.65584952632392,0.940053949701299,
-2.87439859723607));
#155522=CARTESIAN_POINT('Ctrl Pts',(6.980977999,0.939268254,-2.741522602));
#155523=CARTESIAN_POINT('Ctrl Pts',(6.830462824,1.004934719,-3.124792514));
#155524=CARTESIAN_POINT('Ctrl Pts',(6.638894171,1.069390921,-3.489281327));
#155525=CARTESIAN_POINT('Ctrl Pts',(6.657736333,0.939268254,-2.870025595));
#155526=CARTESIAN_POINT('Ctrl Pts',(6.500166082,1.004934719,-3.235548881));
#155527=CARTESIAN_POINT('Ctrl Pts',(6.303527553,1.069390921,-3.581625384));
#155528=CARTESIAN_POINT('Origin',(-0.183416398185337,0.803719072608364,
0.0546141480222323));
#155529=CARTESIAN_POINT('Ctrl Pts',(6.39587161,1.069390921,-3.916992003));
#155530=CARTESIAN_POINT('Ctrl Pts',(6.183616263,1.004503495,-4.263573754));
#155531=CARTESIAN_POINT('Ctrl Pts',(5.935152372,0.939276009000001,-4.585189889));
#155532=CARTESIAN_POINT('Ctrl Pts',(6.303527553,1.069390921,-3.581625384));
#155533=CARTESIAN_POINT('Ctrl Pts',(6.10944517,1.004503495,-3.923203163));
#155534=CARTESIAN_POINT('Ctrl Pts',(5.87958855800001,0.939276009000001,
-4.241808386));
#155535=CARTESIAN_POINT('',(5.88232873095194,0.940053948109766,-4.23800766024314));
#155536=CARTESIAN_POINT('Origin',(-0.162073690401495,0.946431358264443,
0.115488049280784));
#155537=CARTESIAN_POINT('Ctrl Pts',(6.08456170750433,0.979367659144574,
-4.38498675280478));
#155538=CARTESIAN_POINT('Ctrl Pts',(6.05084410437289,0.973133928914535,
-4.36043688345674));
#155539=CARTESIAN_POINT('Ctrl Pts',(6.01711563512004,0.966746137004887,
-4.33590011995558));
#155540=CARTESIAN_POINT('Ctrl Pts',(5.9497165849654,0.953652667153041,-4.28691443395892));
#155541=CARTESIAN_POINT('Ctrl Pts',(5.91600662413242,0.946939346097956,
-4.26243688720522));
#155542=CARTESIAN_POINT('Ctrl Pts',(5.88232873168166,0.940053949827562,
-4.238007658753));
#155543=CARTESIAN_POINT('Ctrl Pts',(6.22842029200001,0.939268254,-4.17813124));
#155544=CARTESIAN_POINT('Ctrl Pts',(5.999032377,1.004934719,-4.520084201));
#155545=CARTESIAN_POINT('Ctrl Pts',(5.733588172,1.069390921,-4.83486987100001));
#155546=CARTESIAN_POINT('Ctrl Pts',(5.885111492,0.939268254,-4.234142502));
#155547=CARTESIAN_POINT('Ctrl Pts',(5.652648444,1.004934719,-4.557247111));
#155548=CARTESIAN_POINT('Ctrl Pts',(5.38621099600001,1.069390921,-4.852961066));
#155549=CARTESIAN_POINT('Origin',(-0.167387900493161,0.803718943983406,
0.0927664531750083));
#155550=CARTESIAN_POINT('Ctrl Pts',(5.40430219,1.069390921,-5.200338242));
#155551=CARTESIAN_POINT('Ctrl Pts',(5.122504424,1.004503495,-5.493188479));
#155552=CARTESIAN_POINT('Ctrl Pts',(4.810711519,0.939276009000001,-5.753873015));
#155553=CARTESIAN_POINT('Ctrl Pts',(5.386210996,1.069390921,-4.852961066));
#155554=CARTESIAN_POINT('Ctrl Pts',(5.123237026,1.004503495,-5.144830971));
#155555=CARTESIAN_POINT('Ctrl Pts',(4.830263629,0.939276009000001,-5.406575004));
#155556=CARTESIAN_POINT('',(4.83375678100282,0.940053947060246,-5.40345219171606));
#155557=CARTESIAN_POINT('Origin',(-0.133457977517737,0.946431359286523,
0.147629070274841));
#155558=CARTESIAN_POINT('Ctrl Pts',(4.99966550307941,0.979367659095725,
-5.59046910848041));
#155559=CARTESIAN_POINT('Ctrl Pts',(4.97201370358805,0.973133930785602,
-5.559244922896));
#155560=CARTESIAN_POINT('Ctrl Pts',(4.94434846128487,0.96674613782819,-5.52803118575712));
#155561=CARTESIAN_POINT('Ctrl Pts',(4.88905563426153,0.953652667068031,
-5.46570194974581));
#155562=CARTESIAN_POINT('Ctrl Pts',(4.86139574168978,0.946939345779763,
-5.43455002807549));
#155563=CARTESIAN_POINT('Ctrl Pts',(4.83375678201755,0.940053949586176,
-5.40345219025493));
#155564=CARTESIAN_POINT('Ctrl Pts',(5.184628575,0.939268254,-5.419375106));
#155565=CARTESIAN_POINT('Ctrl Pts',(4.88709384300001,1.004934719,-5.704021776));
#155566=CARTESIAN_POINT('Ctrl Pts',(4.56018596200001,1.069390921,-5.954385274));
#155567=CARTESIAN_POINT('Ctrl Pts',(4.837305378,0.939268254,-5.400275611));
#155568=CARTESIAN_POINT('Ctrl Pts',(4.540819247,1.004934719,-5.66585353));
#155569=CARTESIAN_POINT('Ctrl Pts',(4.217041199,1.069390921,-5.897377682));
#155570=CARTESIAN_POINT('Origin',(-0.143532263022791,0.803719077910381,
0.126580913646047));
#155571=CARTESIAN_POINT('Ctrl Pts',(4.160033607,1.069390921,-6.24052244500001));
#155572=CARTESIAN_POINT('Ctrl Pts',(3.821869971,1.004503495,-6.46594781600001));
#155573=CARTESIAN_POINT('Ctrl Pts',(3.461327142,0.939276009000001,-6.65351143500001));
#155574=CARTESIAN_POINT('Ctrl Pts',(4.217041199,1.069390921,-5.897377682));
#155575=CARTESIAN_POINT('Ctrl Pts',(3.897472013,1.004503495,-6.125892201));
#155576=CARTESIAN_POINT('Ctrl Pts',(3.555080941,0.939276009000001,-6.31853618300001));
#155577=CARTESIAN_POINT('',(3.55916373788445,0.940053947075642,-6.31623730607955));
#155578=CARTESIAN_POINT('Origin',(-0.0986017871388895,0.946431370250801,
0.172866876304308));
#155579=CARTESIAN_POINT('Ctrl Pts',(3.68099049666104,0.979367659141269,
-6.53454734171104));
#155580=CARTESIAN_POINT('Ctrl Pts',(3.66069745649746,0.973133930415714,
-6.49810883838615));
#155581=CARTESIAN_POINT('Ctrl Pts',(3.64038904380532,0.966746137680773,
-6.46167765320151));
#155582=CARTESIAN_POINT('Ctrl Pts',(3.59978787616403,0.953652667071589,
-6.38891931766773));
#155583=CARTESIAN_POINT('Ctrl Pts',(3.57947139933411,0.946939345954821,
-6.35254965228124));
#155584=CARTESIAN_POINT('Ctrl Pts',(3.55916373886498,0.940053949718943,
-6.31623730502998));
#155585=CARTESIAN_POINT('Ctrl Pts',(3.898409388,0.939268254,-6.407215015));
#155586=CARTESIAN_POINT('Ctrl Pts',(3.546640232,1.004934719,-6.621245631));
#155587=CARTESIAN_POINT('Ctrl Pts',(3.173554525,1.069390921,-6.79548023900001));
#155588=CARTESIAN_POINT('Ctrl Pts',(3.563312241,0.939268254,-6.313897835));
#155589=CARTESIAN_POINT('Ctrl Pts',(3.216666389,1.004934719,-6.509530936));
#155590=CARTESIAN_POINT('Ctrl Pts',(2.850687243,1.069390921,-6.666039472));
#155591=CARTESIAN_POINT('Origin',(-0.112965338103565,0.803719091406703,
0.154476604966692));
#155592=CARTESIAN_POINT('Ctrl Pts',(2.721246476,1.069390921,-6.988906754));
#155593=CARTESIAN_POINT('Ctrl Pts',(2.342529127,1.004503495,-7.13636662));
#155594=CARTESIAN_POINT('Ctrl Pts',(1.950094955,0.939276009000001,-7.242039054));
#155595=CARTESIAN_POINT('Ctrl Pts',(2.850687243,1.069390921,-6.666039472));
#155596=CARTESIAN_POINT('Ctrl Pts',(2.48946554,1.004503495,-6.82051352));
#155597=CARTESIAN_POINT('Ctrl Pts',(2.11366662,0.939276009000001,-6.935049634));
#155598=CARTESIAN_POINT('',(2.11814815318168,0.940053947040107,-6.93368218303118));
#155599=CARTESIAN_POINT('Origin',(-0.0591353114936999,0.946431348139323,
0.190021965440267));
#155600=CARTESIAN_POINT('Ctrl Pts',(2.19019646628857,0.979367659164797,
-7.1730774035426));
#155601=CARTESIAN_POINT('Ctrl Pts',(2.17821106626055,0.97313392993309,-7.13312840511824));
#155602=CARTESIAN_POINT('Ctrl Pts',(2.1662090814254,0.96674613745119,-7.09318325406989));
#155603=CARTESIAN_POINT('Ctrl Pts',(2.14219803858705,0.953652667117197,
-7.01339791887875));
#155604=CARTESIAN_POINT('Ctrl Pts',(2.13017495246056,0.946939345817816,
-6.97351111311087));
#155605=CARTESIAN_POINT('Ctrl Pts',(2.11814815529179,0.940053949598351,
-6.93368218195176));
#155606=CARTESIAN_POINT('Ctrl Pts',(2.429904911,0.939268254,-7.09546067));
#155607=CARTESIAN_POINT('Ctrl Pts',(2.040349667,1.004934719,-7.2288674));
#155608=CARTESIAN_POINT('Ctrl Pts',(1.638531205,1.069390921,-7.3188261));
#155609=CARTESIAN_POINT('Ctrl Pts',(2.122702584,0.939268254,-6.932289213));
#155610=CARTESIAN_POINT('Ctrl Pts',(1.742105785,1.004934719,-7.04882990900001));
#155611=CARTESIAN_POINT('Ctrl Pts',(1.35103832,1.069390921,-7.123004665));
#155612=CARTESIAN_POINT('Origin',(-0.0771164253396961,0.803719107667327,
0.175149470351337));
#155613=CARTESIAN_POINT('Ctrl Pts',(1.155216884,1.069390921,-7.410497551));
#155614=CARTESIAN_POINT('Ctrl Pts',(0.753654224,1.004503495,-7.473096852));
#155615=CARTESIAN_POINT('Ctrl Pts',(0.347678495,0.939276009000001,-7.491936977));
#155616=CARTESIAN_POINT('Ctrl Pts',(1.35103832,1.069390921,-7.123004665));
#155617=CARTESIAN_POINT('Ctrl Pts',(0.965054424999999,1.004503495,-7.196215207));
#155618=CARTESIAN_POINT('Ctrl Pts',(0.573419596,0.939276009000001,-7.227287871));
#155619=CARTESIAN_POINT('',(0.578090315769932,0.940053947054566,-7.22691578804911));
#155620=CARTESIAN_POINT('Origin',(-0.0169036609396048,0.946431334859754,
0.198291733152491));
#155621=CARTESIAN_POINT('Ctrl Pts',(0.596991283107538,0.97936765917447,
-7.47620233865752));
#155622=CARTESIAN_POINT('Ctrl Pts',(0.593873944611415,0.973133921644323,
-7.43461076353645));
#155623=CARTESIAN_POINT('Ctrl Pts',(0.590739588336705,0.966746133474978,
-7.3930194660492));
#155624=CARTESIAN_POINT('Ctrl Pts',(0.584441400587957,0.953652667122777,
-7.30993782852173));
#155625=CARTESIAN_POINT('Ctrl Pts',(0.581273891583116,0.946939345895764,
-7.26839894647513));
#155626=CARTESIAN_POINT('Ctrl Pts',(0.578090316875115,0.940053949636729,
-7.2269157875357));
#155627=CARTESIAN_POINT('Ctrl Pts',(0.847780781,0.939268254,-7.451930471));
#155628=CARTESIAN_POINT('Ctrl Pts',(0.438654618,1.004934719,-7.498475363));
#155629=CARTESIAN_POINT('Ctrl Pts',(0.026891988,1.069390921,-7.499951788));
#155630=CARTESIAN_POINT('Ctrl Pts',(0.582837713,0.939268254,-7.226534453));
#155631=CARTESIAN_POINT('Ctrl Pts',(0.186086252,1.004934719,-7.258533431));
#155632=CARTESIAN_POINT('Ctrl Pts',(-0.211783654,1.069390921,-7.246906077));
#155633=CARTESIAN_POINT('Origin',(-0.0376615330110996,0.803719054725182,
0.187632234918865));
#155634=CARTESIAN_POINT('Ctrl Pts',(-0.464829365,1.069390921,-7.485581718));
#155635=CARTESIAN_POINT('Ctrl Pts',(-0.870460713,1.004503495,-7.46039338));
#155636=CARTESIAN_POINT('Ctrl Pts',(-1.270995025,0.939276009000001,-7.391520253));
#155637=CARTESIAN_POINT('Ctrl Pts',(-0.211783654,1.069390921,-7.246906077));
#155638=CARTESIAN_POINT('Ctrl Pts',(-0.604481562,1.004503495,-7.23542986900001));
#155639=CARTESIAN_POINT('Ctrl Pts',(-0.993639891,0.939276009000001,-7.18158616));
#155640=CARTESIAN_POINT('',(-0.988998383218434,0.940053947070287,-7.18222684270956));
#155641=CARTESIAN_POINT('Origin',(0.0261184061910333,0.946431356628239,
0.197289686170977));
#155642=CARTESIAN_POINT('Ctrl Pts',(-1.02412854958253,0.979367659146776,
-7.42974836134486));
#155643=CARTESIAN_POINT('Ctrl Pts',(-1.0182320549564,0.973133929868704,
-7.38845909318597));
#155644=CARTESIAN_POINT('Ctrl Pts',(-1.01235222786181,0.966746137434024,
-7.34716635363524));
#155645=CARTESIAN_POINT('Ctrl Pts',(-1.00064306753657,0.953652667137174,
-7.26467316949527));
#155646=CARTESIAN_POINT('Ctrl Pts',(-0.994806890059517,0.946939345921978,
-7.22342452261311));
#155647=CARTESIAN_POINT('Ctrl Pts',(-0.9889983814996,0.940053949703201,
-7.18222684251186));
#155648=CARTESIAN_POINT('Ctrl Pts',(-0.773984637,0.939268254,-7.45995628600001));
#155649=CARTESIAN_POINT('Ctrl Pts',(-1.183551433,1.004934719,-7.417462952));
#155650=CARTESIAN_POINT('Ctrl Pts',(-1.586004669,1.069390921,-7.330388065));
#155651=CARTESIAN_POINT('Ctrl Pts',(-0.984280001000001,0.939268254,-7.182874973));
#155652=CARTESIAN_POINT('Ctrl Pts',(-1.378634468,1.004934719,-7.128835996));
#155653=CARTESIAN_POINT('Ctrl Pts',(-1.764702859,1.069390921,-7.03195021400001));
#155654=CARTESIAN_POINT('Origin',(0.00355437245078333,0.803719069914868,
0.191341631743444));
#155655=CARTESIAN_POINT('Ctrl Pts',(-2.06314071,1.069390921,-7.210648404));
#155656=CARTESIAN_POINT('Ctrl Pts',(-2.453873874,1.004503495,-7.098850206));
#155657=CARTESIAN_POINT('Ctrl Pts',(-2.83023823,0.939276009000001,-6.945484257));
#155658=CARTESIAN_POINT('Ctrl Pts',(-1.764702859,1.069390921,-7.03195021400001));
#155659=CARTESIAN_POINT('Ctrl Pts',(-2.145752663,1.004503495,-6.936323872));
#155660=CARTESIAN_POINT('Ctrl Pts',(-2.51423788,0.939276009000001,-6.800081461));
#155661=CARTESIAN_POINT('',(-2.50984261641908,0.940053947041797,-6.80170495217655));
#155662=CARTESIAN_POINT('Origin',(0.0679191305552662,0.946431346107127,
0.187062182692088));
#155663=CARTESIAN_POINT('Ctrl Pts',(-2.59736126895321,0.979367659134186,
-7.0358876083094));
#155664=CARTESIAN_POINT('Ctrl Pts',(-2.58272665904198,0.973133929858945,
-6.99683123235415));
#155665=CARTESIAN_POINT('Ctrl Pts',(-2.56810758069108,0.966746137396923,
-6.95776788295547));
#155666=CARTESIAN_POINT('Ctrl Pts',(-2.53893857804772,0.953652667032495,
-6.87972046655708));
#155667=CARTESIAN_POINT('Ctrl Pts',(-2.52437160761352,0.946939345850515,
-6.84069079594145));
#155668=CARTESIAN_POINT('Ctrl Pts',(-2.50984261543138,0.940053949591765,
-6.80170495209428));
#155669=CARTESIAN_POINT('Ctrl Pts',(-2.359559393,0.939268254,-7.119162835));
#155670=CARTESIAN_POINT('Ctrl Pts',(-2.750415934,1.004934719,-6.98961821800001));
#155671=CARTESIAN_POINT('Ctrl Pts',(-3.124741511,1.069390921,-6.818063544));
#155672=CARTESIAN_POINT('Ctrl Pts',(-2.505373877,0.939268254,-6.803352243));
#155673=CARTESIAN_POINT('Ctrl Pts',(-2.878891773,1.004934719,-6.665802114));
#155674=CARTESIAN_POINT('Ctrl Pts',(-3.23510652,1.069390921,-6.488188176));
#155675=CARTESIAN_POINT('Origin',(0.0446040535888903,0.803719077786697,
0.186104077523978));
#155676=CARTESIAN_POINT('Ctrl Pts',(-3.564981888,1.069390921,-6.59855318500001));
#155677=CARTESIAN_POINT('Ctrl Pts',(-3.922546621,1.004503495,-6.405372686));
#155678=CARTESIAN_POINT('Ctrl Pts',(-4.257142641,0.939276009000001,-6.174685136));
#155679=CARTESIAN_POINT('Ctrl Pts',(-3.23510652,1.069390921,-6.488188176));
#155680=CARTESIAN_POINT('Ctrl Pts',(-3.586690754,1.004503495,-6.31288308));
#155681=CARTESIAN_POINT('Ctrl Pts',(-3.917272901,0.939276009000001,-6.100612512));
#155682=CARTESIAN_POINT('',(-3.91332939950011,0.940053948078126,-6.10314289857884));
#155683=CARTESIAN_POINT('Origin',(0.106544188480028,0.946431356239456,0.168088403438719));
#155684=CARTESIAN_POINT('Ctrl Pts',(-4.04914426237965,0.979367659183749,
-6.31303657046451));
#155685=CARTESIAN_POINT('Ctrl Pts',(-4.02645583639741,0.973133930248886,
-6.27803932140032));
#155686=CARTESIAN_POINT('Ctrl Pts',(-4.00378107790911,0.966746137632722,
-6.24303192029114));
#155687=CARTESIAN_POINT('Ctrl Pts',(-3.95851614221157,0.95365266713256,
-6.17307968194312));
#155688=CARTESIAN_POINT('Ctrl Pts',(-3.93589951412828,0.946939346036999,
-6.13809397195536));
#155689=CARTESIAN_POINT('Ctrl Pts',(-3.91332939753396,0.940053949787857,
-6.10314289951169));
#155690=CARTESIAN_POINT('Ctrl Pts',(-3.834803774,0.939268254,-6.44548524300001));
#155691=CARTESIAN_POINT('Ctrl Pts',(-4.188674043,1.004934719,-6.234946704));
#155692=CARTESIAN_POINT('Ctrl Pts',(-4.517368912,1.069390921,-5.98693394900001));
#155693=CARTESIAN_POINT('Ctrl Pts',(-3.909319254,0.939268254,-6.105712323));
#155694=CARTESIAN_POINT('Ctrl Pts',(-4.244535298,1.004934719,-5.891082733));
#155695=CARTESIAN_POINT('Ctrl Pts',(-4.554240196,1.069390921,-5.64104566900001));
#155696=CARTESIAN_POINT('Origin',(0.08356823025853,0.80371894377527,0.172164714886629));
#155697=CARTESIAN_POINT('Ctrl Pts',(-4.900128476,1.069390921,-5.677916952));
#155698=CARTESIAN_POINT('Ctrl Pts',(-5.207805447,1.004503495,-5.412387059));
#155699=CARTESIAN_POINT('Ctrl Pts',(-5.484987794,0.939276009000001,-5.115164602));
#155700=CARTESIAN_POINT('Ctrl Pts',(-4.554240196,1.069390921,-5.641045669));
#155701=CARTESIAN_POINT('Ctrl Pts',(-4.859919172,1.004503495,-5.394258892));
#155702=CARTESIAN_POINT('Ctrl Pts',(-5.137140595,0.939276009000001,-5.115885701));
#155703=CARTESIAN_POINT('',(-5.13383324781926,0.940053948082874,-5.11920466472028));
#155704=CARTESIAN_POINT('Origin',(0.140187158168336,0.9464314117376,0.141254600293041));
#155705=CARTESIAN_POINT('Ctrl Pts',(-5.31159377033098,0.979367659185378,
-5.29499495970319));
#155706=CARTESIAN_POINT('Ctrl Pts',(-5.28191237207512,0.973133921633951,
-5.26569322721615));
#155707=CARTESIAN_POINT('Ctrl Pts',(-5.2522422024183,0.966746133433956,
-5.23637870407356));
#155708=CARTESIAN_POINT('Ctrl Pts',(-5.1929978910845,0.953652667097977,
-5.17779255156783));
#155709=CARTESIAN_POINT('Ctrl Pts',(-5.16338913336467,0.946939345930828,
-5.14848669395025));
#155710=CARTESIAN_POINT('Ctrl Pts',(-5.13383324626273,0.940053949730156,
-5.11920466590403));
#155711=CARTESIAN_POINT('Ctrl Pts',(-5.130736993,0.939268254,-5.47042392400001));
#155712=CARTESIAN_POINT('Ctrl Pts',(-5.431074409,1.004934719,-5.188736012));
#155713=CARTESIAN_POINT('Ctrl Pts',(-5.698769164,1.069390921,-4.875861977));
#155714=CARTESIAN_POINT('Ctrl Pts',(-5.130469208,0.939268254,-5.12257608100001));
#155715=CARTESIAN_POINT('Ctrl Pts',(-5.41170907,1.004934719,-4.840902871));
#155716=CARTESIAN_POINT('Ctrl Pts',(-5.660422662,1.069390921,-4.530134136));
#155717=CARTESIAN_POINT('Origin',(0.11862458411581,0.80371897769967,0.15017473186036));
#155718=CARTESIAN_POINT('Ctrl Pts',(-6.006150502,1.069390921,-4.491787634));
#155719=CARTESIAN_POINT('Ctrl Pts',(-6.249553078,1.004503495,-4.166324228));
#155720=CARTESIAN_POINT('Ctrl Pts',(-6.456361013,0.939276009000001,-3.816464655));
#155721=CARTESIAN_POINT('Ctrl Pts',(-5.660422662,1.069390921,-4.530134136));
#155722=CARTESIAN_POINT('Ctrl Pts',(-5.905903171,1.004503495,-4.223405152));
#155723=CARTESIAN_POINT('Ctrl Pts',(-6.116801304,0.939276009000001,-3.891945762));
#155724=CARTESIAN_POINT('',(-6.11428476024431,0.940053948058558,-3.89589811155744));
#155725=CARTESIAN_POINT('Origin',(0.16727548068703,0.946431357451162,0.107816230720738));
#155726=CARTESIAN_POINT('Ctrl Pts',(-6.32567905648818,0.979367659135639,
-4.02936526868395));
#155727=CARTESIAN_POINT('Ctrl Pts',(-6.29039262764721,0.973133928858821,
-4.00712924358955));
#155728=CARTESIAN_POINT('Ctrl Pts',(-6.25511435220885,0.966746136961554,
-3.98487827339719));
#155729=CARTESIAN_POINT('Ctrl Pts',(-6.18466083040325,0.953652667160767,
-3.94039759680165));
#155730=CARTESIAN_POINT('Ctrl Pts',(-6.14944441594141,0.94693934598928,
-3.91814190177741));
#155731=CARTESIAN_POINT('Ctrl Pts',(-6.11428475859154,0.940053949754415,
-3.89589811364495));
#155732=CARTESIAN_POINT('Ctrl Pts',(-6.186762652,0.939268254,-4.239571663));
#155733=CARTESIAN_POINT('Ctrl Pts',(-6.419523772,1.004934719,-3.899905791));
#155734=CARTESIAN_POINT('Ctrl Pts',(-6.61370130300001,1.069390921,-3.536800117));
#155735=CARTESIAN_POINT('Ctrl Pts',(-6.111724124,0.939268254,-3.899913875));
#155736=CARTESIAN_POINT('Ctrl Pts',(-6.32583734,1.004934719,-3.564367771));
#155737=CARTESIAN_POINT('Ctrl Pts',(-6.501930055,1.069390921,-3.207398566));
#155738=CARTESIAN_POINT('Origin',(0.148134494418555,0.80371897014872,0.121163037150532));
#155739=CARTESIAN_POINT('Ctrl Pts',(-6.831331606,1.069390921,-3.095627318));
#155740=CARTESIAN_POINT('Ctrl Pts',(-6.999078553,1.004503495,-2.725448706));
#155741=CARTESIAN_POINT('Ctrl Pts',(-7.12584196800001,0.939276009000001,
-2.339311063));
#155742=CARTESIAN_POINT('Ctrl Pts',(-6.501930055,1.069390921,-3.207398566));
#155743=CARTESIAN_POINT('Ctrl Pts',(-6.675733702,1.004503495,-2.855069682));
#155744=CARTESIAN_POINT('Ctrl Pts',(-6.81044718200001,0.939276009000001,
-2.486022764));
#155745=CARTESIAN_POINT('',(-6.80883911175379,0.940053947055498,-2.49042369268793));
#155746=CARTESIAN_POINT('Origin',(0.186541774058421,0.946431338254617,0.0693361714653745));
#155747=CARTESIAN_POINT('Ctrl Pts',(-7.043982621342,0.979367659152127,-2.57532693620972));
#155748=CARTESIAN_POINT('Ctrl Pts',(-7.00474108494745,0.973133929429406,
-2.5611963175052));
#155749=CARTESIAN_POINT('Ctrl Pts',(-6.96550429303653,0.966746137216144,
-2.5470493483575));
#155750=CARTESIAN_POINT('Ctrl Pts',(-6.88713590294071,0.95365266710452,
-2.51875402924264));
#155751=CARTESIAN_POINT('Ctrl Pts',(-6.84795851182924,0.946939345877625,
-2.50458914798822));
#155752=CARTESIAN_POINT('Ctrl Pts',(-6.808839110773,0.940053949626277,-2.49042369414692));
#155753=CARTESIAN_POINT('Ctrl Pts',(-6.953502166,0.939268254,-2.810481743));
#155754=CARTESIAN_POINT('Ctrl Pts',(-7.107803339,1.004934719,-2.428720309));
#155755=CARTESIAN_POINT('Ctrl Pts',(-7.21938412,1.069390921,-2.032361415));
#155756=CARTESIAN_POINT('Ctrl Pts',(-6.807201613,0.939268254,-2.49489603));
#155757=CARTESIAN_POINT('Ctrl Pts',(-6.94417648700001,1.004934719,-2.121166795));
#155758=CARTESIAN_POINT('Ctrl Pts',(-7.039414425,1.069390921,-1.734688604));
#155759=CARTESIAN_POINT('Origin',(0.170717629805586,0.803719092771659,0.0864857378840431));
#155760=CARTESIAN_POINT('Ctrl Pts',(-7.337087236,1.069390921,-1.554718909));
#155761=CARTESIAN_POINT('Ctrl Pts',(-7.421334894,1.004503495,-1.157134232));
#155762=CARTESIAN_POINT('Ctrl Pts',(-7.462126472,0.939276009000001,-0.752773886));
#155763=CARTESIAN_POINT('Ctrl Pts',(-7.039414425,1.069390921,-1.734688604));
#155764=CARTESIAN_POINT('Ctrl Pts',(-7.133414344,1.004503495,-1.353234327));
#155765=CARTESIAN_POINT('Ctrl Pts',(-7.185644119,0.939276009000001,-0.963856104));
#155766=CARTESIAN_POINT('',(-7.18501971399297,0.940053947079714,-0.9684998294504));
#155767=CARTESIAN_POINT('Origin',(0.197085704960005,0.946431359289948,0.027614151461707));
#155768=CARTESIAN_POINT('Ctrl Pts',(-7.4329173874246,0.979367659184994,
-1.0008691788516));
#155769=CARTESIAN_POINT('Ctrl Pts',(-7.3915556332617,0.973133929796456,
-0.995504696752814));
#155770=CARTESIAN_POINT('Ctrl Pts',(-7.35019499413787,0.966746137377657,
-0.990123226044648));
#155771=CARTESIAN_POINT('Ctrl Pts',(-7.26757615490654,0.953652667071922,
-0.979336322679543));
#155772=CARTESIAN_POINT('Ctrl Pts',(-7.2262696785515,0.94693934584413,-0.973924589329538));
#155773=CARTESIAN_POINT('Ctrl Pts',(-7.18501971341776,0.94005394961285,
-0.968499830609128));
#155774=CARTESIAN_POINT('Ctrl Pts',(-7.39510364700001,0.939268254,-1.24997682));
#155775=CARTESIAN_POINT('Ctrl Pts',(-7.463729921,1.004934719,-0.843970566000001));
#155776=CARTESIAN_POINT('Ctrl Pts',(-7.48749656,1.069390921,-0.432891753));
#155777=CARTESIAN_POINT('Ctrl Pts',(-7.18438192,0.939268254,-0.97321962));
#155778=CARTESIAN_POINT('Ctrl Pts',(-7.23781366,1.004934719,-0.578782418));
#155779=CARTESIAN_POINT('Ctrl Pts',(-7.2477436,1.069390921,-0.180866531));
#155780=CARTESIAN_POINT('Origin',(0.185317934167133,0.803719109795523,0.0477644810006672));
#155781=CARTESIAN_POINT('Ctrl Pts',(-7.499768822,1.069390921,0.058886428));
#155782=CARTESIAN_POINT('Ctrl Pts',(-7.496577864,1.004503495,0.465286552));
#155783=CARTESIAN_POINT('Ctrl Pts',(-7.449490235,0.939276009000001,0.868962162));
#155784=CARTESIAN_POINT('Ctrl Pts',(-7.24774360000001,1.069390921,-0.180866531));
#155785=CARTESIAN_POINT('Ctrl Pts',(-7.25754446,1.004503495,0.211876761));
#155786=CARTESIAN_POINT('Ctrl Pts',(-7.22484832400001,0.939276009000001,
0.603379396));
#155787=CARTESIAN_POINT('',(-7.22523678108189,0.940053948086643,0.598710009952622));
#155788=CARTESIAN_POINT('Origin',(0.198414091245139,0.946431379860457,-0.0153990371398191));
#155789=CARTESIAN_POINT('Ctrl Pts',(-7.47429719712509,0.979367659133194,
0.62038810919019));
#155790=CARTESIAN_POINT('Ctrl Pts',(-7.43274924742846,0.973133928964554,
0.616735617683767));
#155791=CARTESIAN_POINT('Ctrl Pts',(-7.39119874306821,0.966746137007537,
0.613099958047034));
#155792=CARTESIAN_POINT('Ctrl Pts',(-7.30819262379929,0.95365266714958,
0.605874061569174));
#155793=CARTESIAN_POINT('Ctrl Pts',(-7.2666885075572,0.946939345977453,
0.602279600214168));
#155794=CARTESIAN_POINT('Ctrl Pts',(-7.22523678098003,0.940053949744611,
0.598710007937336));
#155795=CARTESIAN_POINT('Ctrl Pts',(-7.4909183,0.939268254,0.36897563));
#155796=CARTESIAN_POINT('Ctrl Pts',(-7.470660787,1.004934719,0.780242304));
#155797=CARTESIAN_POINT('Ctrl Pts',(-7.405501982,1.069390921,1.186819448));
#155798=CARTESIAN_POINT('Ctrl Pts',(-7.22562851299999,0.939268254,0.593963458000001));
#155799=CARTESIAN_POINT('Ctrl Pts',(-7.193018709,1.004934719,0.990665182));
#155800=CARTESIAN_POINT('Ctrl Pts',(-7.11717634,1.069390921,1.381412661));
#155801=CARTESIAN_POINT('Origin',(0.191253352313244,0.803718922848623,0.00680992009186643));
#155802=CARTESIAN_POINT('Ctrl Pts',(-7.311769554,1.069390921,1.669738302));
#155803=CARTESIAN_POINT('Ctrl Pts',(-7.221289184,1.004503495,2.065951054));
#155804=CARTESIAN_POINT('Ctrl Pts',(-7.08852411500001,0.939276009000001,
2.450066505));
#155805=CARTESIAN_POINT('Ctrl Pts',(-7.11717634,1.069390921,1.381412661));
#155806=CARTESIAN_POINT('Ctrl Pts',(-7.04231986300001,1.004503495,1.767080728));
#155807=CARTESIAN_POINT('Ctrl Pts',(-6.926226651,0.939276009000001,2.142401545));
#155808=CARTESIAN_POINT('',(-6.92760980555269,0.94005394704967,2.13792483369844));
#155809=CARTESIAN_POINT('Origin',(0.190464918460538,0.946431351991406,-0.057692183818133));
#155810=CARTESIAN_POINT('Ctrl Pts',(-7.16618717754861,0.979367659162817,
2.21263673886222));
#155811=CARTESIAN_POINT('Ctrl Pts',(-7.12639577943535,0.973133929903967,
2.20013806146995));
#155812=CARTESIAN_POINT('Ctrl Pts',(-7.08659825869256,0.966746137413077,
2.18765527027077));
#155813=CARTESIAN_POINT('Ctrl Pts',(-7.00708612763533,0.953652667044357,
2.16275444828855));
#155814=CARTESIAN_POINT('Ctrl Pts',(-6.96732505701767,0.946939345769651,
2.15032186507112));
#155815=CARTESIAN_POINT('Ctrl Pts',(-6.92760980569742,0.940053949535198,
2.13792483185428));
#155816=CARTESIAN_POINT('Ctrl Pts',(-7.23646594,0.939268254,1.97067519));
#155817=CARTESIAN_POINT('Ctrl Pts',(-7.128271858,1.004934719,2.36797191));
#155818=CARTESIAN_POINT('Ctrl Pts',(-6.977234361,1.069390921,2.751036289));
#155819=CARTESIAN_POINT('Ctrl Pts',(-6.929012748,0.939268254,2.133373465));
#155820=CARTESIAN_POINT('Ctrl Pts',(-6.811886199,1.004934719,2.513790379));
#155821=CARTESIAN_POINT('Ctrl Pts',(-6.653817825,1.069390921,2.879098531));
#155822=CARTESIAN_POINT('Origin',(0.188246019438175,0.803719090896389,-0.034463192469657));
#155823=CARTESIAN_POINT('Ctrl Pts',(-6.781880067,1.069390921,3.202515068));
#155824=CARTESIAN_POINT('Ctrl Pts',(-6.60834104800001,1.004503495,3.570013982));
#155825=CARTESIAN_POINT('Ctrl Pts',(-6.396106485,0.939276009000001,3.916608461));
#155826=CARTESIAN_POINT('Ctrl Pts',(-6.653817825,1.069390921,2.879098531));
#155827=CARTESIAN_POINT('Ctrl Pts',(-6.497804216,1.004503495,3.239657963));
#155828=CARTESIAN_POINT('Ctrl Pts',(-6.303742317,0.939276009000001,3.58124738));
#155829=CARTESIAN_POINT('',(-6.30605549550746,0.94005394707995,3.57717266853147));
#155830=CARTESIAN_POINT('Origin',(0.173609964766765,0.94643137782079,-0.0972877614143342));
#155831=CARTESIAN_POINT('Ctrl Pts',(-6.52299420951791,0.979367659152604,
3.70142493378223));
#155832=CARTESIAN_POINT('Ctrl Pts',(-6.48681995481761,0.973133929282097,
3.68066449204472));
#155833=CARTESIAN_POINT('Ctrl Pts',(-6.45063631116856,0.966746137137303,
3.65991825214105));
#155834=CARTESIAN_POINT('Ctrl Pts',(-6.37833607187544,0.953652667104105,
3.61850684058575));
#155835=CARTESIAN_POINT('Ctrl Pts',(-6.34217723114372,0.946939345906579,
3.59781746951572));
#155836=CARTESIAN_POINT('Ctrl Pts',(-6.30605549594103,0.940053949701714,
3.57717266689846));
#155837=CARTESIAN_POINT('Ctrl Pts',(-6.643644474,0.939268254,3.480228168));
#155838=CARTESIAN_POINT('Ctrl Pts',(-6.452572859,1.004934719,3.844977782));
#155839=CARTESIAN_POINT('Ctrl Pts',(-6.222719017,1.069390921,4.186617732));
#155840=CARTESIAN_POINT('Ctrl Pts',(-6.308404047,0.939268254,3.573029299));
#155841=CARTESIAN_POINT('Ctrl Pts',(-6.112237461,1.004934719,3.919373532));
#155842=CARTESIAN_POINT('Ctrl Pts',(-5.879334183,1.069390921,4.242160954));
#155843=CARTESIAN_POINT('Origin',(0.176436100079234,0.803719120296965,-0.0741246307396093));
#155844=CARTESIAN_POINT('Ctrl Pts',(-5.934877406,1.069390921,4.585545789));
#155845=CARTESIAN_POINT('Ctrl Pts',(-5.68639423,1.004503495,4.907147023));
#155846=CARTESIAN_POINT('Ctrl Pts',(-5.404614025,0.939276009000001,5.200014158));
#155847=CARTESIAN_POINT('Ctrl Pts',(-5.879334183,1.069390921,4.242160954));
#155848=CARTESIAN_POINT('Ctrl Pts',(-5.649458466,1.004503495,4.560752393));
#155849=CARTESIAN_POINT('Ctrl Pts',(-5.386501999,0.939276009000001,4.852638067));
#155850=CARTESIAN_POINT('',(-5.3896370399433,0.940053947055203,4.8491558857356));
#155851=CARTESIAN_POINT('Origin',(0.148636968835451,0.946431371091245,-0.132334142889854));
#155852=CARTESIAN_POINT('Ctrl Pts',(-5.5747932828214,0.979367659164909,
5.01713861212506));
#155853=CARTESIAN_POINT('Ctrl Pts',(-5.54392760548416,0.973133921651111,
4.98908710816583));
#155854=CARTESIAN_POINT('Ctrl Pts',(-5.51304976423055,0.966746133499498,
4.96104750887767));
#155855=CARTESIAN_POINT('Ctrl Pts',(-5.45134211096734,0.953652667146328,
4.90506187481743));
#155856=CARTESIAN_POINT('Ctrl Pts',(-5.42047624750108,0.946939346057015,
4.87708312846141));
#155857=CARTESIAN_POINT('Ctrl Pts',(-5.38963704040107,0.94005394978954,
4.84915588455596));
#155858=CARTESIAN_POINT('Ctrl Pts',(-5.74017357700001,0.939268254,4.827049544));
#155859=CARTESIAN_POINT('Ctrl Pts',(-5.475158725,1.004934719,5.142196766));
#155860=CARTESIAN_POINT('Ctrl Pts',(-5.177236248,1.069390921,5.426437582));
#155861=CARTESIAN_POINT('Ctrl Pts',(-5.392821385,0.939268254,4.845614255));
#155862=CARTESIAN_POINT('Ctrl Pts',(-5.126787292,1.004934719,5.141691134));
#155863=CARTESIAN_POINT('Ctrl Pts',(-4.829939409,1.069390921,5.406864646));
#155864=CARTESIAN_POINT('Origin',(0.156376705074808,0.803719083698706,-0.110320379162943));
#155865=CARTESIAN_POINT('Ctrl Pts',(-4.810366473,1.069390921,5.754161485));
#155866=CARTESIAN_POINT('Ctrl Pts',(-4.498557937,1.004503495,6.014827323));
#155867=CARTESIAN_POINT('Ctrl Pts',(-4.16040782,0.939276009000001,6.240272973));
#155868=CARTESIAN_POINT('Ctrl Pts',(-4.829939409,1.069390921,5.406864646));
#155869=CARTESIAN_POINT('Ctrl Pts',(-4.536950317,1.004503495,5.66859111));
#155870=CARTESIAN_POINT('Ctrl Pts',(-4.217394834,0.939276009000001,5.89712479200001));
#155871=CARTESIAN_POINT('',(-4.22120514517481,0.940053948808827,5.89439796322484));
#155872=CARTESIAN_POINT('Origin',(0.116713988276355,0.946431391368445,-0.161192793784344));
#155873=CARTESIAN_POINT('Ctrl Pts',(-4.36592121772472,0.979367659169013,
6.09825646575288));
#155874=CARTESIAN_POINT('Ctrl Pts',(-4.34180743928535,0.973133930010902,
6.06422562774249));
#155875=CARTESIAN_POINT('Ctrl Pts',(-4.31767917226086,0.966746137510712,
6.03020373075736));
#155876=CARTESIAN_POINT('Ctrl Pts',(-4.26944945116904,0.953652667121064,
5.96226166741486));
#155877=CARTESIAN_POINT('Ctrl Pts',(-4.24531981791811,0.946939346056006,
5.92830180049019));
#155878=CARTESIAN_POINT('Ctrl Pts',(-4.22120514626669,0.940053949810634,
5.89439796224477));
#155879=CARTESIAN_POINT('Ctrl Pts',(-4.568298544,0.939268254,5.948163449));
#155880=CARTESIAN_POINT('Ctrl Pts',(-4.241732254,1.004934719,6.198972345));
#155881=CARTESIAN_POINT('Ctrl Pts',(-3.889671666,1.069390921,6.412523242));
#155882=CARTESIAN_POINT('Ctrl Pts',(-4.225076389,0.939268254,5.891623674));
#155883=CARTESIAN_POINT('Ctrl Pts',(-3.901614248,1.004934719,6.123588974));
#155884=CARTESIAN_POINT('Ctrl Pts',(-3.554702037,1.069390921,6.318749356));
#155885=CARTESIAN_POINT('Origin',(0.129005056016377,0.803719098892777,-0.141357475233095));
#155886=CARTESIAN_POINT('Ctrl Pts',(-3.460928151,1.069390921,6.653718985));
#155887=CARTESIAN_POINT('Ctrl Pts',(-3.100374075,1.004503495,6.841260983));
#155888=CARTESIAN_POINT('Ctrl Pts',(-2.721665569,0.939276009000001,6.988743559));
#155889=CARTESIAN_POINT('Ctrl Pts',(-3.554702037,1.069390921,6.318749356));
#155890=CARTESIAN_POINT('Ctrl Pts',(-3.212299413,1.004503495,6.511372807));
#155891=CARTESIAN_POINT('Ctrl Pts',(-2.851086974,0.939276009000001,6.665868515));
#155892=CARTESIAN_POINT('',(-2.85539438941291,0.940053948098198,6.66402454208368));
#155893=CARTESIAN_POINT('Origin',(0.0793335642571924,0.94643133914452,-0.1825142284368));
#155894=CARTESIAN_POINT('Ctrl Pts',(-2.9529035287323,0.979367659117687,
6.89422662433445));
#155895=CARTESIAN_POINT('Ctrl Pts',(-2.93666913907019,0.97313392913207,
6.85580765366883));
#155896=CARTESIAN_POINT('Ctrl Pts',(-2.92041868086989,0.966746137072281,
6.81739430829125));
#155897=CARTESIAN_POINT('Ctrl Pts',(-2.8879220802227,0.953652667109427,
6.74067273051987));
#155898=CARTESIAN_POINT('Ctrl Pts',(-2.87165695187532,0.946939345996193,
6.70231966810689));
#155899=CARTESIAN_POINT('Ctrl Pts',(-2.85539439105084,0.940053949768782,
6.66402454108775));
#155900=CARTESIAN_POINT('Ctrl Pts',(-3.182814947,0.939268254,6.79114784200001));
#155901=CARTESIAN_POINT('Ctrl Pts',(-2.809967097,1.004934719,6.965890866));
#155902=CARTESIAN_POINT('Ctrl Pts',(-2.420230359,1.069390921,7.098766443));
#155903=CARTESIAN_POINT('Ctrl Pts',(-2.859771516,0.939268254,6.662147317));
#155904=CARTESIAN_POINT('Ctrl Pts',(-2.494006057,1.004934719,6.819154599));
#155905=CARTESIAN_POINT('Ctrl Pts',(-2.113250748,1.069390921,6.93517637));
#155906=CARTESIAN_POINT('Origin',(0.095601296301798,0.803718949325442,-0.165784735215747));
#155907=CARTESIAN_POINT('Ctrl Pts',(-1.949660675,1.069390921,7.24215598100001));
#155908=CARTESIAN_POINT('Ctrl Pts',(-1.557220167,1.004503495,7.347804883));
#155909=CARTESIAN_POINT('Ctrl Pts',(-1.155661261,0.939276009000001,7.410428264));
#155910=CARTESIAN_POINT('Ctrl Pts',(-2.113250748,1.069390921,6.93517637));
#155911=CARTESIAN_POINT('Ctrl Pts',(-1.73744496,1.004503495,7.049689948));
#155912=CARTESIAN_POINT('Ctrl Pts',(-1.351465456,0.939276009000001,7.122923636));
#155913=CARTESIAN_POINT('',(-1.35606856648097,0.940053947035547,7.1220487401457));
#155914=CARTESIAN_POINT('Origin',(0.0382436804210429,0.946431393530997,
-0.195301735553574));
#155915=CARTESIAN_POINT('Ctrl Pts',(-1.40181135298697,0.979367659138296,
7.36783040874983));
#155916=CARTESIAN_POINT('Ctrl Pts',(-1.3942154481657,0.973133921591531,
7.32681968872295));
#155917=CARTESIAN_POINT('Ctrl Pts',(-1.38660265533696,0.966746133408986,
7.28581108465508));
#155918=CARTESIAN_POINT('Ctrl Pts',(-1.37135868269623,0.953652667065727,
7.20389742909375));
#155919=CARTESIAN_POINT('Ctrl Pts',(-1.36371859852421,0.946939345797094,
7.162944517369));
#155920=CARTESIAN_POINT('Ctrl Pts',(-1.35606856762555,0.940053949578423,
7.12204873950346));
#155921=CARTESIAN_POINT('Ctrl Pts',(-1.648506461,0.939268254,7.31658571));
#155922=CARTESIAN_POINT('Ctrl Pts',(-1.246811002,1.004934719,7.407092072));
#155923=CARTESIAN_POINT('Ctrl Pts',(-0.837621771,1.069390921,7.453079214));
#155924=CARTESIAN_POINT('Ctrl Pts',(-1.360746905,0.939268254,7.121156357));
#155925=CARTESIAN_POINT('Ctrl Pts',(-0.969780916,1.004934719,7.195864134));
#155926=CARTESIAN_POINT('Ctrl Pts',(-0.572986203,1.069390921,7.227322244));
#155927=CARTESIAN_POINT('Origin',(0.0577273861487002,0.803719070356922,
-0.182460475737256));
#155928=CARTESIAN_POINT('Ctrl Pts',(-0.347229232,1.069390921,7.491957812));
#155929=CARTESIAN_POINT('Ctrl Pts',(0.058747626,1.004503495,7.510773593));
#155930=CARTESIAN_POINT('Ctrl Pts',(0.464380483,0.939276009000001,7.485609579));
#155931=CARTESIAN_POINT('Ctrl Pts',(-0.572986203,1.069390921,7.227322244));
#155932=CARTESIAN_POINT('Ctrl Pts',(-0.181349511,1.004503495,7.258371422));
#155933=CARTESIAN_POINT('Ctrl Pts',(0.211349085,0.939276009000001,7.24691876300001));
#155934=CARTESIAN_POINT('Origin',(-0.00463470785240436,0.946431364356144,
-0.198957029881124));
#155935=CARTESIAN_POINT('Ctrl Pts',(-1.35877392498063,4.81811592995236,
7.12153743297961));
#155936=CARTESIAN_POINT('Ctrl Pts',(-1.35490612249032,4.81875342547618,
7.1222710489898));
#155937=CARTESIAN_POINT('Ctrl Pts',(-1.35103832,4.819390921,7.123004665));
#155938=CARTESIAN_POINT('Ctrl Pts',(-1.344855702,4.820409947,7.12417733800001));
#155939=CARTESIAN_POINT('Ctrl Pts',(-1.338671059,4.821428571,7.125339276));
#155940=CARTESIAN_POINT('Ctrl Pts',(-0.955718432,4.884501699,7.19728639));
#155941=CARTESIAN_POINT('Ctrl Pts',(-0.567260438,4.948754474,7.227773903));
#155942=CARTESIAN_POINT('Ctrl Pts',(-1.21606691400034,4.81811592995236,
7.33154082511742));
#155943=CARTESIAN_POINT('Ctrl Pts',(-1.21208516350017,4.81875342547618,
7.33219682755871));
#155944=CARTESIAN_POINT('Ctrl Pts',(-1.208103413,4.819390921,7.33285283));
#155945=CARTESIAN_POINT('Ctrl Pts',(-1.201738651,4.820409947,7.333901439));
#155946=CARTESIAN_POINT('Ctrl Pts',(-1.195372079,4.821428571,7.334938996));
#155947=CARTESIAN_POINT('Ctrl Pts',(-0.801154479,4.884501699,7.399184481));
#155948=CARTESIAN_POINT('Ctrl Pts',(-0.402321868,4.948754474,7.420807342));
#155949=CARTESIAN_POINT('',(-0.57198312172941,4.94797310013266,7.22740172850988));
#155950=CARTESIAN_POINT('Origin',(-0.00829022335223695,5.08885443639218,
-0.190840199381178));
#155951=CARTESIAN_POINT('Ctrl Pts',(-0.571982217557311,4.94797287193578,
7.22740176977812));
#155952=CARTESIAN_POINT('Ctrl Pts',(-0.573456838245926,4.94458997048659,
7.24802737088461));
#155953=CARTESIAN_POINT('Ctrl Pts',(-0.574945447045747,4.94124830640299,
7.26865888388256));
#155954=CARTESIAN_POINT('Ctrl Pts',(-0.576449088949175,4.93794661992768,
7.28929564968059));
#155955=CARTESIAN_POINT('Ctrl Pts',(-2.16235458594344,4.95685569181143,
6.91814254814242));
#155956=CARTESIAN_POINT('Ctrl Pts',(-1.76154032246365,4.88876675985096,
7.04342220983006));
#155957=CARTESIAN_POINT('Ctrl Pts',(-1.34893983835,4.819390921,7.12157531593001));
#155958=CARTESIAN_POINT('Ctrl Pts',(-1.3218087413993,4.8148290198817,7.12671437800155));
#155959=CARTESIAN_POINT('Ctrl Pts',(-1.2946776444487,4.81026711876327,7.13185344007204));
#155960=CARTESIAN_POINT('Ctrl Pts',(-2.16460409637423,4.95685569181143,
6.91931998895273));
#155961=CARTESIAN_POINT('Ctrl Pts',(-1.76372161586533,4.88876675985096,
7.04472997983171));
#155962=CARTESIAN_POINT('Ctrl Pts',(-1.35103832,4.819390921,7.123004665));
#155963=CARTESIAN_POINT('Ctrl Pts',(-1.32390177765177,4.8148290198817,7.12815172166587));
#155964=CARTESIAN_POINT('Ctrl Pts',(-1.29676523530354,4.81026711876327,
7.13329877833112));
#155965=CARTESIAN_POINT('Ctrl Pts',(-2.38955513945283,4.95685569181143,
7.03706406998286));
#155966=CARTESIAN_POINT('Ctrl Pts',(-1.98185095603346,4.88876675985096,
7.17550697999575));
#155967=CARTESIAN_POINT('Ctrl Pts',(-1.560886485,4.819390921,7.265939572));
#155968=CARTESIAN_POINT('Ctrl Pts',(-1.53320540289719,4.8148290198817,7.27188608809886));
#155969=CARTESIAN_POINT('Ctrl Pts',(-1.50552432079462,4.81026711876327,
7.27783260419724));
#155970=CARTESIAN_POINT('',(-2.11228819893379,4.94797311771878,6.93546962696871));
#155971=CARTESIAN_POINT('Origin',(0.0156522182859661,4.69654718398349,-0.1918471612771));
#155972=CARTESIAN_POINT('Ctrl Pts',(-2.12995512149651,4.93794661942987,
6.9949564549365));
#155973=CARTESIAN_POINT('Ctrl Pts',(-2.12405034199266,4.94124830642815,
6.97512540270629));
#155974=CARTESIAN_POINT('Ctrl Pts',(-2.11816137081836,4.94458997052876,
6.95529624952042));
#155975=CARTESIAN_POINT('Ctrl Pts',(-2.1122872006493,4.94797287203487,6.93546979394767));
#155976=CARTESIAN_POINT('Ctrl Pts',(-2.85886884210992,4.81811592995234,
6.66058590328662));
#155977=CARTESIAN_POINT('Ctrl Pts',(-2.85525045263496,4.81875342547617,
6.6621343435833));
#155978=CARTESIAN_POINT('Ctrl Pts',(-2.85163206316,4.81939092100001,6.66368278388));
#155979=CARTESIAN_POINT('Ctrl Pts',(-2.84584812772,4.820409947,6.66615793995999));
#155980=CARTESIAN_POINT('Ctrl Pts',(-2.84005990385,4.821428571,6.66862305261));
#155981=CARTESIAN_POINT('Ctrl Pts',(-2.48165357213,4.884501699,6.82126257693001));
#155982=CARTESIAN_POINT('Ctrl Pts',(-2.10895180115,4.948754474,6.93460856659));
#155983=CARTESIAN_POINT('Ctrl Pts',(-2.85792658132591,4.81811592995234,
6.66294361747922));
#155984=CARTESIAN_POINT('Ctrl Pts',(-2.85430691216296,4.81875342547617,
6.66449154473961));
#155985=CARTESIAN_POINT('Ctrl Pts',(-2.850687243,4.81939092100001,6.666039472));
#155986=CARTESIAN_POINT('Ctrl Pts',(-2.844901262,4.820409947,6.668513808));
#155987=CARTESIAN_POINT('Ctrl Pts',(-2.839110994,4.821428571,6.670978097));
#155988=CARTESIAN_POINT('Ctrl Pts',(-2.48057809,4.884501699,6.823566622));
#155989=CARTESIAN_POINT('Ctrl Pts',(-2.107755942,4.948754474,6.93684834));
#155990=CARTESIAN_POINT('Ctrl Pts',(-2.76370050292588,4.81811592995234,
6.89871503673933));
#155991=CARTESIAN_POINT('Ctrl Pts',(-2.75995286496294,4.81875342547617,
6.90021166036967));
#155992=CARTESIAN_POINT('Ctrl Pts',(-2.756205227,4.81939092100001,6.901708284));
#155993=CARTESIAN_POINT('Ctrl Pts',(-2.75021469,4.820409947,6.904100612));
#155994=CARTESIAN_POINT('Ctrl Pts',(-2.744220009,4.821428571,6.906482536));
#155995=CARTESIAN_POINT('Ctrl Pts',(-2.373029877,4.884501699,7.053971129));
#155996=CARTESIAN_POINT('Ctrl Pts',(-1.988170027,4.948754474,7.160825681));
#155997=CARTESIAN_POINT('Origin',(0.0329293447624329,5.08885503540763,-0.188162932465979));
#155998=CARTESIAN_POINT('Ctrl Pts',(-3.59899609457623,4.95685569337321,
6.29155789759412));
#155999=CARTESIAN_POINT('Ctrl Pts',(-3.23448406651575,4.88876676064928,
6.50007181265036));
#156000=CARTESIAN_POINT('Ctrl Pts',(-2.84833055488,4.819390921,6.66509465184));
#156001=CARTESIAN_POINT('Ctrl Pts',(-2.82293850999083,4.81482901910993,
6.67594595116572));
#156002=CARTESIAN_POINT('Ctrl Pts',(-2.79754646510191,4.81026711721972,
6.6867972504915));
#156003=CARTESIAN_POINT('Ctrl Pts',(-3.60144612767277,4.95685569337321,
6.29222423224807));
#156004=CARTESIAN_POINT('Ctrl Pts',(-3.23689549438232,4.88876676064928,
6.50088009410198));
#156005=CARTESIAN_POINT('Ctrl Pts',(-2.850687243,4.819390921,6.666039472));
#156006=CARTESIAN_POINT('Ctrl Pts',(-2.82529159862497,4.81482901910993,
6.67689974961262));
#156007=CARTESIAN_POINT('Ctrl Pts',(-2.79989595425014,4.81026711721972,
6.68776002722526));
#156008=CARTESIAN_POINT('Ctrl Pts',(-3.84644943732711,4.95685569337321,
6.35885769764247));
#156009=CARTESIAN_POINT('Ctrl Pts',(-3.47803828103868,4.88876676064928,
6.58170823926466));
#156010=CARTESIAN_POINT('Ctrl Pts',(-3.086356055,4.819390921,6.76052148800001));
#156011=CARTESIAN_POINT('Ctrl Pts',(-3.06060046203974,4.81482901910993,
6.77227959430188));
#156012=CARTESIAN_POINT('Ctrl Pts',(-3.03484486907951,4.81026711721972,
6.78403770060382));
#156013=CARTESIAN_POINT('',(-3.55382503325055,4.9479731176806,6.31924267752363));
#156014=CARTESIAN_POINT('Origin',(0.0565277989466323,4.69654717972231,-0.18399723361456));
#156015=CARTESIAN_POINT('Ctrl Pts',(-3.58386682219125,4.93794661934438,
6.37354087035044));
#156016=CARTESIAN_POINT('Ctrl Pts',(-3.57383700388081,4.94124830645077,
6.35544280984233));
#156017=CARTESIAN_POINT('Ctrl Pts',(-3.56382303182418,4.9445899705472,6.3373432059445));
#156018=CARTESIAN_POINT('Ctrl Pts',(-3.55382409446741,4.9479728720179,6.31924305487698));
#156019=CARTESIAN_POINT('Ctrl Pts',(-4.22385916096707,4.81811592995213,
5.89029281182821));
#156020=CARTESIAN_POINT('Ctrl Pts',(-4.22065823623853,4.81875342547606,
5.89258289768411));
#156021=CARTESIAN_POINT('Ctrl Pts',(-4.21745731151,4.819390921,5.89487298353999));
#156022=CARTESIAN_POINT('Ctrl Pts',(-4.21234068653,4.820409947,5.89853364772001));
#156023=CARTESIAN_POINT('Ctrl Pts',(-4.20721771493,4.821428571,5.90218542367));
#156024=CARTESIAN_POINT('Ctrl Pts',(-3.89000370937,4.884501699,6.12830308735));
#156025=CARTESIAN_POINT('Ctrl Pts',(-3.55038153655001,4.948754474,6.31911897488));
#156026=CARTESIAN_POINT('Ctrl Pts',(-4.22344576856042,4.81811592995213,
5.89279796219157));
#156027=CARTESIAN_POINT('Ctrl Pts',(-4.22024348378021,4.81875342547606,
5.89508782209578));
#156028=CARTESIAN_POINT('Ctrl Pts',(-4.217041199,4.819390921,5.897377682));
#156029=CARTESIAN_POINT('Ctrl Pts',(-4.2119224,4.820409947,5.90103798500001));
#156030=CARTESIAN_POINT('Ctrl Pts',(-4.206797255,4.821428571,5.904689396));
#156031=CARTESIAN_POINT('Ctrl Pts',(-3.889448673,4.884501699,6.130784462));
#156032=CARTESIAN_POINT('Ctrl Pts',(-3.549695121,4.948754474,6.321563458));
#156033=CARTESIAN_POINT('Ctrl Pts',(-4.18210652789557,4.81811592995213,
6.14331299852691));
#156034=CARTESIAN_POINT('Ctrl Pts',(-4.17876823794779,4.81875342547606,
6.14558026326346));
#156035=CARTESIAN_POINT('Ctrl Pts',(-4.175429948,4.819390921,6.147847528));
#156036=CARTESIAN_POINT('Ctrl Pts',(-4.170093747,4.820409947,6.151471713));
#156037=CARTESIAN_POINT('Ctrl Pts',(-4.164751262,4.821428571,6.155086629));
#156038=CARTESIAN_POINT('Ctrl Pts',(-3.833945036,4.884501699,6.378921927));
#156039=CARTESIAN_POINT('Ctrl Pts',(-3.481053566,4.948754474,6.56601177));
#156040=CARTESIAN_POINT('Origin',(0.0726090705661236,5.08885504255354,-0.176685151946212));
#156041=CARTESIAN_POINT('Ctrl Pts',(-4.86735251457583,4.95685568844401,
5.37078701507674));
#156042=CARTESIAN_POINT('Ctrl Pts',(-4.55618691247175,4.88876675812967,
5.65278529087343));
#156043=CARTESIAN_POINT('Ctrl Pts',(-4.21453650053,4.819390921,5.89696156949));
#156044=CARTESIAN_POINT('Ctrl Pts',(-4.19207081821782,4.81482901952818,
5.91301770907552));
#156045=CARTESIAN_POINT('Ctrl Pts',(-4.1696051359056,4.81026711805618,5.92907384866106));
#156046=CARTESIAN_POINT('Ctrl Pts',(-4.86988850951164,4.95685568844401,
5.3709110865213));
#156047=CARTESIAN_POINT('Ctrl Pts',(-4.55871571911483,4.88876675812967,
5.6530562894507));
#156048=CARTESIAN_POINT('Ctrl Pts',(-4.217041199,4.819390921,5.897377682));
#156049=CARTESIAN_POINT('Ctrl Pts',(-4.19457393142246,4.81482901952818,
5.91344336374728));
#156050=CARTESIAN_POINT('Ctrl Pts',(-4.17210666384516,4.81026711805618,
5.92950904549473));
#156051=CARTESIAN_POINT('Ctrl Pts',(-5.12348800309282,4.95685568844401,
5.38331823097723));
#156052=CARTESIAN_POINT('Ctrl Pts',(-4.81159638342372,4.88876675812967,
5.68015614717736));
#156053=CARTESIAN_POINT('Ctrl Pts',(-4.467511046,4.819390921,5.938988933));
#156054=CARTESIAN_POINT('Ctrl Pts',(-4.44488525188809,4.81482901952818,
5.95600883092791));
#156055=CARTESIAN_POINT('Ctrl Pts',(-4.42225945777601,4.81026711805618,
5.9730287288553));
#156056=CARTESIAN_POINT('',(-4.82918895415257,4.94797309993411,5.40753499076431));
#156057=CARTESIAN_POINT('Origin',(0.094760193322927,4.69654721337739,-0.167543692837909));
#156058=CARTESIAN_POINT('Ctrl Pts',(-4.87020089538197,4.9379466194895,5.45410559722007));
#156059=CARTESIAN_POINT('Ctrl Pts',(-4.8565150415706,4.94124830103405,5.43858679968498));
#156060=CARTESIAN_POINT('Ctrl Pts',(-4.84284433309257,4.94458995962699,
5.42306308763061));
#156061=CARTESIAN_POINT('Ctrl Pts',(-4.82918818983745,4.94797285533979,
5.40753560967742));
#156062=CARTESIAN_POINT('Ctrl Pts',(-5.39134652093208,4.81811592995213,
4.84457617665));
#156063=CARTESIAN_POINT('Ctrl Pts',(-5.38871273241604,4.81875342547607,
4.847500825375));
#156064=CARTESIAN_POINT('Ctrl Pts',(-5.3860789439,4.819390921,4.85042547409999));
#156065=CARTESIAN_POINT('Ctrl Pts',(-5.38186887673,4.820409947,4.85510047648001));
#156066=CARTESIAN_POINT('Ctrl Pts',(-5.37765070077,4.821428571,4.85976816369));
#156067=CARTESIAN_POINT('Ctrl Pts',(-5.11646159673,4.884501699,5.14879095710001));
#156068=CARTESIAN_POINT('Ctrl Pts',(-4.82579937693,4.948754474,5.40815440248));
#156069=CARTESIAN_POINT('Ctrl Pts',(-5.39148132667972,4.81811592995213,
4.84711162513907));
#156070=CARTESIAN_POINT('Ctrl Pts',(-5.38884616133986,4.81875342547607,
4.85003634556953));
#156071=CARTESIAN_POINT('Ctrl Pts',(-5.386210996,4.819390921,4.852961066));
#156072=CARTESIAN_POINT('Ctrl Pts',(-5.381998728,4.820409947,4.857636183));
#156073=CARTESIAN_POINT('Ctrl Pts',(-5.377778351,4.821428571,4.862303981));
#156074=CARTESIAN_POINT('Ctrl Pts',(-5.116452959,4.884501699,5.151333635));
#156075=CARTESIAN_POINT('Ctrl Pts',(-4.825654501,4.948754474,5.410689294));
#156076=CARTESIAN_POINT('Ctrl Pts',(-5.4049619014445,4.81811592995213,5.10065647404533));
#156077=CARTESIAN_POINT('Ctrl Pts',(-5.40218905372225,4.81875342547607,
5.10358836502267));
#156078=CARTESIAN_POINT('Ctrl Pts',(-5.399416206,4.819390921,5.10652025600001));
#156079=CARTESIAN_POINT('Ctrl Pts',(-5.394983855,4.820409947,5.111206835));
#156080=CARTESIAN_POINT('Ctrl Pts',(-5.390543374,4.821428571,5.115885712));
#156081=CARTESIAN_POINT('Ctrl Pts',(-5.115589186,4.884501699,5.405601425));
#156082=CARTESIAN_POINT('Ctrl Pts',(-4.811166908,4.948754474,5.664178446));
#156083=CARTESIAN_POINT('Origin',(0.108891420928572,5.08885434269428,-0.156943200427216));
#156084=CARTESIAN_POINT('Ctrl Pts',(-5.90811696378675,4.95685568770243,
4.19888409086371));
#156085=CARTESIAN_POINT('Ctrl Pts',(-5.66484753557328,4.88876675775061,
4.54118080731132));
#156086=CARTESIAN_POINT('Ctrl Pts',(-5.38367540411,4.819390921,4.85309311810001));
#156087=CARTESIAN_POINT('Ctrl Pts',(-5.36518655435748,4.81482902001977,
4.87360332947881));
#156088=CARTESIAN_POINT('Ctrl Pts',(-5.34669770460441,4.81026711903938,
4.89411354085806));
#156089=CARTESIAN_POINT('Ctrl Pts',(-5.91062034026415,4.95685568770243,
4.19846009763442));
#156090=CARTESIAN_POINT('Ctrl Pts',(-5.66737547681082,4.88876675775061,
4.54090185142077));
#156091=CARTESIAN_POINT('Ctrl Pts',(-5.386210996,4.819390921,4.852961066));
#156092=CARTESIAN_POINT('Ctrl Pts',(-5.36772264932633,4.81482902001977,
4.87348093723415));
#156093=CARTESIAN_POINT('Ctrl Pts',(-5.34923430265263,4.81026711903938,
4.89400080846849));
#156094=CARTESIAN_POINT('Ctrl Pts',(-6.16095798800407,4.95685568770243,
4.15606077470563));
#156095=CARTESIAN_POINT('Ctrl Pts',(-5.92016960056519,4.88876675775061,
4.51300626236517));
#156096=CARTESIAN_POINT('Ctrl Pts',(-5.63977018500001,4.819390921,4.839755856));
#156097=CARTESIAN_POINT('Ctrl Pts',(-5.6213321462153,4.81482902001977,4.86124171276682));
#156098=CARTESIAN_POINT('Ctrl Pts',(-5.6028941074302,4.81026711903938,4.8827275695335));
#156099=CARTESIAN_POINT('',(-5.87874536368429,4.94797309819258,4.24297694153243));
#156100=CARTESIAN_POINT('Origin',(0.128561535844363,4.69654720238666,-0.143255839490103));
#156101=CARTESIAN_POINT('Ctrl Pts',(-5.92880978556242,4.93794661941978,
4.27964240952211));
#156102=CARTESIAN_POINT('Ctrl Pts',(-5.91210778970961,4.94124830639064,
4.267428466771));
#156103=CARTESIAN_POINT('Ctrl Pts',(-5.89541952835817,4.94458997046672,
4.25520646896433));
#156104=CARTESIAN_POINT('Ctrl Pts',(-5.878744682587,4.94797287194661,4.24297766149803));
#156105=CARTESIAN_POINT('Ctrl Pts',(-6.306740508148,4.81811592995213,3.57233254198123));
#156106=CARTESIAN_POINT('Ctrl Pts',(-6.30479700952399,4.81875342547606,
3.57575500105562));
#156107=CARTESIAN_POINT('Ctrl Pts',(-6.3028535109,4.819390921,3.57917746013));
#156108=CARTESIAN_POINT('Ctrl Pts',(-6.29974686065001,4.820409947,3.58464820408));
#156109=CARTESIAN_POINT('Ctrl Pts',(-6.2966307174,4.821428571,3.59011354672));
#156110=CARTESIAN_POINT('Ctrl Pts',(-6.10367942619001,4.884501699,3.92852708364));
#156111=CARTESIAN_POINT('Ctrl Pts',(-5.87556820104999,4.948754474,4.2443105418));
#156112=CARTESIAN_POINT('Ctrl Pts',(-6.30741720870541,4.81811592995213,
3.57477973384487));
#156113=CARTESIAN_POINT('Ctrl Pts',(-6.30547238085271,4.81875342547606,
3.57820255892243));
#156114=CARTESIAN_POINT('Ctrl Pts',(-6.303527553,4.819390921,3.581625384));
#156115=CARTESIAN_POINT('Ctrl Pts',(-6.300418778,4.820409947,3.587096713));
#156116=CARTESIAN_POINT('Ctrl Pts',(-6.297300509,4.821428571,3.592562637));
#156117=CARTESIAN_POINT('Ctrl Pts',(-6.104217591,4.884501699,3.931012172));
#156118=CARTESIAN_POINT('Ctrl Pts',(-5.875971639,4.948754474,4.246817313));
#156119=CARTESIAN_POINT('Ctrl Pts',(-6.37508726444723,4.81811592995213,
3.81949892020891));
#156120=CARTESIAN_POINT('Ctrl Pts',(-6.37300951372361,4.81875342547606,
3.82295834560446));
#156121=CARTESIAN_POINT('Ctrl Pts',(-6.370931763,4.819390921,3.826417771));
#156122=CARTESIAN_POINT('Ctrl Pts',(-6.367610513,4.820409947,3.831947605));
#156123=CARTESIAN_POINT('Ctrl Pts',(-6.364279669,4.821428571,3.837471665));
#156124=CARTESIAN_POINT('Ctrl Pts',(-6.158034072,4.884501699,4.179521008));
#156125=CARTESIAN_POINT('Ctrl Pts',(-5.916315434,4.948754474,4.497494433));
#156126=CARTESIAN_POINT('Origin',(0.140086370307819,5.0888550933578,-0.129867356607448));
#156127=CARTESIAN_POINT('Ctrl Pts',(-6.67262443499624,4.95685568835189,
2.83064600545431));
#156128=CARTESIAN_POINT('Ctrl Pts',(-6.50862618644082,4.88876675808259,
3.21723575405344));
#156129=CARTESIAN_POINT('Ctrl Pts',(-6.30107962914,4.819390921,3.5822994261));
#156130=CARTESIAN_POINT('Ctrl Pts',(-6.28743212615761,4.81482901953652,
3.60630467879053));
#156131=CARTESIAN_POINT('Ctrl Pts',(-6.27378462317401,4.81026711807287,
3.6303099314808));
#156132=CARTESIAN_POINT('Ctrl Pts',(-6.67497813791429,4.95685568835189,
2.82969377301616));
#156133=CARTESIAN_POINT('Ctrl Pts',(-6.51103505853922,4.88876675808259,
3.21641988734669));
#156134=CARTESIAN_POINT('Ctrl Pts',(-6.303527553,4.819390921,3.581625384));
#156135=CARTESIAN_POINT('Ctrl Pts',(-6.28988261791864,4.81482901953652,
3.60563996255826));
#156136=CARTESIAN_POINT('Ctrl Pts',(-6.27623768283663,4.81026711807287,
3.62965454111647));
#156137=CARTESIAN_POINT('Ctrl Pts',(-6.91034842971931,4.95685568835189,
2.73447052920114));
#156138=CARTESIAN_POINT('Ctrl Pts',(-6.75192226837977,4.88876675808259,
3.13483321667203));
#156139=CARTESIAN_POINT('Ctrl Pts',(-6.548319939,4.819390921,3.514221174));
#156140=CARTESIAN_POINT('Ctrl Pts',(-6.53493179402859,4.81482901953652,
3.5391683393324));
#156141=CARTESIAN_POINT('Ctrl Pts',(-6.52154364905773,4.81026711807287,
3.56411550466487));
#156142=CARTESIAN_POINT('',(-6.65341820032519,4.94797309994886,2.88002202749723));
#156143=CARTESIAN_POINT('Origin',(0.156351623027657,4.69654720595462,-0.112269673876696));
#156144=CARTESIAN_POINT('Ctrl Pts',(-6.71019411991621,4.93794661929365,
2.90506789926301));
#156145=CARTESIAN_POINT('Ctrl Pts',(-6.69125700190066,4.94124830104398,
2.8967299597595));
#156146=CARTESIAN_POINT('Ctrl Pts',(-6.67233156532678,4.94458995962745,
2.88838120181602));
#156147=CARTESIAN_POINT('Ctrl Pts',(-6.65341776657222,4.94797285537006,
2.88002291003781));
#156148=CARTESIAN_POINT('Ctrl Pts',(-6.92723831926984,4.81811592995213,
2.13305060920743));
#156149=CARTESIAN_POINT('Ctrl Pts',(-6.92607598581492,4.81875342547607,
2.13681084778371));
#156150=CARTESIAN_POINT('Ctrl Pts',(-6.92491365236001,4.819390921,2.14057108636));
#156151=CARTESIAN_POINT('Ctrl Pts',(-6.92305568165001,4.820409947,2.14658176523));
#156152=CARTESIAN_POINT('Ctrl Pts',(-6.92118727974,4.821428571,2.15258920948));
#156153=CARTESIAN_POINT('Ctrl Pts',(-6.80549598965,4.884501699,2.52456965116));
#156154=CARTESIAN_POINT('Ctrl Pts',(-6.6506019875,4.948754474,2.88200743695));
#156155=CARTESIAN_POINT('Ctrl Pts',(-6.92842527283416,4.81811592995213,
2.13529511646558));
#156156=CARTESIAN_POINT('Ctrl Pts',(-6.92726171991708,4.81875342547607,
2.13905599823279));
#156157=CARTESIAN_POINT('Ctrl Pts',(-6.926098167,4.819390921,2.14281688));
#156158=CARTESIAN_POINT('Ctrl Pts',(-6.924238247,4.820409947,2.148828587));
#156159=CARTESIAN_POINT('Ctrl Pts',(-6.922367894,4.821428571,2.154837056));
#156160=CARTESIAN_POINT('Ctrl Pts',(-6.806555793,4.884501699,2.52688095));
#156161=CARTESIAN_POINT('Ctrl Pts',(-6.651534875,4.948754474,2.884368874));
#156162=CARTESIAN_POINT('Ctrl Pts',(-7.04712062926671,4.81811592995213,
2.35974584228107));
#156163=CARTESIAN_POINT('Ctrl Pts',(-7.04583513013336,4.81875342547607,
2.36357104314054));
#156164=CARTESIAN_POINT('Ctrl Pts',(-7.04454963100001,4.819390921,2.367396244));
#156165=CARTESIAN_POINT('Ctrl Pts',(-7.042494782,4.820409947,2.373510764));
#156166=CARTESIAN_POINT('Ctrl Pts',(-7.04042932,4.821428571,2.379621708));
#156167=CARTESIAN_POINT('Ctrl Pts',(-6.91253612799999,4.884501699,2.758010834));
#156168=CARTESIAN_POINT('Ctrl Pts',(-6.744823625,4.948754474,3.120512579));
#156169=CARTESIAN_POINT('Origin',(0.164726360945872,5.08885438716697,-0.0967156443673012));
#156170=CARTESIAN_POINT('Ctrl Pts',(-7.12512740838388,4.95685569400282,
1.33005002914295));
#156171=CARTESIAN_POINT('Ctrl Pts',(-7.04806871480836,4.88876676097111,
1.74285631658049));
#156172=CARTESIAN_POINT('Ctrl Pts',(-6.92385237336,4.819390921,2.14400139464));
#156173=CARTESIAN_POINT('Ctrl Pts',(-6.91568435966481,4.81482901872219,
2.17037923231526));
#156174=CARTESIAN_POINT('Ctrl Pts',(-6.90751634597049,4.81026711644424,
2.19675706999057));
#156175=CARTESIAN_POINT('Ctrl Pts',(-7.12722138118998,4.95685569400282,
1.32861408279614));
#156176=CARTESIAN_POINT('Ctrl Pts',(-7.05024588158478,4.88876676097111,
1.74154168808874));
#156177=CARTESIAN_POINT('Ctrl Pts',(-6.926098167,4.819390921,2.14281688));
#156178=CARTESIAN_POINT('Ctrl Pts',(-6.91793466595719,4.81482901872219,
2.16920327348772));
#156179=CARTESIAN_POINT('Ctrl Pts',(-6.90977116491436,4.81026711644424,
2.19558966697542));
#156180=CARTESIAN_POINT('Ctrl Pts',(-7.3366186618006,4.95685569400282,1.18501944811523));
#156181=CARTESIAN_POINT('Ctrl Pts',(-7.26796255922654,4.88876676097111,
1.61007883891379));
#156182=CARTESIAN_POINT('Ctrl Pts',(-7.150677531,4.819390921,2.024365416));
#156183=CARTESIAN_POINT('Ctrl Pts',(-7.14296529518933,4.81482901872219,
2.05160739073463));
#156184=CARTESIAN_POINT('Ctrl Pts',(-7.13525305937811,4.81026711644424,
2.07884936546924));
#156185=CARTESIAN_POINT('',(-7.11698457125967,4.94797311770983,1.38240044863595));
#156186=CARTESIAN_POINT('Origin',(0.17683115899466,4.69654717205242,-0.0760339757490586));
#156187=CARTESIAN_POINT('Ctrl Pts',(-7.17781723575636,4.93794661952795,
1.39465564104632));
#156188=CARTESIAN_POINT('Ctrl Pts',(-7.15753041337576,4.94124830639808,
1.39058355349331));
#156189=CARTESIAN_POINT('Ctrl Pts',(-7.13725267401122,4.94458997048373,
1.38649838771534));
#156190=CARTESIAN_POINT('Ctrl Pts',(-7.11698425112877,4.94797287196985,
1.38240140852592));
#156191=CARTESIAN_POINT('Ctrl Pts',(-7.22382616583707,4.8181159299523,0.594029601741248));
#156192=CARTESIAN_POINT('Ctrl Pts',(-7.22349934711854,4.81875342547615,
0.597951795075624));
#156193=CARTESIAN_POINT('Ctrl Pts',(-7.22317252840001,4.819390921,0.60187398841));
#156194=CARTESIAN_POINT('Ctrl Pts',(-7.22265011411001,4.820409947,0.60814354927));
#156195=CARTESIAN_POINT('Ctrl Pts',(-7.22211681729,4.821428571,0.61441219304));
#156196=CARTESIAN_POINT('Ctrl Pts',(-7.18909512433,4.884501699,1.00256614643));
#156197=CARTESIAN_POINT('Ctrl Pts',(-7.11466101674,4.948754474,1.38494486827));
#156198=CARTESIAN_POINT('Ctrl Pts',(-7.22546787182024,4.8181159299523,0.595966473718428));
#156199=CARTESIAN_POINT('Ctrl Pts',(-7.22514000041012,4.81875342547615,
0.599889557359214));
#156200=CARTESIAN_POINT('Ctrl Pts',(-7.22481212900001,4.819390921,0.603812641));
#156201=CARTESIAN_POINT('Ctrl Pts',(-7.224288032,4.820409947,0.610083625));
#156202=CARTESIAN_POINT('Ctrl Pts',(-7.22375305,4.821428571,0.616353689));
#156203=CARTESIAN_POINT('Ctrl Pts',(-7.190627011,4.884501699,1.004595582));
#156204=CARTESIAN_POINT('Ctrl Pts',(-7.116079733,4.948754474,1.387050553));
#156205=CARTESIAN_POINT('Ctrl Pts',(-7.3896384701368,4.8181159299523,0.789653671436417));
#156206=CARTESIAN_POINT('Ctrl Pts',(-7.3892053295684,4.81875342547615,0.793665785718209));
#156207=CARTESIAN_POINT('Ctrl Pts',(-7.388772189,4.819390921,0.7976779));
#156208=CARTESIAN_POINT('Ctrl Pts',(-7.388079821,4.820409947,0.804091198));
#156209=CARTESIAN_POINT('Ctrl Pts',(-7.387376321,4.821428571,0.810503285));
#156210=CARTESIAN_POINT('Ctrl Pts',(-7.343815678,4.884501699,1.207539139));
#156211=CARTESIAN_POINT('Ctrl Pts',(-7.257951359,4.948754474,1.597619026));
#156212=CARTESIAN_POINT('Origin',(0.181669057018288,5.08885504760921,-0.0590436952889718));
#156213=CARTESIAN_POINT('Ctrl Pts',(-7.24446733055631,4.95685568893944,
-0.232737546559316));
#156214=CARTESIAN_POINT('Ctrl Pts',(-7.25795137311849,4.88876675838292,
0.186982886110066));
#156215=CARTESIAN_POINT('Ctrl Pts',(-7.22287347641,4.819390921,0.605452241600001));
#156216=CARTESIAN_POINT('Ctrl Pts',(-7.22056688208267,4.81482901940451,
0.632969257502106));
#156217=CARTESIAN_POINT('Ctrl Pts',(-7.21826028775529,4.81026711780884,
0.660486273404169));
#156218=CARTESIAN_POINT('Ctrl Pts',(-7.24620366143262,4.95685568893944,
-0.234590063517152));
#156219=CARTESIAN_POINT('Ctrl Pts',(-7.25979503268815,4.88876675838292,
0.185230966400782));
#156220=CARTESIAN_POINT('Ctrl Pts',(-7.224812129,4.819390921,0.603812641));
#156221=CARTESIAN_POINT('Ctrl Pts',(-7.22251178106663,4.81482901940451,
0.631337042596366));
#156222=CARTESIAN_POINT('Ctrl Pts',(-7.2202114331332,4.81026711780884,0.658861444192682));
#156223=CARTESIAN_POINT('Ctrl Pts',(-7.41983674906335,4.95685568893944,
-0.419841759300748));
#156224=CARTESIAN_POINT('Ctrl Pts',(-7.44416098965419,4.88876675838292,
0.0100389954723747));
#156225=CARTESIAN_POINT('Ctrl Pts',(-7.418677388,4.819390921,0.439852581));
#156226=CARTESIAN_POINT('Ctrl Pts',(-7.41700167946185,4.81482901940451,
0.468115552022235));
#156227=CARTESIAN_POINT('Ctrl Pts',(-7.41532597092326,4.81026711780884,
0.496378523044461));
#156228=CARTESIAN_POINT('',(-7.24776867689946,4.94797309998237,-0.179860590483462));
#156229=CARTESIAN_POINT('Origin',(0.18904191733669,4.69654715983599,-0.0362428711872403));
#156230=CARTESIAN_POINT('Ctrl Pts',(-7.30981359466555,4.93794661942718,
-0.180969163199008));
#156231=CARTESIAN_POINT('Ctrl Pts',(-7.28912572194307,4.94124830104116,
-0.180584981752446));
#156232=CARTESIAN_POINT('Ctrl Pts',(-7.26844390838857,4.94458995964329,
-0.180215524655243));
#156233=CARTESIAN_POINT('Ctrl Pts',(-7.24776865382235,4.94797285551049,
-0.179859607395719));
#156234=CARTESIAN_POINT('Ctrl Pts',(-7.18263592795554,4.81811592995231,
-0.972767571003609));
#156235=CARTESIAN_POINT('Ctrl Pts',(-7.18315990615277,4.81875342547615,
-0.968866820156804));
#156236=CARTESIAN_POINT('Ctrl Pts',(-7.18368388435,4.819390921,-0.96496606931));
#156237=CARTESIAN_POINT('Ctrl Pts',(-7.18452145479,4.82040994700001,-0.95873078391));
#156238=CARTESIAN_POINT('Ctrl Pts',(-7.18534819926,4.821428571,-0.95249405318));
#156239=CARTESIAN_POINT('Ctrl Pts',(-7.23654016133,4.884501699,-0.566316237149999));
#156240=CARTESIAN_POINT('Ctrl Pts',(-7.24604640355999,4.948754474,-0.17687618393));
#156241=CARTESIAN_POINT('Ctrl Pts',(-7.18465562199173,4.81811592995231,
-0.971228900270977));
#156242=CARTESIAN_POINT('Ctrl Pts',(-7.18517876349587,4.81875342547615,
-0.967327053635489));
#156243=CARTESIAN_POINT('Ctrl Pts',(-7.185701905,4.819390921,-0.963425207));
#156244=CARTESIAN_POINT('Ctrl Pts',(-7.186538138,4.82040994700001,-0.95718817));
#156245=CARTESIAN_POINT('Ctrl Pts',(-7.187363542,4.821428571,-0.95094969));
#156246=CARTESIAN_POINT('Ctrl Pts',(-7.238472502,4.884501699,-0.564663559));
#156247=CARTESIAN_POINT('Ctrl Pts',(-7.247884611,4.948754474,-0.175124711));
#156248=CARTESIAN_POINT('Ctrl Pts',(-7.38662502560986,4.81811592995231,
-0.817361827007792));
#156249=CARTESIAN_POINT('Ctrl Pts',(-7.38706449780493,4.81875342547615,
-0.813350401503896));
#156250=CARTESIAN_POINT('Ctrl Pts',(-7.38750397,4.819390921,-0.809338976));
#156251=CARTESIAN_POINT('Ctrl Pts',(-7.388206459,4.82040994700001,-0.802926779000001));
#156252=CARTESIAN_POINT('Ctrl Pts',(-7.388897816,4.821428571,-0.796513372));
#156253=CARTESIAN_POINT('Ctrl Pts',(-7.431706569,4.884501699,-0.399395744));
#156254=CARTESIAN_POINT('Ctrl Pts',(-7.431705355,4.948754474,2.2582E-5));
#156255=CARTESIAN_POINT('Origin',(0.190112165852048,5.08885462582407,-0.0186099193378765));
#156256=CARTESIAN_POINT('Ctrl Pts',(-7.02506401246283,4.95685569218473,
-1.78464262253522));
#156257=CARTESIAN_POINT('Ctrl Pts',(-7.12846029442096,4.88876676004178,
-1.37763368220099));
#156258=CARTESIAN_POINT('Ctrl Pts',(-7.18416104268,4.819390921,-0.96140718635));
#156259=CARTESIAN_POINT('Ctrl Pts',(-7.18782372009859,4.81482901964336,
-0.934037654790715));
#156260=CARTESIAN_POINT('Ctrl Pts',(-7.1914863975165,4.81026711828654,-0.90666812323139));
#156261=CARTESIAN_POINT('Ctrl Pts',(-7.0263615124981,4.95685569218473,-1.78682508849492));
#156262=CARTESIAN_POINT('Ctrl Pts',(-7.12988423930301,4.88876676004178,
-1.37974097530298));
#156263=CARTESIAN_POINT('Ctrl Pts',(-7.185701905,4.819390921,-0.963425207));
#156264=CARTESIAN_POINT('Ctrl Pts',(-7.1893722704815,4.81482901964336,-0.936049805210888));
#156265=CARTESIAN_POINT('Ctrl Pts',(-7.19304263596297,4.81026711828654,
-0.908674403421743));
#156266=CARTESIAN_POINT('Ctrl Pts',(-7.15611151602414,4.95685569218473,
-2.0050716844652));
#156267=CARTESIAN_POINT('Ctrl Pts',(-7.27227872750701,4.88876676004178,
-1.59047028550176));
#156268=CARTESIAN_POINT('Ctrl Pts',(-7.339788137,4.819390921,-1.165227272));
#156269=CARTESIAN_POINT('Ctrl Pts',(-7.34422730877804,4.81482901964336,
-1.13726484722787));
#156270=CARTESIAN_POINT('Ctrl Pts',(-7.34866648055661,4.81026711828654,
-1.10930242245574));
#156271=CARTESIAN_POINT('',(-7.03965514124212,4.94797311768998,-1.7337115899803));
#156272=CARTESIAN_POINT('Origin',(0.192413371046692,4.69654719529238,0.00524289899331731));
#156273=CARTESIAN_POINT('Ctrl Pts',(-7.10001119442563,4.93794661929334,
-1.74813205044452));
#156274=CARTESIAN_POINT('Ctrl Pts',(-7.07988954751257,4.94124830637727,
-1.74330956268131));
#156275=CARTESIAN_POINT('Ctrl Pts',(-7.05977065306694,4.9445899704517,-1.73850275691499));
#156276=CARTESIAN_POINT('Ctrl Pts',(-7.03965525371808,4.94797287189028,
-1.73371058431184));
#156277=CARTESIAN_POINT('Ctrl Pts',(-6.80559361859715,4.81811592995213,
-2.49407921308506));
#156278=CARTESIAN_POINT('Ctrl Pts',(-6.80694389264858,4.81875342547607,
-2.49038229955253));
#156279=CARTESIAN_POINT('Ctrl Pts',(-6.80829416670001,4.819390921,-2.48668538602));
#156280=CARTESIAN_POINT('Ctrl Pts',(-6.81045255733,4.820409947,-2.48077593118));
#156281=CARTESIAN_POINT('Ctrl Pts',(-6.81260068542,4.821428571,-2.47486273772));
#156282=CARTESIAN_POINT('Ctrl Pts',(-6.94561262344,4.884501699,-2.10871830233));
#156283=CARTESIAN_POINT('Ctrl Pts',(-7.03861471392,4.948754474,-1.7304267022));
#156284=CARTESIAN_POINT('Ctrl Pts',(-6.80789686203718,4.81811592995213,
-2.49301069013484));
#156285=CARTESIAN_POINT('Ctrl Pts',(-6.80924655451859,4.81875342547607,
-2.48931252656742));
#156286=CARTESIAN_POINT('Ctrl Pts',(-6.810596247,4.819390921,-2.485614363));
#156287=CARTESIAN_POINT('Ctrl Pts',(-6.81275370800001,4.820409947,-2.47970291));
#156288=CARTESIAN_POINT('Ctrl Pts',(-6.814900903,4.821428571,-2.47378772));
#156289=CARTESIAN_POINT('Ctrl Pts',(-6.947855064,4.884501699,-2.107519659));
#156290=CARTESIAN_POINT('Ctrl Pts',(-7.04078646,4.948754474,-1.729111338));
#156291=CARTESIAN_POINT('Ctrl Pts',(-7.03822120603974,4.81811592995213,
-2.38615839511329));
#156292=CARTESIAN_POINT('Ctrl Pts',(-7.03951274151988,4.81875342547607,
-2.38233522805665));
#156293=CARTESIAN_POINT('Ctrl Pts',(-7.040804277,4.819390921,-2.378512061));
#156294=CARTESIAN_POINT('Ctrl Pts',(-7.042868775,4.820409947,-2.372400792));
#156295=CARTESIAN_POINT('Ctrl Pts',(-7.044922661,4.821428571,-2.366285948));
#156296=CARTESIAN_POINT('Ctrl Pts',(-7.17209912,4.884501699,-1.987655326));
#156297=CARTESIAN_POINT('Ctrl Pts',(-7.257961068,4.948754474,-1.597574918));
#156298=CARTESIAN_POINT('Origin',(0.189670017113995,5.08885506248735,0.0226941950227263));
#156299=CARTESIAN_POINT('Ctrl Pts',(-6.47717652379903,4.95685568712946,
-3.25309974465563));
#156300=CARTESIAN_POINT('Ctrl Pts',(-6.66565034037312,4.88876675745772,
-2.87783360445593));
#156301=CARTESIAN_POINT('Ctrl Pts',(-6.80952522398,4.819390921,-2.4833122827));
#156302=CARTESIAN_POINT('Ctrl Pts',(-6.81898590893967,4.81482902029794,
-2.45737000673472));
#156303=CARTESIAN_POINT('Ctrl Pts',(-6.82844659389913,4.81026711959574,
-2.43142773077));
#156304=CARTESIAN_POINT('Ctrl Pts',(-6.47797452333863,4.95685568712946,
-3.25551010993541));
#156305=CARTESIAN_POINT('Ctrl Pts',(-6.6665879885029,4.88876675745772,-2.88019773628271));
#156306=CARTESIAN_POINT('Ctrl Pts',(-6.810596247,4.819390921,-2.485614363));
#156307=CARTESIAN_POINT('Ctrl Pts',(-6.82006570220355,4.81482902029794,
-2.45966800675379));
#156308=CARTESIAN_POINT('Ctrl Pts',(-6.82953515740693,4.81026711959574,
-2.4337216505078));
#156309=CARTESIAN_POINT('Ctrl Pts',(-6.55777447729816,4.95685568712946,
-3.49654663791317));
#156310=CARTESIAN_POINT('Ctrl Pts',(-6.76035280148079,4.88876675745772,
-3.11661091896105));
#156311=CARTESIAN_POINT('Ctrl Pts',(-6.917698549,4.819390921,-2.715822393));
#156312=CARTESIAN_POINT('Ctrl Pts',(-6.92804502859184,4.81482902029794,
-2.68946800865921));
#156313=CARTESIAN_POINT('Ctrl Pts',(-6.93839150818421,4.81026711959574,
-2.66311362431852));
#156314=CARTESIAN_POINT('',(-6.50237519691556,4.9479731000183,-3.20649612919631));
#156315=CARTESIAN_POINT('Origin',(0.186787698060051,4.69654717645868,0.0464834694545685));
#156316=CARTESIAN_POINT('Ctrl Pts',(-6.55822016114327,4.93794661955904,
-3.23355422788455));
#156317=CARTESIAN_POINT('Ctrl Pts',(-6.53960567031831,4.94124830107305,
-3.22451894133828));
#156318=CARTESIAN_POINT('Ctrl Pts',(-6.52099049576717,4.94458995968661,
-3.21549956301667));
#156319=CARTESIAN_POINT('Ctrl Pts',(-6.50237558887183,4.94797285554171,
-3.20649522704559));
#156320=CARTESIAN_POINT('Ctrl Pts',(-6.11032931624113,4.81811592995213,
-3.89877048441623));
#156321=CARTESIAN_POINT('Ctrl Pts',(-6.11244274850557,4.81875342547607,
-3.89545027115312));
#156322=CARTESIAN_POINT('Ctrl Pts',(-6.11455618077,4.819390921,-3.89213005789));
#156323=CARTESIAN_POINT('Ctrl Pts',(-6.11793446712,4.820409947,-3.88682275217));
#156324=CARTESIAN_POINT('Ctrl Pts',(-6.1213035352,4.821428571,-3.88150959062));
#156325=CARTESIAN_POINT('Ctrl Pts',(-6.32991595857,4.884501699,-3.55251904328));
#156326=CARTESIAN_POINT('Ctrl Pts',(-6.50206522372001,4.948754474,-3.20306439151));
#156327=CARTESIAN_POINT('Ctrl Pts',(-6.11280841197595,4.81811592995213,
-3.89822207217761));
#156328=CARTESIAN_POINT('Ctrl Pts',(-6.11492154498798,4.81875342547607,
-3.89490051308881));
#156329=CARTESIAN_POINT('Ctrl Pts',(-6.117034678,4.819390921,-3.891578954));
#156330=CARTESIAN_POINT('Ctrl Pts',(-6.120412486,4.820409947,-3.886269497));
#156331=CARTESIAN_POINT('Ctrl Pts',(-6.123781072,4.821428571,-3.880954185));
#156332=CARTESIAN_POINT('Ctrl Pts',(-6.332363645,4.884501699,-3.551830482));
#156333=CARTESIAN_POINT('Ctrl Pts',(-6.50446896,4.948754474,-3.202246641));
#156334=CARTESIAN_POINT('Ctrl Pts',(-6.36071798545746,4.81811592995213,
-3.84338084831584));
#156335=CARTESIAN_POINT('Ctrl Pts',(-6.36280119322874,4.81875342547607,
-3.83992470665792));
#156336=CARTESIAN_POINT('Ctrl Pts',(-6.364884401,4.819390921,-3.836468565));
#156337=CARTESIAN_POINT('Ctrl Pts',(-6.368214374,4.820409947,-3.83094398));
#156338=CARTESIAN_POINT('Ctrl Pts',(-6.371534752,4.821428571,-3.825413623));
#156339=CARTESIAN_POINT('Ctrl Pts',(-6.577132288,4.884501699,-3.482974354));
#156340=CARTESIAN_POINT('Ctrl Pts',(-6.74484258800001,4.948754474,-3.12047159));
#156341=CARTESIAN_POINT('Origin',(0.180357139429196,5.08885511133933,0.0629370989123257));
#156342=CARTESIAN_POINT('Ctrl Pts',(-5.62642342793858,4.95685569311866,
-4.56944559844393));
#156343=CARTESIAN_POINT('Ctrl Pts',(-5.89116197315354,4.88876676051917,
-4.24346925844328));
#156344=CARTESIAN_POINT('Ctrl Pts',(-6.11648357412,4.819390921,-3.88910045677));
#156345=CARTESIAN_POINT('Ctrl Pts',(-6.13129989983707,4.81482901911934,
-3.86579845835072));
#156346=CARTESIAN_POINT('Ctrl Pts',(-6.14611622555393,4.81026711723851,
-3.84249645993146));
#156347=CARTESIAN_POINT('Ctrl Pts',(-5.6266846134028,4.95685569311866,-4.57197115702515));
#156348=CARTESIAN_POINT('Ctrl Pts',(-5.8915694811121,4.88876676051917,-4.24597968480163));
#156349=CARTESIAN_POINT('Ctrl Pts',(-6.117034678,4.819390921,-3.891578954));
#156350=CARTESIAN_POINT('Ctrl Pts',(-6.13186044606048,4.81482901911934,
-3.86827485603784));
#156351=CARTESIAN_POINT('Ctrl Pts',(-6.14668621412129,4.81026711723851,
-3.84497075807568));
#156352=CARTESIAN_POINT('Ctrl Pts',(-5.65280315982447,4.95685569311866,
-4.82452701514691));
#156353=CARTESIAN_POINT('Ctrl Pts',(-5.93232027696772,4.88876676051917,
-4.49702232063717));
#156354=CARTESIAN_POINT('Ctrl Pts',(-6.172145066,4.819390921,-4.139428677));
#156355=CARTESIAN_POINT('Ctrl Pts',(-6.18791506840579,4.81482901911934,
-4.11591462474872));
#156356=CARTESIAN_POINT('Ctrl Pts',(-6.20368507081199,4.81026711723851,
-4.09240057249751));
#156357=CARTESIAN_POINT('',(-5.66105136716546,4.94797311770236,-4.52934849656686));
#156358=CARTESIAN_POINT('Origin',(0.172428333552543,4.69654718770639,0.085550693991383));
#156359=CARTESIAN_POINT('Ctrl Pts',(-5.7097740428877,4.93794661935847,-4.56777900152391));
#156360=CARTESIAN_POINT('Ctrl Pts',(-5.69353704127715,4.94124830632178,
-4.5549533693698));
#156361=CARTESIAN_POINT('Ctrl Pts',(-5.67729595263904,4.94458997037757,
-4.5421431261003));
#156362=CARTESIAN_POINT('Ctrl Pts',(-5.66105189175548,4.9479728717964,-4.52934763110827));
#156363=CARTESIAN_POINT('Ctrl Pts',(-5.12935280446128,4.81811592995225,
-5.12115957988297));
#156364=CARTESIAN_POINT('Ctrl Pts',(-5.13213057353563,4.81875342547613,
-5.11837131681149));
#156365=CARTESIAN_POINT('Ctrl Pts',(-5.13490834261001,4.819390921,-5.11558305374));
#156366=CARTESIAN_POINT('Ctrl Pts',(-5.13934856031,4.82040994700001,-5.11112606156001));
#156367=CARTESIAN_POINT('Ctrl Pts',(-5.14378103484,4.821428571,-5.10666136836));
#156368=CARTESIAN_POINT('Ctrl Pts',(-5.4182394588,4.884501699,-4.83020794186));
#156369=CARTESIAN_POINT('Ctrl Pts',(-5.66148638954,4.948754474,-4.5259303487));
#156370=CARTESIAN_POINT('Ctrl Pts',(-5.13189183273185,4.81811592995225,
-5.12115692153167));
#156371=CARTESIAN_POINT('Ctrl Pts',(-5.13466959886593,4.81875342547613,
-5.11836727976584));
#156372=CARTESIAN_POINT('Ctrl Pts',(-5.13744736500001,4.819390921,-5.115577638));
#156373=CARTESIAN_POINT('Ctrl Pts',(-5.141887578,4.82040994700001,-5.11111844200001));
#156374=CARTESIAN_POINT('Ctrl Pts',(-5.146320044,4.821428571,-5.106651545));
#156375=CARTESIAN_POINT('Ctrl Pts',(-5.42077794,4.884501699,-4.830061659));
#156376=CARTESIAN_POINT('Ctrl Pts',(-5.66400972,4.948754474,-4.525648449));
#156377=CARTESIAN_POINT('Ctrl Pts',(-5.38579465978926,4.81811592995225,
-5.12089108640102));
#156378=CARTESIAN_POINT('Ctrl Pts',(-5.38857213189463,4.81875342547613,
-5.11796357520052));
#156379=CARTESIAN_POINT('Ctrl Pts',(-5.391349604,4.819390921,-5.115036064));
#156380=CARTESIAN_POINT('Ctrl Pts',(-5.395789347,4.82040994700001,-5.110356486));
#156381=CARTESIAN_POINT('Ctrl Pts',(-5.40022096,4.821428571,-5.105669209));
#156382=CARTESIAN_POINT('Ctrl Pts',(-5.67462606,4.884501699,-4.815433373));
#156383=CARTESIAN_POINT('Ctrl Pts',(-5.916342766,4.948754474,-4.497458479));
#156384=CARTESIAN_POINT('Origin',(0.162609572644723,5.08885473206602,0.100236046809242));
#156385=CARTESIAN_POINT('Ctrl Pts',(-4.51258505800762,4.95685569008051,
-5.67212920879434));
#156386=CARTESIAN_POINT('Ctrl Pts',(-4.84120943276726,4.88876675896619,
-5.41068498147605));
#156387=CARTESIAN_POINT('Ctrl Pts',(-5.13744194926001,4.819390921,-5.11303861561001));
#156388=CARTESIAN_POINT('Ctrl Pts',(-5.15692112007753,4.81482901869991,
-5.09346647520961));
#156389=CARTESIAN_POINT('Ctrl Pts',(-5.17640029089601,4.81026711639968,
-5.07389433480971));
#156390=CARTESIAN_POINT('Ctrl Pts',(-4.51229721666626,4.95685569008051,
-5.67465186837979));
#156391=CARTESIAN_POINT('Ctrl Pts',(-4.84106774596149,4.88876675896619,
-5.41322431763507));
#156392=CARTESIAN_POINT('Ctrl Pts',(-5.137447365,4.819390921,-5.115577638));
#156393=CARTESIAN_POINT('Ctrl Pts',(-5.15693620874494,4.81482901869991,
-5.09600547696734));
#156394=CARTESIAN_POINT('Ctrl Pts',(-5.17642505249043,4.81026711639968,
-5.07643331593493));
#156395=CARTESIAN_POINT('Ctrl Pts',(-4.48351308253065,4.95685569008051,
-5.92691782692511));
#156396=CARTESIAN_POINT('Ctrl Pts',(-4.82689906538418,4.88876675896619,
-5.66715793353732));
#156397=CARTESIAN_POINT('Ctrl Pts',(-5.13798893900001,4.819390921,-5.369479877));
#156398=CARTESIAN_POINT('Ctrl Pts',(-5.15844507548202,4.81482901869991,
-5.34990565273664));
#156399=CARTESIAN_POINT('Ctrl Pts',(-5.17890121196401,4.81026711639968,
-5.33033142847279));
#156400=CARTESIAN_POINT('',(-4.55502311951874,4.94797310000155,-5.64041354953503));
#156401=CARTESIAN_POINT('Origin',(0.150006191366085,4.69654718716523,0.120617561408115));
#156402=CARTESIAN_POINT('Ctrl Pts',(-4.59434523651735,4.93794661933408,
-5.6884195057972));
#156403=CARTESIAN_POINT('Ctrl Pts',(-4.58124499947238,4.9412483010484,-5.67240328103802));
#156404=CARTESIAN_POINT('Ctrl Pts',(-4.56813746317855,4.94458995965945,
-5.6564012061072));
#156405=CARTESIAN_POINT('Ctrl Pts',(-4.55502385387762,4.94797285546293,
-5.64041289547318));
#156406=CARTESIAN_POINT('Ctrl Pts',(-3.90853345679646,4.81811592995226,
-6.10408894376807));
#156407=CARTESIAN_POINT('Ctrl Pts',(-3.91184567755823,4.81875342547613,
-6.10196300756403));
#156408=CARTESIAN_POINT('Ctrl Pts',(-3.91515789832001,4.819390921,-6.09983707136));
#156409=CARTESIAN_POINT('Ctrl Pts',(-3.92045242816,4.820409947,-6.09643879767));
#156410=CARTESIAN_POINT('Ctrl Pts',(-3.92574105073,4.821428571,-6.09303133678));
#156411=CARTESIAN_POINT('Ctrl Pts',(-4.25321210359,4.884501699,-5.88204168643));
#156412=CARTESIAN_POINT('Ctrl Pts',(-4.5561827445,4.948754474,-5.6371688346));
#156413=CARTESIAN_POINT('Ctrl Pts',(-3.91101369547004,4.81811592995226,
-6.10463216359936));
#156414=CARTESIAN_POINT('Ctrl Pts',(-3.91432620973502,4.81875342547613,
-6.10250488029968));
#156415=CARTESIAN_POINT('Ctrl Pts',(-3.917638724,4.819390921,-6.100377597));
#156416=CARTESIAN_POINT('Ctrl Pts',(-3.922933723,4.820409947,-6.09697717));
#156417=CARTESIAN_POINT('Ctrl Pts',(-3.928222811,4.821428571,-6.093567555));
#156418=CARTESIAN_POINT('Ctrl Pts',(-4.255722683,4.884501699,-5.882444522));
#156419=CARTESIAN_POINT('Ctrl Pts',(-4.558707681,4.948754474,-5.637435967));
#156420=CARTESIAN_POINT('Ctrl Pts',(-4.15903756282845,4.81811592995226,
-6.15895414672832));
#156421=CARTESIAN_POINT('Ctrl Pts',(-4.16237942741423,4.81875342547613,
-6.15669215386416));
#156422=CARTESIAN_POINT('Ctrl Pts',(-4.165721292,4.819390921,-6.154430161));
#156423=CARTESIAN_POINT('Ctrl Pts',(-4.171063207,4.820409947,-6.150814403));
#156424=CARTESIAN_POINT('Ctrl Pts',(-4.176398838,4.821428571,-6.147189377));
#156425=CARTESIAN_POINT('Ctrl Pts',(-4.506780624,4.884501699,-5.922728079));
#156426=CARTESIAN_POINT('Ctrl Pts',(-4.811201331,4.948754474,-5.664149207));
#156427=CARTESIAN_POINT('Origin',(0.137261010202675,5.08885510563361,0.132850046849201));
#156428=CARTESIAN_POINT('Ctrl Pts',(-3.18774320373244,4.95685569209715,
-6.50959038225223));
#156429=CARTESIAN_POINT('Ctrl Pts',(-3.56488730825351,4.88876675999702,
-6.32490309878235));
#156430=CARTESIAN_POINT('Ctrl Pts',(-3.91817924964,4.819390921,-6.09789677132001));
#156431=CARTESIAN_POINT('Ctrl Pts',(-3.94141043440046,4.81482901979346,
-6.08296966623404));
#156432=CARTESIAN_POINT('Ctrl Pts',(-3.96464161916139,4.81026711858739,
-6.06804256114847));
#156433=CARTESIAN_POINT('Ctrl Pts',(-3.18691979471379,4.95685569209715,
-6.51199218607273));
#156434=CARTESIAN_POINT('Ctrl Pts',(-3.56420305179831,4.88876675999702,
-6.32735260820541));
#156435=CARTESIAN_POINT('Ctrl Pts',(-3.917638724,4.819390921,-6.100377597));
#156436=CARTESIAN_POINT('Ctrl Pts',(-3.94087935997272,4.81482901979346,
-6.08545255115646));
#156437=CARTESIAN_POINT('Ctrl Pts',(-3.96411999594573,4.81026711858739,
-6.07052750531346));
#156438=CARTESIAN_POINT('Ctrl Pts',(-3.10457889284941,4.95685569209715,
-6.75217256812281));
#156439=CARTESIAN_POINT('Ctrl Pts',(-3.49577740627834,4.88876675999702,
-6.5723035505118));
#156440=CARTESIAN_POINT('Ctrl Pts',(-3.86358616,4.819390921,-6.348460165));
#156441=CARTESIAN_POINT('Ctrl Pts',(-3.88777191719758,4.81482901979346,
-6.33374104339812));
#156442=CARTESIAN_POINT('Ctrl Pts',(-3.91195767439497,4.81026711858739,
-6.3190219217962));
#156443=CARTESIAN_POINT('',(-3.23600699950429,4.9479731176986,-6.48773913498767));
#156444=CARTESIAN_POINT('Origin',(0.120569870483082,4.69654718513396,0.150044397100799));
#156445=CARTESIAN_POINT('Ctrl Pts',(-3.26408995160878,4.93794661963025,
-6.54307583744842));
#156446=CARTESIAN_POINT('Ctrl Pts',(-3.25473899234202,4.94124830639095,
-6.52461786857059));
#156447=CARTESIAN_POINT('Ctrl Pts',(-3.24537786108337,4.94458997045841,
-6.50617215046991));
#156448=CARTESIAN_POINT('Ctrl Pts',(-3.23600783896611,4.94797287203117,
-6.4877385697174));
#156449=CARTESIAN_POINT('Ctrl Pts',(-2.50495542924116,4.81811592995212,
-6.80159789469528));
#156450=CARTESIAN_POINT('Ctrl Pts',(-2.50864722546058,4.81875342547606,
-6.80023369102764));
#156451=CARTESIAN_POINT('Ctrl Pts',(-2.51233902168,4.819390921,-6.79886948736));
#156452=CARTESIAN_POINT('Ctrl Pts',(-2.51824029658,4.820409947,-6.79668883047));
#156453=CARTESIAN_POINT('Ctrl Pts',(-2.52413777697,4.821428571,-6.79449793217));
#156454=CARTESIAN_POINT('Ctrl Pts',(-2.88930927728,4.884501699,-6.65883769814));
#156455=CARTESIAN_POINT('Ctrl Pts',(-3.2378370587,4.948754474,-6.48481956928001));
#156456=CARTESIAN_POINT('Ctrl Pts',(-2.50726090509375,4.81811592995212,
-6.80266159234725));
#156457=CARTESIAN_POINT('Ctrl Pts',(-2.51095327754687,4.81875342547606,
-6.80129613617363));
#156458=CARTESIAN_POINT('Ctrl Pts',(-2.51464565,4.819390921,-6.79993068000001));
#156459=CARTESIAN_POINT('Ctrl Pts',(-2.520547846,4.820409947,-6.797748021));
#156460=CARTESIAN_POINT('Ctrl Pts',(-2.526446244,4.821428571,-6.795555119));
#156461=CARTESIAN_POINT('Ctrl Pts',(-2.891674563,4.884501699,-6.659770816));
#156462=CARTESIAN_POINT('Ctrl Pts',(-3.240245538,4.948754474,-6.485623243));
#156463=CARTESIAN_POINT('Ctrl Pts',(-2.73780849035282,4.81811592995212,
-6.90903135754417));
#156464=CARTESIAN_POINT('Ctrl Pts',(-2.74155848617641,4.81875342547606,
-6.90754065077208));
#156465=CARTESIAN_POINT('Ctrl Pts',(-2.745308482,4.819390921,-6.906049944));
#156466=CARTESIAN_POINT('Ctrl Pts',(-2.751302788,4.820409947,-6.903667074));
#156467=CARTESIAN_POINT('Ctrl Pts',(-2.757292947,4.821428571,-6.901273802));
#156468=CARTESIAN_POINT('Ctrl Pts',(-3.128203135,4.884501699,-6.753082602));
#156469=CARTESIAN_POINT('Ctrl Pts',(-3.481093468,4.948754474,-6.565990615));
#156470=CARTESIAN_POINT('Origin',(0.10549315056409,5.08885506891935,0.159251289995697));
#156471=CARTESIAN_POINT('Ctrl Pts',(-1.71384602885931,4.9568556919657,-7.04267033616501));
#156472=CARTESIAN_POINT('Ctrl Pts',(-2.12187502117099,4.88876675992982,
-6.94337577306025));
#156473=CARTESIAN_POINT('Ctrl Pts',(-2.51570684263,4.819390921,-6.79762405168));
#156474=CARTESIAN_POINT('Ctrl Pts',(-2.54160378198105,4.81482901971299,
-6.78803995186074));
#156475=CARTESIAN_POINT('Ctrl Pts',(-2.56750072133154,4.8102671184258,-6.7784558520405));
#156476=CARTESIAN_POINT('Ctrl Pts',(-1.71252555387243,4.9568556919657,-7.04483897854714));
#156477=CARTESIAN_POINT('Ctrl Pts',(-2.12068019013151,4.88876675992982,
-6.9456209194025));
#156478=CARTESIAN_POINT('Ctrl Pts',(-2.51464565,4.819390921,-6.79993068));
#156479=CARTESIAN_POINT('Ctrl Pts',(-2.54055137692377,4.81482901971299,
-6.79035062301057));
#156480=CARTESIAN_POINT('Ctrl Pts',(-2.56645710384759,4.8102671184258,-6.78077056602059));
#156481=CARTESIAN_POINT('Ctrl Pts',(-1.58047805518487,4.9568556919657,-7.26170321676013));
#156482=CARTESIAN_POINT('Ctrl Pts',(-2.00119708618366,4.88876675992982,
-7.1701355536279));
#156483=CARTESIAN_POINT('Ctrl Pts',(-2.408526387,4.819390921,-7.03059351200001));
#156484=CARTESIAN_POINT('Ctrl Pts',(-2.43531087119952,4.81482901971299,
-7.02141773799681));
#156485=CARTESIAN_POINT('Ctrl Pts',(-2.46209535539906,4.8102671184258,-7.01224196399419));
#156486=CARTESIAN_POINT('',(-1.76567881676234,4.94797311766291,-7.03170524848912));
#156487=CARTESIAN_POINT('Origin',(0.0854958773501102,4.69654720986263,0.172455336006564));
#156488=CARTESIAN_POINT('Ctrl Pts',(-1.78120944981267,4.93794661947598,
-7.09178521407223));
#156489=CARTESIAN_POINT('Ctrl Pts',(-1.77604502744539,4.9412483063804,-7.07174860270665));
#156490=CARTESIAN_POINT('Ctrl Pts',(-1.7708680381815,4.94458997045698,-7.05172176875845));
#156491=CARTESIAN_POINT('Ctrl Pts',(-1.76567975786171,4.94797287184847,
-7.03170487683643));
#156492=CARTESIAN_POINT('Ctrl Pts',(-0.984248470461467,4.81811592995224,
-7.18107168715767));
#156493=CARTESIAN_POINT('Ctrl Pts',(-0.988147217940733,4.81875342547613,
-7.18053300485384));
#156494=CARTESIAN_POINT('Ctrl Pts',(-0.99204596542,4.819390921,-7.17999432255));
#156495=CARTESIAN_POINT('Ctrl Pts',(-0.998278048469998,4.820409947,-7.17913324784));
#156496=CARTESIAN_POINT('Ctrl Pts',(-1.00450862757,4.821428571,-7.17826135544));
#156497=CARTESIAN_POINT('Ctrl Pts',(-1.3903055601,4.884501699,-7.1242738604));
#156498=CARTESIAN_POINT('Ctrl Pts',(-1.76809370969,4.948754474,-7.02924734988));
#156499=CARTESIAN_POINT('Ctrl Pts',(-0.986271382026669,4.81811592995224,
-7.18260612530429));
#156500=CARTESIAN_POINT('Ctrl Pts',(-0.990170961513334,4.81875342547613,
-7.18206634365215));
#156501=CARTESIAN_POINT('Ctrl Pts',(-0.994070541,4.819390921,-7.181526562));
#156502=CARTESIAN_POINT('Ctrl Pts',(-1.000303954,4.820409947,-7.18066373));
#156503=CARTESIAN_POINT('Ctrl Pts',(-1.00653586,4.821428571,-7.179790078));
#156504=CARTESIAN_POINT('Ctrl Pts',(-1.392414954,4.884501699,-7.125693629));
#156505=CARTESIAN_POINT('Ctrl Pts',(-1.770273114,4.948754474,-7.030549986));
#156506=CARTESIAN_POINT('Ctrl Pts',(-1.18856253854683,4.81811592995224,
-7.33604993996594));
#156507=CARTESIAN_POINT('Ctrl Pts',(-1.19254531877341,4.81875342547613,
-7.33540022348297));
#156508=CARTESIAN_POINT('Ctrl Pts',(-1.196528099,4.819390921,-7.33475050700001));
#156509=CARTESIAN_POINT('Ctrl Pts',(-1.202894507,4.820409947,-7.33371194600001));
#156510=CARTESIAN_POINT('Ctrl Pts',(-1.209259103,4.821428571,-7.332662334));
#156511=CARTESIAN_POINT('Ctrl Pts',(-1.603354344,4.884501699,-7.267670489));
#156512=CARTESIAN_POINT('Ctrl Pts',(-1.988213545,4.948754474,-7.160813598));
#156513=CARTESIAN_POINT('Origin',(0.0687924138857683,5.08885501609288,0.178205812545522));
#156514=CARTESIAN_POINT('Ctrl Pts',(-0.159811349130863,4.95685568709043,
-7.24644285164568));
#156515=CARTESIAN_POINT('Ctrl Pts',(-0.579646230555093,4.88876675743777,
-7.23718391136641));
#156516=CARTESIAN_POINT('Ctrl Pts',(-0.99560278045,4.819390921,-7.17950198642001));
#156517=CARTESIAN_POINT('Ctrl Pts',(-1.02295455786329,4.81482902039626,
-7.17570903455444));
#156518=CARTESIAN_POINT('Ctrl Pts',(-1.05030633527657,4.81026711979238,
-7.17191608268926));
#156519=CARTESIAN_POINT('Ctrl Pts',(-0.158055552108266,4.95685568709043,
-7.24827692929834));
#156520=CARTESIAN_POINT('Ctrl Pts',(-0.577996693906887,4.88876675743777,
-7.23911971407556));
#156521=CARTESIAN_POINT('Ctrl Pts',(-0.994070541,4.819390921,-7.181526562));
#156522=CARTESIAN_POINT('Ctrl Pts',(-1.02143003144691,4.81482902039626,
-7.17773944751295));
#156523=CARTESIAN_POINT('Ctrl Pts',(-1.04878952189387,4.81026711979238,
-7.17395233302586));
#156524=CARTESIAN_POINT('Ctrl Pts',(0.0175241501514,4.95685568709043,-7.43168469456425));
#156525=CARTESIAN_POINT('Ctrl Pts',(-0.41304302908634,4.88876675743777,
-7.43269998499101));
#156526=CARTESIAN_POINT('Ctrl Pts',(-0.840846596,4.819390921,-7.38398412));
#156527=CARTESIAN_POINT('Ctrl Pts',(-0.868977389809564,4.81482902039626,
-7.38078074335875));
#156528=CARTESIAN_POINT('Ctrl Pts',(-0.897108183619176,4.81026711979238,
-7.37757736671704));
#156529=CARTESIAN_POINT('',(-0.212789476047507,4.94797309998795,-7.24687665554507));
#156530=CARTESIAN_POINT('Origin',(0.0464242208071746,4.69654713733818,0.186802261620559));
#156531=CARTESIAN_POINT('Ctrl Pts',(-0.215041574107111,4.93794661934344,
-7.3088905962304));
#156532=CARTESIAN_POINT('Ctrl Pts',(-0.214305172576142,4.94124830105344,
-7.28821226501762));
#156533=CARTESIAN_POINT('Ctrl Pts',(-0.213554397023954,4.94458995967662,
-7.26754078098889));
#156534=CARTESIAN_POINT('Ctrl Pts',(-0.212790456728527,4.94797285555638,
-7.2468765792746));
#156535=CARTESIAN_POINT('Ctrl Pts',(0.58248085480347,4.81811592995213,-7.22476655041542));
#156536=CARTESIAN_POINT('Ctrl Pts',(0.578557456876735,4.81875342547606,
-7.22507857698772));
#156537=CARTESIAN_POINT('Ctrl Pts',(0.574634058950001,4.819390921,-7.22539060356));
#156538=CARTESIAN_POINT('Ctrl Pts',(0.56836257257,4.820409947,-7.22588937285));
#156539=CARTESIAN_POINT('Ctrl Pts',(0.5620902297,4.821428571,-7.22637725608));
#156540=CARTESIAN_POINT('Ctrl Pts',(0.17370729917,4.884501699,-7.25658689547));
#156541=CARTESIAN_POINT('Ctrl Pts',(-0.21567626421,4.948754474,-7.24499533628));
#156542=CARTESIAN_POINT('Ctrl Pts',(0.580835096616913,4.81811592995213,
-7.22669998041422));
#156543=CARTESIAN_POINT('Ctrl Pts',(0.576910649808457,4.81875342547606,
-7.22701111220712));
#156544=CARTESIAN_POINT('Ctrl Pts',(0.572986203000001,4.819390921,-7.227322244));
#156545=CARTESIAN_POINT('Ctrl Pts',(0.56671304,4.820409947,-7.227819583));
#156546=CARTESIAN_POINT('Ctrl Pts',(0.560439023,4.821428571,-7.228306033));
#156547=CARTESIAN_POINT('Ctrl Pts',(0.17195243,4.884501699,-7.258426928));
#156548=CARTESIAN_POINT('Ctrl Pts',(-0.217524687,4.948754474,-7.246736025));
#156549=CARTESIAN_POINT('Ctrl Pts',(0.416259277961255,4.81811592995213,
-7.42004298029423));
#156550=CARTESIAN_POINT('Ctrl Pts',(0.412229942980628,4.81875342547606,
-7.42026463414712));
#156551=CARTESIAN_POINT('Ctrl Pts',(0.408200608,4.819390921,-7.420486288));
#156552=CARTESIAN_POINT('Ctrl Pts',(0.401759783,4.820409947,-7.42084059800001));
#156553=CARTESIAN_POINT('Ctrl Pts',(0.395318353,4.821428571,-7.421183725));
#156554=CARTESIAN_POINT('Ctrl Pts',(-0.003534487,4.884501699,-7.442430181));
#156555=CARTESIAN_POINT('Ctrl Pts',(-0.402366966,4.948754474,-7.420804897));
#156556=CARTESIAN_POINT('Origin',(0.0288751199735729,5.08885504792801,0.18882771706922));
#156557=CARTESIAN_POINT('Ctrl Pts',(1.40169596736114,4.95685568822406,-7.11137975895541));
#156558=CARTESIAN_POINT('Ctrl Pts',(0.98968619117965,4.88876675801725,-7.19258937817722));
#156559=CARTESIAN_POINT('Ctrl Pts',(0.571054562559999,4.819390921,-7.22567438806));
#156560=CARTESIAN_POINT('Ctrl Pts',(0.543526877900215,4.81482901971525,
-7.22784993729411));
#156561=CARTESIAN_POINT('Ctrl Pts',(0.515999193240412,4.81026711843093,
-7.23002548652851));
#156562=CARTESIAN_POINT('Ctrl Pts',(1.40380498731083,4.95685568822406,-7.11279351242862));
#156563=CARTESIAN_POINT('Ctrl Pts',(0.991713302934894,4.88876675801725,
-7.19412532127777));
#156564=CARTESIAN_POINT('Ctrl Pts',(0.572986203,4.819390921,-7.227322244));
#156565=CARTESIAN_POINT('Ctrl Pts',(0.54545224049573,4.81482901971525,-7.2295051522131));
#156566=CARTESIAN_POINT('Ctrl Pts',(0.517918277991468,4.81026711843093,
-7.23168806042634));
#156567=CARTESIAN_POINT('Ctrl Pts',(1.61470698227998,4.95685568822406,-7.25416885975011));
#156568=CARTESIAN_POINT('Ctrl Pts',(1.19442447845929,4.88876675801725,-7.34771963133292));
#156569=CARTESIAN_POINT('Ctrl Pts',(0.766150247,4.819390921,-7.392107838));
#156570=CARTESIAN_POINT('Ctrl Pts',(0.737988500047442,4.81482901971525,
-7.39502664411069));
#156571=CARTESIAN_POINT('Ctrl Pts',(0.709826753094835,4.81026711843093,
-7.39794545022136));
#156572=CARTESIAN_POINT('',(1.3500496883036,4.9479730999751,-7.123192154401));
#156573=CARTESIAN_POINT('Origin',(0.00518181707668791,4.69654721187571,
0.1924151738053));
#156574=CARTESIAN_POINT('Ctrl Pts',(1.36118140704012,4.93794661927204,-7.18424037761141));
#156575=CARTESIAN_POINT('Ctrl Pts',(1.35745536226788,4.94124830104824,-7.16388718961221));
#156576=CARTESIAN_POINT('Ctrl Pts',(1.35374482708709,4.9445899596398,-7.14353759904923));
#156577=CARTESIAN_POINT('Ctrl Pts',(1.35004871438277,4.94797285546353,-7.12319229067635));
#156578=CARTESIAN_POINT('Ctrl Pts',(2.1219740218502,4.81811592995224,-6.93063935649274));
#156579=CARTESIAN_POINT('Ctrl Pts',(2.1182094271201,4.81875342547612,-6.93178750320637));
#156580=CARTESIAN_POINT('Ctrl Pts',(2.11444483239,4.819390921,-6.93293564992));
#156581=CARTESIAN_POINT('Ctrl Pts',(2.10842719028,4.820409947,-6.93477094336));
#156582=CARTESIAN_POINT('Ctrl Pts',(2.10240637238,4.821428571,-6.93659578717));
#156583=CARTESIAN_POINT('Ctrl Pts',(1.72959779769,4.884501699,-7.04958999141));
#156584=CARTESIAN_POINT('Ctrl Pts',(1.34682596407,4.948754474,-7.12197539235));
#156585=CARTESIAN_POINT('Ctrl Pts',(2.1207823708793,4.81811592995224,-6.93288137335194));
#156586=CARTESIAN_POINT('Ctrl Pts',(2.11701655943965,4.81875342547612,-6.93402887167597));
#156587=CARTESIAN_POINT('Ctrl Pts',(2.113250748,4.819390921,-6.93517637000001));
#156588=CARTESIAN_POINT('Ctrl Pts',(2.107231161,4.820409947,-6.937010627));
#156589=CARTESIAN_POINT('Ctrl Pts',(2.1012084,4.821428571,-6.938834431));
#156590=CARTESIAN_POINT('Ctrl Pts',(1.728279509,4.884501699,-7.05176425));
#156591=CARTESIAN_POINT('Ctrl Pts',(1.345394953,4.948754474,-7.12407274100001));
#156592=CARTESIAN_POINT('Ctrl Pts',(2.00161727379,4.81811592995224,-7.15708305927198));
#156593=CARTESIAN_POINT('Ctrl Pts',(1.997729791395,4.81875342547612,-7.15816571863599));
#156594=CARTESIAN_POINT('Ctrl Pts',(1.993842309,4.819390921,-7.159248378));
#156595=CARTESIAN_POINT('Ctrl Pts',(1.987628233,4.820409947,-7.160978991));
#156596=CARTESIAN_POINT('Ctrl Pts',(1.981411162,4.821428571,-7.162698814));
#156597=CARTESIAN_POINT('Ctrl Pts',(1.59645064,4.884501699,-7.269190109));
#156598=CARTESIAN_POINT('Ctrl Pts',(1.202293846,4.948754474,-7.333807606));
#156599=CARTESIAN_POINT('Origin',(-0.0123919794028246,5.08885456115538,
0.190618511251751));
#156600=CARTESIAN_POINT('Ctrl Pts',(2.89766155263498,4.95685569176659,-6.64379644459623));
#156601=CARTESIAN_POINT('Ctrl Pts',(2.51274199308637,4.88876675982804,-6.81167735636691));
#156602=CARTESIAN_POINT('Ctrl Pts',(2.11101002792,4.819390921,-6.93398228561));
#156603=CARTESIAN_POINT('Ctrl Pts',(2.08459360491011,4.81482901987171,-6.94202460991387));
#156604=CARTESIAN_POINT('Ctrl Pts',(2.0581771819,4.81026711874384,-6.95006693421685));
#156605=CARTESIAN_POINT('Ctrl Pts',(2.90002518007121,4.95685569176659,-6.64472376834042));
#156606=CARTESIAN_POINT('Ctrl Pts',(2.51505189446649,4.88876675982804,-6.81274162086169));
#156607=CARTESIAN_POINT('Ctrl Pts',(2.113250748,4.819390921,-6.93517637));
#156608=CARTESIAN_POINT('Ctrl Pts',(2.08682977588114,4.81482901987171,-6.94322723078481));
#156609=CARTESIAN_POINT('Ctrl Pts',(2.06040880376209,4.81026711874384,-6.9512780915691));
#156610=CARTESIAN_POINT('Ctrl Pts',(3.13638792369391,4.95685569176659,-6.73745614275944));
#156611=CARTESIAN_POINT('Ctrl Pts',(2.74604203247821,4.88876675982804,-6.91916807033975));
#156612=CARTESIAN_POINT('Ctrl Pts',(2.337322756,4.819390921,-7.054584809));
#156613=CARTESIAN_POINT('Ctrl Pts',(2.31044687298363,4.81482901987171,-7.06348931787967));
#156614=CARTESIAN_POINT('Ctrl Pts',(2.28357098996724,4.81026711874384,-7.0723938267588));
#156615=CARTESIAN_POINT('',(2.84976204342522,4.94797311766865,-6.66643508049058));
#156616=CARTESIAN_POINT('Origin',(-0.0363028520273356,4.69654719454111,
0.189030396997524));
#156617=CARTESIAN_POINT('Ctrl Pts',(2.87375706015906,4.93794661954414,-6.72366306308529));
#156618=CARTESIAN_POINT('Ctrl Pts',(2.86574277996985,4.94124830641424,-6.7045866805003));
#156619=CARTESIAN_POINT('Ctrl Pts',(2.85774442166727,4.944589970506,-6.68551047643368));
#156620=CARTESIAN_POINT('Ctrl Pts',(2.84976106911649,4.94797287194898,-6.66643535407212));
#156621=CARTESIAN_POINT('Ctrl Pts',(3.56224604129919,4.81811592995226,-6.31244316851444));
#156622=CARTESIAN_POINT('Ctrl Pts',(3.55881627853959,4.81875342547613,-6.31437374918723));
#156623=CARTESIAN_POINT('Ctrl Pts',(3.55538651578,4.819390921,-6.31630432986));
#156624=CARTESIAN_POINT('Ctrl Pts',(3.54990409701001,4.82040994700001,-6.31939033098));
#156625=CARTESIAN_POINT('Ctrl Pts',(3.5444163292,4.821428571,-6.32246680877));
#156626=CARTESIAN_POINT('Ctrl Pts',(3.20461422651,4.884501699,-6.51296209527));
#156627=CARTESIAN_POINT('Ctrl Pts',(2.84635210687,4.948754474,-6.66593979512));
#156628=CARTESIAN_POINT('Ctrl Pts',(3.56156421782362,4.81811592995226,-6.31488893800906));
#156629=CARTESIAN_POINT('Ctrl Pts',(3.55813312741181,4.81875342547613,-6.31681914700453));
#156630=CARTESIAN_POINT('Ctrl Pts',(3.554702037,4.819390921,-6.318749356));
#156631=CARTESIAN_POINT('Ctrl Pts',(3.549217496,4.82040994700001,-6.321834763));
#156632=CARTESIAN_POINT('Ctrl Pts',(3.543727607,4.821428571,-6.324910643));
#156633=CARTESIAN_POINT('Ctrl Pts',(3.20379416,4.884501699,-6.515368914));
#156634=CARTESIAN_POINT('Ctrl Pts',(2.84540542,4.948754474,-6.668295734));
#156635=CARTESIAN_POINT('Ctrl Pts',(3.49338187026653,4.81811592995226,-6.55946588747069));
#156636=CARTESIAN_POINT('Ctrl Pts',(3.48981801463327,4.81875342547613,-6.56135892873535));
#156637=CARTESIAN_POINT('Ctrl Pts',(3.486254159,4.819390921,-6.56325197));
#156638=CARTESIAN_POINT('Ctrl Pts',(3.480557395,4.82040994700001,-6.56627796500001));
#156639=CARTESIAN_POINT('Ctrl Pts',(3.474855387,4.821428571,-6.569294066));
#156640=CARTESIAN_POINT('Ctrl Pts',(3.121787509,4.884501699,-6.756050787));
#156641=CARTESIAN_POINT('Ctrl Pts',(2.750736733,4.948754474,-6.90388962200001));
#156642=CARTESIAN_POINT('Origin',(-0.0530789841776808,5.088854266967,0.183496663322691));
#156643=CARTESIAN_POINT('Ctrl Pts',(4.25813567976833,4.95685569138745,-5.86555659771945));
#156644=CARTESIAN_POINT('Ctrl Pts',(3.91830476069365,4.88876675963424,-6.11225887305368));
#156645=CARTESIAN_POINT('Ctrl Pts',(3.55225701086,4.819390921,-6.31806487721999));
#156646=CARTESIAN_POINT('Ctrl Pts',(3.52818705236385,4.81482902010773,-6.33159792579308));
#156647=CARTESIAN_POINT('Ctrl Pts',(3.50411709386742,4.81026711921589,-6.34513097436566));
#156648=CARTESIAN_POINT('Ctrl Pts',(4.26064339410638,4.95685569138745,-5.86595413111433));
#156649=CARTESIAN_POINT('Ctrl Pts',(3.92078944326703,4.88876675963424,-6.11280169512173));
#156650=CARTESIAN_POINT('Ctrl Pts',(3.554702037,4.819390921,-6.318749356));
#156651=CARTESIAN_POINT('Ctrl Pts',(3.53062947084212,4.81482902010773,-6.33229171939924));
#156652=CARTESIAN_POINT('Ctrl Pts',(3.50655690468406,4.81026711921589,-6.34583408279862));
#156653=CARTESIAN_POINT('Ctrl Pts',(4.51141482791148,4.95685569138745,-5.9057074706027));
#156654=CARTESIAN_POINT('Ctrl Pts',(4.16925770060524,4.88876675963424,-6.16708390192625));
#156655=CARTESIAN_POINT('Ctrl Pts',(3.799204651,4.819390921,-6.387197234));
#156656=CARTESIAN_POINT('Ctrl Pts',(3.77487131866991,4.81482902010773,-6.40167108002116));
#156657=CARTESIAN_POINT('Ctrl Pts',(3.75053798634005,4.81026711921589,-6.41614492604184));
#156658=CARTESIAN_POINT('',(4.21622267410172,4.94797311771113,-5.89796293161155));
#156659=CARTESIAN_POINT('Origin',(-0.0760899040411644,4.69654718804145,
0.176806699785292));
#156660=CARTESIAN_POINT('Ctrl Pts',(4.25195902492911,4.93794661940964,-5.94869473723432));
#156661=CARTESIAN_POINT('Ctrl Pts',(4.24003125643147,4.94124830642766,-5.93178718271987));
#156662=CARTESIAN_POINT('Ctrl Pts',(4.2281190752871,4.94458997053798,-5.91487638029457));
#156663=CARTESIAN_POINT('Ctrl Pts',(4.21622178143906,4.9479728720019,-5.89796340846924));
#156664=CARTESIAN_POINT('Ctrl Pts',(4.83595139454949,4.81811592995224,-5.39908415713318));
#156665=CARTESIAN_POINT('Ctrl Pts',(4.83301683562474,4.81875342547612,-5.40170689882159));
#156666=CARTESIAN_POINT('Ctrl Pts',(4.8300822767,4.819390921,-5.40432964051));
#156667=CARTESIAN_POINT('Ctrl Pts',(4.82539143303,4.820409947,-5.40852204951));
#156668=CARTESIAN_POINT('Ctrl Pts',(4.82069331814,4.821428571,-5.41270630934));
#156669=CARTESIAN_POINT('Ctrl Pts',(4.52978645493,4.884501699,-5.67179532928999));
#156670=CARTESIAN_POINT('Ctrl Pts',(4.21278598864,4.948754474,-5.89821226196999));
#156671=CARTESIAN_POINT('Ctrl Pts',(4.83581127987154,4.81811592995224,-5.40161931777024));
#156672=CARTESIAN_POINT('Ctrl Pts',(4.83287534443577,4.81875342547612,-5.40424198188512));
#156673=CARTESIAN_POINT('Ctrl Pts',(4.829939409,4.819390921,-5.406864646));
#156674=CARTESIAN_POINT('Ctrl Pts',(4.825246365,4.820409947,-5.411056931));
#156675=CARTESIAN_POINT('Ctrl Pts',(4.82054605,4.821428571,-5.415241063));
#156676=CARTESIAN_POINT('Ctrl Pts',(4.529502956,4.884501699,-5.674322168));
#156677=CARTESIAN_POINT('Ctrl Pts',(4.212367892,4.948754474,-5.90071663));
#156678=CARTESIAN_POINT('Ctrl Pts',(4.82179981207699,4.81811592995224,-5.65513538147644));
#156679=CARTESIAN_POINT('Ctrl Pts',(4.81872622553849,4.81875342547612,-5.65775028823822));
#156680=CARTESIAN_POINT('Ctrl Pts',(4.815652639,4.819390921,-5.660365195));
#156681=CARTESIAN_POINT('Ctrl Pts',(4.81073956200001,4.820409947,-5.66454508));
#156682=CARTESIAN_POINT('Ctrl Pts',(4.805819236,4.821428571,-5.668716429));
#156683=CARTESIAN_POINT('Ctrl Pts',(4.501153063,4.884501699,-5.927006039));
#156684=CARTESIAN_POINT('Ctrl Pts',(4.170558228,4.948754474,-6.151153433));
#156685=CARTESIAN_POINT('Origin',(-0.0912841262940889,5.08885421242553,
0.167795861051647));
#156686=CARTESIAN_POINT('Ctrl Pts',(5.41950410049451,4.95685568701706,-4.81304986278409));
#156687=CARTESIAN_POINT('Ctrl Pts',(5.14065194348953,4.88876675740027,-5.12703796729849));
#156688=CARTESIAN_POINT('Ctrl Pts',(4.82740440351001,4.819390921,-5.4067217783));
#156689=CARTESIAN_POINT('Ctrl Pts',(4.8068063940441,4.81482902041816,-5.42511276003547));
#156690=CARTESIAN_POINT('Ctrl Pts',(4.78620838457831,4.81026711983679,-5.44350374177202));
#156691=CARTESIAN_POINT('Ctrl Pts',(5.42203864379239,4.95685568701706,-4.81289901763019));
#156692=CARTESIAN_POINT('Ctrl Pts',(5.14319522626593,4.88876675740027,-5.12703396517967));
#156693=CARTESIAN_POINT('Ctrl Pts',(4.829939409,4.819390921,-5.40686464600001));
#156694=CARTESIAN_POINT('Ctrl Pts',(4.80934085525011,4.81482902041816,-5.42526528535617));
#156695=CARTESIAN_POINT('Ctrl Pts',(4.78874230150022,4.81026711983679,-5.44366592471281));
#156696=CARTESIAN_POINT('Ctrl Pts',(5.67549297358001,4.95685568701706,-4.79781450224067));
#156697=CARTESIAN_POINT('Ctrl Pts',(5.39752350390582,4.88876675740026,-5.12663375329746));
#156698=CARTESIAN_POINT('Ctrl Pts',(5.083439958,4.819390921,-5.421151416));
#156699=CARTESIAN_POINT('Ctrl Pts',(5.06278697585029,4.81482902041816,-5.44051781742368));
#156700=CARTESIAN_POINT('Ctrl Pts',(5.04213399370004,4.81026711983679,-5.4598842188474));
#156701=CARTESIAN_POINT('',(5.38553741667845,4.94797309998007,-4.8537086189417));
#156702=CARTESIAN_POINT('Origin',(-0.112319138838276,4.69654718411941,0.156315944691232));
#156703=CARTESIAN_POINT('Ctrl Pts',(5.43134411167541,4.93794661940633,-4.89557205706981));
#156704=CARTESIAN_POINT('Ctrl Pts',(5.41606060857847,4.94124830110674,-4.88162393184319));
#156705=CARTESIAN_POINT('Ctrl Pts',(5.40079162965653,4.9445899597274,-4.86766928403193));
#156706=CARTESIAN_POINT('Ctrl Pts',(5.3855367237962,4.94797285563725,-4.85370931688512));
#156707=CARTESIAN_POINT('Ctrl Pts',(5.88353303667876,4.81811592995213,-4.23326996873311));
#156708=CARTESIAN_POINT('Ctrl Pts',(5.88123089797938,4.81875342547606,-4.23646223596155));
#156709=CARTESIAN_POINT('Ctrl Pts',(5.87892875928001,4.819390921,-4.23965450319));
#156710=CARTESIAN_POINT('Ctrl Pts',(5.87524882883,4.820409947,-4.2447572893));
#156711=CARTESIAN_POINT('Ctrl Pts',(5.87156004599,4.821428571,-4.24985367917));
#156712=CARTESIAN_POINT('Ctrl Pts',(5.64315090426,4.884501699,-4.56542171849));
#156713=CARTESIAN_POINT('Ctrl Pts',(5.38223467966999,4.948754474,-4.85469087829));
#156714=CARTESIAN_POINT('Ctrl Pts',(5.88394118241643,4.81811592995213,-4.23577597926327));
#156715=CARTESIAN_POINT('Ctrl Pts',(5.88163768270821,4.81875342547606,-4.23896846663164));
#156716=CARTESIAN_POINT('Ctrl Pts',(5.879334183,4.819390921,-4.242160954));
#156717=CARTESIAN_POINT('Ctrl Pts',(5.875652077,4.820409947,-4.247264092));
#156718=CARTESIAN_POINT('Ctrl Pts',(5.871961118,4.821428571,-4.25236083));
#156719=CARTESIAN_POINT('Ctrl Pts',(5.643417229,4.884501699,-4.567950425));
#156720=CARTESIAN_POINT('Ctrl Pts',(5.382364723,4.948754474,-4.857226574));
#156721=CARTESIAN_POINT('Ctrl Pts',(5.92475575618305,4.81811592995213,-4.4863770322797));
#156722=CARTESIAN_POINT('Ctrl Pts',(5.92231615559152,4.81875342547606,-4.48959153363985));
#156723=CARTESIAN_POINT('Ctrl Pts',(5.919876555,4.819390921,-4.492806035));
#156724=CARTESIAN_POINT('Ctrl Pts',(5.91597689399999,4.820409947,-4.497944362));
#156725=CARTESIAN_POINT('Ctrl Pts',(5.912068319,4.821428571,-4.503075913));
#156726=CARTESIAN_POINT('Ctrl Pts',(5.670049703,4.884501699,-4.820821076));
#156727=CARTESIAN_POINT('Ctrl Pts',(5.395369056,4.948754474,-5.110796145));
#156728=CARTESIAN_POINT('Origin',(-0.125223862622925,5.08885502181064,0.144251894682397));
#156729=CARTESIAN_POINT('Ctrl Pts',(6.32746257224836,4.95685569308826,-3.53549021668554));
#156730=CARTESIAN_POINT('Ctrl Pts',(6.12262797809732,4.88876676050363,-3.90208244265041));
#156731=CARTESIAN_POINT('Ctrl Pts',(5.8768277322,4.819390921,-4.24256637770999));
#156732=CARTESIAN_POINT('Ctrl Pts',(5.86066480615082,4.81482901928418,-4.26495535719707));
#156733=CARTESIAN_POINT('Ctrl Pts',(5.84450188010154,4.81026711756876,-4.28734433668393));
#156734=CARTESIAN_POINT('Ctrl Pts',(6.32990543207855,4.95685569308826,-3.53479804630303));
#156735=CARTESIAN_POINT('Ctrl Pts',(6.12511093998675,4.88876676050363,-3.90153180347262));
#156736=CARTESIAN_POINT('Ctrl Pts',(5.879334183,4.819390921,-4.242160954));
#156737=CARTESIAN_POINT('Ctrl Pts',(5.86317280149572,4.81482901928418,-4.26455948232562));
#156738=CARTESIAN_POINT('Ctrl Pts',(5.84701141999185,4.81026711756876,-4.28695801065105));
#156739=CARTESIAN_POINT('Ctrl Pts',(6.57419141509754,4.95685569308826,-3.46558100805243));
#156740=CARTESIAN_POINT('Ctrl Pts',(6.37340712892996,4.88876676050363,-3.84646788569382));
#156741=CARTESIAN_POINT('Ctrl Pts',(6.129979263,4.819390921,-4.201618583));
#156742=CARTESIAN_POINT('Ctrl Pts',(6.11397233598914,4.81482901928418,-4.22497199518201));
#156743=CARTESIAN_POINT('Ctrl Pts',(6.09796540897784,4.81026711756876,-4.24832540736376));
#156744=CARTESIAN_POINT('',(6.3030304192409,4.94797311771796,-3.58250023232274));
#156745=CARTESIAN_POINT('Origin',(-0.143296611127498,4.6965471432477,0.128516156270087));
#156746=CARTESIAN_POINT('Ctrl Pts',(6.35676558557265,4.93794661960481,-3.61353786707144));
#156747=CARTESIAN_POINT('Ctrl Pts',(6.33884093764623,4.94124830641803,-3.60320132726921));
#156748=CARTESIAN_POINT('Ctrl Pts',(6.32092907315555,4.94458997050698,-3.59285529378713));
#156749=CARTESIAN_POINT('Ctrl Pts',(6.30302980933956,4.94797287201421,-3.58250104001691));
#156750=CARTESIAN_POINT('Ctrl Pts',(6.65600721331838,4.81811592995226,-2.86951278315679));
#156751=CARTESIAN_POINT('Ctrl Pts',(6.6544451401742,4.81875342547613,-2.87312530844839));
#156752=CARTESIAN_POINT('Ctrl Pts',(6.65288306703001,4.819390921,-2.87673783374));
#156753=CARTESIAN_POINT('Ctrl Pts',(6.65038611907,4.820409947,-2.88251239538));
#156754=CARTESIAN_POINT('Ctrl Pts',(6.64787915151,4.821428571,-2.8882826146));
#156755=CARTESIAN_POINT('Ctrl Pts',(6.49264788863,4.884501699,-3.24557406119));
#156756=CARTESIAN_POINT('Ctrl Pts',(6.30001605838,4.948754474,-3.58416954491));
#156757=CARTESIAN_POINT('Ctrl Pts',(6.65694453501851,4.81811592995226,-2.87187246525453));
#156758=CARTESIAN_POINT('Ctrl Pts',(6.65538118000926,4.81875342547613,-2.87548549812727));
#156759=CARTESIAN_POINT('Ctrl Pts',(6.653817825,4.819390921,-2.879098531));
#156760=CARTESIAN_POINT('Ctrl Pts',(6.651318828,4.820409947,-2.884873904));
#156761=CARTESIAN_POINT('Ctrl Pts',(6.64880981,4.821428571,-2.890644931));
#156762=CARTESIAN_POINT('Ctrl Pts',(6.493451584,4.884501699,-3.247986396));
#156763=CARTESIAN_POINT('Ctrl Pts',(6.300688161,4.948754474,-3.586618002));
#156764=CARTESIAN_POINT('Ctrl Pts',(6.75067670503122,4.81811592995226,-3.1078406750286));
#156765=CARTESIAN_POINT('Ctrl Pts',(6.74898516351561,4.81875342547613,-3.1115044660143));
#156766=CARTESIAN_POINT('Ctrl Pts',(6.747293622,4.819390921,-3.115168257));
#156767=CARTESIAN_POINT('Ctrl Pts',(6.744589721,4.820409947,-3.121024766));
#156768=CARTESIAN_POINT('Ctrl Pts',(6.741875659,4.821428571,-3.126876571));
#156769=CARTESIAN_POINT('Ctrl Pts',(6.573821121,4.884501699,-3.489219877));
#156770=CARTESIAN_POINT('Ctrl Pts',(6.36789842300001,4.948754474,-3.831463711));
#156771=CARTESIAN_POINT('Origin',(-0.153306328492075,5.08885506698253,0.11396006920804));
#156772=CARTESIAN_POINT('Ctrl Pts',(6.93955589199911,4.9568556875656,-2.09261503770074));
#156773=CARTESIAN_POINT('Ctrl Pts',(6.81831671158644,4.88876675768066,-2.49466990755172));
#156774=CARTESIAN_POINT('Ctrl Pts',(6.65145712774,4.819390921,-2.88003328896));
#156775=CARTESIAN_POINT('Ctrl Pts',(6.6404850525028,4.81482902001618,-2.90537337382057));
#156776=CARTESIAN_POINT('Ctrl Pts',(6.62951297726621,4.81026711903278,-2.93071345868095));
#156777=CARTESIAN_POINT('Ctrl Pts',(6.9417928429581,4.9568556875656,-2.09141390723561));
#156778=CARTESIAN_POINT('Ctrl Pts',(6.82062325206529,4.88876675768066,-2.49359837861227));
#156779=CARTESIAN_POINT('Ctrl Pts',(6.653817825,4.819390921,-2.879098531));
#156780=CARTESIAN_POINT('Ctrl Pts',(6.64284931091445,4.81482902001618,-2.90444760941933));
#156781=CARTESIAN_POINT('Ctrl Pts',(6.63188079682888,4.81026711903278,-2.92979668783863));
#156782=CARTESIAN_POINT('Ctrl Pts',(7.16548793885633,4.9568556875656,-1.9713008607217));
#156783=CARTESIAN_POINT('Ctrl Pts',(7.0512772999503,4.88876675768066,-2.38644548466673));
#156784=CARTESIAN_POINT('Ctrl Pts',(6.889887551,4.819390921,-2.785622735));
#156785=CARTESIAN_POINT('Ctrl Pts',(6.87927515207644,4.81482902001618,-2.81187116929824));
#156786=CARTESIAN_POINT('Ctrl Pts',(6.86866275315322,4.81026711903278,-2.83811960359658));
#156787=CARTESIAN_POINT('',(6.92580073240705,4.94797309995735,-2.14377816991343));
#156788=CARTESIAN_POINT('Origin',(-0.167573576195836,4.69654721101772,0.0947069641933204));
#156789=CARTESIAN_POINT('Ctrl Pts',(6.98495176452533,4.93794661944175,-2.16253866418928));
#156790=CARTESIAN_POINT('Ctrl Pts',(6.96522416660578,4.94124830102568,-2.1562970657359));
#156791=CARTESIAN_POINT('Ctrl Pts',(6.94550701213803,4.94458995962433,-2.1500434483145));
#156792=CARTESIAN_POINT('Ctrl Pts',(6.92580039661835,4.94797285546969,-2.14377909421981));
#156793=CARTESIAN_POINT('Ctrl Pts',(7.11725388874147,4.81811592995212,-1.37158036941615));
#156794=CARTESIAN_POINT('Ctrl Pts',(7.11650492238074,4.81875342547606,-1.37544423513808));
#156795=CARTESIAN_POINT('Ctrl Pts',(7.11575595602,4.819390921,-1.37930810086));
#156796=CARTESIAN_POINT('Ctrl Pts',(7.11455874574,4.820409947,-1.385484426));
#156797=CARTESIAN_POINT('Ctrl Pts',(7.11335081559,4.821428571,-1.39165866431));
#156798=CARTESIAN_POINT('Ctrl Pts',(7.03855587389999,4.884501699,-1.77396696899));
#156799=CARTESIAN_POINT('Ctrl Pts',(6.92321568887,4.948754474,-2.14605642768));
#156800=CARTESIAN_POINT('Ctrl Pts',(7.11867655828793,4.81811592995212,-1.373683387019));
#156801=CARTESIAN_POINT('Ctrl Pts',(7.11792644914396,4.81875342547606,-1.3775480240095));
#156802=CARTESIAN_POINT('Ctrl Pts',(7.11717634,4.819390921,-1.381412661));
#156803=CARTESIAN_POINT('Ctrl Pts',(7.115977303,4.820409947,-1.387590219));
#156804=CARTESIAN_POINT('Ctrl Pts',(7.114767544,4.821428571,-1.393765687));
#156805=CARTESIAN_POINT('Ctrl Pts',(7.03985936,4.884501699,-1.776150134));
#156806=CARTESIAN_POINT('Ctrl Pts',(6.92439842400001,4.948754474,-2.148303159));
#156807=CARTESIAN_POINT('Ctrl Pts',(7.26094351293389,4.81811592995212,-1.58398514730385));
#156808=CARTESIAN_POINT('Ctrl Pts',(7.26007912546694,4.81875342547606,-1.58792691115193));
#156809=CARTESIAN_POINT('Ctrl Pts',(7.259214738,4.819390921,-1.591868675));
#156810=CARTESIAN_POINT('Ctrl Pts',(7.257833029,4.820409947,-1.598169519));
#156811=CARTESIAN_POINT('Ctrl Pts',(7.256440385,4.821428571,-1.604467956));
#156812=CARTESIAN_POINT('Ctrl Pts',(7.17020797,4.884501699,-1.994466635));
#156813=CARTESIAN_POINT('Ctrl Pts',(7.042671937,4.948754474,-2.372976291));
#156814=CARTESIAN_POINT('Origin',(-0.174217518094983,5.08885440428902,0.0783386349219456));
#156815=CARTESIAN_POINT('Ctrl Pts',(7.22716330708476,4.95685568851546,-0.551891470492521));
#156816=CARTESIAN_POINT('Ctrl Pts',(7.19518854433772,4.88876675816619,-0.970609363519733));
#156817=CARTESIAN_POINT('Ctrl Pts',(7.11507177985001,4.819390921,-1.38283304498));
#156818=CARTESIAN_POINT('Ctrl Pts',(7.10980359427104,4.81482901954,-1.40993936745616));
#156819=CARTESIAN_POINT('Ctrl Pts',(7.10453540869258,4.81026711808047,-1.43704568993249));
#156820=CARTESIAN_POINT('Ctrl Pts',(7.2290897518345,4.95685568851546,-0.550237543452612));
#156821=CARTESIAN_POINT('Ctrl Pts',(7.19721081214112,4.88876675816619,-0.96906704830979));
#156822=CARTESIAN_POINT('Ctrl Pts',(7.11717634000001,4.819390921,-1.381412661));
#156823=CARTESIAN_POINT('Ctrl Pts',(7.11191356566496,4.81482901954,-1.40852700122815));
#156824=CARTESIAN_POINT('Ctrl Pts',(7.10665079133035,4.81026711808047,-1.43564134145638));
#156825=CARTESIAN_POINT('Ctrl Pts',(7.42173422680767,4.95685568851546,-0.384844839461617));
#156826=CARTESIAN_POINT('Ctrl Pts',(7.39943759248132,4.88876675816619,-0.814835527315462));
#156827=CARTESIAN_POINT('Ctrl Pts',(7.327632355,4.819390921,-1.239374263));
#156828=CARTESIAN_POINT('Ctrl Pts',(7.32291070505559,4.81482901954,-1.26729037842628));
#156829=CARTESIAN_POINT('Ctrl Pts',(7.31818905511107,4.81026711808047,-1.2952064938526));
#156830=CARTESIAN_POINT('',(7.22472829738214,4.94797309996594,-0.604815395171998));
#156831=CARTESIAN_POINT('Origin',(-0.18401515634942,4.69654714103903,0.0564694460061609));
#156832=CARTESIAN_POINT('Ctrl Pts',(7.28652936242152,4.93794661929278,-0.610421556976864));
#156833=CARTESIAN_POINT('Ctrl Pts',(7.26592122571832,4.94124830102619,-0.608566733030478));
#156834=CARTESIAN_POINT('Ctrl Pts',(7.24532070465871,4.94458995961649,-0.606697926929616));
#156835=CARTESIAN_POINT('Ctrl Pts',(7.22472816812392,4.94797285536847,-0.604816370059737));
#156836=CARTESIAN_POINT('Ctrl Pts',(7.24570568262718,4.81811592995212,0.190485620212301));
#156837=CARTESIAN_POINT('Ctrl Pts',(7.24580484410859,4.81875342547606,0.186551083671151));
#156838=CARTESIAN_POINT('Ctrl Pts',(7.24590400559,4.819390921,0.18261654713));
#156839=CARTESIAN_POINT('Ctrl Pts',(7.24606251356999,4.820409947,0.17632725586));
#156840=CARTESIAN_POINT('Ctrl Pts',(7.24621010232,4.821428571,0.17003769794));
#156841=CARTESIAN_POINT('Ctrl Pts',(7.25534880874,4.884501699,-0.21941115215));
#156842=CARTESIAN_POINT('Ctrl Pts',(7.22269344875,4.948754474,-0.60759609609));
#156843=CARTESIAN_POINT('Ctrl Pts',(7.24754717756366,4.81811592995212,0.188737601888497));
#156844=CARTESIAN_POINT('Ctrl Pts',(7.24764538878184,4.81875342547606,0.184802066444248));
#156845=CARTESIAN_POINT('Ctrl Pts',(7.2477436,4.819390921,0.180866531));
#156846=CARTESIAN_POINT('Ctrl Pts',(7.247900589,4.820409947,0.174575643));
#156847=CARTESIAN_POINT('Ctrl Pts',(7.248046656,4.821428571,0.168284491));
#156848=CARTESIAN_POINT('Ctrl Pts',(7.257091136,4.884501699,-0.221263065));
#156849=CARTESIAN_POINT('Ctrl Pts',(7.224331513,4.948754474,-0.609536047));
#156850=CARTESIAN_POINT('Ctrl Pts',(7.43169667121216,4.81811592995212,0.0139357695080179));
#156851=CARTESIAN_POINT('Ctrl Pts',(7.43169985610608,4.81875342547606,0.00990034375400896));
#156852=CARTESIAN_POINT('Ctrl Pts',(7.431703041,4.819390921,0.005864918));
#156853=CARTESIAN_POINT('Ctrl Pts',(7.431708132,4.820409947,-0.000585643));
#156854=CARTESIAN_POINT('Ctrl Pts',(7.431702024,4.821428571,-0.007036203));
#156855=CARTESIAN_POINT('Ctrl Pts',(7.431323862,4.884501699,-0.40645435));
#156856=CARTESIAN_POINT('Ctrl Pts',(7.388137938,4.948754474,-0.803531138));
#156857=CARTESIAN_POINT('Origin',(-0.186981779434326,5.08885376242707,0.0390553085750223));
#156858=CARTESIAN_POINT('Ctrl Pts',(7.17683659769354,4.95685568833166,1.01463792187901));
#156859=CARTESIAN_POINT('Ctrl Pts',(7.23562135714399,4.88876675807225,0.59883579236326));
#156860=CARTESIAN_POINT('Ctrl Pts',(7.24599358387,4.819390921,0.1790269366));
#156861=CARTESIAN_POINT('Ctrl Pts',(7.24667562358123,4.81482901957461,0.151421840960049));
#156862=CARTESIAN_POINT('Ctrl Pts',(7.24735766329251,4.81026711814964,0.123816745320095));
#156863=CARTESIAN_POINT('Ctrl Pts',(7.1783624578197,4.95685568833166,1.01666730969899));
#156864=CARTESIAN_POINT('Ctrl Pts',(7.23726479326338,4.88876675807225,0.600776776901795));
#156865=CARTESIAN_POINT('Ctrl Pts',(7.2477436,4.819390921,0.180866531));
#156866=CARTESIAN_POINT('Ctrl Pts',(7.24843264802317,4.81482901957461,0.153254768315198));
#156867=CARTESIAN_POINT('Ctrl Pts',(7.2491216960458,4.81026711814964,0.125643005630368));
#156868=CARTESIAN_POINT('Ctrl Pts',(7.33094847043569,4.95685568833166,1.21960609169697));
#156869=CARTESIAN_POINT('Ctrl Pts',(7.40160840520117,4.88876675807225,0.794875230755259));
#156870=CARTESIAN_POINT('Ctrl Pts',(7.422745213,4.819390921,0.364825971));
#156871=CARTESIAN_POINT('Ctrl Pts',(7.42413509221002,4.81482901957461,0.336547503829866));
#156872=CARTESIAN_POINT('Ctrl Pts',(7.42552497141996,4.81026711814964,0.3082690366597));
#156873=CARTESIAN_POINT('',(7.18583559604642,4.94797309996092,0.962427875205284));
#156874=CARTESIAN_POINT('Origin',(-0.191852051531565,4.69654718848674,0.0155914013782869));
#156875=CARTESIAN_POINT('Ctrl Pts',(7.24739694602179,4.93794661920552,0.970238183677667));
#156876=CARTESIAN_POINT('Ctrl Pts',(7.2268718837182,4.94124830101889,0.967619503186338));
#156877=CARTESIAN_POINT('Ctrl Pts',(7.20635125317722,4.94458995960823,0.965016114428145));
#156878=CARTESIAN_POINT('Ctrl Pts',(7.18583567941776,4.94797285540608,0.962426895097326));
#156879=CARTESIAN_POINT('Ctrl Pts',(7.03535633396982,4.81811592995228,1.74364471283293));
#156880=CARTESIAN_POINT('Ctrl Pts',(7.03629898575991,4.81875342547614,1.73982348006647));
#156881=CARTESIAN_POINT('Ctrl Pts',(7.03724163755,4.819390921,1.7360022473));
#156882=CARTESIAN_POINT('Ctrl Pts',(7.03874845077001,4.820409947,1.72989407023));
#156883=CARTESIAN_POINT('Ctrl Pts',(7.04024465825,4.821428571,1.72378328719));
#156884=CARTESIAN_POINT('Ctrl Pts',(7.13288969786,4.884501699,1.34540408529));
#156885=CARTESIAN_POINT('Ctrl Pts',(7.18444608966999,4.948754474,0.95927475253));
#156886=CARTESIAN_POINT('Ctrl Pts',(7.03753054804711,4.81811592995228,1.74233342918212));
#156887=CARTESIAN_POINT('Ctrl Pts',(7.03847248652355,4.81875342547614,1.73851101659106));
#156888=CARTESIAN_POINT('Ctrl Pts',(7.039414425,4.819390921,1.734688604));
#156889=CARTESIAN_POINT('Ctrl Pts',(7.040920098,4.820409947,1.728578541));
#156890=CARTESIAN_POINT('Ctrl Pts',(7.042415162,4.821428571,1.722465874));
#156891=CARTESIAN_POINT('Ctrl Pts',(7.134989397,4.884501699,1.343970018));
#156892=CARTESIAN_POINT('Ctrl Pts',(7.186462889,4.948754474,0.957732292));
#156893=CARTESIAN_POINT('Ctrl Pts',(7.25495195577528,4.81811592995228,1.61120506410024));
#156894=CARTESIAN_POINT('Ctrl Pts',(7.25582256288765,4.81875342547614,1.60726466905012));
#156895=CARTESIAN_POINT('Ctrl Pts',(7.25669317,4.819390921,1.603324274));
#156896=CARTESIAN_POINT('Ctrl Pts',(7.258084821,4.820409947,1.597025618));
#156897=CARTESIAN_POINT('Ctrl Pts',(7.259465537,4.821428571,1.590724555));
#156898=CARTESIAN_POINT('Ctrl Pts',(7.344959311,4.884501699,1.200563289));
#156899=CARTESIAN_POINT('Ctrl Pts',(7.388142822,4.948754474,0.803486239));
#156900=CARTESIAN_POINT('Origin',(-0.191011727371936,5.08885504122789,-0.00205421031792302));
#156901=CARTESIAN_POINT('Ctrl Pts',(6.79092898502783,4.95685568875588,2.5337239759622));
#156902=CARTESIAN_POINT('Ctrl Pts',(6.93772455677668,4.88876675828909,2.14028005350535));
#156903=CARTESIAN_POINT('Ctrl Pts',(7.0381007817,4.819390921,1.73251581655));
#156904=CARTESIAN_POINT('Ctrl Pts',(7.04470115542056,4.81482901947769,1.70570273052457));
#156905=CARTESIAN_POINT('Ctrl Pts',(7.05130152914082,4.81026711795524,1.67888964449888));
#156906=CARTESIAN_POINT('Ctrl Pts',(6.79198291299492,4.95685568875588,2.53603393264285));
#156907=CARTESIAN_POINT('Ctrl Pts',(6.9389123159695,4.88876675828909,2.14252894909245));
#156908=CARTESIAN_POINT('Ctrl Pts',(7.039414425,4.819390921,1.734688604));
#156909=CARTESIAN_POINT('Ctrl Pts',(7.04602307639943,4.81482901947769,1.70787051338158));
#156910=CARTESIAN_POINT('Ctrl Pts',(7.0526317277983,4.81026711795524,1.68105242276316));
#156911=CARTESIAN_POINT('Ctrl Pts',(6.89737570970381,4.95685568875588,2.76702960070795));
#156912=CARTESIAN_POINT('Ctrl Pts',(7.05768823525181,4.88876675828909,2.36741850780217));
#156913=CARTESIAN_POINT('Ctrl Pts',(7.170778755,4.819390921,1.951967349));
#156914=CARTESIAN_POINT('Ctrl Pts',(7.17821517428315,4.81482901947769,1.92464879908613));
#156915=CARTESIAN_POINT('Ctrl Pts',(7.18565159356626,4.81026711795524,1.89733024917257));
#156916=CARTESIAN_POINT('',(6.81094120886271,4.94797309996511,2.48466908736485));
#156917=CARTESIAN_POINT('Origin',(-0.190718463343362,4.69654718882403,-0.0260156744271445));
#156918=CARTESIAN_POINT('Ctrl Pts',(6.869384302947,4.93794661951538,2.50553066725023));
#156919=CARTESIAN_POINT('Ctrl Pts',(6.84990204463961,4.9412483010766,2.49856092685401));
#156920=CARTESIAN_POINT('Ctrl Pts',(6.83042082661489,4.94458995967786,2.49160707485885));
#156921=CARTESIAN_POINT('Ctrl Pts',(6.81094150090676,4.94797285556573,2.48466814837251));
#156922=CARTESIAN_POINT('Ctrl Pts',(6.49604154141455,4.81811592995212,3.21527291645958));
#156923=CARTESIAN_POINT('Ctrl Pts',(6.49778360652728,4.81875342547606,3.21174366421979));
#156924=CARTESIAN_POINT('Ctrl Pts',(6.49952567164,4.819390921,3.20821441198));
#156925=CARTESIAN_POINT('Ctrl Pts',(6.50231033377,4.820409947,3.20257296093));
#156926=CARTESIAN_POINT('Ctrl Pts',(6.50508519853,4.821428571,3.19692668465));
#156927=CARTESIAN_POINT('Ctrl Pts',(6.67690459158,4.884501699,2.84730972435));
#156928=CARTESIAN_POINT('Ctrl Pts',(6.81026201690001,4.948754474,2.48129098042));
#156929=CARTESIAN_POINT('Ctrl Pts',(6.49844681077687,4.81811592995212,3.21445968164217));
#156930=CARTESIAN_POINT('Ctrl Pts',(6.50018843288844,4.81875342547606,3.21092912382109));
#156931=CARTESIAN_POINT('Ctrl Pts',(6.501930055,4.819390921,3.207398566));
#156932=CARTESIAN_POINT('Ctrl Pts',(6.504714009,4.820409947,3.201755028));
#156933=CARTESIAN_POINT('Ctrl Pts',(6.507488162,4.821428571,3.196106666));
#156934=CARTESIAN_POINT('Ctrl Pts',(6.679263483,4.884501699,2.846360558));
#156935=CARTESIAN_POINT('Ctrl Pts',(6.81256324800001,4.948754474,2.480218134));
#156936=CARTESIAN_POINT('Ctrl Pts',(6.73897374700992,4.81811592995212,3.13313619990097));
#156937=CARTESIAN_POINT('Ctrl Pts',(6.74067106900496,4.81875342547606,3.12947508395048));
#156938=CARTESIAN_POINT('Ctrl Pts',(6.742368391,4.819390921,3.125813968));
#156939=CARTESIAN_POINT('Ctrl Pts',(6.745081532,4.820409947,3.119961735));
#156940=CARTESIAN_POINT('Ctrl Pts',(6.747784509,4.821428571,3.114104801));
#156941=CARTESIAN_POINT('Ctrl Pts',(6.91515262499999,4.884501699,2.751443923));
#156942=CARTESIAN_POINT('Ctrl Pts',(7.042686358,4.948754474,2.372933492));
#156943=CARTESIAN_POINT('Origin',(-0.186104172907255,5.08885501602928,-0.0430679738727974));
#156944=CARTESIAN_POINT('Ctrl Pts',(6.08748506749854,4.95685569264032,3.93433593143617));
#156945=CARTESIAN_POINT('Ctrl Pts',(6.31542746113433,4.88876676027466,3.58164720780548));
#156946=CARTESIAN_POINT('Ctrl Pts',(6.50111420902001,4.819390921,3.20499418263));
#156947=CARTESIAN_POINT('Ctrl Pts',(6.51332429053711,4.81482901950453,3.18022685704854));
#156948=CARTESIAN_POINT('Ctrl Pts',(6.52553437205403,4.8102671180095,3.1554595314668));
#156949=CARTESIAN_POINT('Ctrl Pts',(6.08801778279943,4.95685569264032,3.93681844597466));
#156950=CARTESIAN_POINT('Ctrl Pts',(6.3161040050993,4.88876676027466,3.58409885859014));
#156951=CARTESIAN_POINT('Ctrl Pts',(6.501930055,4.819390921,3.207398566));
#156952=CARTESIAN_POINT('Ctrl Pts',(6.51414929650819,4.81482901950453,3.18262813228619));
#156953=CARTESIAN_POINT('Ctrl Pts',(6.52636853801631,4.8102671180095,3.15785769857232));
#156954=CARTESIAN_POINT('Ctrl Pts',(6.14128931288863,4.95685569264032,4.18506989982365));
#156955=CARTESIAN_POINT('Ctrl Pts',(6.38375840159689,4.88876676027466,3.82926393705604));
#156956=CARTESIAN_POINT('Ctrl Pts',(6.583514653,4.819390921,3.447836903));
#156957=CARTESIAN_POINT('Ctrl Pts',(6.59664989361871,4.81482901950453,3.42275565605227));
#156958=CARTESIAN_POINT('Ctrl Pts',(6.60978513423729,4.8102671180095,3.3976744091045));
#156959=CARTESIAN_POINT('',(6.11757475519473,4.94797311771029,3.89072994474234));
#156960=CARTESIAN_POINT('Origin',(-0.180667002327166,4.69654715766115,-0.0664062771459656));
#156961=CARTESIAN_POINT('Ctrl Pts',(6.17016688510887,4.93794661935354,3.92366731976889));
#156962=CARTESIAN_POINT('Ctrl Pts',(6.15263837057492,4.94124830638632,3.91267240131556));
#156963=CARTESIAN_POINT('Ctrl Pts',(6.13510745688151,4.94458997046307,3.90169322281712));
#156964=CARTESIAN_POINT('Ctrl Pts',(6.11757518297218,4.94797287189733,3.89072902756295));
#156965=CARTESIAN_POINT('Ctrl Pts',(5.65297906669916,4.81811592995212,4.53655853165158));
#156966=CARTESIAN_POINT('Ctrl Pts',(5.65543908785958,4.81875342547607,4.53348628412579));
#156967=CARTESIAN_POINT('Ctrl Pts',(5.65789910902,4.819390921,4.53041403660001));
#156968=CARTESIAN_POINT('Ctrl Pts',(5.66183141196,4.820409947,4.52550309999));
#156969=CARTESIAN_POINT('Ctrl Pts',(5.66575518471,4.821428571,4.52058534395));
#156970=CARTESIAN_POINT('Ctrl Pts',(5.90871484845,4.884501699,4.21607832444));
#156971=CARTESIAN_POINT('Ctrl Pts',(6.11763766114001,4.948754474,3.88728480021));
#156972=CARTESIAN_POINT('Ctrl Pts',(5.65550292364228,4.81811592995212,4.53628137163685));
#156973=CARTESIAN_POINT('Ctrl Pts',(5.65796279282114,4.81875342547607,4.53320775381843));
#156974=CARTESIAN_POINT('Ctrl Pts',(5.660422662,4.819390921,4.530134136));
#156975=CARTESIAN_POINT('Ctrl Pts',(5.664354722,4.820409947,4.525221009));
#156976=CARTESIAN_POINT('Ctrl Pts',(5.668278248,4.821428571,4.520301063));
#156977=CARTESIAN_POINT('Ctrl Pts',(5.911222633,4.884501699,4.215658441));
#156978=CARTESIAN_POINT('Ctrl Pts',(6.120115721,4.948754474,3.886731733));
#156979=CARTESIAN_POINT('Ctrl Pts',(5.90788861795456,4.81811592995212,4.50856537016347));
#156980=CARTESIAN_POINT('Ctrl Pts',(5.91033328897728,4.81875342547607,4.50535472308173));
#156981=CARTESIAN_POINT('Ctrl Pts',(5.91277796,4.819390921,4.50214407600001));
#156982=CARTESIAN_POINT('Ctrl Pts',(5.916685726,4.820409947,4.49701191));
#156983=CARTESIAN_POINT('Ctrl Pts',(5.920584577,4.821428571,4.491872968));
#156984=CARTESIAN_POINT('Ctrl Pts',(6.162001088,4.884501699,4.173670097));
#156985=CARTESIAN_POINT('Ctrl Pts',(6.367921707,4.948754474,3.831425012));
#156986=CARTESIAN_POINT('Origin',(-0.172494949443869,5.08885499938439,-0.0820680645597976));
#156987=CARTESIAN_POINT('Ctrl Pts',(5.09939714484627,4.95685568743367,5.15098266598226));
#156988=CARTESIAN_POINT('Ctrl Pts',(5.39782800952324,4.88876675761323,4.85554049568293));
#156989=CARTESIAN_POINT('Ctrl Pts',(5.6601427614,4.819390921,4.52761058301));
#156990=CARTESIAN_POINT('Ctrl Pts',(5.6773916183094,4.81482902019137,4.50604711355382));
#156991=CARTESIAN_POINT('Ctrl Pts',(5.6946404752189,4.81026711938254,4.48448364409787));
#156992=CARTESIAN_POINT('Ctrl Pts',(5.09938373833295,4.95685568743367,5.15352165875207));
#156993=CARTESIAN_POINT('Ctrl Pts',(5.39796170382317,4.88876675761323,4.85808026518442));
#156994=CARTESIAN_POINT('Ctrl Pts',(5.660422662,4.819390921,4.530134136));
#156995=CARTESIAN_POINT('Ctrl Pts',(5.67768113289997,4.81482902019137,4.50856960020544));
#156996=CARTESIAN_POINT('Ctrl Pts',(5.69493960379982,4.81026711938254,4.48700506441108));
#156997=CARTESIAN_POINT('Ctrl Pts',(5.09804308700086,4.95685568743367,5.40742093573342));
#156998=CARTESIAN_POINT('Ctrl Pts',(5.41133113381643,4.88876675761323,5.11205721533326));
#156999=CARTESIAN_POINT('Ctrl Pts',(5.688412722,4.819390921,4.782489435));
#157000=CARTESIAN_POINT('Ctrl Pts',(5.70663259195628,4.81482902019137,4.76081826536794));
#157001=CARTESIAN_POINT('Ctrl Pts',(5.72485246191249,4.81026711938254,4.73914709573632));
#157002=CARTESIAN_POINT('',(5.13815735487595,4.94797309995233,5.11486457517324));
#157003=CARTESIAN_POINT('Origin',(-0.162167537007684,4.69654715563134,-0.10369164188563));
#157004=CARTESIAN_POINT('Ctrl Pts',(5.18243932158301,4.93794661922244,5.15833764928942));
#157005=CARTESIAN_POINT('Ctrl Pts',(5.1676842196987,4.94124830104337,5.14383169758156));
#157006=CARTESIAN_POINT('Ctrl Pts',(5.15292339167731,4.94458995965422,5.12934060138166));
#157007=CARTESIAN_POINT('Ctrl Pts',(5.13815801437043,4.94797285546854,5.11486384540008));
#157008=CARTESIAN_POINT('Ctrl Pts',(4.54558957227979,4.81811592995213,5.64571971271425));
#157009=CARTESIAN_POINT('Ctrl Pts',(4.54865252210489,4.81875342547607,5.64324812455213));
#157010=CARTESIAN_POINT('Ctrl Pts',(4.55171547193,4.819390921,5.64077653638999));
#157011=CARTESIAN_POINT('Ctrl Pts',(4.55661154632,4.820409947,5.63682574379));
#157012=CARTESIAN_POINT('Ctrl Pts',(4.56150075553,4.821428571,5.6328664576));
#157013=CARTESIAN_POINT('Ctrl Pts',(4.86424016452,4.884501699,5.38770778825));
#157014=CARTESIAN_POINT('Ctrl Pts',(5.1389593677,4.948754474,5.11151350319));
#157015=CARTESIAN_POINT('Ctrl Pts',(4.54811400406023,4.81811592995213,5.64599158717321));
#157016=CARTESIAN_POINT('Ctrl Pts',(4.55117710003011,4.81875342547607,5.64351862808661));
#157017=CARTESIAN_POINT('Ctrl Pts',(4.554240196,4.819390921,5.641045669));
#157018=CARTESIAN_POINT('Ctrl Pts',(4.559136504,4.820409947,5.637092685));
#157019=CARTESIAN_POINT('Ctrl Pts',(4.564025943,4.821428571,5.633131207));
#157020=CARTESIAN_POINT('Ctrl Pts',(4.866779581,4.884501699,5.387836821));
#157021=CARTESIAN_POINT('Ctrl Pts',(5.141498385,4.948754474,5.111506076));
#157022=CARTESIAN_POINT('Ctrl Pts',(4.80055718210447,4.81811592995213,5.67317903306961));
#157023=CARTESIAN_POINT('Ctrl Pts',(4.80363489255224,4.81875342547607,5.67056898153481));
#157024=CARTESIAN_POINT('Ctrl Pts',(4.806712603,4.819390921,5.66795893));
#157025=CARTESIAN_POINT('Ctrl Pts',(4.811632272,4.820409947,5.663786806));
#157026=CARTESIAN_POINT('Ctrl Pts',(4.81654469,4.821428571,5.659606147));
#157027=CARTESIAN_POINT('Ctrl Pts',(5.120721229,4.884501699,5.400740096));
#157028=CARTESIAN_POINT('Ctrl Pts',(5.39540011500001,4.948754474,5.110763357));
#157029=CARTESIAN_POINT('Origin',(-0.150820013878292,5.08885506147785,-0.117230767712908));
#157030=CARTESIAN_POINT('Ctrl Pts',(3.87286705614322,4.95685568876092,6.12677520712686));
#157031=CARTESIAN_POINT('Ctrl Pts',(4.22783210957198,4.88876675829167,5.9023941230321));
#157032=CARTESIAN_POINT('Ctrl Pts',(4.55450932862001,4.819390921,5.63852094492999));
#157033=CARTESIAN_POINT('Ctrl Pts',(4.57599042881487,4.8148290194499,5.62116960897195));
#157034=CARTESIAN_POINT('Ctrl Pts',(4.59747152901017,4.81026711789965,5.60381827301339));
#157035=CARTESIAN_POINT('Ctrl Pts',(3.87230815465685,4.95685568876092,6.12925195764689));
#157036=CARTESIAN_POINT('Ctrl Pts',(4.22741670280422,4.88876675829167,5.90490325445912));
#157037=CARTESIAN_POINT('Ctrl Pts',(4.554240196,4.819390921,5.641045669));
#157038=CARTESIAN_POINT('Ctrl Pts',(4.57573091464835,4.8148290194499,5.62369535835715));
#157039=CARTESIAN_POINT('Ctrl Pts',(4.59722163329677,4.81026711789965,5.60634504771392));
#157040=CARTESIAN_POINT('Ctrl Pts',(3.81641800601945,4.95685568876092,6.3769270096507));
#157041=CARTESIAN_POINT('Ctrl Pts',(4.1858760260283,4.88876675829167,6.15581639716052));
#157042=CARTESIAN_POINT('Ctrl Pts',(4.527326934,4.819390921,5.893518076));
#157043=CARTESIAN_POINT('Ctrl Pts',(4.54977949799321,4.8148290194499,5.87627029687959));
#157044=CARTESIAN_POINT('Ctrl Pts',(4.57223206198565,4.81026711789965,5.85902251775936));
#157045=CARTESIAN_POINT('',(3.91848540259602,4.94797309996321,6.09983383216804));
#157046=CARTESIAN_POINT('Origin',(-0.136085764728019,4.69654715609852,-0.13612896908482));
#157047=CARTESIAN_POINT('Ctrl Pts',(3.95238665388103,4.93794661950124,6.15180984468191));
#157048=CARTESIAN_POINT('Ctrl Pts',(3.9410948705015,4.94124830105337,6.13447112212709));
#157049=CARTESIAN_POINT('Ctrl Pts',(3.92979429991244,4.9445899596633,6.11714567805156));
#157050=CARTESIAN_POINT('Ctrl Pts',(3.91848620333279,4.94797285553905,6.09983326138289));
#157051=CARTESIAN_POINT('Ctrl Pts',(3.22565336150107,4.81811592995213,6.49089331482735));
#157052=CARTESIAN_POINT('Ctrl Pts',(3.22917601981553,4.81875342547607,6.48913795466867));
#157053=CARTESIAN_POINT('Ctrl Pts',(3.23269867813,4.819390921,6.48738259451));
#157054=CARTESIAN_POINT('Ctrl Pts',(3.2383295889,4.820409947,6.48457668047));
#157055=CARTESIAN_POINT('Ctrl Pts',(3.2439556203,4.821428571,6.48176099564));
#157056=CARTESIAN_POINT('Ctrl Pts',(3.59231901789,4.884501699,6.30741402349));
#157057=CARTESIAN_POINT('Ctrl Pts',(3.91998904488,4.948754474,6.09673351488));
#157058=CARTESIAN_POINT('Ctrl Pts',(3.22806032850429,4.81811592995213,6.491701511246));
#157059=CARTESIAN_POINT('Ctrl Pts',(3.23158342425215,4.81875342547607,6.489944843623));
#157060=CARTESIAN_POINT('Ctrl Pts',(3.23510652,4.819390921,6.48818817600001));
#157061=CARTESIAN_POINT('Ctrl Pts',(3.24073813,4.820409947,6.485380172));
#157062=CARTESIAN_POINT('Ctrl Pts',(3.246364857,4.821428571,6.482562396));
#157063=CARTESIAN_POINT('Ctrl Pts',(3.594771326,4.884501699,6.308085939));
#157064=CARTESIAN_POINT('Ctrl Pts',(3.922470298,4.948754474,6.097272075));
#157065=CARTESIAN_POINT('Ctrl Pts',(3.46875702882678,4.81811592995213,6.57252115311178));
#157066=CARTESIAN_POINT('Ctrl Pts',(3.47232386791339,4.81875342547607,6.57063373905589));
#157067=CARTESIAN_POINT('Ctrl Pts',(3.475890707,4.819390921,6.568746325));
#157068=CARTESIAN_POINT('Ctrl Pts',(3.48159224,4.820409947,6.565729325));
#157069=CARTESIAN_POINT('Ctrl Pts',(3.487288527,4.821428571,6.562702432));
#157070=CARTESIAN_POINT('Ctrl Pts',(3.840002137,4.884501699,6.37527749));
#157071=CARTESIAN_POINT('Ctrl Pts',(4.17059561,4.948754474,6.151128087));
#157072=CARTESIAN_POINT('Origin',(-0.122092848167099,5.08885500771978,-0.14691196824937));
#157073=CARTESIAN_POINT('Ctrl Pts',(2.4652460103968,4.95685568917762,6.81608654441024));
#157074=CARTESIAN_POINT('Ctrl Pts',(2.86014748013306,4.88876675850466,6.67325835902554));
#157075=CARTESIAN_POINT('Ctrl Pts',(3.23591210149,4.819390921,6.48578033413));
#157076=CARTESIAN_POINT('Ctrl Pts',(3.26062101125556,4.81482901918335,6.47345246360451));
#157077=CARTESIAN_POINT('Ctrl Pts',(3.28532992102107,4.81026711736656,6.46112459307846));
#157078=CARTESIAN_POINT('Ctrl Pts',(2.46416774756807,4.95685568917762,6.81838524258134));
#157079=CARTESIAN_POINT('Ctrl Pts',(2.85920239626229,4.88876675850466,6.67561952817654));
#157080=CARTESIAN_POINT('Ctrl Pts',(3.23510652,4.819390921,6.488188176));
#157081=CARTESIAN_POINT('Ctrl Pts',(3.25982460293285,4.81482901918335,6.47586337450206));
#157082=CARTESIAN_POINT('Ctrl Pts',(3.2845426858658,4.81026711736656,6.46353857300428));
#157083=CARTESIAN_POINT('Ctrl Pts',(2.35634146469517,4.95685568917762,7.04825505969156));
#157084=CARTESIAN_POINT('Ctrl Pts',(2.76469400918577,4.88876675850466,6.91173644327635));
#157085=CARTESIAN_POINT('Ctrl Pts',(3.154548371,4.819390921,6.728972363));
#157086=CARTESIAN_POINT('Ctrl Pts',(3.1801837706632,4.81482901918335,6.71695446426431));
#157087=CARTESIAN_POINT('Ctrl Pts',(3.20581917032638,4.81026711736656,6.7049365655283));
#157088=CARTESIAN_POINT('',(2.51558942704793,4.9479730999938,6.79958163914524));
#157089=CARTESIAN_POINT('Origin',(-0.103640466394893,4.69654717413986,-0.162200810867108));
#157090=CARTESIAN_POINT('Ctrl Pts',(2.53752478034511,4.93794661939396,6.85763024779903));
#157091=CARTESIAN_POINT('Ctrl Pts',(2.53022430469866,4.94124830104487,6.83826949569286));
#157092=CARTESIAN_POINT('Ctrl Pts',(2.52291239351571,4.9445899596398,6.81891982227765));
#157093=CARTESIAN_POINT('Ctrl Pts',(2.51559033183994,4.94797285549285,6.79958125379799));
#157094=CARTESIAN_POINT('Ctrl Pts',(1.75488918513372,4.81811592995213,7.03255995761173));
#157095=CARTESIAN_POINT('Ctrl Pts',(1.75870683623686,4.81875342547607,7.03160290467086));
#157096=CARTESIAN_POINT('Ctrl Pts',(1.76252448734,4.819390921,7.03064585173001));
#157097=CARTESIAN_POINT('Ctrl Pts',(1.76862693918,4.820409947,7.02911601851));
#157098=CARTESIAN_POINT('Ctrl Pts',(1.77472672631,4.821428571,7.02757559326));
#157099=CARTESIAN_POINT('Ctrl Pts',(2.15242502647,4.884501699,6.93219258975));
#157100=CARTESIAN_POINT('Ctrl Pts',(2.51772439171,4.948754474,6.79687704404));
#157101=CARTESIAN_POINT('Ctrl Pts',(1.75706614025099,4.81811592995213,7.03386668559916));
#157102=CARTESIAN_POINT('Ctrl Pts',(1.76088449962549,4.81875342547607,7.03290844979959));
#157103=CARTESIAN_POINT('Ctrl Pts',(1.764702859,4.819390921,7.031950214));
#157104=CARTESIAN_POINT('Ctrl Pts',(1.770806443,4.820409947,7.03041849));
#157105=CARTESIAN_POINT('Ctrl Pts',(1.776907359,4.821428571,7.028876172));
#157106=CARTESIAN_POINT('Ctrl Pts',(2.154675559,4.884501699,6.93337597));
#157107=CARTESIAN_POINT('Ctrl Pts',(2.52003186,4.948754474,6.79793640900001));
#157108=CARTESIAN_POINT('Ctrl Pts',(1.9747616519787,4.81811592995213,7.16453948434252));
#157109=CARTESIAN_POINT('Ctrl Pts',(1.97865083848935,4.81875342547607,7.16346296267127));
#157110=CARTESIAN_POINT('Ctrl Pts',(1.982540025,4.819390921,7.162386441));
#157111=CARTESIAN_POINT('Ctrl Pts',(1.988756825,4.820409947,7.160665639));
#157112=CARTESIAN_POINT('Ctrl Pts',(1.994970628,4.821428571,7.158934046));
#157113=CARTESIAN_POINT('Ctrl Pts',(2.379728812,4.884501699,7.051713995));
#157114=CARTESIAN_POINT('Ctrl Pts',(2.750778689,4.948754474,6.90387290500001));
#157115=CARTESIAN_POINT('Origin',(-0.0876565393637996,5.08885494092209,
-0.169723292818464));
#157116=CARTESIAN_POINT('Ctrl Pts',(0.9423528081216,4.95685568855937,7.18668524794689));
#157117=CARTESIAN_POINT('Ctrl Pts',(1.35872553599178,4.88876675818864,7.13208844931892));
#157118=CARTESIAN_POINT('Ctrl Pts',(1.76600722127,4.819390921,7.02977184234001));
#157119=CARTESIAN_POINT('Ctrl Pts',(1.79278857613182,4.81482901954031,7.02304387626926));
#157120=CARTESIAN_POINT('Ctrl Pts',(1.81956993099389,4.81026711808049,7.01631591019912));
#157121=CARTESIAN_POINT('Ctrl Pts',(0.940805602326207,4.95685568855937,
7.18869840920379));
#157122=CARTESIAN_POINT('Ctrl Pts',(1.35729496608203,4.88876675818864,7.13419125054935));
#157123=CARTESIAN_POINT('Ctrl Pts',(1.764702859,4.819390921,7.03195021400001));
#157124=CARTESIAN_POINT('Ctrl Pts',(1.79149251281487,4.81482901954031,7.02522721716447));
#157125=CARTESIAN_POINT('Ctrl Pts',(1.81828216663001,4.81026711808049,7.01850422032941));
#157126=CARTESIAN_POINT('Ctrl Pts',(0.786085022786937,4.95685568855937,
7.39001453489349));
#157127=CARTESIAN_POINT('Ctrl Pts',(1.21423797510712,4.88876675818864,7.34447137359237));
#157128=CARTESIAN_POINT('Ctrl Pts',(1.634266632,4.819390921,7.24978738));
#157129=CARTESIAN_POINT('Ctrl Pts',(1.66188618112043,4.81482901954031,7.24356130668562));
#157130=CARTESIAN_POINT('Ctrl Pts',(1.68950573024058,4.81026711808049,7.23733523337184));
#157131=CARTESIAN_POINT('',(0.995067285914387,4.94797309999901,7.18138856534732));
#157132=CARTESIAN_POINT('Origin',(-0.0663489787352659,4.69654714665182,
-0.180687961604724));
#157133=CARTESIAN_POINT('Ctrl Pts',(1.00401106893079,4.9379466193054,7.24279548235482));
#157134=CARTESIAN_POINT('Ctrl Pts',(1.00104326306824,4.94124830106007,7.22231798754459));
#157135=CARTESIAN_POINT('Ctrl Pts',(0.998061908143027,4.94458995965412,
7.20184885391167));
#157136=CARTESIAN_POINT('Ctrl Pts',(0.995068252627058,4.94797285554153,
7.18138838348548));
#157137=CARTESIAN_POINT('Ctrl Pts',(0.202068341494658,4.81811592995213,
7.24539191659084));
#157138=CARTESIAN_POINT('Ctrl Pts',(0.206002476142329,4.81875342547607,
7.24527792053542));
#157139=CARTESIAN_POINT('Ctrl Pts',(0.20993661079,4.819390921,7.24516392448001));
#157140=CARTESIAN_POINT('Ctrl Pts',(0.21622525964,4.820409947,7.24498170368));
#157141=CARTESIAN_POINT('Ctrl Pts',(0.22251358328,4.821428571,7.24478856649));
#157142=CARTESIAN_POINT('Ctrl Pts',(0.61188603345,4.884501699,7.23282953454999));
#157143=CARTESIAN_POINT('Ctrl Pts',(0.9977337452,4.948754474,7.17920615693));
#157144=CARTESIAN_POINT('Ctrl Pts',(0.203913492723773,4.81811592995213,
7.24713607501221));
#157145=CARTESIAN_POINT('Ctrl Pts',(0.207848573361887,4.81875342547607,
7.24702107600611));
#157146=CARTESIAN_POINT('Ctrl Pts',(0.211783654,4.819390921,7.246906077));
#157147=CARTESIAN_POINT('Ctrl Pts',(0.218073815,4.820409947,7.246722253));
#157148=CARTESIAN_POINT('Ctrl Pts',(0.224363648,4.821428571,7.24652751));
#157149=CARTESIAN_POINT('Ctrl Pts',(0.613829558,4.884501699,7.234469046));
#157150=CARTESIAN_POINT('Ctrl Pts',(0.999759534,4.948754474,7.180736792));
#157151=CARTESIAN_POINT('Ctrl Pts',(0.388428615635301,4.81811592995213,
7.42155191714905));
#157152=CARTESIAN_POINT('Ctrl Pts',(0.39245829531765,4.81875342547607,7.42133662307452));
#157153=CARTESIAN_POINT('Ctrl Pts',(0.396487975,4.819390921,7.421121329));
#157154=CARTESIAN_POINT('Ctrl Pts',(0.402929351,4.820409947,7.420777185));
#157155=CARTESIAN_POINT('Ctrl Pts',(0.40937012,4.821428571,7.420421861));
#157156=CARTESIAN_POINT('Ctrl Pts',(0.808182013,4.884501699,7.398420191));
#157157=CARTESIAN_POINT('Ctrl Pts',(1.202338414,4.948754474,7.333800299));
#157158=CARTESIAN_POINT('Origin',(-0.0491212403127217,5.08885412658079,
-0.18459499834712));
#157159=CARTESIAN_POINT('Ctrl Pts',(-0.576653346,4.948733649,7.227030574));
#157160=CARTESIAN_POINT('Ctrl Pts',(-0.182976184,4.884619049,7.258442542));
#157161=CARTESIAN_POINT('Ctrl Pts',(0.211783654,4.819390921,7.246906077));
#157162=CARTESIAN_POINT('Ctrl Pts',(0.215742295038516,4.81873681508671,
7.24679038963925));
#157163=CARTESIAN_POINT('Ctrl Pts',(0.219700936077032,4.81808270917342,
7.24667470227851));
#157164=CARTESIAN_POINT('Ctrl Pts',(-0.769900980000001,4.948733649,7.391718134));
#157165=CARTESIAN_POINT('Ctrl Pts',(-0.367252812,4.884619049,7.433656857));
#157166=CARTESIAN_POINT('Ctrl Pts',(0.037568402,4.819390921,7.431610398));
#157167=CARTESIAN_POINT('Ctrl Pts',(0.0416279382464466,4.81873681508671,
7.43158987616418));
#157168=CARTESIAN_POINT('Ctrl Pts',(0.0456874744928932,4.81808270917342,
7.43156935432838));
#157169=CARTESIAN_POINT('Origin',(-0.0259541685259539,4.69654854547677,
-0.190718431943377));
#157170=CARTESIAN_POINT('Ctrl Pts',(0.206665513,0.940053947,7.24705384000001));
#157171=CARTESIAN_POINT('Ctrl Pts',(0.604521557,1.005711878,7.235708109));
#157172=CARTESIAN_POINT('Ctrl Pts',(0.998744615,1.070155008,7.180878024));
#157173=CARTESIAN_POINT('Ctrl Pts',(0.459542598,0.940053947,7.485908135));
#157174=CARTESIAN_POINT('Ctrl Pts',(0.870511505,1.005711878,7.46067970300001));
#157175=CARTESIAN_POINT('Ctrl Pts',(1.276248909,1.070155008,7.390614908));
#157176=CARTESIAN_POINT('',(0.459542605383732,0.940053946884193,7.48590813582171));
#157177=CARTESIAN_POINT('',(1.0261937944465,1.03040248140644,7.42946339183112));
#157178=CARTESIAN_POINT('Origin',(0.0103931857568756,0.803673959797629,
-0.186267928095857));
#157179=CARTESIAN_POINT('Ctrl Pts',(0.994070540727961,1.06939092128209,
7.18152656204117));
#157180=CARTESIAN_POINT('Ctrl Pts',(0.999368724668876,1.06258635416255,
7.22279958838759));
#157181=CARTESIAN_POINT('Ctrl Pts',(1.0046992679533,1.05593965772069,7.26411847661544));
#157182=CARTESIAN_POINT('Ctrl Pts',(1.01540706332824,1.04295320028424,7.34675130349826));
#157183=CARTESIAN_POINT('Ctrl Pts',(1.02079005965345,1.03660648770934,7.38810953196721));
#157184=CARTESIAN_POINT('Ctrl Pts',(1.02619379318487,1.03040248141801,7.42946339193619));
#157185=CARTESIAN_POINT('',(0.333104057544598,0.940053946665902,7.36648098740755));
#157186=CARTESIAN_POINT('Origin',(1.29020058525775E-14,1.03148891300017,
-5.85469173142172E-14));
#157187=CARTESIAN_POINT('',(1.02255389523182,0.849330499810774,7.42996524430959));
#157188=CARTESIAN_POINT('Origin',(-0.0107703989177524,0.946426667970798,
-0.19229223055656));
#157189=CARTESIAN_POINT('',(1.58082723656417,0.940053948012009,7.33150634364829));
#157190=CARTESIAN_POINT('Origin',(-0.018799123902504,0.803583936067687,
-0.190543498808742));
#157191=CARTESIAN_POINT('Origin',(-0.0396491737200962,0.946429284259858,
-0.188708477980701));
#157192=CARTESIAN_POINT('Ctrl Pts',(0.989441248,1.070162746,7.182165831));
#157193=CARTESIAN_POINT('Ctrl Pts',(1.37862488,1.005280647,7.12855048));
#157194=CARTESIAN_POINT('Ctrl Pts',(1.759736143,0.940053947,7.033194773));
#157195=CARTESIAN_POINT('Ctrl Pts',(1.77283532249515,0.937812039362714,
7.02991730092518));
#157196=CARTESIAN_POINT('Ctrl Pts',(1.78593450199029,0.935570131725414,
7.02663982885036));
#157197=CARTESIAN_POINT('Ctrl Pts',(0.778916875456521,1.070162746,7.45996317561611));
#157198=CARTESIAN_POINT('Ctrl Pts',(1.1831536518329,1.005280647,7.41775561500099));
#157199=CARTESIAN_POINT('Ctrl Pts',(1.58046261703313,0.940053947,7.3321142923038));
#157200=CARTESIAN_POINT('Ctrl Pts',(1.59411852793229,0.937812039362713,
7.32917071344081));
#157201=CARTESIAN_POINT('Ctrl Pts',(1.60777443883138,0.935570131725414,
7.32622713457786));
#157202=CARTESIAN_POINT('',(1.67028170264392,0.940053949937996,7.18235055439685));
#157203=CARTESIAN_POINT('Ctrl Pts',(1.759736143,0.940053947,7.03319477300001));
#157204=CARTESIAN_POINT('Ctrl Pts',(2.145851537,1.005711878,6.936587009));
#157205=CARTESIAN_POINT('Ctrl Pts',(2.519071031,1.070155008,6.798292516));
#157206=CARTESIAN_POINT('Ctrl Pts',(2.058047714,0.940053947,7.212103688));
#157207=CARTESIAN_POINT('Ctrl Pts',(2.45398503,1.005711878,7.099118916));
#157208=CARTESIAN_POINT('Ctrl Pts',(2.835174659,1.070155008,6.943470649));
#157209=CARTESIAN_POINT('',(2.05804772140884,0.940053946884192,7.21210368721667));
#157210=CARTESIAN_POINT('',(2.59931696986772,1.03040248142397,7.03516533471204));
#157211=CARTESIAN_POINT('Origin',(-0.0298918993812045,0.803673986466962,
-0.184147321042287));
#157212=CARTESIAN_POINT('Ctrl Pts',(2.51464564999319,1.06939092119121,6.79993067959644));
#157213=CARTESIAN_POINT('Ctrl Pts',(2.52869245150643,1.06258635149592,6.83909982773586));
#157214=CARTESIAN_POINT('Ctrl Pts',(2.54278071547496,1.05593965239104,6.87830681115066));
#157215=CARTESIAN_POINT('Ctrl Pts',(2.57100176913631,1.0429532017803,6.95670582817617));
#157216=CARTESIAN_POINT('Ctrl Pts',(2.58514970700579,1.03660649073983,6.99593992918472));
#157217=CARTESIAN_POINT('Ctrl Pts',(2.59931696867331,1.03040248144127,7.03516533503894));
#157218=CARTESIAN_POINT('',(1.90889193047692,0.940053946665902,7.12264922997018));
#157219=CARTESIAN_POINT('Origin',(-6.26452015262124E-13,1.03148891300033,
-1.8253627775966E-12));
#157220=CARTESIAN_POINT('',(2.59587005224225,0.849330499783684,7.03643792502342));
#157221=CARTESIAN_POINT('Origin',(-0.0518557823053684,0.946426648330426,
-0.18548135075145));
#157222=CARTESIAN_POINT('',(3.11992552026395,0.940053948012017,6.82026867260148));
#157223=CARTESIAN_POINT('Origin',(-0.0593208284644847,0.803583927461065,
-0.182047421518711));
#157224=CARTESIAN_POINT('Origin',(-0.0792889380638379,0.946429283724577,
-0.175773157664761));
#157225=CARTESIAN_POINT('Ctrl Pts',(2.510262011,1.070162746,6.80155016400001));
#157226=CARTESIAN_POINT('Ctrl Pts',(2.878821031,1.005280647,6.665525334));
#157227=CARTESIAN_POINT('Ctrl Pts',(3.230523466,0.940053947,6.490471334));
#157228=CARTESIAN_POINT('Ctrl Pts',(3.24261183409407,0.937812039407971,
6.48445455112403));
#157229=CARTESIAN_POINT('Ctrl Pts',(3.2547002021882,0.935570131815929,6.47843776824816));
#157230=CARTESIAN_POINT('Ctrl Pts',(2.36437779987387,1.070162746,7.11810927904205));
#157231=CARTESIAN_POINT('Ctrl Pts',(2.75009036708949,1.005280647,6.98998954958823));
#157232=CARTESIAN_POINT('Ctrl Pts',(3.11970011633105,0.940053947,6.82094079016248));
#157233=CARTESIAN_POINT('Ctrl Pts',(3.13240397691135,0.937812039407971,
6.81513041347349));
#157234=CARTESIAN_POINT('Ctrl Pts',(3.14510783749165,0.935570131815929,
6.80932003678452));
#157235=CARTESIAN_POINT('',(3.17522450484935,0.940053949937996,6.65536999669985));
#157236=CARTESIAN_POINT('Ctrl Pts',(3.230523466,0.940053947,6.49047133400001));
#157237=CARTESIAN_POINT('Ctrl Pts',(3.586843883,1.005711878,6.31311881000001));
#157238=CARTESIAN_POINT('Ctrl Pts',(3.921608485,1.070155008,6.097826407));
#157239=CARTESIAN_POINT('Ctrl Pts',(3.560320807,0.940053947,6.601069288));
#157240=CARTESIAN_POINT('Ctrl Pts',(3.922712942,1.005711878,6.405611219));
#157241=CARTESIAN_POINT('Ctrl Pts',(4.261530793,1.070155008,6.171657419));
#157242=CARTESIAN_POINT('',(3.56032081408952,0.940053946884188,6.60106928563899));
#157243=CARTESIAN_POINT('',(4.05089897255837,1.03040248143616,6.31191076539481));
#157244=CARTESIAN_POINT('Origin',(-0.0687791674829624,0.80367396202427,
-0.173416020060584));
#157245=CARTESIAN_POINT('Ctrl Pts',(3.9176387235532,1.06939092116972,6.10037759740578));
#157246=CARTESIAN_POINT('Ctrl Pts',(3.93977731881556,1.06258635418866,6.13561133127413));
#157247=CARTESIAN_POINT('Ctrl Pts',(3.96196453935034,1.0559396579215,6.17087310068767));
#157248=CARTESIAN_POINT('Ctrl Pts',(4.00637928790532,1.04295320259416,6.24137252538175));
#157249=CARTESIAN_POINT('Ctrl Pts',(4.02863062364503,1.03660649242267,6.2766479612956));
#157250=CARTESIAN_POINT('Ctrl Pts',(4.05089897146474,1.03040248145668,6.31191076594333));
#157251=CARTESIAN_POINT('',(3.39542213831681,0.940053946665902,6.54577031005759));
#157252=CARTESIAN_POINT('Origin',(-3.6949610038306E-13,1.03148891300017,
-5.41667405373758E-13));
#157253=CARTESIAN_POINT('',(4.04780621136812,0.849330499792421,6.31389458847702));
#157254=CARTESIAN_POINT('Origin',(-0.0905162729480125,0.946426679995198,
-0.169997196421141));
#157255=CARTESIAN_POINT('',(4.51313955453792,0.940053948012019,5.99012281865662));
#157256=CARTESIAN_POINT('Origin',(-0.0970687103584039,0.803583922662045,
-0.165038982853876));
#157257=CARTESIAN_POINT('Origin',(-0.1152210911026,0.946429287942322,-0.154618692676783));
#157258=CARTESIAN_POINT('Ctrl Pts',(3.913705713,1.070162746,6.102901571));
#157259=CARTESIAN_POINT('Ctrl Pts',(4.24440671,1.005280647,5.890827631));
#157260=CARTESIAN_POINT('Ctrl Pts',(4.550255102,0.940053947,5.644260669));
#157261=CARTESIAN_POINT('Ctrl Pts',(4.56076742050196,0.937812039364825,
5.63578591319158));
#157262=CARTESIAN_POINT('Ctrl Pts',(4.5712797390039,0.935570131729636,5.62731115738306));
#157263=CARTESIAN_POINT('Ctrl Pts',(3.83928304573905,1.070162746,6.44342050299382));
#157264=CARTESIAN_POINT('Ctrl Pts',(4.18843591351092,1.005280647,6.23537934193769));
#157265=CARTESIAN_POINT('Ctrl Pts',(4.51306390582548,0.940053947,5.99082767768925));
#157266=CARTESIAN_POINT('Ctrl Pts',(4.52422169817986,0.937812039364825,
5.98242218970237));
#157267=CARTESIAN_POINT('Ctrl Pts',(4.53537949053428,0.935570131729636,
5.97401670171551));
#157268=CARTESIAN_POINT('',(4.53169733829032,0.940053949937996,5.81719173486759));
#157269=CARTESIAN_POINT('Ctrl Pts',(4.550255102,0.940053947,5.644260669));
#157270=CARTESIAN_POINT('Ctrl Pts',(4.860119396,1.005711878,5.394456192));
#157271=CARTESIAN_POINT('Ctrl Pts',(5.14077588500001,1.070155008,5.112232712));
#157272=CARTESIAN_POINT('Ctrl Pts',(4.896117256,0.940053947,5.681376225));
#157273=CARTESIAN_POINT('Ctrl Pts',(5.208019157,1.005711878,5.41258426));
#157274=CARTESIAN_POINT('Ctrl Pts',(5.488622484,1.070155008,5.11126434800001));
#157275=CARTESIAN_POINT('',(4.89611726241347,0.94005394688418,5.68137622117121));
#157276=CARTESIAN_POINT('',(5.31306544163784,1.03040248139847,5.29351826402951));
#157277=CARTESIAN_POINT('Origin',(-0.104450594516354,0.803673959972207,
-0.154576303251013));
#157278=CARTESIAN_POINT('Ctrl Pts',(5.13744736507667,1.0693909212065,5.11557763819519));
#157279=CARTESIAN_POINT('Ctrl Pts',(5.16664259530524,1.06258635144726,5.14522849550555));
#157280=CARTESIAN_POINT('Ctrl Pts',(5.19589134248179,1.05593965230488,5.17489628147042));
#157281=CARTESIAN_POINT('Ctrl Pts',(5.25442297546138,1.04295320044881,5.23419959482863));
#157282=CARTESIAN_POINT('Ctrl Pts',(5.2837372741119,1.03660648808713,5.26386694208382));
#157283=CARTESIAN_POINT('Ctrl Pts',(5.31306544069633,1.03040248141083,5.2935182648699));
#157284=CARTESIAN_POINT('',(4.72318618057174,0.940053946665902,5.66281844568906));
#157285=CARTESIAN_POINT('Origin',(-1.31101726696947E-12,1.03148891300044,
-1.34310965127504E-12));
#157286=CARTESIAN_POINT('',(5.31047145089205,0.849330499771562,5.29612055861479));
#157287=CARTESIAN_POINT('Origin',(-0.124944554379689,0.946426703525078,
-0.14656457946748));
#157288=CARTESIAN_POINT('',(5.69532420086373,0.940053948010709,4.87988547605802));
#157289=CARTESIAN_POINT('Origin',(-0.130277934429539,0.803583951405237,
-0.140313671440268));
#157290=CARTESIAN_POINT('Origin',(-0.14576573591514,0.946429263697512,-0.12623466299575));
#157291=CARTESIAN_POINT('Ctrl Pts',(5.13414888600001,1.070162746,5.118888084));
#157292=CARTESIAN_POINT('Ctrl Pts',(5.411528649,1.005280647,4.840681376));
#157293=CARTESIAN_POINT('Ctrl Pts',(5.657221867,0.940053947,4.534130649));
#157294=CARTESIAN_POINT('Ctrl Pts',(5.66566659185461,0.937812039229164,
4.52359418989632));
#157295=CARTESIAN_POINT('Ctrl Pts',(5.6741113167094,0.935570131458313,4.51305773079268));
#157296=CARTESIAN_POINT('Ctrl Pts',(5.13466768313965,1.070162746,5.46744454586968));
#157297=CARTESIAN_POINT('Ctrl Pts',(5.4309348517102,1.005280647,5.1892097256946));
#157298=CARTESIAN_POINT('Ctrl Pts',(5.69540184317356,0.940053947,4.88059012097109));
#157299=CARTESIAN_POINT('Ctrl Pts',(5.70449184164491,0.937812039229164,
4.86998255244376));
#157300=CARTESIAN_POINT('Ctrl Pts',(5.71358184011627,0.935570131458314,
4.85937498391645));
#157301=CARTESIAN_POINT('',(5.67627304106311,0.940053949938004,4.70700805305583));
#157302=CARTESIAN_POINT('Ctrl Pts',(5.657221867,0.940053947,4.534130649));
#157303=CARTESIAN_POINT('Ctrl Pts',(5.906141128,1.005711878,4.223554798));
#157304=CARTESIAN_POINT('Ctrl Pts',(6.119566318,1.070155008,3.887596697));
#157305=CARTESIAN_POINT('Ctrl Pts',(6.002976704,0.940053947,4.496028325));
#157306=CARTESIAN_POINT('Ctrl Pts',(6.249804185,1.005711878,4.166470877));
#157307=CARTESIAN_POINT('Ctrl Pts',(6.459072287,1.070155008,3.811874236));
#157308=CARTESIAN_POINT('',(6.00297670939691,0.9400539468842,4.49602831991059));
#157309=CARTESIAN_POINT('',(6.3267988756447,1.03040248135818,4.02760673190842));
#157310=CARTESIAN_POINT('Origin',(-0.135237854469713,0.803673991008168,
-0.128508530935612));
#157311=CARTESIAN_POINT('Ctrl Pts',(6.11703467735814,1.06939092122838,3.89157895396036));
#157312=CARTESIAN_POINT('Ctrl Pts',(6.15192139724256,1.06258635146732,3.91426047917283));
#157313=CARTESIAN_POINT('Ctrl Pts',(6.18686402201107,1.05593965231519,3.9369470327545));
#157314=CARTESIAN_POINT('Ctrl Pts',(6.25677568131884,1.04295319969706,3.98228129938604));
#157315=CARTESIAN_POINT('Ctrl Pts',(6.29178223507313,1.03660648657069,4.00495333581444));
#157316=CARTESIAN_POINT('Ctrl Pts',(6.3267988749145,1.03040248136766,4.02760673295417));
#157317=CARTESIAN_POINT('',(5.83009928675315,0.940053946665909,4.51507948538187));
#157318=CARTESIAN_POINT('Origin',(4.10695782937509E-13,1.03148891299983,
2.1467203015213E-13));
#157319=CARTESIAN_POINT('',(6.32482494729382,0.849330499764723,4.03070581740142));
#157320=CARTESIAN_POINT('Origin',(-0.153530836941408,0.946426677340838,
-0.116278825077462));
#157321=CARTESIAN_POINT('',(6.61120181473465,0.940053948010707,3.54147011535873));
#157322=CARTESIAN_POINT('Origin',(-0.157395227955885,0.803583957882191,
-0.109027212856986));
#157323=CARTESIAN_POINT('Origin',(-0.169494640360354,0.946429293361835,
-0.0919481097987146));
#157324=CARTESIAN_POINT('Ctrl Pts',(6.114524963,1.070162746,3.895521079));
#157325=CARTESIAN_POINT('Ctrl Pts',(6.32561352300001,1.005280647,3.564190239));
#157326=CARTESIAN_POINT('Ctrl Pts',(6.499663225,0.940053947,3.211989719));
#157327=CARTESIAN_POINT('Ctrl Pts',(6.50564548947943,0.937812039280326,
3.19988423053191));
#157328=CARTESIAN_POINT('Ctrl Pts',(6.51162775395894,0.93557013156064,3.18777874206383));
#157329=CARTESIAN_POINT('Ctrl Pts',(6.1899609672,1.070162746,4.2358169583214));
#157330=CARTESIAN_POINT('Ctrl Pts',(6.41948931138866,1.005280647,3.90039843070349));
#157331=CARTESIAN_POINT('Ctrl Pts',(6.61142911963172,0.940053947,3.54214159525235));
#157332=CARTESIAN_POINT('Ctrl Pts',(6.6180262851761,0.937812039280326,3.52982794509029));
#157333=CARTESIAN_POINT('Ctrl Pts',(6.62462345072036,0.93557013156064,3.5175142949283));
#157334=CARTESIAN_POINT('',(6.55543252479518,0.940053949938004,3.37672990639611));
#157335=CARTESIAN_POINT('Ctrl Pts',(6.499663225,0.940053947,3.211989719));
#157336=CARTESIAN_POINT('Ctrl Pts',(6.675998265,1.005711878,2.855164676));
#157337=CARTESIAN_POINT('Ctrl Pts',(6.812212632,1.070155008,2.481180981));
#157338=CARTESIAN_POINT('Ctrl Pts',(6.829143632,0.940053947,3.100451136));
#157339=CARTESIAN_POINT('Ctrl Pts',(6.999355314,1.005711878,2.725537947));
#157340=CARTESIAN_POINT('Ctrl Pts',(7.127503049,1.070155008,2.334245122));
#157341=CARTESIAN_POINT('',(6.82914363621652,0.940053946884184,3.10045112982859));
#157342=CARTESIAN_POINT('',(7.04469822610831,1.03040248142797,2.5733687845793));
#157343=CARTESIAN_POINT('Origin',(-0.159701616024189,0.803673941611579,
-0.0964319565452881));
#157344=CARTESIAN_POINT('Ctrl Pts',(6.81059624699143,1.06939092111156,2.48561436359438));
#157345=CARTESIAN_POINT('Ctrl Pts',(6.84954319235847,1.06258635136358,2.5002659938163));
#157346=CARTESIAN_POINT('Ctrl Pts',(6.88854581641247,1.05593965223858,2.51491051690288));
#157347=CARTESIAN_POINT('Ctrl Pts',(6.96656848502177,1.04295320336159,2.54415594493735));
#157348=CARTESIAN_POINT('Ctrl Pts',(7.00563039808937,1.03660649398555,2.55877253825662));
#157349=CARTESIAN_POINT('Ctrl Pts',(7.04469822533426,1.03040248145228,2.57336878626287));
#157350=CARTESIAN_POINT('',(6.664403429376,0.940053946665909,3.15622042565031));
#157351=CARTESIAN_POINT('Origin',(1.58206781009085E-12,1.03148891299961,
5.70507183161872E-13));
#157352=CARTESIAN_POINT('',(7.04343665848193,0.849330499775803,2.57681975219681));
#157353=CARTESIAN_POINT('Origin',(-0.174937395364666,0.946426703968627,
-0.080555512952542));
#157354=CARTESIAN_POINT('',(7.217946980252,0.940053948011585,2.0374595491609));
#157355=CARTESIAN_POINT('Origin',(-0.177153273325414,0.803583973570313,
-0.0726429733030526));
#157356=CARTESIAN_POINT('Origin',(-0.185298049236705,0.946429317162114,
-0.0533620738118479));
#157357=CARTESIAN_POINT('Ctrl Pts',(6.80899264800001,1.070162746,2.490003838));
#157358=CARTESIAN_POINT('Ctrl Pts',(6.943919739,1.005280647,2.121041529));
#157359=CARTESIAN_POINT('Ctrl Pts',(7.038187555,0.940053947,1.73965972));
#157360=CARTESIAN_POINT('Ctrl Pts',(7.04142763503705,0.937812039448509,
1.7265512420669));
#157361=CARTESIAN_POINT('Ctrl Pts',(7.0446677150741,0.935570131897005,1.7134427641338));
#157362=CARTESIAN_POINT('Ctrl Pts',(6.95581855636277,1.070162746,2.80612727794603));
#157363=CARTESIAN_POINT('Ctrl Pts',(7.10787558656333,1.005280647,2.42920883961683));
#157364=CARTESIAN_POINT('Ctrl Pts',(7.21831331925159,0.940053947,2.03806646438908));
#157365=CARTESIAN_POINT('Ctrl Pts',(7.22210917565524,0.937812039448509,
2.02462250593755));
#157366=CARTESIAN_POINT('Ctrl Pts',(7.22590503205889,0.935570131897005,
2.01117854748595));
#157367=CARTESIAN_POINT('',(7.12806727013939,0.940053949938004,1.88855962198939));
#157368=CARTESIAN_POINT('Ctrl Pts',(7.038187555,0.940053947,1.73965972));
#157369=CARTESIAN_POINT('Ctrl Pts',(7.133693143,1.005711878,1.353270226));
#157370=CARTESIAN_POINT('Ctrl Pts',(7.186327454,1.070155008,0.958748));
#157371=CARTESIAN_POINT('Ctrl Pts',(7.335987395,0.940053947,1.559900299));
#157372=CARTESIAN_POINT('Ctrl Pts',(7.421624369,1.005711878,1.157161891));
#157373=CARTESIAN_POINT('Ctrl Pts',(7.46265969,1.070155008,0.7474693));
#157374=CARTESIAN_POINT('',(7.33598739777246,0.940053946884192,1.55990029209667));
#157375=CARTESIAN_POINT('',(7.43319531680987,1.03040248137726,0.998802974411074));
#157376=CARTESIAN_POINT('Origin',(-0.176697923435072,0.803673966896485,
-0.0598462981616252));
#157377=CARTESIAN_POINT('Ctrl Pts',(7.18570190537006,1.06939092111547,0.963425207554627));
#157378=CARTESIAN_POINT('Ctrl Pts',(7.22688794226064,1.06258635431296,0.969361846302531));
#157379=CARTESIAN_POINT('Ctrl Pts',(7.26812682594864,1.05593965822805,0.975279574506992));
#157380=CARTESIAN_POINT('Ctrl Pts',(7.35061233071141,1.04295319985269,0.987068702007152));
#157381=CARTESIAN_POINT('Ctrl Pts',(7.39190315818797,1.03660648691664,0.992946414394434));
#157382=CARTESIAN_POINT('Ctrl Pts',(7.43319531658188,1.03040248138745,0.99880297566297));
#157383=CARTESIAN_POINT('',(7.1870874754579,0.940053946665909,1.64978000750524));
#157384=CARTESIAN_POINT('Origin',(2.90566182226115E-13,1.03148891300033,
-6.53773910008759E-14));
#157385=CARTESIAN_POINT('',(7.43270510019514,0.849330500339288,1.00244445928462));
#157386=CARTESIAN_POINT('Origin',(-0.188164822754386,0.946426684333019,
-0.0410658480806596));
#157387=CARTESIAN_POINT('',(7.48718896703835,0.940053948011584,0.438179637481235));
#157388=CARTESIAN_POINT('Origin',(-0.188627616963447,0.803583944653875,
-0.0328619031245316));
#157389=CARTESIAN_POINT('Origin',(-0.192437196061649,0.946429297142976,
-0.0122808963513313));
#157390=CARTESIAN_POINT('Ctrl Pts',(7.185079405,1.070162746,0.968056785));
#157391=CARTESIAN_POINT('Ctrl Pts',(7.23753598500001,1.005280647,0.578715273));
#157392=CARTESIAN_POINT('Ctrl Pts',(7.247614057,0.940053947,0.185985165));
#157393=CARTESIAN_POINT('Ctrl Pts',(7.24796045053153,0.937812039325257,
0.17248663382751));
#157394=CARTESIAN_POINT('Ctrl Pts',(7.24830684406306,0.935570131650501,
0.158988102655022));
#157395=CARTESIAN_POINT('Ctrl Pts',(7.39642979953016,1.070162746,1.24522620453934));
#157396=CARTESIAN_POINT('Ctrl Pts',(7.46390549870593,1.005280647,0.844432143122291));
#157397=CARTESIAN_POINT('Ctrl Pts',(7.48767721009522,0.940053947,0.438693611337785));
#157398=CARTESIAN_POINT('Ctrl Pts',(7.48849426786764,0.937812039325257,
0.424747967478025));
#157399=CARTESIAN_POINT('Ctrl Pts',(7.48931132564014,0.935570131650498,
0.41080232361826));
#157400=CARTESIAN_POINT('',(7.36740151176666,0.940053949938004,0.312082388401445));
#157401=CARTESIAN_POINT('Ctrl Pts',(7.24761405700001,0.940053947,0.185985165));
#157402=CARTESIAN_POINT('Ctrl Pts',(7.257824457,1.005711878,-0.211901635));
#157403=CARTESIAN_POINT('Ctrl Pts',(7.224417591,1.070155008,-0.608514971));
#157404=CARTESIAN_POINT('Ctrl Pts',(7.49980854000001,0.940053947,-0.053589743));
#157405=CARTESIAN_POINT('Ctrl Pts',(7.496866517,1.005711878,-0.465321769));
#157406=CARTESIAN_POINT('Ctrl Pts',(7.448870658,1.070155008,-0.874257356));
#157407=CARTESIAN_POINT('',(7.49980854123035,0.940053946884195,-0.05358975035691));
#157408=CARTESIAN_POINT('',(7.47412445611645,1.03040248135761,-0.62246575367252));
#157409=CARTESIAN_POINT('Origin',(-0.185431817958654,0.803673979949119,
-0.0204623074656415));
#157410=CARTESIAN_POINT('Ctrl Pts',(7.22481212868082,1.06939092120208,-0.603812640052707));
#157411=CARTESIAN_POINT('Ctrl Pts',(7.26631147867449,1.06258635144333,-0.606868578566119));
#157412=CARTESIAN_POINT('Ctrl Pts',(7.30785837722625,1.05593965229337,-0.609954346170825));
#157413=CARTESIAN_POINT('Ctrl Pts',(7.39094942006576,1.04295324244345,-0.616172764027325));
#157414=CARTESIAN_POINT('Ctrl Pts',(7.43253811868122,1.03660657331793,-0.619308753071964));
#157415=CARTESIAN_POINT('Ctrl Pts',(7.47412445621601,1.03040248136036,-0.62246575236655));
#157416=CARTESIAN_POINT('',(7.37371129851838,0.940053946665909,0.0661977089534413));
#157417=CARTESIAN_POINT('Origin',(-1.32099192695634E-12,1.03148891300011,
1.23267010748024E-13));
#157418=CARTESIAN_POINT('',(7.47442851198712,0.849330499786397,-0.618804022598348));
#157419=CARTESIAN_POINT('Origin',(-0.192593390699098,0.946426691613029,
0.000344107344360314));
#157420=CARTESIAN_POINT('',(7.40633831793416,0.940053948010714,-1.18158906852439));
#157421=CARTESIAN_POINT('Origin',(-0.191281893020457,0.803583929448492,
0.00845574576009325));
#157422=CARTESIAN_POINT('Origin',(-0.190578083564067,0.946429301495116,
0.02937453071876));
#157423=CARTESIAN_POINT('Ctrl Pts',(7.225199835,1.070162746,-0.599155527));
#157424=CARTESIAN_POINT('Ctrl Pts',(7.192733093,1.005280647,-0.990671065));
#157425=CARTESIAN_POINT('Ctrl Pts',(7.118150181,0.940053947,-1.376385849));
#157426=CARTESIAN_POINT('Ctrl Pts',(7.11558669079624,0.937812039276247,
-1.38964325667839));
#157427=CARTESIAN_POINT('Ctrl Pts',(7.11302320059262,0.935570131552479,
-1.40290066435676));
#157428=CARTESIAN_POINT('Ctrl Pts',(7.49119220641564,1.070162746,-0.373900262498168));
#157429=CARTESIAN_POINT('Ctrl Pts',(7.47093148525627,1.005280647,-0.779829261873931));
#157430=CARTESIAN_POINT('Ctrl Pts',(7.40692563609068,0.940053947,-1.18119206712137));
#157431=CARTESIAN_POINT('Ctrl Pts',(7.40472569024625,0.937812039276248,
-1.19498731313431));
#157432=CARTESIAN_POINT('Ctrl Pts',(7.40252574440196,0.935570131552477,
-1.20878255914725));
#157433=CARTESIAN_POINT('',(7.26224424685807,0.940053949938004,-1.27898747034023));
#157434=CARTESIAN_POINT('Ctrl Pts',(7.118150181,0.940053947,-1.376385849));
#157435=CARTESIAN_POINT('Ctrl Pts',(7.042587967,1.005711878,-1.767165211));
#157436=CARTESIAN_POINT('Ctrl Pts',(6.924701991,1.070155008,-2.147324459));
#157437=CARTESIAN_POINT('Ctrl Pts',(7.312946974,0.940053947,-1.664573988));
#157438=CARTESIAN_POINT('Ctrl Pts',(7.221563518,1.005711878,-2.0660475));
#157439=CARTESIAN_POINT('Ctrl Pts',(7.086780713,1.070155008,-2.455104709));
#157440=CARTESIAN_POINT('',(7.31294697361584,0.940053946884197,-1.66457399541545));
#157441=CARTESIAN_POINT('',(7.16557184278519,1.03040248136924,-2.21462867485676));
#157442=CARTESIAN_POINT('Origin',(-0.185495574279347,0.803673981046612,
0.0198785268233517));
#157443=CARTESIAN_POINT('Ctrl Pts',(6.92609816677978,1.06939092119062,-2.14281687978802));
#157444=CARTESIAN_POINT('Ctrl Pts',(6.96597033263714,1.06258635417184,-2.15472250079013));
#157445=CARTESIAN_POINT('Ctrl Pts',(7.00588252084771,1.05593965785563,-2.16666747443939));
#157446=CARTESIAN_POINT('Ctrl Pts',(7.08569446013349,1.04295320004583,-2.19060271567495));
#157447=CARTESIAN_POINT('Ctrl Pts',(7.12563698639577,1.03660648728853,-2.20260581656275));
#157448=CARTESIAN_POINT('Ctrl Pts',(7.16557184309803,1.03040248138017,-2.21462867362724));
#157449=CARTESIAN_POINT('',(7.215548577078,0.940053946665909,-1.52047992050266));
#157450=CARTESIAN_POINT('Origin',(-6.3274038786254E-13,1.03148891299978,
1.57968256531138E-13));
#157451=CARTESIAN_POINT('',(7.16665595397576,0.849330499759727,-2.21111791586516));
#157452=CARTESIAN_POINT('Origin',(-0.188016845225611,0.946426674270018,
0.0417380006194687));
#157453=CARTESIAN_POINT('',(6.9791755234254,0.940053948011584,-2.74610798041312));
#157454=CARTESIAN_POINT('Origin',(-0.18499204033991,0.803583928938046,0.0493779806989719));
#157455=CARTESIAN_POINT('Origin',(-0.179807836070603,0.946429282548676,
0.0696564257744658));
#157456=CARTESIAN_POINT('Ctrl Pts',(6.92747795,1.070162746,-2.138351993));
#157457=CARTESIAN_POINT('Ctrl Pts',(6.811605995,1.005280647,-2.513734725));
#157458=CARTESIAN_POINT('Ctrl Pts',(6.655849513,0.940053947,-2.874398591));
#157459=CARTESIAN_POINT('Ctrl Pts',(6.6504960051112,0.937812039321254,-2.88679497301278));
#157460=CARTESIAN_POINT('Ctrl Pts',(6.64514249722251,0.935570131642496,
-2.8991913550255));
#157461=CARTESIAN_POINT('Ctrl Pts',(7.23567479171325,1.070162746,-1.97554356806818));
#157462=CARTESIAN_POINT('Ctrl Pts',(7.12862501943956,1.005280647,-2.36762671770142));
#157463=CARTESIAN_POINT('Ctrl Pts',(6.97983445285341,0.940053947,-2.74584651830165));
#157464=CARTESIAN_POINT('Ctrl Pts',(6.97472037052588,0.937812039321253,
-2.75884631555064));
#157465=CARTESIAN_POINT('Ctrl Pts',(6.9696062881982,0.935570131642497,-2.77184611279955));
#157466=CARTESIAN_POINT('',(6.81751251259641,0.940053949938004,-2.81025329724772));
#157467=CARTESIAN_POINT('Ctrl Pts',(6.655849513,0.940053947,-2.874398591));
#157468=CARTESIAN_POINT('Ctrl Pts',(6.49804789100001,1.005711878,-3.239798106));
#157469=CARTESIAN_POINT('Ctrl Pts',(6.301195022,1.070155008,-3.585727442));
#157470=CARTESIAN_POINT('Ctrl Pts',(6.784140134,0.940053947,-3.197724603));
#157471=CARTESIAN_POINT('Ctrl Pts',(6.608588236,1.005711878,-3.570167146));
#157472=CARTESIAN_POINT('Ctrl Pts',(6.393320778,1.070155008,-3.921154095));
#157473=CARTESIAN_POINT('',(6.78414013202652,0.940053946884191,-3.19772461020444));
#157474=CARTESIAN_POINT('',(6.52196505392216,1.03040248138268,-3.70323802043655));
#157475=CARTESIAN_POINT('Origin',(-0.176885230900306,0.803673982213261,
0.0592896936848697));
#157476=CARTESIAN_POINT('Ctrl Pts',(6.30352755236845,1.06939092115757,-3.58162538384938));
#157477=CARTESIAN_POINT('Ctrl Pts',(6.33990818722998,1.06258635142359,-3.60182400325982));
#157478=CARTESIAN_POINT('Ctrl Pts',(6.37631945100853,1.05593965229467,-3.62206965996145));
#157479=CARTESIAN_POINT('Ctrl Pts',(6.44911979335023,1.04295324246494,-3.66260236648865));
#157480=CARTESIAN_POINT('Ctrl Pts',(6.485547906345,1.03660657334913,-3.68291115436475));
#157481=CARTESIAN_POINT('Ctrl Pts',(6.52196505456613,1.03040248138544,-3.70323801928368));
#157482=CARTESIAN_POINT('',(6.71999482265735,0.940053946665909,-3.03606159886512));
#157483=CARTESIAN_POINT('Origin',(-1.33400235302616E-12,1.03148891300006,
7.94937032866372E-13));
#157484=CARTESIAN_POINT('',(6.5237785286103,0.849330499784263,-3.70004239307047));
#157485=CARTESIAN_POINT('Origin',(-0.174648438018141,0.946426696792022,
0.0811801132268097));
#157486=CARTESIAN_POINT('',(6.22567423713443,0.940053948012022,-4.18222193475387));
#157487=CARTESIAN_POINT('Origin',(-0.170052142850048,0.803583965490886,
0.0879913438511026));
#157488=CARTESIAN_POINT('Origin',(-0.160630037195878,0.946429248627739,
0.106681332694981));
#157489=CARTESIAN_POINT('Ctrl Pts',(6.305834896,1.070162746,-3.577561496));
#157490=CARTESIAN_POINT('Ctrl Pts',(6.111975772,1.005280647,-3.919258944));
#157491=CARTESIAN_POINT('Ctrl Pts',(5.88232872,0.940053947,-4.238007649));
#157492=CARTESIAN_POINT('Ctrl Pts',(5.87443551850391,0.937812039335438,
-4.24896336444796));
#157493=CARTESIAN_POINT('Ctrl Pts',(5.86654231700796,0.935570131670863,
-4.25991907989585));
#157494=CARTESIAN_POINT('Ctrl Pts',(6.64182526572518,1.070162746,-3.4848126526049));
#157495=CARTESIAN_POINT('Ctrl Pts',(6.4529919693508,1.005280647,-3.84471657929409));
#157496=CARTESIAN_POINT('Ctrl Pts',(6.22637396689046,0.940053947,-4.18210823669196));
#157497=CARTESIAN_POINT('Ctrl Pts',(6.21858487689136,0.937812039335437,
-4.19370472927367));
#157498=CARTESIAN_POINT('Ctrl Pts',(6.21079578689226,0.935570131670863,
-4.20530122185541));
#157499=CARTESIAN_POINT('',(6.05400147015755,0.940053949938004,-4.21011480237209));
#157500=CARTESIAN_POINT('Ctrl Pts',(5.88232872,0.940053947,-4.238007649));
#157501=CARTESIAN_POINT('Ctrl Pts',(5.649666317,1.005711878,-4.560941642));
#157502=CARTESIAN_POINT('Ctrl Pts',(5.383051178,1.070155008,-4.856465795));
#157503=CARTESIAN_POINT('Ctrl Pts',(5.938114442,0.940053947,-4.58135317));
#157504=CARTESIAN_POINT('Ctrl Pts',(5.686602712,1.005711878,-4.907349744));
#157505=CARTESIAN_POINT('Ctrl Pts',(5.400916269,1.070155008,-5.203854673));
#157506=CARTESIAN_POINT('',(5.93811443852413,0.940053946884183,-4.58135317661113));
#157507=CARTESIAN_POINT('',(5.57339842761695,1.03040248139026,-5.01868807215372));
#157508=CARTESIAN_POINT('Origin',(-0.160004360491645,0.80367397061341,0.095928749465683));
#157509=CARTESIAN_POINT('Ctrl Pts',(5.38621099635172,1.0693909211544,-4.85296106572622));
#157510=CARTESIAN_POINT('Ctrl Pts',(5.4173989531335,1.06258635419649,-4.88050820243491));
#157511=CARTESIAN_POINT('Ctrl Pts',(5.44860670944017,1.05593965794799,-4.90810785948304));
#157512=CARTESIAN_POINT('Ctrl Pts',(5.51099190624788,1.0429532023085,-4.96334305032409));
#157513=CARTESIAN_POINT('Ctrl Pts',(5.54220277780223,1.03660649187402,-4.99100819024458));
#157514=CARTESIAN_POINT('Ctrl Pts',(5.57339842834238,1.03040248140988,-5.01868807116424));
#157515=CARTESIAN_POINT('',(5.91022157977611,0.940053946665909,-4.40968041114037));
#157516=CARTESIAN_POINT('Origin',(-5.79831321845248E-13,1.03148891300033,
5.99346960949987E-13));
#157517=CARTESIAN_POINT('',(5.57585647005732,0.849330499761024,-5.01595699988355));
#157518=CARTESIAN_POINT('Origin',(-0.153113955485447,0.94642670548866,0.116826443368859));
#157519=CARTESIAN_POINT('',(5.18106734053611,0.940053948010703,-5.42277984334141));
#157520=CARTESIAN_POINT('Origin',(-0.147161145078586,0.803583943981683,
0.122490578603415));
#157521=CARTESIAN_POINT('Origin',(-0.13394123761439,0.946429246866666,0.138717858777231));
#157522=CARTESIAN_POINT('Ctrl Pts',(5.389338011,1.070162746,-4.8494882));
#157523=CARTESIAN_POINT('Ctrl Pts',(5.12655635500001,1.005280647,-5.14152297));
#157524=CARTESIAN_POINT('Ctrl Pts',(4.833756773,0.940053947,-5.403452179));
#157525=CARTESIAN_POINT('Ctrl Pts',(4.82369295517009,0.937812039337555,
-5.41245495088139));
#157526=CARTESIAN_POINT('Ctrl Pts',(4.81362913734007,0.935570131675098,
-5.4214577227628));
#157527=CARTESIAN_POINT('Ctrl Pts',(5.73741137229587,1.070162746,-4.83113577047591));
#157528=CARTESIAN_POINT('Ctrl Pts',(5.47562418787128,1.005280647,-5.14203176680072));
#157529=CARTESIAN_POINT('Ctrl Pts',(5.18177515547889,0.940053947,-5.42281922306667));
#157530=CARTESIAN_POINT('Ctrl Pts',(5.17167526697736,0.937812039337554,
-5.43247017198359));
#157531=CARTESIAN_POINT('Ctrl Pts',(5.16157537847578,0.9355701316751,-5.44212112090062));
#157532=CARTESIAN_POINT('',(5.00741204770229,0.940053949938004,-5.41311601880107));
#157533=CARTESIAN_POINT('Ctrl Pts',(4.833756773,0.940053947,-5.403452179));
#157534=CARTESIAN_POINT('Ctrl Pts',(4.537112626,1.005711878,-5.668820616));
#157535=CARTESIAN_POINT('Ctrl Pts',(4.213201843,1.070155008,-5.900121205));
#157536=CARTESIAN_POINT('Ctrl Pts',(4.814429119,0.940053947,-5.75076275500001));
#157537=CARTESIAN_POINT('Ctrl Pts',(4.498717966,1.005711878,-6.015070122));
#157538=CARTESIAN_POINT('Ctrl Pts',(4.155970918,1.070155008,-6.24322879));
#157539=CARTESIAN_POINT('',(4.81442911420674,0.940053946884196,-5.75076276067055));
#157540=CARTESIAN_POINT('',(4.36422588487778,1.0304024813986,-6.09946984755704));
#157541=CARTESIAN_POINT('Origin',(-0.135641776486256,0.803673954689217,
0.128082311223656));
#157542=CARTESIAN_POINT('Ctrl Pts',(4.21704119950274,1.06939092120473,-5.89737768206881));
#157543=CARTESIAN_POINT('Ctrl Pts',(4.24157817909531,1.06258635425499,-5.93098527065094));
#157544=CARTESIAN_POINT('Ctrl Pts',(4.26612320501677,1.05593965799867,-5.96464840807458));
#157545=CARTESIAN_POINT('Ctrl Pts',(4.3151759308655,1.04295320406734,-6.03200319497704));
#157546=CARTESIAN_POINT('Ctrl Pts',(4.33970991495528,1.03660649541051,-6.0657309438879));
#157547=CARTESIAN_POINT('Ctrl Pts',(4.3642258862629,1.03040248142576,-6.09946984635852));
#157548=CARTESIAN_POINT('',(4.82409294445209,0.940053946665909,-5.57710746833892));
#157549=CARTESIAN_POINT('Origin',(-2.55871712706579E-14,1.03148891300033,
5.63785129692462E-15));
#157550=CARTESIAN_POINT('',(4.36721355993799,0.849330499767501,-6.09733103257099));
#157551=CARTESIAN_POINT('Origin',(-0.124420020460023,0.946426691654718,
0.147010116000383));
#157552=CARTESIAN_POINT('',(3.89419949472767,0.940053948010701,-6.40977459130316));
#157553=CARTESIAN_POINT('Origin',(-0.117388650912164,0.803583922843219,
0.151261955103784));
#157554=CARTESIAN_POINT('Origin',(-0.100989597831267,0.946429327963876,
0.164268201422029));
#157555=CARTESIAN_POINT('Ctrl Pts',(4.22084167,1.070162746,-5.894658226));
#157556=CARTESIAN_POINT('Ctrl Pts',(3.90142486,1.005280647,-6.123375096));
#157557=CARTESIAN_POINT('Ctrl Pts',(3.559163733,0.940053947,-6.316237292));
#157558=CARTESIAN_POINT('Ctrl Pts',(3.54739987259014,0.93781203948184,-6.32286616034962));
#157559=CARTESIAN_POINT('Ctrl Pts',(3.53563601218029,0.935570131963667,
-6.32949502869939));
#157560=CARTESIAN_POINT('Ctrl Pts',(4.564722499399,1.070162746,-5.95156034962586));
#157561=CARTESIAN_POINT('Ctrl Pts',(4.24222230535363,1.005280647,-6.19891126289899));
#157562=CARTESIAN_POINT('Ctrl Pts',(3.89488229582533,0.940053947,-6.40996520962909));
#157563=CARTESIAN_POINT('Ctrl Pts',(3.88294386909641,0.93781203948184,-6.41721934681388));
#157564=CARTESIAN_POINT('Ctrl Pts',(3.8710054423675,0.93557013196367,-6.42447348399874));
#157565=CARTESIAN_POINT('',(3.72668160336882,0.940053949938004,-6.36300594715486));
#157566=CARTESIAN_POINT('Ctrl Pts',(3.559163733,0.940053947,-6.316237292));
#157567=CARTESIAN_POINT('Ctrl Pts',(3.212408591,1.005711878,-6.511631839));
#157568=CARTESIAN_POINT('Ctrl Pts',(2.846347872,1.070155008,-6.667893505));
#157569=CARTESIAN_POINT('Ctrl Pts',(3.465626441,0.940053947,-6.651273064));
#157570=CARTESIAN_POINT('Ctrl Pts',(3.100478168,1.005711878,-6.841532507));
#157571=CARTESIAN_POINT('Ctrl Pts',(2.716696986,1.070155008,-6.99067646800001));
#157572=CARTESIAN_POINT('',(3.46562643508481,0.940053946884187,-6.65127306852387));
#157573=CARTESIAN_POINT('',(2.95098699066175,1.03040248141321,-6.89504719174915));
#157574=CARTESIAN_POINT('Origin',(-0.104936565028214,0.803673979513478,
0.154246636087574));
#157575=CARTESIAN_POINT('Ctrl Pts',(2.85068724327674,1.06939092112309,-6.66603947209202));
#157576=CARTESIAN_POINT('Ctrl Pts',(2.86742593070085,1.06258635140717,-6.70413607482185));
#157577=CARTESIAN_POINT('Ctrl Pts',(2.88416053581012,1.05593965229657,-6.74228865949464));
#157578=CARTESIAN_POINT('Ctrl Pts',(2.91758713608327,1.04295320302106,-6.81861358783656));
#157579=CARTESIAN_POINT('Ctrl Pts',(2.9342970631903,1.03660649331213,-6.85682688896462));
#157580=CARTESIAN_POINT('Ctrl Pts',(2.95098699231288,1.03040248143631,-6.89504719088899));
#157581=CARTESIAN_POINT('',(3.51239508520041,0.940053946665902,-6.48375517897489));
#157582=CARTESIAN_POINT('Origin',(3.30464822173582E-13,1.03148891299967,
-9.38051719634458E-13));
#157583=CARTESIAN_POINT('',(2.95436459746952,0.84933049977548,-6.89360064298541));
#157584=CARTESIAN_POINT('Origin',(-0.0899083695330682,0.94642667139641,
0.170319820844224));
#157585=CARTESIAN_POINT('',(2.42524320939457,0.940053948010701,-7.09705540292411));
#157586=CARTESIAN_POINT('Origin',(-0.0821273225261276,0.803583927069448,
0.172960628750021));
#157587=CARTESIAN_POINT('Origin',(-0.0633156235864346,0.946429243334707,
0.182137290076859));
#157588=CARTESIAN_POINT('Ctrl Pts',(2.854983464,1.070162746,-6.664200584));
#157589=CARTESIAN_POINT('Ctrl Pts',(2.493867074,1.005280647,-6.818905009));
#157590=CARTESIAN_POINT('Ctrl Pts',(2.118148151,0.940053947,-6.933682168));
#157591=CARTESIAN_POINT('Ctrl Pts',(2.10523431145353,0.937812039322795,
-6.93762717508959));
#157592=CARTESIAN_POINT('Ctrl Pts',(2.09232047190712,0.935570131645578,
-6.94157218217907));
#157593=CARTESIAN_POINT('Ctrl Pts',(3.17859227582898,1.070162746,-6.79369658044958));
#157594=CARTESIAN_POINT('Ctrl Pts',(2.81045882138829,1.005280647,-6.96593655959706));
#157595=CARTESIAN_POINT('Ctrl Pts',(2.42586906972625,0.940053947,-7.09738834677674));
#157596=CARTESIAN_POINT('Ctrl Pts',(2.41265033082292,0.937812039322796,
-7.10190647770869));
#157597=CARTESIAN_POINT('Ctrl Pts',(2.39943159191954,0.935570131645576,
-7.10642460864078));
#157598=CARTESIAN_POINT('',(2.27169566876624,0.940053949938004,-7.01536878858059));
#157599=CARTESIAN_POINT('Ctrl Pts',(2.118148151,0.940053947,-6.933682168));
#157600=CARTESIAN_POINT('Ctrl Pts',(1.7374959,1.005711878,-7.049966394));
#157601=CARTESIAN_POINT('Ctrl Pts',(1.346401839,1.070155008,-7.123882515));
#157602=CARTESIAN_POINT('Ctrl Pts',(1.954774922,0.940053947,-7.240777238));
#157603=CARTESIAN_POINT('Ctrl Pts',(1.557263457,1.005711878,-7.348092436));
#157604=CARTESIAN_POINT('Ctrl Pts',(1.150393323,1.070155008,-7.411247884));
#157605=CARTESIAN_POINT('',(1.95477491526828,0.940053946884195,-7.24077724113414));
#157606=CARTESIAN_POINT('',(1.39976322578504,1.03040248139436,-7.36821979250953));
#157607=CARTESIAN_POINT('Origin',(-0.0693247149754145,0.80367397856932,
0.173198591715785));
#157608=CARTESIAN_POINT('Ctrl Pts',(1.35103831954935,1.06939092127104,-7.12300466507705));
#157609=CARTESIAN_POINT('Ctrl Pts',(1.35919602246169,1.06258635152761,-7.16380891331529));
#157610=CARTESIAN_POINT('Ctrl Pts',(1.36733770403458,1.05593965239,-7.20466695716615));
#157611=CARTESIAN_POINT('Ctrl Pts',(1.38357520950748,1.04295320012166,-7.28639320066194));
#157612=CARTESIAN_POINT('Ctrl Pts',(1.39167974182571,1.03660648740826,-7.32730525705295));
#157613=CARTESIAN_POINT('Ctrl Pts',(1.39976322701735,1.03040248140542,-7.36821979220919));
#157614=CARTESIAN_POINT('',(2.03646153453295,0.940053946665909,-7.08722970356521));
#157615=CARTESIAN_POINT('Origin',(-1.22081164621868E-13,1.03148891300022,
7.35522753814166E-13));
#157616=CARTESIAN_POINT('',(1.40337283012418,0.849330499797391,-7.36753314876967));
#157617=CARTESIAN_POINT('Origin',(-0.0511926721854314,0.946426678719604,
0.185665675650389));
#157618=CARTESIAN_POINT('',(0.842885249819145,0.940053948012019,-7.45248579171939));
#157619=CARTESIAN_POINT('Origin',(-0.0430257937312871,0.803583941878107,
0.186571820443324));
#157620=CARTESIAN_POINT('Origin',(-0.022681201455298,0.946429259171787,
0.191490017379453));
#157621=CARTESIAN_POINT('Ctrl Pts',(1.355629403,1.070162746,-7.12213233));
#157622=CARTESIAN_POINT('Ctrl Pts',(0.969698837,1.005280647,-7.195590502));
#157623=CARTESIAN_POINT('Ctrl Pts',(0.578090316999999,0.940053947,-7.226915773));
#157624=CARTESIAN_POINT('Ctrl Pts',(0.564630335631451,0.937812039273551,
-7.22799245428371));
#157625=CARTESIAN_POINT('Ctrl Pts',(0.551170354262883,0.935570131547088,
-7.22906913556744));
#157626=CARTESIAN_POINT('Ctrl Pts',(1.64383461035206,1.070162746,-7.31816711034626));
#157627=CARTESIAN_POINT('Ctrl Pts',(1.24728140782744,1.005280647,-7.40724240375129));
#157628=CARTESIAN_POINT('Ctrl Pts',(0.843424901635076,0.940053947,-7.45294549263674));
#157629=CARTESIAN_POINT('Ctrl Pts',(0.82954394457899,0.937812039273551,
-7.45451635407991));
#157630=CARTESIAN_POINT('Ctrl Pts',(0.815662987522898,0.935570131547088,
-7.45608721552305));
#157631=CARTESIAN_POINT('',(0.710487769969494,0.940053949938004,-7.33970078274537));
#157632=CARTESIAN_POINT('Ctrl Pts',(0.578090317,0.940053947,-7.226915773));
#157633=CARTESIAN_POINT('Ctrl Pts',(0.181339832,1.005711878,-7.258652356));
#157634=CARTESIAN_POINT('Ctrl Pts',(-0.216500448,1.070155008,-7.246766697));
#157635=CARTESIAN_POINT('Ctrl Pts',(0.3525203,0.940053947,-7.49171071500001));
#157636=CARTESIAN_POINT('Ctrl Pts',(-0.058767163,1.005711878,-7.51106372900001));
#157637=CARTESIAN_POINT('Ctrl Pts',(-0.469701454,1.070155008,-7.485277586));
#157638=CARTESIAN_POINT('Ctrl Pts',(-0.211783653451336,1.06939092118085,
-7.246906076998));
#157639=CARTESIAN_POINT('Ctrl Pts',(-0.212588380605611,1.06258635139668,
-7.28851000993393));
#157640=CARTESIAN_POINT('Ctrl Pts',(-0.213420318916879,1.05593965224487,
-7.33016303650157));
#157641=CARTESIAN_POINT('Ctrl Pts',(-0.215131163835453,1.04295320260911,
-7.41346913277568));
#157642=CARTESIAN_POINT('Ctrl Pts',(-0.216010993470867,1.03660649245927,
-7.45516690495362));
#157643=CARTESIAN_POINT('Ctrl Pts',(-0.216911912134888,1.03040248144745,
-7.49686262505193));
#157644=CARTESIAN_POINT('',(0.465305306457437,0.940053946665909,-7.35931324412915));
#157645=CARTESIAN_POINT('Ctrl Pts',(-0.207112381,1.070162746,-7.247041083));
#157646=CARTESIAN_POINT('Ctrl Pts',(-0.599811441,1.005280647,-7.23581818000001));
#157647=CARTESIAN_POINT('Ctrl Pts',(-0.988998379000001,0.940053947,-7.182226828));
#157648=CARTESIAN_POINT('Ctrl Pts',(-1.00237512739108,0.937812039399596,
-7.18038483906961));
#157649=CARTESIAN_POINT('Ctrl Pts',(-1.01575187578216,0.935570131799181,
-7.17854285013935));
#157650=CARTESIAN_POINT('Ctrl Pts',(0.0322130647155368,1.070162746,-7.5004482804543));
#157651=CARTESIAN_POINT('Ctrl Pts',(-0.37421749868138,1.005280647,-7.50219382593539));
#157652=CARTESIAN_POINT('Ctrl Pts',(-0.778456877626605,0.940053947,-7.46001119120499));
#157653=CARTESIAN_POINT('Ctrl Pts',(-0.792350993625732,0.937812039399596,
-7.4585613314174));
#157654=CARTESIAN_POINT('Ctrl Pts',(-0.806245109624853,0.93557013179918,
-7.45711147162981));
#157655=CARTESIAN_POINT('',(-0.883941747984165,0.940053949938004,-7.32083652582854));
#157656=CARTESIAN_POINT('Ctrl Pts',(-0.988998379000001,0.940053947,-7.182226828));
#157657=CARTESIAN_POINT('Ctrl Pts',(-1.383295485,1.005711878,-7.127931801));
#157658=CARTESIAN_POINT('Ctrl Pts',(-1.769279415,1.070155008,-7.030800122));
#157659=CARTESIAN_POINT('Ctrl Pts',(-1.266217779,0.940053947,-7.392340126));
#157660=CARTESIAN_POINT('Ctrl Pts',(-1.672049896,1.005711878,-7.32282603));
#157661=CARTESIAN_POINT('Ctrl Pts',(-2.067833513,1.070155008,-7.209304028));
#157662=CARTESIAN_POINT('',(-1.26621778643958,0.940053946884194,-7.39234012602042));
#157663=CARTESIAN_POINT('',(-1.82344449210477,1.03040248140051,-7.27496049378735));
#157664=CARTESIAN_POINT('Origin',(0.00980681374477876,0.803673982828573,
0.186299599692954));
#157665=CARTESIAN_POINT('Ctrl Pts',(-1.76470285870304,1.0693909211237,-7.03195021484481));
#157666=CARTESIAN_POINT('Ctrl Pts',(-1.77443238319902,1.06258635439378,
-7.0724084603665));
#157667=CARTESIAN_POINT('Ctrl Pts',(-1.78419903575377,1.05593965838706,
-7.11290879976689));
#157668=CARTESIAN_POINT('Ctrl Pts',(-1.80377824443044,1.04295319938803,
-7.19389952326287));
#157669=CARTESIAN_POINT('Ctrl Pts',(-1.81360129805581,1.03660648596745,
-7.23443330970032));
#157670=CARTESIAN_POINT('Ctrl Pts',(-1.8234444908508,1.03040248140673,-7.27496049406823));
#157671=CARTESIAN_POINT('',(-1.12760808102257,0.940053946665909,-7.28728347668704));
#157672=CARTESIAN_POINT('Origin',(1.82688066063807E-13,1.03148891300028,
1.05688027773887E-12));
#157673=CARTESIAN_POINT('',(-1.81988018947365,0.849330499782048,-7.27585294622769));
#157674=CARTESIAN_POINT('Origin',(0.0314977611362444,0.946426717532798,
0.190000801711974));
#157675=CARTESIAN_POINT('',(-2.36423563052596,0.940053948011583,-7.11761125000035));
#157676=CARTESIAN_POINT('Origin',(0.0392903192037833,0.80358394884751,0.18739407073207));
#157677=CARTESIAN_POINT('Origin',(0.0598196617767915,0.946429284061458,
0.183315221226698));
#157678=CARTESIAN_POINT('Ctrl Pts',(-1.76016982,1.070162746,-7.03308625));
#157679=CARTESIAN_POINT('Ctrl Pts',(-2.141275202,1.005280647,-6.93770704300001));
#157680=CARTESIAN_POINT('Ctrl Pts',(-2.509842609,0.940053947,-6.801704939));
#157681=CARTESIAN_POINT('Ctrl Pts',(-2.5225106438222,0.937812039302131,
-6.7970304090317));
#157682=CARTESIAN_POINT('Ctrl Pts',(-2.53517867864446,0.935570131604248,
-6.79235587906328));
#157683=CARTESIAN_POINT('Ctrl Pts',(-1.58091472751367,1.070162746,-7.33201682380305));
#157684=CARTESIAN_POINT('Ctrl Pts',(-1.9782184109335,1.005280647,-7.2463510030766));
#157685=CARTESIAN_POINT('Ctrl Pts',(-2.36393887816032,0.940053947,-7.11825505777561));
#157686=CARTESIAN_POINT('Ctrl Pts',(-2.37719648102391,0.937812039302131,
-7.11385227048396));
#157687=CARTESIAN_POINT('Ctrl Pts',(-2.39045408388743,0.935570131604251,
-7.10944948319232));
#157688=CARTESIAN_POINT('',(-2.4370391315969,0.940053949938004,-6.95965808951324));
#157689=CARTESIAN_POINT('Ctrl Pts',(-2.509842609,0.940053947,-6.801704939));
#157690=CARTESIAN_POINT('Ctrl Pts',(-2.883249442,1.005711878,-6.663917077));
#157691=CARTESIAN_POINT('Ctrl Pts',(-3.239328843,1.070155008,-6.486081147));
#157692=CARTESIAN_POINT('Ctrl Pts',(-2.825748922,0.940053947,-6.947311928));
#157693=CARTESIAN_POINT('Ctrl Pts',(-3.207149434,1.005711878,-6.792181124));
#157694=CARTESIAN_POINT('Ctrl Pts',(-3.569275975,1.070155008,-6.596231425));
#157695=CARTESIAN_POINT('',(-2.82574892929789,0.940053946884188,-6.94731192641957));
#157696=CARTESIAN_POINT('',(-3.34471483303188,1.03040248138734,-6.71288929457019));
#157697=CARTESIAN_POINT('Origin',(0.0496264431287224,0.803673994692571,
0.179835839121838));
#157698=CARTESIAN_POINT('Ctrl Pts',(-3.23510652003408,1.06939092112879,
-6.48818817562549));
#157699=CARTESIAN_POINT('Ctrl Pts',(-3.25330590091125,1.06258635422436,
-6.5256089706994));
#157700=CARTESIAN_POINT('Ctrl Pts',(-3.27155059089123,1.05593965801357,
-6.56306289431301));
#157701=CARTESIAN_POINT('Ctrl Pts',(-3.308082654659,1.04295320088744,-6.63795113776892));
#157702=CARTESIAN_POINT('Ctrl Pts',(-3.32638961188595,1.03660648899569,
-6.67542559096316));
#157703=CARTESIAN_POINT('Ctrl Pts',(-3.34471483187464,1.03040248140146,
-6.71288929505088));
#157704=CARTESIAN_POINT('',(-2.66779576740801,0.940053946665909,-6.87450843275956));
#157705=CARTESIAN_POINT('Origin',(-4.28693539000768E-13,1.03148891300006,
-1.08116640640255E-12));
#157706=CARTESIAN_POINT('',(-3.34142571261753,0.849330499763146,-6.71452710230813));
#157707=CARTESIAN_POINT('Origin',(0.0716058869507563,0.946426693350637,
0.1787875325584));
#157708=CARTESIAN_POINT('',(-3.83903714025104,0.940053948010709,-6.44296467836105));
#157709=CARTESIAN_POINT('Origin',(0.0786558872479498,0.803583953786049,
0.174566560624118));
#157710=CARTESIAN_POINT('Origin',(0.0978284994784367,0.946429275126823,
0.166170014912738));
#157711=CARTESIAN_POINT('Ctrl Pts',(-3.230923675,1.070162746,-6.490272121));
#157712=CARTESIAN_POINT('Ctrl Pts',(-3.582615315,1.005280647,-6.315196435));
#157713=CARTESIAN_POINT('Ctrl Pts',(-3.913329389,0.940053947,-6.10314288700001));
#157714=CARTESIAN_POINT('Ctrl Pts',(-3.92469636653137,0.937812039286857,
-6.09585439187666));
#157715=CARTESIAN_POINT('Ctrl Pts',(-3.93606334406277,0.9355701315737,-6.08856589675335));
#157716=CARTESIAN_POINT('Ctrl Pts',(-3.12012070378108,1.070162746,-6.82074841004759));
#157717=CARTESIAN_POINT('Ctrl Pts',(-3.48972002877604,1.005280647,-6.6516768603758));
#157718=CARTESIAN_POINT('Ctrl Pts',(-3.83888572403908,0.940053947,-6.44365722863245));
#157719=CARTESIAN_POINT('Ctrl Pts',(-3.85088690247331,0.937812039286857,
-6.4365073832947));
#157720=CARTESIAN_POINT('Ctrl Pts',(-3.86288808090748,0.935570131573697,
-6.42935753795705));
#157721=CARTESIAN_POINT('',(-3.87618327441021,0.940053949938004,-6.27305377597788));
#157722=CARTESIAN_POINT('Ctrl Pts',(-3.913329389,0.940053947,-6.103142887));
#157723=CARTESIAN_POINT('Ctrl Pts',(-4.24838586,1.005711878,-5.888304997));
#157724=CARTESIAN_POINT('Ctrl Pts',(-4.557910854,1.070155008,-5.638080227));
#157725=CARTESIAN_POINT('Ctrl Pts',(-4.253151186,0.940053947,-6.177435146));
#157726=CARTESIAN_POINT('Ctrl Pts',(-4.592286229,1.005711878,-5.943941379));
#157727=CARTESIAN_POINT('Ctrl Pts',(-4.903823059,1.070155008,-5.674726372));
#157728=CARTESIAN_POINT('',(-4.25315119279166,0.940053946884186,-6.1774351428866));
#157729=CARTESIAN_POINT('',(-4.70959002624101,1.03040248143653,-5.83693085285918));
#157730=CARTESIAN_POINT('Origin',(0.0871253604258709,0.803673999127675,
0.164962849378982));
#157731=CARTESIAN_POINT('Ctrl Pts',(-4.55424019564849,1.06939092116492,
-5.6410456689495));
#157732=CARTESIAN_POINT('Ctrl Pts',(-4.58005845053803,1.06258635411618,
-5.67367925829113));
#157733=CARTESIAN_POINT('Ctrl Pts',(-4.60592807690455,1.05593965775849,
-5.70633546168935));
#157734=CARTESIAN_POINT('Ctrl Pts',(-4.65770463307133,1.04295324250708,
-5.77161933531371));
#157735=CARTESIAN_POINT('Ctrl Pts',(-4.68363929647117,1.03660657338509,
-5.80428196715605));
#157736=CARTESIAN_POINT('Ctrl Pts',(-4.70959002478975,1.03040248144053,
-5.83693085401346));
#157737=CARTESIAN_POINT('',(-4.08324028920423,0.940053946665909,-6.14028901536671));
#157738=CARTESIAN_POINT('Ctrl Pts',(-4.55060313,1.070162746,-5.643980081));
#157739=CARTESIAN_POINT('Ctrl Pts',(-4.856436318,1.005280647,-5.39739426));
#157740=CARTESIAN_POINT('Ctrl Pts',(-5.133833235,0.940053947,-5.119204656));
#157741=CARTESIAN_POINT('Ctrl Pts',(-5.14336764735008,0.937812039408671,
-5.10964299819672));
#157742=CARTESIAN_POINT('Ctrl Pts',(-5.15290205970014,0.93557013181733,
-5.10008134039349));
#157743=CARTESIAN_POINT('Ctrl Pts',(-4.51343330428368,1.070162746,-5.99054938140099));
#157744=CARTESIAN_POINT('Ctrl Pts',(-4.8380462168537,1.005280647,-5.74597770079901));
#157745=CARTESIAN_POINT('Ctrl Pts',(-5.13433054042948,0.940053947,-5.46776114999407));
#157746=CARTESIAN_POINT('Ctrl Pts',(-5.1445141320295,0.937812039408671,
-5.4581985660019));
#157747=CARTESIAN_POINT('Ctrl Pts',(-5.15469772362943,0.93557013181733,
-5.44863598200959));
#157748=CARTESIAN_POINT('',(-5.1343295360762,0.940053947994143,-5.46705224605016));
#157749=CARTESIAN_POINT('Origin',(0.131263079631537,0.946429252240351,0.141254971903578));
#157750=CARTESIAN_POINT('',(-5.13408139500295,0.940053949938004,-5.29312843988776));
#157751=CARTESIAN_POINT('Origin',(3.29163779566599E-13,1.03148891300067,
2.43294967505747E-13));
#157752=CARTESIAN_POINT('',(-4.70672988344602,0.84933049976998,-5.83923743366367));
#157753=CARTESIAN_POINT('Origin',(0.108365671171387,0.946426717023636,0.159214253106947));
#157754=CARTESIAN_POINT('Origin',(0.114343691470368,0.803583965489527,0.153576714676756));
#157755=CARTESIAN_POINT('Ctrl Pts',(-5.133833235,0.940053947,-5.119204656));
#157756=CARTESIAN_POINT('Ctrl Pts',(-5.414872477,1.005711878,-4.83736232));
#157757=CARTESIAN_POINT('Ctrl Pts',(-5.663370019,1.070155008,-4.526448942));
#157758=CARTESIAN_POINT('Ctrl Pts',(-5.48168082800001,0.940053947,-5.118708363));
#157759=CARTESIAN_POINT('Ctrl Pts',(-5.762692823,1.005711878,-4.81776954000001));
#157760=CARTESIAN_POINT('Ctrl Pts',(-6.00907282800001,1.070155008,-4.487877421));
#157761=CARTESIAN_POINT('',(-5.48168083392426,0.940053946884176,-5.11870835851933));
#157762=CARTESIAN_POINT('',(-5.30775703292102,0.940053946665848,-5.11895650802657));
#157763=CARTESIAN_POINT('',(-5.85425002368675,1.03040248140204,-4.6880440119527));
#157764=CARTESIAN_POINT('Origin',(0.12055094137318,0.803673950252423,0.142377062403563));
#157765=CARTESIAN_POINT('Ctrl Pts',(-5.66042266110811,1.06939092119514,
-4.5301341364565));
#157766=CARTESIAN_POINT('Ctrl Pts',(-5.69265256937191,1.06258635144978,
-4.55645461935443));
#157767=CARTESIAN_POINT('Ctrl Pts',(-5.72493751116658,1.05593965231105,
-4.58278614556));
#157768=CARTESIAN_POINT('Ctrl Pts',(-5.78953782558348,1.04295320444697,
-4.63541342140573));
#157769=CARTESIAN_POINT('Ctrl Pts',(-5.8218878647054,1.03660649618985,-4.66173740606064));
#157770=CARTESIAN_POINT('Ctrl Pts',(-5.85425002241471,1.03040248143066,
-4.68804401325544));
#157771=CARTESIAN_POINT('Origin',(-7.68482499857726E-13,1.03148891300006,
-6.66133814775094E-13));
#157772=CARTESIAN_POINT('',(-6.18954639384257,0.94005394801071,-4.23550651616131));
#157773=CARTESIAN_POINT('Origin',(0.158559547460965,0.946429307724211,0.109734571990215));
#157774=CARTESIAN_POINT('',(-5.85195259583044,0.849330499752317,-4.69091151220864));
#157775=CARTESIAN_POINT('Origin',(0.140058776211579,0.946426676654599,0.132196708814087));
#157776=CARTESIAN_POINT('Origin',(0.144684649935504,0.80358397165336,0.125405500795563));
#157777=CARTESIAN_POINT('Ctrl Pts',(-5.65750144,1.070162746,-4.533781805));
#157778=CARTESIAN_POINT('Ctrl Pts',(-5.903175755,1.005280647,-4.227215929));
#157779=CARTESIAN_POINT('Ctrl Pts',(-6.114284746,0.940053947,-3.895898106));
#157780=CARTESIAN_POINT('Ctrl Pts',(-6.12154077546899,0.937812039371516,
-3.8845103774343));
#157781=CARTESIAN_POINT('Ctrl Pts',(-6.12879680493797,0.935570131743017,
-3.87312264886852));
#157782=CARTESIAN_POINT('Ctrl Pts',(-5.69570277961804,1.070162746,-4.88023892213736));
#157783=CARTESIAN_POINT('Ctrl Pts',(-5.96015074082017,1.005280647,-4.57160301106027));
#157784=CARTESIAN_POINT('Ctrl Pts',(-6.18969976651681,0.940053947,-4.23619863575172));
#157785=CARTESIAN_POINT('Ctrl Pts',(-6.19758959862271,0.937812039371516,
-4.22467044825133));
#157786=CARTESIAN_POINT('Ctrl Pts',(-6.20547943072859,0.935570131743017,
-4.21314226075093));
#157787=CARTESIAN_POINT('',(-6.15191557598767,0.940053949937996,-4.06570230088741));
#157788=CARTESIAN_POINT('Ctrl Pts',(-6.114284746,0.940053947,-3.895898106));
#157789=CARTESIAN_POINT('Ctrl Pts',(-6.328165675,1.005711878,-3.560229957));
#157790=CARTESIAN_POINT('Ctrl Pts',(-6.504016297,1.070155008,-3.203165935));
#157791=CARTESIAN_POINT('Ctrl Pts',(-6.453893166,0.940053947,-3.820636465));
#157792=CARTESIAN_POINT('Ctrl Pts',(-6.663642306,1.005711878,-3.466324153));
#157793=CARTESIAN_POINT('Ctrl Pts',(-6.833345029,1.070155008,-3.09118031));
#157794=CARTESIAN_POINT('',(-6.45389317085123,0.940053946884177,-3.82063645932707));
#157795=CARTESIAN_POINT('',(-6.72517179580522,1.03040248141041,-3.3199494442733));
#157796=CARTESIAN_POINT('Origin',(0.148339177973227,0.803673947869585,0.11313337249165));
#157797=CARTESIAN_POINT('Ctrl Pts',(-6.50193005456292,1.06939092119945,
-3.2073985664642));
#157798=CARTESIAN_POINT('Ctrl Pts',(-6.53906455727252,1.06258635401515,
-3.22617520648721));
#157799=CARTESIAN_POINT('Ctrl Pts',(-6.57625517898209,1.05593965751181,
-3.24495080022106));
#157800=CARTESIAN_POINT('Ctrl Pts',(-6.65065852245689,1.04295320266092,
-3.2824605419063));
#157801=CARTESIAN_POINT('Ctrl Pts',(-6.68791112565472,1.03660649256361,
-3.30121479015096));
#157802=CARTESIAN_POINT('Ctrl Pts',(-6.72517179514983,1.03040248143128,
-3.31994944530406));
#157803=CARTESIAN_POINT('',(-6.28408895707088,0.940053946665902,-3.85826728375583));
#157804=CARTESIAN_POINT('Origin',(-1.09461051334137E-12,1.03148891300011,
-5.60966204044E-13));
#157805=CARTESIAN_POINT('',(-6.72354450891251,0.849330499744447,-3.32324378227747));
#157806=CARTESIAN_POINT('Origin',(0.165202437536132,0.946426669462313,0.0989974117800008));
#157807=CARTESIAN_POINT('',(-6.95534693954528,0.940053948010697,-2.8059132146749));
#157808=CARTESIAN_POINT('Origin',(0.168260764014773,0.803583930496838,0.0913708078726105));
#157809=CARTESIAN_POINT('Origin',(0.178442577358902,0.946429305675131,0.0730836020607856));
#157810=CARTESIAN_POINT('Ctrl Pts',(-6.499861271,1.070162746,-3.211588931));
#157811=CARTESIAN_POINT('Ctrl Pts',(-6.673889256,1.005280647,-2.859377679));
#157812=CARTESIAN_POINT('Ctrl Pts',(-6.808839097,0.940053947,-2.49042369));
#157813=CARTESIAN_POINT('Ctrl Pts',(-6.81347745935914,0.93781203943013,
-2.4777423686872));
#157814=CARTESIAN_POINT('Ctrl Pts',(-6.8181158217183,0.935570131860246,
-2.46506104737443));
#157815=CARTESIAN_POINT('Ctrl Pts',(-6.61164752301968,1.070162746,-3.54173391418792));
#157816=CARTESIAN_POINT('Ctrl Pts',(-6.80356523949808,1.005280647,-3.18346524449584));
#157817=CARTESIAN_POINT('Ctrl Pts',(-6.95564551169704,0.940053947,-2.8065561823157));
#157818=CARTESIAN_POINT('Ctrl Pts',(-6.96087266428134,0.93781203943013,
-2.79360143710162));
#157819=CARTESIAN_POINT('Ctrl Pts',(-6.96609981686578,0.935570131860243,
-2.78064669188749));
#157820=CARTESIAN_POINT('',(-6.88209302200538,0.940053949937988,-2.64816844109373));
#157821=CARTESIAN_POINT('Ctrl Pts',(-6.808839097,0.940053947,-2.49042369));
#157822=CARTESIAN_POINT('Ctrl Pts',(-6.945560879,1.005711878,-2.116625199));
#157823=CARTESIAN_POINT('Ctrl Pts',(-7.040542002,1.070155008,-1.730106449));
#157824=CARTESIAN_POINT('Ctrl Pts',(-7.124328633,0.940053947,-2.343915853));
#157825=CARTESIAN_POINT('Ctrl Pts',(-7.253007281,1.005711878,-1.9527973));
#157826=CARTESIAN_POINT('Ctrl Pts',(-7.33809761200001,1.070155008,-1.549943043));
#157827=CARTESIAN_POINT('',(-7.12432863651568,0.940053946884185,-2.34391584642018));
#157828=CARTESIAN_POINT('',(-7.28163201009094,1.03040248138348,-1.79661772960873));
#157829=CARTESIAN_POINT('Origin',(0.16919157413491,0.803673975598803,0.0785998784174352));
#157830=CARTESIAN_POINT('Ctrl Pts',(-7.039414425409,1.06939092121324,-1.73468860427594));
#157831=CARTESIAN_POINT('Ctrl Pts',(-7.07971716454285,1.06258635436219,
-1.74504343605081));
#157832=CARTESIAN_POINT('Ctrl Pts',(-7.12007448535464,1.05593965822046,
-1.75538518191534));
#157833=CARTESIAN_POINT('Ctrl Pts',(-7.20080181548591,1.04295320175447,
-1.77602344967893));
#157834=CARTESIAN_POINT('Ctrl Pts',(-7.241215088716,1.03660649073035,-1.78633102704174));
#157835=CARTESIAN_POINT('Ctrl Pts',(-7.28163200969059,1.03040248140093,
-1.79661773077921));
#157836=CARTESIAN_POINT('',(-6.9665838656709,0.940053946665902,-2.41716976956639));
#157837=CARTESIAN_POINT('Origin',(-1.03866568124111E-12,1.03148891300022,
-2.78531538111526E-13));
#157838=CARTESIAN_POINT('',(-7.2807509534696,0.849330499739627,-1.80018486640627));
#157839=CARTESIAN_POINT('Origin',(0.182621432084888,0.946426675897866,0.0611692177252093));
#157840=CARTESIAN_POINT('',(-7.39592319216369,0.940053948011588,-1.24511853176423));
#157841=CARTESIAN_POINT('Origin',(0.183968884429788,0.803583937744143,0.0530635059579526));
#157842=CARTESIAN_POINT('Origin',(0.189981445166029,0.946429293144479,0.0330150515353095));
#157843=CARTESIAN_POINT('Ctrl Pts',(-7.038294813,1.070162746,-1.739225727));
#157844=CARTESIAN_POINT('Ctrl Pts',(-7.13253911200001,1.005280647,-1.357838106));
#157845=CARTESIAN_POINT('Ctrl Pts',(-7.185019699,0.940053947,-0.96849983));
#157846=CARTESIAN_POINT('Ctrl Pts',(-7.18682350978693,0.937812039434179,
-0.955117880175332));
#157847=CARTESIAN_POINT('Ctrl Pts',(-7.1886273205737,0.935570131868345,
-0.941735930350652));
#157848=CARTESIAN_POINT('Ctrl Pts',(-7.21843897667503,1.070162746,-2.03762136480417));
#157849=CARTESIAN_POINT('Ctrl Pts',(-7.32885259013869,1.005280647,-1.64647218155056));
#157850=CARTESIAN_POINT('Ctrl Pts',(-7.39635300274975,0.940053947,-1.24568228101568));
#157851=CARTESIAN_POINT('Ctrl Pts',(-7.39867306011474,0.937812039434179,
-1.23190672728822));
#157852=CARTESIAN_POINT('Ctrl Pts',(-7.40099311747971,0.935570131868342,
-1.21813117356077));
#157853=CARTESIAN_POINT('',(-7.29047144671895,0.940053949937996,-1.10680916809047));
#157854=CARTESIAN_POINT('Ctrl Pts',(-7.185019699,0.940053947,-0.96849983));
#157855=CARTESIAN_POINT('Ctrl Pts',(-7.238189376,1.005711878,-0.574049398));
#157856=CARTESIAN_POINT('Ctrl Pts',(-7.247859787,1.070155008,-0.176149108));
#157857=CARTESIAN_POINT('Ctrl Pts',(-7.461638412,0.940053947,-0.75759634));
#157858=CARTESIAN_POINT('Ctrl Pts',(-7.503229697,1.005711878,-0.347959816));
#157859=CARTESIAN_POINT('Ctrl Pts',(-7.499728906,1.070155008,0.063767838));
#157860=CARTESIAN_POINT('',(-7.46163841400411,0.940053946884194,-0.757596332849195));
#157861=CARTESIAN_POINT('',(-7.49761120468137,1.0304024813601,-0.189278166809903));
#157862=CARTESIAN_POINT('Origin',(0.182132582553779,0.803673978539305,0.0403910626042792));
#157863=CARTESIAN_POINT('Ctrl Pts',(-7.24774360045422,1.06939092115902,
-0.180866531000679));
#157864=CARTESIAN_POINT('Ctrl Pts',(-7.28933006618477,1.06258635442796,
-0.18231537485848));
#157865=CARTESIAN_POINT('Ctrl Pts',(-7.33096702426481,1.0559396584134,-0.183739705341759));
#157866=CARTESIAN_POINT('Ctrl Pts',(-7.41424361053092,1.04295320219039,
-0.186541472070499));
#157867=CARTESIAN_POINT('Ctrl Pts',(-7.4559278651807,1.03660649163244,-0.187920404768487));
#157868=CARTESIAN_POINT('Ctrl Pts',(-7.49761120453003,1.03040248137935,
-0.189278168028761));
#157869=CARTESIAN_POINT('',(-7.32332905573954,0.940053946665902,-0.863048082967379));
#157870=CARTESIAN_POINT('Origin',(-1.02782365951626E-13,1.03148891300017,
-9.97465998686664E-14));
#157871=CARTESIAN_POINT('',(-7.49751757547009,0.849330500331513,-0.192951307338575));
#157872=CARTESIAN_POINT('Origin',(0.191501740654354,0.946426720742303,0.0204809236977732));
#157873=CARTESIAN_POINT('',(-7.49067429688827,0.940053948011587,0.373896511679711));
#157874=CARTESIAN_POINT('Origin',(0.191074840971184,0.80358395566385,0.012275030548928));
#157875=CARTESIAN_POINT('Origin',(0.192636884694252,0.946429308031184,-0.00859721590453562));
#157876=CARTESIAN_POINT('Ctrl Pts',(-7.24762551100001,1.070162746,-0.185538262));
#157877=CARTESIAN_POINT('Ctrl Pts',(-7.257679367,1.005280647,0.207192467));
#157878=CARTESIAN_POINT('Ctrl Pts',(-7.225236766,0.940053947,0.598710006));
#157879=CARTESIAN_POINT('Ctrl Pts',(-7.22412168102199,0.937812039412696,
0.612166859424246));
#157880=CARTESIAN_POINT('Ctrl Pts',(-7.2230065960441,0.935570131825379,
0.62562371284849));
#157881=CARTESIAN_POINT('Ctrl Pts',(-7.48770424676855,1.070162746,-0.438231905210894));
#157882=CARTESIAN_POINT('Ctrl Pts',(-7.51145093952435,1.005280647,-0.0324919097134924));
#157883=CARTESIAN_POINT('Ctrl Pts',(-7.4912152481729,0.940053947,0.373438339134095));
#157884=CARTESIAN_POINT('Ctrl Pts',(-7.49051972701397,0.937812039412696,
0.387390571959122));
#157885=CARTESIAN_POINT('Ctrl Pts',(-7.48982420585515,0.93557013182538,
0.401342804784149));
#157886=CARTESIAN_POINT('',(-7.35795552980536,0.940053949937996,0.486303271575305));
#157887=CARTESIAN_POINT('Ctrl Pts',(-7.225236766,0.940053947,0.598710006));
#157888=CARTESIAN_POINT('Ctrl Pts',(-7.192368183,1.005711878,0.995368314));
#157889=CARTESIAN_POINT('Ctrl Pts',(-7.116275704,1.070155008,1.386044769));
#157890=CARTESIAN_POINT('Ctrl Pts',(-7.450050271,0.940053947,0.864147535));
#157891=CARTESIAN_POINT('Ctrl Pts',(-7.402609431,1.005711878,1.273147882));
#157892=CARTESIAN_POINT('Ctrl Pts',(-7.310681212,1.070155008,1.674497005));
#157893=CARTESIAN_POINT('',(-7.45005027142285,0.940053946884191,0.864147542426273));
#157894=CARTESIAN_POINT('',(-7.36301043203333,1.0304024814159,1.426911832604));
#157895=CARTESIAN_POINT('Origin',(0.186557358451386,0.803674007595516,0.000293611196806182));
#157896=CARTESIAN_POINT('Ctrl Pts',(-7.11717634030228,1.06939092119072,
1.38141266024738));
#157897=CARTESIAN_POINT('Ctrl Pts',(-7.15810199822856,1.06258635413951,
1.38893755060872));
#157898=CARTESIAN_POINT('Ctrl Pts',(-7.19907169867902,1.05593965777816,
1.39649723575846));
#157899=CARTESIAN_POINT('Ctrl Pts',(-7.28100362967791,1.04295320030069,
1.4116629786443));
#157900=CARTESIAN_POINT('Ctrl Pts',(-7.32200977315745,1.03660648775052,
1.41927716981832));
#157901=CARTESIAN_POINT('Ctrl Pts',(-7.36301043220623,1.03040248142752,
1.42691183134996));
#157902=CARTESIAN_POINT('',(-7.33764351829699,0.940053946665902,0.731428772536595));
#157903=CARTESIAN_POINT('Origin',(-5.11743425413158E-13,1.03148891299978,
6.89552581700781E-14));
#157904=CARTESIAN_POINT('',(-7.36370860840547,0.84933050033943,1.42330444080272));
#157905=CARTESIAN_POINT('Origin',(0.191427338004395,0.946426677476739,-0.0211651271497584));
#157906=CARTESIAN_POINT('',(-7.23516979657277,0.94005394801158,1.97542857061911));
#157907=CARTESIAN_POINT('Origin',(0.189246193072801,0.803583945876243,-0.0290873467451794));
#157908=CARTESIAN_POINT('Origin',(0.186285059628298,0.94642927109937,-0.0498074733912154));
#157909=CARTESIAN_POINT('Ctrl Pts',(-7.118065296,1.070162746,1.376824766));
#157910=CARTESIAN_POINT('Ctrl Pts',(-7.0434586,1.005280647,1.762534951));
#157911=CARTESIAN_POINT('Ctrl Pts',(-6.927609792,0.940053947,2.137924827));
#157912=CARTESIAN_POINT('Ctrl Pts',(-6.92362795126682,0.93781203933228,
2.15082735681355));
#157913=CARTESIAN_POINT('Ctrl Pts',(-6.91964611053353,0.935570131664546,
2.16372988662716));
#157914=CARTESIAN_POINT('Ctrl Pts',(-7.40685278759771,1.070162746,1.18164879131978));
#157915=CARTESIAN_POINT('Ctrl Pts',(-7.3428221904726,1.005280647,1.58300764889336));
#157916=CARTESIAN_POINT('Ctrl Pts',(-7.2357965942918,0.940053947,1.97509739841982));
#157917=CARTESIAN_POINT('Ctrl Pts',(-7.23211801627514,0.93781203933228,
1.98857391978146));
#157918=CARTESIAN_POINT('Ctrl Pts',(-7.22843943825845,0.935570131664544,
2.00205044114303));
#157919=CARTESIAN_POINT('',(-7.08138978994764,0.940053949937996,2.0566767108959));
#157920=CARTESIAN_POINT('Ctrl Pts',(-6.927609792,0.940053947,2.137924827));
#157921=CARTESIAN_POINT('Ctrl Pts',(-6.81023984700001,1.005711878,2.518243711));
#157922=CARTESIAN_POINT('Ctrl Pts',(-6.65194247900001,1.070155008,2.883428734));
#157923=CARTESIAN_POINT('Ctrl Pts',(-7.090106059,0.940053947,2.445484832));
#157924=CARTESIAN_POINT('Ctrl Pts',(-6.955851376,1.005711878,2.8347246));
#157925=CARTESIAN_POINT('Ctrl Pts',(-6.779794189,1.070155008,3.206928554));
#157926=CARTESIAN_POINT('',(-7.09010605781718,0.940053946884182,2.44548483938707));
#157927=CARTESIAN_POINT('',(-6.88412347496954,1.03040248139212,2.97638102061096));
#157928=CARTESIAN_POINT('Origin',(0.182258551121615,0.803674002173012,-0.0398174380776881));
#157929=CARTESIAN_POINT('Ctrl Pts',(-6.65381782566217,1.06939092107355,
2.87909853088944));
#157930=CARTESIAN_POINT('Ctrl Pts',(-6.69216903288866,1.06258635444552,
2.89524529923536));
#157931=CARTESIAN_POINT('Ctrl Pts',(-6.73055577275058,1.05593965854339,
2.91143551651327));
#157932=CARTESIAN_POINT('Ctrl Pts',(-6.80731199029965,1.04295320173078,
2.94385963439241));
#157933=CARTESIAN_POINT('Ctrl Pts',(-6.84572259686926,1.03660649073646,
2.96011091445485));
#157934=CARTESIAN_POINT('Ctrl Pts',(-6.88412347535908,1.03040248140959,
2.97638101943679));
#157935=CARTESIAN_POINT('',(-7.00885792486393,0.940053946665902,2.29170483144534));
#157936=CARTESIAN_POINT('Origin',(-1.03866568124111E-12,1.03148891299989,
4.40836603332606E-13));
#157937=CARTESIAN_POINT('',(-6.88558081090655,0.849330499781311,2.97300805498949));
#157938=CARTESIAN_POINT('Origin',(0.182401896620048,0.946426692996323,-0.0618214724555677));
#157939=CARTESIAN_POINT('',(-6.64135679832037,0.940053948011584,3.48459178406726));
#157940=CARTESIAN_POINT('Origin',(0.178568934923994,0.803583974132988,-0.0690897062119694));
#157941=CARTESIAN_POINT('Origin',(0.171222606441985,0.9464292487965,-0.088688748689485));
#157942=CARTESIAN_POINT('Ctrl Pts',(-6.65567225900001,1.070162746,2.874808998));
#157943=CARTESIAN_POINT('Ctrl Pts',(-6.49989353800001,1.005280647,3.235463259));
#157944=CARTESIAN_POINT('Ctrl Pts',(-6.306055484,0.940053947,3.577172659));
#157945=CARTESIAN_POINT('Ctrl Pts',(-6.29939307402217,0.937812039345993,
3.58891755670764));
#157946=CARTESIAN_POINT('Ctrl Pts',(-6.29273066404431,0.935570131691972,
3.60066245441528));
#157947=CARTESIAN_POINT('Ctrl Pts',(-6.97966512496644,1.070162746,2.74627690293544));
#157948=CARTESIAN_POINT('Ctrl Pts',(-6.83085123717913,1.005280647,3.12448752840956));
#157949=CARTESIAN_POINT('Ctrl Pts',(-6.64204013408926,0.940053947,3.48440309746884));
#157950=CARTESIAN_POINT('Ctrl Pts',(-6.63555050549884,0.937812039345993,
3.49677375962209));
#157951=CARTESIAN_POINT('Ctrl Pts',(-6.62906087690843,0.935570131691969,
3.50914442177529));
#157952=CARTESIAN_POINT('',(-6.47370613432616,0.940053949937996,3.53088223240309));
#157953=CARTESIAN_POINT('Ctrl Pts',(-6.306055484,0.940053947,3.577172659));
#157954=CARTESIAN_POINT('Ctrl Pts',(-6.109672265,1.005711878,3.92336883));
#157955=CARTESIAN_POINT('Ctrl Pts',(-5.876571816,1.070155008,4.245986775));
#157956=CARTESIAN_POINT('Ctrl Pts',(-6.398636369,0.940053947,3.912473977));
#157957=CARTESIAN_POINT('Ctrl Pts',(-6.183845441,1.005711878,4.263752746));
#157958=CARTESIAN_POINT('Ctrl Pts',(-5.93189152599999,1.070155008,4.589407688));
#157959=CARTESIAN_POINT('',(-6.39863636626611,0.940053946884198,3.91247398391473));
#157960=CARTESIAN_POINT('',(-6.08334255562739,1.03040248140864,4.38667794022568));
#157961=CARTESIAN_POINT('Origin',(0.169438150914281,0.803673962997426,-0.0780669157412039));
#157962=CARTESIAN_POINT('Ctrl Pts',(-5.87933418335156,1.06939092119007,
4.2421609543172));
#157963=CARTESIAN_POINT('Ctrl Pts',(-5.91331768376038,1.06258635438258,
4.26617459658952));
#157964=CARTESIAN_POINT('Ctrl Pts',(-5.94732654606767,1.05593965826363,
4.29023831069015));
#157965=CARTESIAN_POINT('Ctrl Pts',(-6.01531802142512,1.04295320100036,
4.33840469011669));
#157966=CARTESIAN_POINT('Ctrl Pts',(-6.0493370692213,1.0366064891846,4.36253317257371));
#157967=CARTESIAN_POINT('Ctrl Pts',(-6.08334255628681,1.03040248142303,
4.38667793916132));
#157968=CARTESIAN_POINT('',(-6.35234592546061,0.940053946665902,3.74482331976312));
#157969=CARTESIAN_POINT('Origin',(4.90059381963448E-14,1.03148891299983,
-1.29236898960272E-13));
#157970=CARTESIAN_POINT('',(-6.08549090775791,0.849330500325969,4.38369711683369));
#157971=CARTESIAN_POINT('Origin',(0.164847907881348,0.946426697543599,-0.0995873118847546));
#157972=CARTESIAN_POINT('',(-5.73700133724396,0.94005394801159,4.83081935903908));
#157973=CARTESIAN_POINT('Origin',(0.15954181886888,0.803583967399387,-0.105861446646613));
#157974=CARTESIAN_POINT('Origin',(0.148154021637887,0.94642927363567,-0.123423023477816));
#157975=CARTESIAN_POINT('Ctrl Pts',(-5.882067385,1.070162746,4.238370357));
#157976=CARTESIAN_POINT('Ctrl Pts',(-5.65240067800001,1.005280647,4.557104901));
#157977=CARTESIAN_POINT('Ctrl Pts',(-5.38963703,0.940053947,4.849155874));
#157978=CARTESIAN_POINT('Ctrl Pts',(-5.38060557750435,0.937812039312306,
4.85919396149436));
#157979=CARTESIAN_POINT('Ctrl Pts',(-5.37157412500868,0.935570131624597,
4.86923204898861));
#157980=CARTESIAN_POINT('Ctrl Pts',(-6.22611607790624,1.070162746,4.18249215983857));
#157981=CARTESIAN_POINT('Ctrl Pts',(-5.99947727211045,1.005280647,4.51986984361793));
#157982=CARTESIAN_POINT('Ctrl Pts',(-5.73770925905211,0.940053947,4.83078198081959));
#157983=CARTESIAN_POINT('Ctrl Pts',(-5.72871202753696,0.937812039312306,
4.84146834561484));
#157984=CARTESIAN_POINT('Ctrl Pts',(-5.7197147960219,0.935570131624597,
4.85215471041007));
#157985=CARTESIAN_POINT('',(-5.56331917461025,0.940053949937996,4.83998762566666));
#157986=CARTESIAN_POINT('Ctrl Pts',(-5.38963702999999,0.940053947,4.849155874));
#157987=CARTESIAN_POINT('Ctrl Pts',(-5.123423198,1.005711878,5.145041583));
#157988=CARTESIAN_POINT('Ctrl Pts',(-4.826419186,1.070155008,5.410007194));
#157989=CARTESIAN_POINT('Ctrl Pts',(-5.407973553,0.940053947,5.196520186));
#157990=CARTESIAN_POINT('Ctrl Pts',(-5.122689766,1.005711878,5.493412553));
#157991=CARTESIAN_POINT('Ctrl Pts',(-4.806620207,1.070155008,5.75729121900001));
#157992=CARTESIAN_POINT('',(-5.40797354882796,0.940053946884182,5.19652019220046));
#157993=CARTESIAN_POINT('',(-4.99811129844124,1.03040248142711,5.59185867529939));
#157994=CARTESIAN_POINT('Origin',(0.148694582446472,0.803673986557815,-0.112665824199406));
#157995=CARTESIAN_POINT('Ctrl Pts',(-4.8299394093612,1.06939092113262,5.40686464598623));
#157996=CARTESIAN_POINT('Ctrl Pts',(-4.85796618327951,1.06258635138517,
5.43762232415357));
#157997=CARTESIAN_POINT('Ctrl Pts',(-4.88600696365171,1.05593965225773,
5.46843435718009));
#157998=CARTESIAN_POINT('Ctrl Pts',(-4.94205445198269,1.04295320341478,
5.53009075102171));
#157999=CARTESIAN_POINT('Ctrl Pts',(-4.97009123117722,1.03660649407792,
5.56096819981129));
#158000=CARTESIAN_POINT('Ctrl Pts',(-4.99811129971693,1.0304024814516,5.5918586739572));
#158001=CARTESIAN_POINT('',(-5.39880529010589,0.940053946665902,5.02283803149846));
#158002=CARTESIAN_POINT('Origin',(-2.32019264911898E-13,1.03148891299983,
2.66713734431434E-13));
#158003=CARTESIAN_POINT('',(-5.00085021307736,0.849330499754917,5.58940937371024));
#158004=CARTESIAN_POINT('Origin',(0.139585301709059,0.9464267015393,-0.132696195866576));
#158005=CARTESIAN_POINT('',(-4.56439006760893,0.940053948010712,5.95116319036083));
#158006=CARTESIAN_POINT('Origin',(0.133054720215192,0.803583963958215,-0.137683229263514));
#158007=CARTESIAN_POINT('Origin',(0.118157849674241,0.946429283675318,-0.152386068274454));
#158008=CARTESIAN_POINT('Ctrl Pts',(-4.833423576,1.070162746,5.403750228));
#158009=CARTESIAN_POINT('Ctrl Pts',(-4.540607845,1.005280647,5.665661383));
#158010=CARTESIAN_POINT('Ctrl Pts',(-4.221205138,0.940053947,5.894397949));
#158011=CARTESIAN_POINT('Ctrl Pts',(-4.21022694371415,0.937812039309391,
5.90225985626249));
#158012=CARTESIAN_POINT('Ctrl Pts',(-4.19924874942829,0.935570131618771,
5.91012176352508));
#158013=CARTESIAN_POINT('Ctrl Pts',(-5.18144076305731,1.070162746,5.42313873171225));
#158014=CARTESIAN_POINT('Ctrl Pts',(-4.88757441729678,1.005280647,5.70390806884625));
#158015=CARTESIAN_POINT('Ctrl Pts',(-4.56508947558847,0.940053947,5.9512788675075));
#158016=CARTESIAN_POINT('Ctrl Pts',(-4.55400534177636,0.937812039309391,
5.95978125220506));
#158017=CARTESIAN_POINT('Ctrl Pts',(-4.54292120796426,0.935570131618772,
5.96828363690254));
#158018=CARTESIAN_POINT('',(-4.3927975929503,0.940053949937996,5.9227805762912));
#158019=CARTESIAN_POINT('Ctrl Pts',(-4.221205138,0.940053947,5.894397949));
#158020=CARTESIAN_POINT('Ctrl Pts',(-3.897608556,1.005711878,6.12613791));
#158021=CARTESIAN_POINT('Ctrl Pts',(-3.55058856,1.070155008,6.321061689));
#158022=CARTESIAN_POINT('Ctrl Pts',(-4.164439905,0.940053947,6.237582888));
#158023=CARTESIAN_POINT('Ctrl Pts',(-3.822002811,1.005711878,6.466206494));
#158024=CARTESIAN_POINT('Ctrl Pts',(-3.45659667,1.070155008,6.655970212));
#158025=CARTESIAN_POINT('',(-4.1644398996237,0.940053946884196,6.2375828931164));
#158026=CARTESIAN_POINT('',(-3.67917391284191,1.03040248141186,6.53557031310756));
#158027=CARTESIAN_POINT('Origin',(0.120998550274901,0.803673961062085,-0.141997014740639));
#158028=CARTESIAN_POINT('Ctrl Pts',(-3.55470203693565,1.06939092122075,
6.31874935624554));
#158029=CARTESIAN_POINT('Ctrl Pts',(-3.5754615686637,1.06258635149433,6.35481286461373));
#158030=CARTESIAN_POINT('Ctrl Pts',(-3.59622309476572,1.05593965237264,
6.39093246815098));
#158031=CARTESIAN_POINT('Ctrl Pts',(-3.63770592193111,1.0429532034737,6.46319592317457));
#158032=CARTESIAN_POINT('Ctrl Pts',(-3.65844947780599,1.03660649420318,
6.49937855271611));
#158033=CARTESIAN_POINT('Ctrl Pts',(-3.67917391437289,1.03040248143664,
6.53557031207056));
#158034=CARTESIAN_POINT('',(-4.19282251981636,0.940053946665902,6.06599041966374));
#158035=CARTESIAN_POINT('Origin',(1.95373231481888E-13,1.03148891300056,
-4.58400678526871E-13));
#158036=CARTESIAN_POINT('',(-3.68237532060303,0.849330499766696,6.53376706031241));
#158037=CARTESIAN_POINT('Origin',(0.107796101383926,0.946426683836144,-0.159600559127751));
#158038=CARTESIAN_POINT('',(-3.17835299299454,0.940053948010695,6.79323724514997));
#158039=CARTESIAN_POINT('Origin',(0.100346144483314,0.80358391676753,-0.163067062224314));
#158040=CARTESIAN_POINT('Origin',(0.0826369660285103,0.94642931938388,-0.174223943159391));
#158041=CARTESIAN_POINT('Ctrl Pts',(-3.558774254,1.070162746,6.316456745));
#158042=CARTESIAN_POINT('Ctrl Pts',(-3.216501235,1.005280647,6.509297835));
#158043=CARTESIAN_POINT('Ctrl Pts',(-2.855394386,0.940053947,6.664024527));
#158044=CARTESIAN_POINT('Ctrl Pts',(-2.84298277861454,0.937812039393734,
6.66934263979257));
#158045=CARTESIAN_POINT('Ctrl Pts',(-2.83057117122915,0.935570131787453,
6.67466075258513));
#158046=CARTESIAN_POINT('Ctrl Pts',(-3.89448703709711,1.070162746,6.41020536373886));
#158047=CARTESIAN_POINT('Ctrl Pts',(-3.54713401528997,1.005280647,6.62123789183456));
#158048=CARTESIAN_POINT('Ctrl Pts',(-3.17901118204665,0.940053947,6.79350056985927));
#158049=CARTESIAN_POINT('Ctrl Pts',(-3.16635842819142,0.937812039393734,
6.79942141221586));
#158050=CARTESIAN_POINT('Ctrl Pts',(-3.15370567433618,0.935570131787455,
6.80534225457233));
#158051=CARTESIAN_POINT('',(-3.01687367847068,0.940053949937996,6.72863089041115));
#158052=CARTESIAN_POINT('Ctrl Pts',(-2.855394386,0.940053947,6.664024527));
#158053=CARTESIAN_POINT('Ctrl Pts',(-2.489546071,1.005711878,6.82078283800001));
#158054=CARTESIAN_POINT('Ctrl Pts',(-2.108736358,1.070155008,6.936550365));
#158055=CARTESIAN_POINT('Ctrl Pts',(-2.726181675,0.940053947,6.986983146));
#158056=CARTESIAN_POINT('Ctrl Pts',(-2.342603253,1.005711878,7.136647807));
#158057=CARTESIAN_POINT('Ctrl Pts',(-1.944946514,1.070155008,7.243423435));
#158058=CARTESIAN_POINT('',(-2.72618166865117,0.940053946884198,6.98698314983959));
#158059=CARTESIAN_POINT('',(-2.18820244488194,1.03040248138689,7.17368594663709));
#158060=CARTESIAN_POINT('Origin',(0.087644423473624,0.803673967492884,-0.16468805624954));
#158061=CARTESIAN_POINT('Ctrl Pts',(-2.11325074753863,1.06939092118773,
6.93517636918274));
#158062=CARTESIAN_POINT('Ctrl Pts',(-2.12577234001398,1.06258635408308,
6.97485940334765));
#158063=CARTESIAN_POINT('Ctrl Pts',(-2.13828382082693,1.05593965766241,
7.01459764785347));
#158064=CARTESIAN_POINT('Ctrl Pts',(-2.16326231440692,1.04295319922269,
7.09408926356511));
#158065=CARTESIAN_POINT('Ctrl Pts',(-2.17574271090272,1.03660648558926,
7.13388524388851));
#158066=CARTESIAN_POINT('Ctrl Pts',(-2.18820244610799,1.03040248139184,
7.1736859462382));
#158067=CARTESIAN_POINT('',(-2.79078802860556,0.940053946665902,6.8255038372746));
#158068=CARTESIAN_POINT('Origin',(-4.74880551548651E-14,1.03148891299972,
3.08780778723872E-13));
#158069=CARTESIAN_POINT('',(-2.19171665066048,0.849330499771342,7.17261306109147));
#158070=CARTESIAN_POINT('Origin',(0.0709664804794227,0.946426656566132,
-0.179042142893574));
#158071=CARTESIAN_POINT('',(-1.64369966596779,0.940053948010708,7.31766707464516));
#158072=CARTESIAN_POINT('Origin',(0.0629454791960926,0.803583969908237,
-0.180826038645768));
#158073=CARTESIAN_POINT('Origin',(0.0432520105150996,0.94642927386581,-0.187915429956872));
#158074=CARTESIAN_POINT('Ctrl Pts',(-2.117720602,1.070162746,6.933812764));
#158075=CARTESIAN_POINT('Ctrl Pts',(-1.741994603,1.005280647,7.048566756));
#158076=CARTESIAN_POINT('Ctrl Pts',(-1.356068566,0.940053947,7.122048725));
#158077=CARTESIAN_POINT('Ctrl Pts',(-1.34280389759946,0.937812039319745,
7.12457437462911));
#158078=CARTESIAN_POINT('Ctrl Pts',(-1.32953922919893,0.935570131639477,
7.12710002425809));
#158079=CARTESIAN_POINT('Ctrl Pts',(-2.42543142519539,1.070162746,7.0975379173685));
#158080=CARTESIAN_POINT('Ctrl Pts',(-2.04083356844032,1.005280647,7.2289659894335));
#158081=CARTESIAN_POINT('Ctrl Pts',(-1.64428585988024,0.940053947,7.31806573416641));
#158082=CARTESIAN_POINT('Ctrl Pts',(-1.63065611388038,0.937812039319745,
7.32112818255068));
#158083=CARTESIAN_POINT('Ctrl Pts',(-1.61702636788052,0.935570131639477,
7.32419063093486));
#158084=CARTESIAN_POINT('',(-1.49988410426394,0.940053949937996,7.21985790168456));
#158085=CARTESIAN_POINT('Ctrl Pts',(-1.356068566,0.940053947,7.122048725));
#158086=CARTESIAN_POINT('Ctrl Pts',(-0.965075178000001,1.005711878,7.19649554));
#158087=CARTESIAN_POINT('Ctrl Pts',(-0.568281989,1.070155008,7.227693656));
#158088=CARTESIAN_POINT('Ctrl Pts',(-1.16045022,0.940053947,7.409679837));
#158089=CARTESIAN_POINT('Ctrl Pts',(-0.75366617,1.005711878,7.473387399));
#158090=CARTESIAN_POINT('Ctrl Pts',(-0.342352821,1.070155008,7.49218222900001));
#158091=CARTESIAN_POINT('',(-1.16045021294829,0.940053946884191,7.40967983939926));
#158092=CARTESIAN_POINT('',(-0.594913062081684,1.03040248135913,7.4763679983408));
#158093=CARTESIAN_POINT('Origin',(0.0501923127855627,0.803673966063474,
-0.179678925408648));
#158094=CARTESIAN_POINT('Ctrl Pts',(-0.572986203044213,1.06939092119402,
7.22732224375387));
#158095=CARTESIAN_POINT('Ctrl Pts',(-0.576684369626288,1.06258635141026,
7.26876929900361));
#158096=CARTESIAN_POINT('Ctrl Pts',(-0.580360792552439,1.05593965225368,
7.31026810206519));
#158097=CARTESIAN_POINT('Ctrl Pts',(-0.587666952126212,1.04295319907133,
7.39327085176534));
#158098=CARTESIAN_POINT('Ctrl Pts',(-0.591300604526767,1.0366064853031,
7.43481934128274));
#158099=CARTESIAN_POINT('Ctrl Pts',(-0.59491306336725,1.03040248136352,
7.47636799821832));
#158100=CARTESIAN_POINT('',(-1.25825939098333,0.940053946665902,7.26586428134924));
#158101=CARTESIAN_POINT('Origin',(2.16764201531848E-13,1.03148891300033,
-1.72735090120391E-12));
#158102=CARTESIAN_POINT('',(-0.598575745926003,0.849330499809727,7.4760756466581));
#158103=CARTESIAN_POINT('Origin',(0.0308185621203441,0.946426654691962,
-0.190111958654687));
#158104=CARTESIAN_POINT('',(-0.0321887715705101,0.940053948012013,7.49993092670776));
#158105=CARTESIAN_POINT('Origin',(0.0226016159826436,0.803583929116596,
-0.190129976591281));
#158106=CARTESIAN_POINT('Origin',(0.00184455323367208,0.946429300663522,
-0.192820044683663));
#158107=CARTESIAN_POINT('Ctrl Pts',(-0.577644689000001,1.070162746,7.226951405));
#158108=CARTESIAN_POINT('Ctrl Pts',(-0.186034238,1.005280647,7.25825252900001));
#158109=CARTESIAN_POINT('Ctrl Pts',(0.206665513,0.940053947,7.24705384));
#158110=CARTESIAN_POINT('Ctrl Pts',(0.220163000300406,0.937812039403535,
7.24666892974179));
#158111=CARTESIAN_POINT('Ctrl Pts',(0.233660487600805,0.935570131807057,
7.24628401948363));
#158112=CARTESIAN_POINT('Ctrl Pts',(-0.842965336257744,1.070162746,7.45299748588597));
#158113=CARTESIAN_POINT('Ctrl Pts',(-0.439106013265268,1.005280647,7.4986756722331));
#158114=CARTESIAN_POINT('Ctrl Pts',(-0.0326755574926569,0.940053947,7.50044627943826));
#158115=CARTESIAN_POINT('Ctrl Pts',(-0.0187061319931008,0.937812039403535,
7.50050713699725));
#158116=CARTESIAN_POINT('Ctrl Pts',(-0.00473670649354516,0.935570131807057,
7.50056799455627));
#158117=CARTESIAN_POINT('',(0.0872383841134713,0.940053949937996,7.37349238228569));
#158118=CARTESIAN_POINT('Ctrl Pts',(-0.575145653352384,4.94745154526473,
7.22714282422102));
#158119=CARTESIAN_POINT('Ctrl Pts',(-0.57356878941999,4.94771235963237,
7.22726762074545));
#158120=CARTESIAN_POINT('Ctrl Pts',(-0.571991925487597,4.947973174,7.22739241726988));
#158121=CARTESIAN_POINT('Ctrl Pts',(-0.414102629595647,4.97408817100001,
7.23988812788054));
#158122=CARTESIAN_POINT('Ctrl Pts',(-0.255818264017313,5.00031307,7.24547672211003));
#158123=CARTESIAN_POINT('Ctrl Pts',(-0.527285648139283,4.94745154526473,
7.28327884871706));
#158124=CARTESIAN_POINT('Ctrl Pts',(-0.525696541069641,4.94771235963237,
7.28339319785853));
#158125=CARTESIAN_POINT('Ctrl Pts',(-0.524107434,4.947973174,7.28350754700001));
#158126=CARTESIAN_POINT('Ctrl Pts',(-0.364992249,4.97408817100001,7.294957175));
#158127=CARTESIAN_POINT('Ctrl Pts',(-0.205528848,5.00031307,7.299447149));
#158128=CARTESIAN_POINT('Origin',(-0.0077921681403096,5.08925695568899,
-0.196936015308897));
#158129=CARTESIAN_POINT('',(-0.500739504532107,4.94797317561532,7.31089209031288));
#158130=CARTESIAN_POINT('Ctrl Pts',(-0.622179465,4.94766207,7.268458786));
#158131=CARTESIAN_POINT('Ctrl Pts',(-0.462446769,4.973931887,7.282131892));
#158132=CARTESIAN_POINT('Ctrl Pts',(-0.30226761,5.00031307,7.288774568));
#158133=CARTESIAN_POINT('Ctrl Pts',(-0.573864989,4.94766207,7.227252519));
#158134=CARTESIAN_POINT('Ctrl Pts',(-0.415037848,4.973931887,7.239863859));
#158135=CARTESIAN_POINT('Ctrl Pts',(-0.255810014,5.00031307,7.24548557600001));
#158136=CARTESIAN_POINT('Ctrl Pts',(-0.571982121404791,4.94797287213543,
7.22740188220303));
#158137=CARTESIAN_POINT('Ctrl Pts',(-0.572436165542444,4.94882769742138,
7.23260489888446));
#158138=CARTESIAN_POINT('Ctrl Pts',(-0.572889190404426,4.94967947054502,
7.23780850677221));
#158139=CARTESIAN_POINT('Ctrl Pts',(-0.573343134511853,4.9505285274177,
7.24301247656969));
#158140=CARTESIAN_POINT('Ctrl Pts',(-0.573764558557747,4.95131675878061,
7.24784363963775));
#158141=CARTESIAN_POINT('Ctrl Pts',(-0.574186775096978,4.95210264917475,
7.25267511613723));
#158142=CARTESIAN_POINT('Ctrl Pts',(-0.574609775307212,4.95288622030903,
7.25750689950655));
#158143=CARTESIAN_POINT('Ctrl Pts',(-0.575032775944805,4.95366979223496,
7.26233868775745));
#158144=CARTESIAN_POINT('Ctrl Pts',(-0.575456560362438,4.95445104509375,
7.26717078409749));
#158145=CARTESIAN_POINT('Ctrl Pts',(-0.575881119919221,4.95523000034009,
7.27200318231908));
#158146=CARTESIAN_POINT('Ctrl Pts',(-0.853730891,5.000313899,7.244911592));
#158147=CARTESIAN_POINT('Ctrl Pts',(-0.742882782,4.98224132,7.257973788));
#158148=CARTESIAN_POINT('Ctrl Pts',(-0.631686945,4.964285714,7.267638682));
#158149=CARTESIAN_POINT('Ctrl Pts',(-0.580289944,4.955986264,7.27210599500001));
#158150=CARTESIAN_POINT('Ctrl Pts',(-0.528834902,4.947660853,7.275845934));
#158151=CARTESIAN_POINT('Ctrl Pts',(-0.892761299,5.000313899,7.194822949));
#158152=CARTESIAN_POINT('Ctrl Pts',(-0.782679553,4.98224132,7.20848231500001));
#158153=CARTESIAN_POINT('Ctrl Pts',(-0.672231452,4.964285714,7.218767545));
#158154=CARTESIAN_POINT('Ctrl Pts',(-0.621180069,4.955986264,7.22352159));
#158155=CARTESIAN_POINT('Ctrl Pts',(-0.570066555,4.947660853,7.227553121));
#158156=CARTESIAN_POINT('Ctrl Pts',(-0.571983137701933,4.94797303766448,
7.22740180177));
#158157=CARTESIAN_POINT('Ctrl Pts',(-0.605444395477702,4.95342302831041,
7.22475356782426));
#158158=CARTESIAN_POINT('Ctrl Pts',(-0.638862058334151,4.95886083424197,
7.22187499458713));
#158159=CARTESIAN_POINT('Ctrl Pts',(-0.672231451656842,4.96428571396197,
7.21876754515345));
#158160=CARTESIAN_POINT('Ctrl Pts',(-0.745099376405782,4.97613189093767,
7.21198188447502));
#158161=CARTESIAN_POINT('Ctrl Pts',(-0.817988928543339,4.98803923900258,
7.20408107381268));
#158162=CARTESIAN_POINT('Ctrl Pts',(-0.890849230764476,5.00000000015126,
7.19505994779791));
#158163=CARTESIAN_POINT('Ctrl Pts',(-0.892761299,5.000313899,7.194822949));
#158164=CARTESIAN_POINT('Ctrl Pts',(-0.782679553,4.98224132,7.20848231500001));
#158165=CARTESIAN_POINT('Ctrl Pts',(-0.672231452,4.964285714,7.218767545));
#158166=CARTESIAN_POINT('Ctrl Pts',(-0.622137718,4.95614194999999,7.223432411));
#158167=CARTESIAN_POINT('Ctrl Pts',(-0.57198407,4.947973174,7.227401623));
#158168=CARTESIAN_POINT('Ctrl Pts',(-0.950940418,5.000313899,7.240157672));
#158169=CARTESIAN_POINT('Ctrl Pts',(-0.840165045,4.98224132,7.254707187));
#158170=CARTESIAN_POINT('Ctrl Pts',(-0.728996408,4.964285714,7.265860928));
#158171=CARTESIAN_POINT('Ctrl Pts',(-0.678575876,4.95614194999999,7.270919708));
#158172=CARTESIAN_POINT('Ctrl Pts',(-0.628089994,4.947973174,7.27527826));
#158173=CARTESIAN_POINT('',(-0.655474541515816,4.94797317334227,7.29864619863935));
#158174=CARTESIAN_POINT('Ctrl Pts',(-1.537156899,4.81863040500001,7.245585413));
#158175=CARTESIAN_POINT('Ctrl Pts',(-1.528521258,4.820029867,7.247417471));
#158176=CARTESIAN_POINT('Ctrl Pts',(-1.519881274,4.821428571,7.24922894));
#158177=CARTESIAN_POINT('Ctrl Pts',(-1.132645864,4.884117105,7.33041714000001));
#158178=CARTESIAN_POINT('Ctrl Pts',(-0.738965005000001,4.947973174,7.369890775));
#158179=CARTESIAN_POINT('Ctrl Pts',(-1.355651883,4.81863040500001,7.12212805100001));
#158180=CARTESIAN_POINT('Ctrl Pts',(-1.347163385,4.820029867,7.12374378300001));
#158181=CARTESIAN_POINT('Ctrl Pts',(-1.338671059,4.821428571,7.125339276));
#158182=CARTESIAN_POINT('Ctrl Pts',(-0.95805352,4.884117105,7.196847686));
#158183=CARTESIAN_POINT('Ctrl Pts',(-0.57198407,4.947973174,7.227401623));
#158184=CARTESIAN_POINT('Ctrl Pts',(-1.35103832261869,4.81939091791739,
7.12300468506627));
#158185=CARTESIAN_POINT('Ctrl Pts',(-1.35423171894372,4.82234724740109,
7.14079909641026));
#158186=CARTESIAN_POINT('Ctrl Pts',(-1.3574262227148,4.82527010320382,7.15859892100757));
#158187=CARTESIAN_POINT('Ctrl Pts',(-1.36063744721484,4.82816321756001,
7.17640053315189));
#158188=CARTESIAN_POINT('Ctrl Pts',(-1.36364364406067,4.83087161470014,
7.19306556241983));
#158189=CARTESIAN_POINT('Ctrl Pts',(-1.36666047782763,4.83355328556713,
7.20973303985136));
#158190=CARTESIAN_POINT('Ctrl Pts',(-1.36968750153964,4.83620904390085,
7.22640277020807));
#158191=CARTESIAN_POINT('Ctrl Pts',(-1.37271455775148,4.83886483074828,
7.24307267954037));
#158192=CARTESIAN_POINT('Ctrl Pts',(-1.37575181232463,4.84149471141675,
7.25974488617966));
#158193=CARTESIAN_POINT('Ctrl Pts',(-1.37879884640616,4.84409946429526,
7.27641920768044));
#158194=CARTESIAN_POINT('Ctrl Pts',(-2.01675012375466,4.94924836941368,
7.12700095619442));
#158195=CARTESIAN_POINT('Ctrl Pts',(-2.01288868187733,4.94861077170684,
7.12808912409721));
#158196=CARTESIAN_POINT('Ctrl Pts',(-2.00902724,4.94797317400001,7.129177292));
#158197=CARTESIAN_POINT('Ctrl Pts',(-1.620660636,4.88384644,7.238620367));
#158198=CARTESIAN_POINT('Ctrl Pts',(-1.222703557,4.818610636,7.30522794400001));
#158199=CARTESIAN_POINT('Ctrl Pts',(-2.11980215310686,4.94924836941368,
6.93318112482194));
#158200=CARTESIAN_POINT('Ctrl Pts',(-2.11604563105343,4.94861077170684,
6.93432522341097));
#158201=CARTESIAN_POINT('Ctrl Pts',(-2.112289109,4.94797317400001,6.935469322));
#158202=CARTESIAN_POINT('Ctrl Pts',(-1.734474873,4.88384644,7.050537656));
#158203=CARTESIAN_POINT('Ctrl Pts',(-1.346396652,4.818610636,7.123883495));
#158204=CARTESIAN_POINT('',(-2.09494101683223,4.94797317334255,6.96801245134783));
#158205=CARTESIAN_POINT('Ctrl Pts',(-2.1153154539966,4.94745154526473,6.93454760851299));
#158206=CARTESIAN_POINT('Ctrl Pts',(-2.1138022814983,4.94771235963237,6.93500846525649));
#158207=CARTESIAN_POINT('Ctrl Pts',(-2.112289109,4.947973174,6.935469322));
#158208=CARTESIAN_POINT('Ctrl Pts',(-1.960777152,4.974088171,6.981614297));
#158209=CARTESIAN_POINT('Ctrl Pts',(-1.807394542,5.00031307,7.021098559));
#158210=CARTESIAN_POINT('Ctrl Pts',(-2.0806476628918,4.94745154526474,6.99964900947169));
#158211=CARTESIAN_POINT('Ctrl Pts',(-2.0791202899459,4.94771235963237,7.00010229623584));
#158212=CARTESIAN_POINT('Ctrl Pts',(-2.077592917,4.947973174,7.00055558299999));
#158213=CARTESIAN_POINT('Ctrl Pts',(-1.924659088,4.974088171,7.04594258599999));
#158214=CARTESIAN_POINT('Ctrl Pts',(-1.769889065,5.00031307,7.084607504));
#158215=CARTESIAN_POINT('Origin',(0.0347258367496797,5.08925692701997,-0.194008213182874));
#158216=CARTESIAN_POINT('Ctrl Pts',(-2.17013704,4.94766207,6.964776065));
#158217=CARTESIAN_POINT('Ctrl Pts',(-2.017078119,4.973931887,7.012467309));
#158218=CARTESIAN_POINT('Ctrl Pts',(-1.862071839,5.00031307,7.053388468));
#158219=CARTESIAN_POINT('Ctrl Pts',(-2.114094,4.94766207,6.934919362));
#158220=CARTESIAN_POINT('Ctrl Pts',(-1.961691214,4.973931887,6.981378996));
#158221=CARTESIAN_POINT('Ctrl Pts',(-1.807394542,5.00031307,7.021098559));
#158222=CARTESIAN_POINT('Ctrl Pts',(-2.11228726159542,4.94797287202588,
6.93546999405279));
#158223=CARTESIAN_POINT('Ctrl Pts',(-2.11384918555808,4.94882769739943,
6.94045376112391));
#158224=CARTESIAN_POINT('Ctrl Pts',(-2.11541024084986,4.94967947054799,
6.94543832469033));
#158225=CARTESIAN_POINT('Ctrl Pts',(-2.11697227168855,4.95052852744352,
6.95042304407898));
#158226=CARTESIAN_POINT('Ctrl Pts',(-2.11842240029988,4.9513167588064,6.95505066347414));
#158227=CARTESIAN_POINT('Ctrl Pts',(-2.11987337024825,4.95210264919842,
6.95967841859454));
#158228=CARTESIAN_POINT('Ctrl Pts',(-2.12132517151473,4.95288622033075,
6.96430630494391));
#158229=CARTESIAN_POINT('Ctrl Pts',(-2.12277697424796,4.95366979225473,
6.96893419596886));
#158230=CARTESIAN_POINT('Ctrl Pts',(-2.12422960866792,4.95445104511177,
6.97356221939012));
#158231=CARTESIAN_POINT('Ctrl Pts',(-2.12568306502001,4.95523000036473,
6.97819037105365));
#158232=CARTESIAN_POINT('Ctrl Pts',(-2.391212971,5.000313899,6.89200268));
#158233=CARTESIAN_POINT('Ctrl Pts',(-2.285764415,4.98224132,6.928588556));
#158234=CARTESIAN_POINT('Ctrl Pts',(-2.179245942,4.964285714,6.961931308));
#158235=CARTESIAN_POINT('Ctrl Pts',(-2.130010915,4.955986264,6.977343013));
#158236=CARTESIAN_POINT('Ctrl Pts',(-2.080562839,4.947660853,6.992056828));
#158237=CARTESIAN_POINT('Ctrl Pts',(-2.418563293,5.000313899,6.834694697));
#158238=CARTESIAN_POINT('Ctrl Pts',(-2.313991557,4.98224132,6.871699036));
#158239=CARTESIAN_POINT('Ctrl Pts',(-2.208336691,4.964285714,6.905486881));
#158240=CARTESIAN_POINT('Ctrl Pts',(-2.159500841,4.955986264,6.921104317));
#158241=CARTESIAN_POINT('Ctrl Pts',(-2.110448992,4.947660853,6.936029488));
#158242=CARTESIAN_POINT('Ctrl Pts',(-2.112289109,4.947973174,6.93546932199999));
#158243=CARTESIAN_POINT('Ctrl Pts',(-2.14439727935191,4.9534229210678,6.92569035367246));
#158244=CARTESIAN_POINT('Ctrl Pts',(-2.17641514247988,4.95886077964643,
6.91569521664372));
#158245=CARTESIAN_POINT('Ctrl Pts',(-2.20833669130953,4.9642857140526,6.90548688090102));
#158246=CARTESIAN_POINT('Ctrl Pts',(-2.27804228996723,4.97613189126059,
6.88319541385734));
#158247=CARTESIAN_POINT('Ctrl Pts',(-2.34752928232983,4.98803923902554,
6.85981022134622));
#158248=CARTESIAN_POINT('Ctrl Pts',(-2.41674687579387,5.00000000018585,
6.83533719297713));
#158249=CARTESIAN_POINT('Ctrl Pts',(-2.418563293,5.000313899,6.834694697));
#158250=CARTESIAN_POINT('Ctrl Pts',(-2.313991557,4.98224132,6.871699036));
#158251=CARTESIAN_POINT('Ctrl Pts',(-2.208336691,4.964285714,6.905486881));
#158252=CARTESIAN_POINT('Ctrl Pts',(-2.16041693,4.95614194999999,6.920811357));
#158253=CARTESIAN_POINT('Ctrl Pts',(-2.112289109,4.947973174,6.93546932199999));
#158254=CARTESIAN_POINT('Ctrl Pts',(-2.485127842,5.000313899,6.866462729));
#158255=CARTESIAN_POINT('Ctrl Pts',(-2.380070051,4.98224132,6.904485514));
#158256=CARTESIAN_POINT('Ctrl Pts',(-2.2738982,4.964285714,6.939276459));
#158257=CARTESIAN_POINT('Ctrl Pts',(-2.22574396,4.95614194999999,6.95505589100001));
#158258=CARTESIAN_POINT('Ctrl Pts',(-2.177375369,4.947973174,6.970165514));
#158259=CARTESIAN_POINT('',(-2.20914309734462,4.94797317334223,6.98710025528443));
#158260=CARTESIAN_POINT('Ctrl Pts',(-3.058805711,4.81863040500001,6.745744357));
#158261=CARTESIAN_POINT('Ctrl Pts',(-3.050765805,4.820029867,6.749389991));
#158262=CARTESIAN_POINT('Ctrl Pts',(-3.042717231,4.821428571,6.753016449));
#158263=CARTESIAN_POINT('Ctrl Pts',(-2.681988233,4.884117105,6.915550681));
#158264=CARTESIAN_POINT('Ctrl Pts',(-2.305997078,4.947973174,7.03873119100001));
#158265=CARTESIAN_POINT('Ctrl Pts',(-2.855004498,4.81863040500001,6.664191573));
#158266=CARTESIAN_POINT('Ctrl Pts',(-2.84706179,4.820029867,6.667594306));
#158267=CARTESIAN_POINT('Ctrl Pts',(-2.839110994,4.821428571,6.670978097));
#158268=CARTESIAN_POINT('Ctrl Pts',(-2.482764276,4.884117105,6.82263620000001));
#158269=CARTESIAN_POINT('Ctrl Pts',(-2.112289109,4.947973174,6.935469322));
#158270=CARTESIAN_POINT('Ctrl Pts',(-2.85068725011375,4.81939091791738,
6.66603949042913));
#158271=CARTESIAN_POINT('Ctrl Pts',(-2.85763125915416,4.82234724729619,
6.68273139310464));
#158272=CARTESIAN_POINT('Ctrl Pts',(-2.8645775133876,4.82527010313846,6.69942834382324));
#158273=CARTESIAN_POINT('Ctrl Pts',(-2.87154048165056,4.8281632175241,6.71612344585626));
#158274=CARTESIAN_POINT('Ctrl Pts',(-2.87805888394757,4.83087161468242,
6.73175261251785));
#158275=CARTESIAN_POINT('Ctrl Pts',(-2.88458820076314,4.83355328556657,
6.74738188348297));
#158276=CARTESIAN_POINT('Ctrl Pts',(-2.8911279536013,4.83620904391647,6.76301116416415));
#158277=CARTESIAN_POINT('Ctrl Pts',(-2.89766777665392,4.8388648307801,6.77864061265008));
#158278=CARTESIAN_POINT('Ctrl Pts',(-2.90421805348943,4.8414947114638,6.79427011238702));
#158279=CARTESIAN_POINT('Ctrl Pts',(-2.91077833579864,4.84409946434516,
6.80989957516688));
#158280=CARTESIAN_POINT('Ctrl Pts',(-3.50169415916581,4.94924836941368,
6.52683397198676));
#158281=CARTESIAN_POINT('Ctrl Pts',(-3.49815691958291,4.94861077170685,
6.52872679499338));
#158282=CARTESIAN_POINT('Ctrl Pts',(-3.49461968,4.947973174,6.530619618));
#158283=CARTESIAN_POINT('Ctrl Pts',(-3.138859897,4.88384644,6.72099131500001));
#158284=CARTESIAN_POINT('Ctrl Pts',(-2.764525494,4.818610636,6.871590653));
#158285=CARTESIAN_POINT('Ctrl Pts',(-3.56067135454208,4.94924836941368,
6.31539240121984));
#158286=CARTESIAN_POINT('Ctrl Pts',(-3.55724860527104,4.94861077170685,
6.31731729260992));
#158287=CARTESIAN_POINT('Ctrl Pts',(-3.553825856,4.947973174,6.319242184));
#158288=CARTESIAN_POINT('Ctrl Pts',(-3.209580998,4.88384644,6.51283917600001));
#158289=CARTESIAN_POINT('Ctrl Pts',(-2.846343018,4.818610636,6.66789557700001));
#158290=CARTESIAN_POINT('',(-3.54387916349532,4.94797317334249,6.35475380005075));
#158291=CARTESIAN_POINT('Ctrl Pts',(-3.55658330557724,4.94745154526473,
6.31769144495039));
#158292=CARTESIAN_POINT('Ctrl Pts',(-3.55520458078862,4.94771235963237,
6.31846681447519));
#158293=CARTESIAN_POINT('Ctrl Pts',(-3.553825856,4.947973174,6.319242184));
#158294=CARTESIAN_POINT('Ctrl Pts',(-3.41577597,4.97408817100001,6.396878907));
#158295=CARTESIAN_POINT('Ctrl Pts',(-3.27446731,5.00031307,6.468412776));
#158296=CARTESIAN_POINT('Ctrl Pts',(-3.53672090509896,4.94745154526473,
6.38872336160057));
#158297=CARTESIAN_POINT('Ctrl Pts',(-3.53532668454948,4.94771235963237,
6.38949439080029));
#158298=CARTESIAN_POINT('Ctrl Pts',(-3.533932464,4.947973174,6.39026542));
#158299=CARTESIAN_POINT('Ctrl Pts',(-3.394331008,4.97408817100001,6.467467552));
#158300=CARTESIAN_POINT('Ctrl Pts',(-3.251491236,5.00031307,6.538499487));
#158301=CARTESIAN_POINT('Origin',(0.075620165187994,5.08925701702758,-0.182007724103123));
#158302=CARTESIAN_POINT('Ctrl Pts',(-3.616621419,4.94766207,6.33542815600001));
#158303=CARTESIAN_POINT('Ctrl Pts',(-3.477393138,4.973931887,6.414907549));
#158304=CARTESIAN_POINT('Ctrl Pts',(-3.334807658,5.00031307,6.488193762));
#158305=CARTESIAN_POINT('Ctrl Pts',(-3.555470326,4.94766207,6.318317083));
#158306=CARTESIAN_POINT('Ctrl Pts',(-3.41661808,4.973931887,6.39645261100001));
#158307=CARTESIAN_POINT('Ctrl Pts',(-3.27446731,5.00031307,6.468412776));
#158308=CARTESIAN_POINT('Ctrl Pts',(-3.55382419701178,4.94797287199161,
6.31924323720788));
#158309=CARTESIAN_POINT('Ctrl Pts',(-3.55642096691804,4.94882769743475,
6.32377471888897));
#158310=CARTESIAN_POINT('Ctrl Pts',(-3.55901705931681,4.94967947057971,
6.32830716537846));
#158311=CARTESIAN_POINT('Ctrl Pts',(-3.56161413796261,4.95052852746963,
6.33283955432302));
#158312=CARTESIAN_POINT('Ctrl Pts',(-3.56402516469487,4.95131675883958,
6.33704724781126));
#158313=CARTESIAN_POINT('Ctrl Pts',(-3.56643704228009,4.95210264923673,
6.34125489297957));
#158314=CARTESIAN_POINT('Ctrl Pts',(-3.56884975996899,4.95288622037288,
6.34546248759392));
#158315=CARTESIAN_POINT('Ctrl Pts',(-3.57126248009547,4.95366979230068,
6.34967008645925));
#158316=CARTESIAN_POINT('Ctrl Pts',(-3.57367604093657,4.95445104516023,
6.35387763583144));
#158317=CARTESIAN_POINT('Ctrl Pts',(-3.57609043208675,4.9552300004188,6.35808513377476));
#158318=CARTESIAN_POINT('Ctrl Pts',(-3.816884591,5.000313899,6.216831382));
#158319=CARTESIAN_POINT('Ctrl Pts',(-3.721766245,4.98224132,6.275230223));
#158320=CARTESIAN_POINT('Ctrl Pts',(-3.624905821,4.964285714,6.330691763));
#158321=CARTESIAN_POINT('Ctrl Pts',(-3.580134942,4.955986264,6.356327227));
#158322=CARTESIAN_POINT('Ctrl Pts',(-3.53500597,4.947660853,6.381326915));
#158323=CARTESIAN_POINT('Ctrl Pts',(-3.831275955,5.000313899,6.154983717));
#158324=CARTESIAN_POINT('Ctrl Pts',(-3.737103887,4.98224132,6.213602748));
#158325=CARTESIAN_POINT('Ctrl Pts',(-3.641182561,4.964285714,6.269313324));
#158326=CARTESIAN_POINT('Ctrl Pts',(-3.596845753,4.955986264,6.295063898));
#158327=CARTESIAN_POINT('Ctrl Pts',(-3.55214918,4.947660853,6.320184824));
#158328=CARTESIAN_POINT('Ctrl Pts',(-3.55382585665352,4.9479731737983,6.31924218509526));
#158329=CARTESIAN_POINT('Ctrl Pts',(-3.60037619299507,4.95664467837811,
6.29306313140172));
#158330=CARTESIAN_POINT('Ctrl Pts',(-3.64659716777283,4.9652738833346,6.26639280945056));
#158331=CARTESIAN_POINT('Ctrl Pts',(-3.7385464658405,4.98260085400305,6.21197461326868));
#158332=CARTESIAN_POINT('Ctrl Pts',(-3.7842501153838,4.99129109054103,6.18423872841419));
#158333=CARTESIAN_POINT('Ctrl Pts',(-3.82964012287192,5.00000000030332,
6.15600166741685));
#158334=CARTESIAN_POINT('Ctrl Pts',(-3.831275955,5.000313899,6.154983717));
#158335=CARTESIAN_POINT('Ctrl Pts',(-3.737103887,4.98224132,6.213602748));
#158336=CARTESIAN_POINT('Ctrl Pts',(-3.641182561,4.964285714,6.269313324));
#158337=CARTESIAN_POINT('Ctrl Pts',(-3.597677446,4.95614194999999,6.294580855));
#158338=CARTESIAN_POINT('Ctrl Pts',(-3.553825856,4.947973174,6.319242184));
#158339=CARTESIAN_POINT('Ctrl Pts',(-3.903113449,5.000313899,6.17169962));
#158340=CARTESIAN_POINT('Ctrl Pts',(-3.808685626,4.98224132,6.231417774));
#158341=CARTESIAN_POINT('Ctrl Pts',(-3.712475039,4.964285714,6.288219134));
#158342=CARTESIAN_POINT('Ctrl Pts',(-3.668838729,4.95614194999999,6.31398139));
#158343=CARTESIAN_POINT('Ctrl Pts',(-3.624849092,4.947973174,6.339135576));
#158344=CARTESIAN_POINT('',(-3.65951457699334,4.94797317334225,6.34884527048642));
#158345=CARTESIAN_POINT('Ctrl Pts',(-4.437428167,4.81863040500001,5.930479793));
#158346=CARTESIAN_POINT('Ctrl Pts',(-4.430359933,4.820029867,5.935768535));
#158347=CARTESIAN_POINT('Ctrl Pts',(-4.423279112,4.821428571,5.941040415));
#158348=CARTESIAN_POINT('Ctrl Pts',(-4.105923812,4.884117105,6.177320758));
#158349=CARTESIAN_POINT('Ctrl Pts',(-3.765203291,4.947973174,6.378448361));
#158350=CARTESIAN_POINT('Ctrl Pts',(-4.220860275,4.81863040500001,5.894644903));
#158351=CARTESIAN_POINT('Ctrl Pts',(-4.213834751,4.820029867,5.89967553000001));
#158352=CARTESIAN_POINT('Ctrl Pts',(-4.206797255,4.821428571,5.904689396));
#158353=CARTESIAN_POINT('Ctrl Pts',(-3.891383734,4.884117105,6.129405827));
#158354=CARTESIAN_POINT('Ctrl Pts',(-3.553825856,4.947973174,6.319242184));
#158355=CARTESIAN_POINT('Ctrl Pts',(-4.21704120998609,4.8193909177524,5.89737769849005));
#158356=CARTESIAN_POINT('Ctrl Pts',(-4.2274111371836,4.82234724726756,5.91218659723742));
#158357=CARTESIAN_POINT('Ctrl Pts',(-4.23778434295171,4.82527010313881,
5.92699994298082));
#158358=CARTESIAN_POINT('Ctrl Pts',(-4.24817347433187,4.82816321750719,
5.94180789041483));
#158359=CARTESIAN_POINT('Ctrl Pts',(-4.2578992888877,4.83087161465861,5.95567039204521));
#158360=CARTESIAN_POINT('Ctrl Pts',(-4.26763578520111,4.83355328553615,
5.96953064924705));
#158361=CARTESIAN_POINT('Ctrl Pts',(-4.2773824756305,4.83620904387986,5.98338867250614));
#158362=CARTESIAN_POINT('Ctrl Pts',(-4.28712927070582,4.83886483073728,
5.99724684455274));
#158363=CARTESIAN_POINT('Ctrl Pts',(-4.29688628617097,4.84149471141519,
6.01110281940253));
#158364=CARTESIAN_POINT('Ctrl Pts',(-4.30665306526583,4.84409946429903,
6.0249566073236));
#158365=CARTESIAN_POINT('Ctrl Pts',(-4.82290286777507,4.94924836941368,
5.62147948639974));
#158366=CARTESIAN_POINT('Ctrl Pts',(-4.81985522788753,4.94861077170684,
5.62408845819987));
#158367=CARTESIAN_POINT('Ctrl Pts',(-4.816807588,4.94797317400001,5.62669743));
#158368=CARTESIAN_POINT('Ctrl Pts',(-4.510289559,4.88384644,5.889096179));
#158369=CARTESIAN_POINT('Ctrl Pts',(-4.177081292,4.818610636,6.116645419));
#158370=CARTESIAN_POINT('Ctrl Pts',(-4.83504752209277,4.94924836941368,
5.40230294817827));
#158371=CARTESIAN_POINT('Ctrl Pts',(-4.83211858954639,4.94861077170684,
5.40491862658914));
#158372=CARTESIAN_POINT('Ctrl Pts',(-4.829189657,4.94797317400001,5.40753430500001));
#158373=CARTESIAN_POINT('Ctrl Pts',(-4.53461068300001,4.88384644,5.670607575));
#158374=CARTESIAN_POINT('Ctrl Pts',(-4.213197547,4.818610636,5.900124272));
#158375=CARTESIAN_POINT('',(-4.82710945999426,4.94797317334255,5.44435392384521));
#158376=CARTESIAN_POINT('Ctrl Pts',(-4.83154927588509,4.94745154526473,
5.40542705122461));
#158377=CARTESIAN_POINT('Ctrl Pts',(-4.83036946644255,4.94771235963237,
5.4064806781123));
#158378=CARTESIAN_POINT('Ctrl Pts',(-4.829189657,4.947973174,5.40753430500001));
#158379=CARTESIAN_POINT('Ctrl Pts',(-4.711056901,4.974088171,5.51303256900001));
#158380=CARTESIAN_POINT('Ctrl Pts',(-4.588429626,5.00031307,5.613271201));
#158381=CARTESIAN_POINT('Ctrl Pts',(-4.82742100891798,4.94745154526473,
5.47906810964861));
#158382=CARTESIAN_POINT('Ctrl Pts',(-4.82622513295899,4.94771235963237,
5.4801208288243));
#158383=CARTESIAN_POINT('Ctrl Pts',(-4.825029257,4.947973174,5.481173548));
#158384=CARTESIAN_POINT('Ctrl Pts',(-4.705287782,4.974088171,5.586580924));
#158385=CARTESIAN_POINT('Ctrl Pts',(-4.581057291,5.00031307,5.6866585));
#158386=CARTESIAN_POINT('Origin',(0.11297875860618,5.08925694774986,-0.161496694229351));
#158387=CARTESIAN_POINT('Ctrl Pts',(-4.893996599,4.94766207,5.409842668));
#158388=CARTESIAN_POINT('Ctrl Pts',(-4.775109118,4.97393188700001,5.517393842));
#158389=CARTESIAN_POINT('Ctrl Pts',(-4.651611577,5.00031307,5.619618328));
#158390=CARTESIAN_POINT('Ctrl Pts',(-4.83059681,4.94766207,5.40627732));
#158391=CARTESIAN_POINT('Ctrl Pts',(-4.711787681,4.97393188700001,5.512435211));
#158392=CARTESIAN_POINT('Ctrl Pts',(-4.588429626,5.00031307,5.613271201));
#158393=CARTESIAN_POINT('Ctrl Pts',(-4.82918826277984,4.94797287201526,
5.40753569026454));
#158394=CARTESIAN_POINT('Ctrl Pts',(-4.83269845602471,4.94882769741037,
5.41140299956885));
#158395=CARTESIAN_POINT('Ctrl Pts',(-4.83620819522548,4.94967947055171,
5.41527139680809));
#158396=CARTESIAN_POINT('Ctrl Pts',(-4.83971888527368,4.95052852743952,
5.41913952584698));
#158397=CARTESIAN_POINT('Ctrl Pts',(-4.84297807326694,4.9513167588061,5.42273054628652));
#158398=CARTESIAN_POINT('Ctrl Pts',(-4.84623808186077,4.95210264920189,
5.42632133664188));
#158399=CARTESIAN_POINT('Ctrl Pts',(-4.84949890005566,4.95288622033443,
5.42991189702264));
#158400=CARTESIAN_POINT('Ctrl Pts',(-4.85275972154501,4.95366979225863,
5.433502461031));
#158401=CARTESIAN_POINT('Ctrl Pts',(-4.8560213534601,4.95445104511235,5.43709279596945));
#158402=CARTESIAN_POINT('Ctrl Pts',(-4.8592837852266,4.95523000036476,5.44068290219272));
#158403=CARTESIAN_POINT('Ctrl Pts',(-5.064082929,5.000313899,5.250967958));
#158404=CARTESIAN_POINT('Ctrl Pts',(-4.983742422,4.98224132,5.328449099));
#158405=CARTESIAN_POINT('Ctrl Pts',(-4.901069133,4.964285714,5.403436108));
#158406=CARTESIAN_POINT('Ctrl Pts',(-4.862855839,4.955986264,5.438096644));
#158407=CARTESIAN_POINT('Ctrl Pts',(-4.824156151,4.947660853,5.472213249));
#158408=CARTESIAN_POINT('Ctrl Pts',(-5.064842411,5.000313899,5.18747254));
#158409=CARTESIAN_POINT('Ctrl Pts',(-4.985473393,4.98224132,5.264965301));
#158410=CARTESIAN_POINT('Ctrl Pts',(-4.903770781,4.964285714,5.339993645));
#158411=CARTESIAN_POINT('Ctrl Pts',(-4.866006155,4.955986264,5.374673287));
#158412=CARTESIAN_POINT('Ctrl Pts',(-4.82775482,4.947660853,5.408815342));
#158413=CARTESIAN_POINT('Ctrl Pts',(-4.82918900301269,4.94797303315607,
5.40753502919794));
#158414=CARTESIAN_POINT('Ctrl Pts',(-4.85422464232958,4.95342302537021,
5.3851768922145));
#158415=CARTESIAN_POINT('Ctrl Pts',(-4.87908618026873,4.95886083280405,
5.36266176634008));
#158416=CARTESIAN_POINT('Ctrl Pts',(-4.90377078123183,4.9642857140524,5.33999364493616));
#158417=CARTESIAN_POINT('Ctrl Pts',(-4.95767392528497,4.97613189121847,
5.29049383644634));
#158418=CARTESIAN_POINT('Ctrl Pts',(-5.01091942444511,4.98803923906662,
5.24009317944469));
#158419=CARTESIAN_POINT('Ctrl Pts',(-5.06346365273142,5.00000000024774,
5.18881834708339));
#158420=CARTESIAN_POINT('Ctrl Pts',(-5.064842411,5.000313899,5.18747254));
#158421=CARTESIAN_POINT('Ctrl Pts',(-4.985473393,4.98224132,5.264965301));
#158422=CARTESIAN_POINT('Ctrl Pts',(-4.903770781,4.964285714,5.339993645));
#158423=CARTESIAN_POINT('Ctrl Pts',(-4.866714564,4.95614194999999,5.374022748));
#158424=CARTESIAN_POINT('Ctrl Pts',(-4.829189657,4.947973174,5.40753430500001));
#158425=CARTESIAN_POINT('Ctrl Pts',(-5.13859381,5.000313899,5.188354696));
#158426=CARTESIAN_POINT('Ctrl Pts',(-5.059211294,4.98224132,5.266975863));
#158427=CARTESIAN_POINT('Ctrl Pts',(-4.977460671,4.964285714,5.343131672));
#158428=CARTESIAN_POINT('Ctrl Pts',(-4.940382678,4.95614194999999,5.377672137));
#158429=CARTESIAN_POINT('Ctrl Pts',(-4.9028289,4.947973174,5.41169470400001));
#158430=CARTESIAN_POINT('',(-4.93877122247881,4.94797317334225,5.41372533678253));
#158431=CARTESIAN_POINT('Ctrl Pts',(-5.608561414,4.818630405,4.83791258399999));
#158432=CARTESIAN_POINT('Ctrl Pts',(-5.602795355,4.820029867,4.844597141));
#158433=CARTESIAN_POINT('Ctrl Pts',(-5.597013377,4.821428571,4.851267933));
#158434=CARTESIAN_POINT('Ctrl Pts',(-5.337870958,4.884117105,5.150246182));
#158435=CARTESIAN_POINT('Ctrl Pts',(-5.048352782,4.947973174,5.419916374));
#158436=CARTESIAN_POINT('Ctrl Pts',(-5.389353317,4.818630405,4.84947119));
#158437=CARTESIAN_POINT('Ctrl Pts',(-5.383573482,4.820029867,4.855894483));
#158438=CARTESIAN_POINT('Ctrl Pts',(-5.377778351,4.821428571,4.862303981));
#158439=CARTESIAN_POINT('Ctrl Pts',(-5.118046414,4.884117105,5.14957125100001));
#158440=CARTESIAN_POINT('Ctrl Pts',(-4.829189657,4.947973174,5.407534305));
#158441=CARTESIAN_POINT('Ctrl Pts',(-5.38621101020249,4.8193909179172,4.85296107987876));
#158442=CARTESIAN_POINT('Ctrl Pts',(-5.39952197013658,4.82234724738473,
4.86519452629106));
#158443=CARTESIAN_POINT('Ctrl Pts',(-5.41283708726114,4.82527010318465,
4.87743161198874));
#158444=CARTESIAN_POINT('Ctrl Pts',(-5.42616659749074,4.82816321755476,
4.88966000170456));
#158445=CARTESIAN_POINT('Ctrl Pts',(-5.43864505593992,4.8308716147002,4.90110764309131));
#158446=CARTESIAN_POINT('Ctrl Pts',(-5.45113346393274,4.83355328557171,
4.91255079625502));
#158447=CARTESIAN_POINT('Ctrl Pts',(-5.46363134748182,4.83620904390926,
4.92398957626564));
#158448=CARTESIAN_POINT('Ctrl Pts',(-5.47612936521519,4.83886483076053,
4.93542847908943));
#158449=CARTESIAN_POINT('Ctrl Pts',(-5.48863689206368,4.84149471143217,
4.94686303899888));
#158450=CARTESIAN_POINT('Ctrl Pts',(-5.50115348427103,4.8440994643342,4.9582933643208));
#158451=CARTESIAN_POINT('Ctrl Pts',(-5.91859799888375,4.94924836941368,
4.45327086703888));
#158452=CARTESIAN_POINT('Ctrl Pts',(-5.91618246294187,4.94861077170684,
4.45647399501944));
#158453=CARTESIAN_POINT('Ctrl Pts',(-5.913766927,4.94797317400001,4.459677123));
#158454=CARTESIAN_POINT('Ctrl Pts',(-5.670823094,4.88384644,4.781833451));
#158455=CARTESIAN_POINT('Ctrl Pts',(-5.394321411,4.818610636,5.07569264400001));
#158456=CARTESIAN_POINT('Ctrl Pts',(-5.88334224037081,4.94924836941368,
4.23660781253323));
#158457=CARTESIAN_POINT('Ctrl Pts',(-5.8810440781854,4.94861077170684,4.23979197176662));
#158458=CARTESIAN_POINT('Ctrl Pts',(-5.878745916,4.94797317400001,4.242976131));
#158459=CARTESIAN_POINT('Ctrl Pts',(-5.647607012,4.88384644,4.563224667));
#158460=CARTESIAN_POINT('Ctrl Pts',(-5.383047642,4.818610636,4.85646971400001));
#158461=CARTESIAN_POINT('',(-5.88462948285355,4.94797317334255,4.2793821087636));
#158462=CARTESIAN_POINT('Ctrl Pts',(-5.88059737102393,4.94745154526473,
4.24041089533189));
#158463=CARTESIAN_POINT('Ctrl Pts',(-5.87967164351197,4.94771235963237,
4.24169351316595));
#158464=CARTESIAN_POINT('Ctrl Pts',(-5.878745916,4.947973174,4.242976131));
#158465=CARTESIAN_POINT('Ctrl Pts',(-5.786054047,4.974088171,4.371402955));
#158466=CARTESIAN_POINT('Ctrl Pts',(-5.687842072,5.00031307,4.495659303));
#158467=CARTESIAN_POINT('Ctrl Pts',(-5.8923962720813,4.94745154526473,4.31321772265892));
#158468=CARTESIAN_POINT('Ctrl Pts',(-5.89145465854065,4.94771235963237,
4.31450290782946));
#158469=CARTESIAN_POINT('Ctrl Pts',(-5.890513045,4.947973174,4.315788093));
#158470=CARTESIAN_POINT('Ctrl Pts',(-5.796230529,4.974088171,4.444471981));
#158471=CARTESIAN_POINT('Ctrl Pts',(-5.696418198,5.00031307,4.568915682));
#158472=CARTESIAN_POINT('Origin',(0.145053772061448,5.08925682528172,-0.133433391065872));
#158473=CARTESIAN_POINT('Ctrl Pts',(-5.942533939,4.94766207,4.23129895));
#158474=CARTESIAN_POINT('Ctrl Pts',(-5.849546304,4.97393188700001,4.361892931));
#158475=CARTESIAN_POINT('Ctrl Pts',(-5.750911309,5.00031307,4.488275785));
#158476=CARTESIAN_POINT('Ctrl Pts',(-5.879849956,4.94766207,4.241446038));
#158477=CARTESIAN_POINT('Ctrl Pts',(-5.786639328,4.97393188700001,4.370662467));
#158478=CARTESIAN_POINT('Ctrl Pts',(-5.687842072,5.00031307,4.495659303));
#158479=CARTESIAN_POINT('Ctrl Pts',(-5.87874485221915,4.94797287197443,
4.24297778393543));
#158480=CARTESIAN_POINT('Ctrl Pts',(-5.88300433631815,4.94882769735767,
4.24600009009462));
#158481=CARTESIAN_POINT('Ctrl Pts',(-5.88726361083142,4.94967947049228,
4.2490235562089));
#158482=CARTESIAN_POINT('Ctrl Pts',(-5.89152375628648,4.9505285273734,4.25204655598669));
#158483=CARTESIAN_POINT('Ctrl Pts',(-5.89547870958579,4.95131675874924,
4.25485299137045));
#158484=CARTESIAN_POINT('Ctrl Pts',(-5.89943441481983,4.95210264915382,
4.2576590256409));
#158485=CARTESIAN_POINT('Ctrl Pts',(-5.90339086128714,4.95288622029679,
4.26046466127556));
#158486=CARTESIAN_POINT('Ctrl Pts',(-5.90734731175169,4.9536697922314,4.2632702997448));
#158487=CARTESIAN_POINT('Ctrl Pts',(-5.91130450444941,4.95445104509708,
4.2660755402845));
#158488=CARTESIAN_POINT('Ctrl Pts',(-5.9152624289547,4.95523000032746,4.26888038538439));
#158489=CARTESIAN_POINT('Ctrl Pts',(-6.07333975212726,5.00000000006602,
4.04081843272464));
#158490=CARTESIAN_POINT('Ctrl Pts',(-6.01205174514958,4.98208534611668,
4.13293414918722));
#158491=CARTESIAN_POINT('Ctrl Pts',(-5.94799829406127,4.964285714,4.2231487833414));
#158492=CARTESIAN_POINT('Ctrl Pts',(-5.91869173970455,4.9561417990393,4.26442493549441));
#158493=CARTESIAN_POINT('Ctrl Pts',(-5.88881516434955,4.94797287197443,
4.30529038626618));
#158494=CARTESIAN_POINT('Ctrl Pts',(-6.06052525045423,5.00000000006602,
3.97901164806512));
#158495=CARTESIAN_POINT('Ctrl Pts',(-6.00017468145858,4.98208534611668,
4.07093300385634));
#158496=CARTESIAN_POINT('Ctrl Pts',(-5.93706413,4.964285714,4.160981797));
#158497=CARTESIAN_POINT('Ctrl Pts',(-5.90818898457355,4.9561417990393,4.2021820712548));
#158498=CARTESIAN_POINT('Ctrl Pts',(-5.87874482871382,4.94797287197443,
4.24297763849028));
#158499=CARTESIAN_POINT('Ctrl Pts',(-5.87874535042468,4.94797301671685,
4.24297691564759));
#158500=CARTESIAN_POINT('Ctrl Pts',(-5.90818924040026,4.95614187119239,
4.20218170623045));
#158501=CARTESIAN_POINT('Ctrl Pts',(-5.93706413,4.964285714,4.160981797));
#158502=CARTESIAN_POINT('Ctrl Pts',(-6.00017468145858,4.98208534611668,
4.07093300385634));
#158503=CARTESIAN_POINT('Ctrl Pts',(-6.06052525045423,5.00000000006602,
3.97901164806513));
#158504=CARTESIAN_POINT('Ctrl Pts',(-6.061582466,5.000313899,3.977400912));
#158505=CARTESIAN_POINT('Ctrl Pts',(-6.000727704,4.98224132,4.07014392800001));
#158506=CARTESIAN_POINT('Ctrl Pts',(-5.93706413,4.964285714,4.160981797));
#158507=CARTESIAN_POINT('Ctrl Pts',(-5.908189518,4.95614194999999,4.20218131));
#158508=CARTESIAN_POINT('Ctrl Pts',(-5.878745916,4.947973174,4.242976131));
#158509=CARTESIAN_POINT('Ctrl Pts',(-6.133799235,5.000313899,3.96240807299999));
#158510=CARTESIAN_POINT('Ctrl Pts',(-6.073173866,4.98224132,4.056256015));
#158511=CARTESIAN_POINT('Ctrl Pts',(-6.009705774,4.964285714,4.148205311));
#158512=CARTESIAN_POINT('Ctrl Pts',(-5.980919823,4.95614194999999,4.189908912));
#158513=CARTESIAN_POINT('Ctrl Pts',(-5.951557878,4.947973174,4.231209003));
#158514=CARTESIAN_POINT('',(-5.98709641432499,4.94797317334225,4.2254656227057));
#158515=CARTESIAN_POINT('Ctrl Pts',(-6.51744456300001,4.81863040500001,
3.51912996));
#158516=CARTESIAN_POINT('Ctrl Pts',(-6.513250293,4.820029867,3.526897768));
#158517=CARTESIAN_POINT('Ctrl Pts',(-6.509037518,4.821428571,3.534655555));
#158518=CARTESIAN_POINT('Ctrl Pts',(-6.32022519,4.884117105,3.882351818));
#158519=CARTESIAN_POINT('Ctrl Pts',(-6.095446908,4.947973174,4.207955121));
#158520=CARTESIAN_POINT('Ctrl Pts',(-6.30584618800001,4.81863040500001,
3.577541593));
#158521=CARTESIAN_POINT('Ctrl Pts',(-6.3015823,4.820029867,3.585057207));
#158522=CARTESIAN_POINT('Ctrl Pts',(-6.297300509,4.821428571,3.592562637));
#158523=CARTESIAN_POINT('Ctrl Pts',(-6.105394932,4.884117105,3.928948446));
#158524=CARTESIAN_POINT('Ctrl Pts',(-5.878745916,4.947973174,4.242976131));
#158525=CARTESIAN_POINT('Ctrl Pts',(-6.30352756992369,4.8193909179172,3.58162539475427));
#158526=CARTESIAN_POINT('Ctrl Pts',(-6.31915715586046,4.82234724729902,
3.59071136724813));
#158527=CARTESIAN_POINT('Ctrl Pts',(-6.3347915846792,4.82527010310562,3.59979999996221));
#158528=CARTESIAN_POINT('Ctrl Pts',(-6.35043820069919,4.82816321747808,
3.60887704594857));
#158529=CARTESIAN_POINT('Ctrl Pts',(-6.36508582432909,4.83087161464152,
3.61737454809917));
#158530=CARTESIAN_POINT('Ctrl Pts',(-6.37974220004758,4.83355328553194,
3.62586552810932));
#158531=CARTESIAN_POINT('Ctrl Pts',(-6.39440688968605,4.83620904388884,
3.63435020025117));
#158532=CARTESIAN_POINT('Ctrl Pts',(-6.40907173677283,4.83886483075945,
3.6428349634892));
#158533=CARTESIAN_POINT('Ctrl Pts',(-6.4237449370543,4.84149471145087,3.65131344117656));
#158534=CARTESIAN_POINT('Ctrl Pts',(-6.43842608023093,4.84409946433625,
3.65978583438252));
#158535=CARTESIAN_POINT('Ctrl Pts',(-6.73754606545279,4.94924836941368,
3.07683225208978));
#158536=CARTESIAN_POINT('Ctrl Pts',(-6.73587558122639,4.94861077170684,
3.08047976154489));
#158537=CARTESIAN_POINT('Ctrl Pts',(-6.734205097,4.94797317400001,3.084127271));
#158538=CARTESIAN_POINT('Ctrl Pts',(-6.566195243,4.88384644,3.450977506));
#158539=CARTESIAN_POINT('Ctrl Pts',(-6.359329057,4.818610636,3.797406123));
#158540=CARTESIAN_POINT('Ctrl Pts',(-6.65653841463485,4.94924836941368,
2.87281360540941));
#158541=CARTESIAN_POINT('Ctrl Pts',(-6.65497848231742,4.94861077170684,
2.87641735770471));
#158542=CARTESIAN_POINT('Ctrl Pts',(-6.65341855,4.94797317400001,2.88002111));
#158543=CARTESIAN_POINT('Ctrl Pts',(-6.496527514,4.88384644,3.242470445));
#158544=CARTESIAN_POINT('Ctrl Pts',(-6.301192412,4.818610636,3.58573203));
#158545=CARTESIAN_POINT('',(-6.6669907716028,4.94797317334255,2.91431114283332));
#158546=CARTESIAN_POINT('Ctrl Pts',(-6.65467526919907,4.94745154526473,
2.87711784001687));
#158547=CARTESIAN_POINT('Ctrl Pts',(-6.65404690959953,4.94771235963237,
2.87856947500844));
#158548=CARTESIAN_POINT('Ctrl Pts',(-6.65341854999999,4.947973174,2.88002111));
#158549=CARTESIAN_POINT('Ctrl Pts',(-6.59050173599999,4.974088171,3.025371398));
#158550=CARTESIAN_POINT('Ctrl Pts',(-6.521297344,5.00031307,3.167835372));
#158551=CARTESIAN_POINT('Ctrl Pts',(-6.68184963465255,4.94745154526473,
2.94568606831802));
#158552=CARTESIAN_POINT('Ctrl Pts',(-6.68120631232628,4.94771235963237,
2.94714362565901));
#158553=CARTESIAN_POINT('Ctrl Pts',(-6.68056299,4.947973174,2.948601183));
#158554=CARTESIAN_POINT('Ctrl Pts',(-6.616147978,4.974088171,3.094544468));
#158555=CARTESIAN_POINT('Ctrl Pts',(-6.54542092200001,5.00031307,3.237535444));
#158556=CARTESIAN_POINT('Origin',(0.170346293524872,5.08925697390287,-0.0991313731653343));
#158557=CARTESIAN_POINT('Ctrl Pts',(-6.71320499500001,4.94766207,2.854904395));
#158558=CARTESIAN_POINT('Ctrl Pts',(-6.65046520500001,4.973931887,3.002434754));
#158559=CARTESIAN_POINT('Ctrl Pts',(-6.58130482,5.00031307,3.147066456));
#158560=CARTESIAN_POINT('Ctrl Pts',(-6.654167854,4.94766207,2.878289453));
#158561=CARTESIAN_POINT('Ctrl Pts',(-6.59091415,4.973931887,3.024522403));
#158562=CARTESIAN_POINT('Ctrl Pts',(-6.521297344,5.00031307,3.167835372));
#158563=CARTESIAN_POINT('Ctrl Pts',(-6.65341786670797,4.94797287202618,
2.88002295259182));
#158564=CARTESIAN_POINT('Ctrl Pts',(-6.6582274728443,4.9488276973978,2.88205893561886));
#158565=CARTESIAN_POINT('Ctrl Pts',(-6.66303712369621,4.94967947052343,
2.88409609656622));
#158566=CARTESIAN_POINT('Ctrl Pts',(-6.66784752488418,4.95052852739581,
2.88613261486336));
#158567=CARTESIAN_POINT('Ctrl Pts',(-6.67231331419332,4.95131675876267,
2.88802323921752));
#158568=CARTESIAN_POINT('Ctrl Pts',(-6.67677975163519,4.95210264915868,
2.88991331020176));
#158569=CARTESIAN_POINT('Ctrl Pts',(-6.68124682727894,4.9528862202939,2.89180283254273));
#158570=CARTESIAN_POINT('Ctrl Pts',(-6.6857139074358,4.95366979222076,2.8936923567927));
#158571=CARTESIAN_POINT('Ctrl Pts',(-6.69018162692286,4.95445104507959,
2.89558133287419));
#158572=CARTESIAN_POINT('Ctrl Pts',(-6.69464997632219,4.95523000034612,
2.89746976556783));
#158573=CARTESIAN_POINT('Ctrl Pts',(-6.800861408,5.000313899,2.639296217));
#158574=CARTESIAN_POINT('Ctrl Pts',(-6.760479825,4.98224132,2.743350299));
#158575=CARTESIAN_POINT('Ctrl Pts',(-6.716933807,4.964285714,2.846120278));
#158576=CARTESIAN_POINT('Ctrl Pts',(-6.696805943,4.955986264,2.893622674));
#158577=CARTESIAN_POINT('Ctrl Pts',(-6.676008248,4.947660853,2.940835644));
#158578=CARTESIAN_POINT('Ctrl Pts',(-6.774889661,5.000313899,2.581350438));
#158579=CARTESIAN_POINT('Ctrl Pts',(-6.735394657,4.98224132,2.685007149));
#158580=CARTESIAN_POINT('Ctrl Pts',(-6.692746959,4.964285714,2.787407065));
#158581=CARTESIAN_POINT('Ctrl Pts',(-6.673034316,4.955986264,2.834738411));
#158582=CARTESIAN_POINT('Ctrl Pts',(-6.652654221,4.947660853,2.88178622));
#158583=CARTESIAN_POINT('Ctrl Pts',(-6.65341826090931,4.94797303315017,
2.88002204190334));
#158584=CARTESIAN_POINT('Ctrl Pts',(-6.66675205370264,4.95342302528965,
2.84921815417841));
#158585=CARTESIAN_POINT('Ctrl Pts',(-6.67986191870764,4.95886083272511,
2.81834489018571));
#158586=CARTESIAN_POINT('Ctrl Pts',(-6.69274695880392,4.96428571390858,
2.78740706557253));
#158587=CARTESIAN_POINT('Ctrl Pts',(-6.72088369664955,4.97613189090849,
2.71984891517555));
#158588=CARTESIAN_POINT('Ctrl Pts',(-6.74804531683569,4.98803923904378,
2.65174931160051));
#158589=CARTESIAN_POINT('Ctrl Pts',(-6.77420342353812,5.00000000021333,
2.58315078520084));
#158590=CARTESIAN_POINT('Ctrl Pts',(-6.774889661,5.000313899,2.581350438));
#158591=CARTESIAN_POINT('Ctrl Pts',(-6.735394657,4.98224132,2.685007149));
#158592=CARTESIAN_POINT('Ctrl Pts',(-6.692746959,4.964285714,2.787407065));
#158593=CARTESIAN_POINT('Ctrl Pts',(-6.673404096,4.95614194999999,2.833850545));
#158594=CARTESIAN_POINT('Ctrl Pts',(-6.65341855,4.947973174,2.88002111));
#158595=CARTESIAN_POINT('Ctrl Pts',(-6.842195025,5.000313899,2.551183652));
#158596=CARTESIAN_POINT('Ctrl Pts',(-6.803161577,4.98224132,2.655870144));
#158597=CARTESIAN_POINT('Ctrl Pts',(-6.760943714,4.964285714,2.759313481));
#158598=CARTESIAN_POINT('Ctrl Pts',(-6.74179580400001,4.95614194999999,
2.806230203));
#158599=CARTESIAN_POINT('Ctrl Pts',(-6.721998624,4.947973174,2.852876671));
#158600=CARTESIAN_POINT('',(-6.75547163206247,4.94797317334224,2.83962783278288));
#158601=CARTESIAN_POINT('Ctrl Pts',(-7.121579248,4.818630405,2.035796731));
#158602=CARTESIAN_POINT('Ctrl Pts',(-7.119152886,4.820029867,2.044284575));
#158603=CARTESIAN_POINT('Ctrl Pts',(-7.116706299,4.821428571,2.052766612));
#158604=CARTESIAN_POINT('Ctrl Pts',(-7.007052717,4.884117105,2.432922999));
#158605=CARTESIAN_POINT('Ctrl Pts',(-6.857524711,4.947973174,2.799234563));
#158606=CARTESIAN_POINT('Ctrl Pts',(-6.92748470000001,4.818630405,2.138330128));
#158607=CARTESIAN_POINT('Ctrl Pts',(-6.924936134,4.820029867,2.146586641));
#158608=CARTESIAN_POINT('Ctrl Pts',(-6.922367894,4.821428571,2.154837056));
#158609=CARTESIAN_POINT('Ctrl Pts',(-6.80726196800001,4.884117105,2.524612378));
#158610=CARTESIAN_POINT('Ctrl Pts',(-6.65341855,4.947973174,2.88002111));
#158611=CARTESIAN_POINT('Ctrl Pts',(-6.92609818576639,4.81939091801858,
2.14281688688501));
#158612=CARTESIAN_POINT('Ctrl Pts',(-6.94331557651135,4.82234724733196,
2.1483305351867));
#158613=CARTESIAN_POINT('Ctrl Pts',(-6.96053826846024,4.82527010314683,
2.15384574070213));
#158614=CARTESIAN_POINT('Ctrl Pts',(-6.97777037186197,4.82816321751424,
2.1593470105455));
#158615=CARTESIAN_POINT('Ctrl Pts',(-6.99390225394218,4.83087161466876,
2.16449703978662));
#158616=CARTESIAN_POINT('Ctrl Pts',(-7.01004128142858,4.83355328554812,
2.1696388179197));
#158617=CARTESIAN_POINT('Ctrl Pts',(-7.02618707245826,4.83620904389281,
2.17477264840198));
#158618=CARTESIAN_POINT('Ctrl Pts',(-7.04233303683825,4.83886483075122,
2.17990653400395));
#158619=CARTESIAN_POINT('Ctrl Pts',(-7.05848580791564,4.84149471142928,
2.18503248530806));
#158620=CARTESIAN_POINT('Ctrl Pts',(-7.0746450282201,4.8440994643031,2.19015078689032));
#158621=CARTESIAN_POINT('Ctrl Pts',(-7.24145396603117,4.94924836941368,
1.55652438013174));
#158622=CARTESIAN_POINT('Ctrl Pts',(-7.24060664351559,4.94861077170684,
1.56044571756587));
#158623=CARTESIAN_POINT('Ctrl Pts',(-7.239759321,4.94797317400001,1.564367055));
#158624=CARTESIAN_POINT('Ctrl Pts',(-7.154539401,4.88384644,1.958757687));
#158625=CARTESIAN_POINT('Ctrl Pts',(-7.026981543,4.818610636,2.341557111));
#158626=CARTESIAN_POINT('Ctrl Pts',(-7.11848225152531,4.94924836941368,
1.37468982618827));
#158627=CARTESIAN_POINT('Ctrl Pts',(-7.11773348976265,4.94861077170684,
1.37854466409414));
#158628=CARTESIAN_POINT('Ctrl Pts',(-7.11698472800001,4.94797317400001,
1.382399502));
#158629=CARTESIAN_POINT('Ctrl Pts',(-7.041677609,4.88384644,1.770101908));
#158630=CARTESIAN_POINT('Ctrl Pts',(-6.92470042800001,4.818610636,2.147329501));
#158631=CARTESIAN_POINT('',(-7.1376109817771,4.94797317334255,1.41297022657449));
#158632=CARTESIAN_POINT('Ctrl Pts',(-7.11758794858711,4.94745154526474,
1.3792939513611));
#158633=CARTESIAN_POINT('Ctrl Pts',(-7.11728633829356,4.94771235963237,
1.38084672668055));
#158634=CARTESIAN_POINT('Ctrl Pts',(-7.11698472799999,4.947973174,1.382399502));
#158635=CARTESIAN_POINT('Ctrl Pts',(-7.086784889,4.974088171,1.537876837));
#158636=CARTESIAN_POINT('Ctrl Pts',(-7.049824001,5.00031307,1.691886981));
#158637=CARTESIAN_POINT('Ctrl Pts',(-7.15886713411728,4.94745154526474,
1.44041740752365));
#158638=CARTESIAN_POINT('Ctrl Pts',(-7.15855218405864,4.94771235963237,
1.44197918326182));
#158639=CARTESIAN_POINT('Ctrl Pts',(-7.158237234,4.947973174,1.443540959));
#158640=CARTESIAN_POINT('Ctrl Pts',(-7.126701702,4.974088171,1.599919494));
#158641=CARTESIAN_POINT('Ctrl Pts',(-7.088367037,5.00031307,1.754771648));
#158642=CARTESIAN_POINT('Origin',(0.187674271491483,5.0892572792628,-0.0601944222287432));
#158643=CARTESIAN_POINT('Ctrl Pts',(-7.169974048,4.94766207,1.345017684));
#158644=CARTESIAN_POINT('Ctrl Pts',(-7.140415745,4.97393188700001,1.502586065));
#158645=CARTESIAN_POINT('Ctrl Pts',(-7.103963832,5.00031307,1.658703797));
#158646=CARTESIAN_POINT('Ctrl Pts',(-7.117344258,4.94766207,1.380547252));
#158647=CARTESIAN_POINT('Ctrl Pts',(-7.087005153,4.97393188700001,1.536959034));
#158648=CARTESIAN_POINT('Ctrl Pts',(-7.049824001,5.00031307,1.691886981));
#158649=CARTESIAN_POINT('Ctrl Pts',(-7.11698445645141,4.94797287217653,
1.38240144844194));
#158650=CARTESIAN_POINT('Ctrl Pts',(-7.12211929286213,4.94882769748685,
1.38335590857904));
#158651=CARTESIAN_POINT('Ctrl Pts',(-7.12725442627626,4.94967947061876,
1.38431150914361));
#158652=CARTESIAN_POINT('Ctrl Pts',(-7.1323901543448,4.95052852750091,1.38526632077196));
#158653=CARTESIAN_POINT('Ctrl Pts',(-7.13715796428302,4.9513167588455,1.3861527307045));
#158654=CARTESIAN_POINT('Ctrl Pts',(-7.14192628825405,4.95210264922268,
1.38703846086629));
#158655=CARTESIAN_POINT('Ctrl Pts',(-7.1466951175664,4.95288622034009,1.38792351800371));
#158656=CARTESIAN_POINT('Ctrl Pts',(-7.15146395169674,4.95366979224915,
1.3888085760353));
#158657=CARTESIAN_POINT('Ctrl Pts',(-7.15623329237243,4.9544510450911,1.38969296126365));
#158658=CARTESIAN_POINT('Ctrl Pts',(-7.16100313117102,4.95523000029981,
1.39057668033257));
#158659=CARTESIAN_POINT('Ctrl Pts',(-7.209231717,5.000313899,1.115606768));
#158660=CARTESIAN_POINT('Ctrl Pts',(-7.192162786,4.98224132,1.22590897));
#158661=CARTESIAN_POINT('Ctrl Pts',(-7.171727357,4.964285714,1.33563735));
#158662=CARTESIAN_POINT('Ctrl Pts',(-7.16228168200001,4.955986264,1.386356063));
#158663=CARTESIAN_POINT('Ctrl Pts',(-7.152119618,4.947660853,1.436936109));
#158664=CARTESIAN_POINT('Ctrl Pts',(-7.171410545,5.000313899,1.064598886));
#158665=CARTESIAN_POINT('Ctrl Pts',(-7.155122041,4.98224132,1.174322419));
#158666=CARTESIAN_POINT('Ctrl Pts',(-7.135484378,4.964285714,1.283496277));
#158667=CARTESIAN_POINT('Ctrl Pts',(-7.126407446,4.955986264,1.333958678));
#158668=CARTESIAN_POINT('Ctrl Pts',(-7.116617714,4.947660853,1.384287653));
#158669=CARTESIAN_POINT('Ctrl Pts',(-7.11698472847237,4.94797317392425,
1.38239950207922));
#158670=CARTESIAN_POINT('Ctrl Pts',(-7.12716810933566,4.9566446894656,1.32997257504285));
#158671=CARTESIAN_POINT('Ctrl Pts',(-7.13676381742098,4.96527388632384,
1.27747875017038));
#158672=CARTESIAN_POINT('Ctrl Pts',(-7.15481559698884,4.98260138485293,
1.17216568210234));
#158673=CARTESIAN_POINT('Ctrl Pts',(-7.1632632328562,4.99129054983285,1.1193827722584));
#158674=CARTESIAN_POINT('Ctrl Pts',(-7.17112737309111,5.0000000005155,1.0665046610168));
#158675=CARTESIAN_POINT('Ctrl Pts',(-7.171410545,5.000313899,1.064598886));
#158676=CARTESIAN_POINT('Ctrl Pts',(-7.155122041,4.98224132,1.174322419));
#158677=CARTESIAN_POINT('Ctrl Pts',(-7.135484378,4.964285714,1.283496277));
#158678=CARTESIAN_POINT('Ctrl Pts',(-7.126577716,4.95614194999999,1.333012078));
#158679=CARTESIAN_POINT('Ctrl Pts',(-7.116984728,4.947973174,1.382399502));
#158680=CARTESIAN_POINT('Ctrl Pts',(-7.230657381,5.000313899,1.02066872));
#158681=CARTESIAN_POINT('Ctrl Pts',(-7.215041014,4.98224132,1.131298737));
#158682=CARTESIAN_POINT('Ctrl Pts',(-7.196047441,4.964285714,1.241399218));
#158683=CARTESIAN_POINT('Ctrl Pts',(-7.187432907,4.95614194999999,1.291335288));
#158684=CARTESIAN_POINT('Ctrl Pts',(-7.178126185,4.947973174,1.341146996));
#158685=CARTESIAN_POINT('',(-7.20796850522684,4.94797317334227,1.32101220153407));
#158686=CARTESIAN_POINT('Ctrl Pts',(-7.39271680200001,4.818630405,0.457271909));
#158687=CARTESIAN_POINT('Ctrl Pts',(-7.392171803,4.820029867,0.466082908));
#158688=CARTESIAN_POINT('Ctrl Pts',(-7.391605803,4.821428571,0.474892584));
#158689=CARTESIAN_POINT('Ctrl Pts',(-7.366238246,4.884117105,0.869733404));
#158690=CARTESIAN_POINT('Ctrl Pts',(-7.29895228100001,4.947973174,1.259624909));
#158691=CARTESIAN_POINT('Ctrl Pts',(-7.225201726,4.818630405,0.599132722));
#158692=CARTESIAN_POINT('Ctrl Pts',(-7.22448765,4.820029867,0.607744069));
#158693=CARTESIAN_POINT('Ctrl Pts',(-7.22375305,4.821428571,0.616353689));
#158694=CARTESIAN_POINT('Ctrl Pts',(-7.19082900000001,4.884117105,1.002228242));
#158695=CARTESIAN_POINT('Ctrl Pts',(-7.116984728,4.947973174,1.382399502));
#158696=CARTESIAN_POINT('Ctrl Pts',(-7.22481214832045,4.81939091801871,
0.603812642716627));
#158697=CARTESIAN_POINT('Ctrl Pts',(-7.24281227785518,4.82234724740094,
0.605496154954794));
#158698=CARTESIAN_POINT('Ctrl Pts',(-7.26081791900121,4.82527010320758,
0.607180048451803));
#158699=CARTESIAN_POINT('Ctrl Pts',(-7.27882975580833,4.82816321756723,
0.608848308897013));
#158700=CARTESIAN_POINT('Ctrl Pts',(-7.29569158745309,4.83087161470539,
0.610410055601027));
#158701=CARTESIAN_POINT('Ctrl Pts',(-7.31255862370503,4.83355328557064,
0.611962208038663));
#158702=CARTESIAN_POINT('Ctrl Pts',(-7.3294305568632,4.83620904390283,0.613505144663772));
#158703=CARTESIAN_POINT('Ctrl Pts',(-7.34630267116798,4.83886483074873,
0.61504809785472));
#158704=CARTESIAN_POINT('Ctrl Pts',(-7.36317972739467,4.8414947114159,0.616581838997027));
#158705=CARTESIAN_POINT('Ctrl Pts',(-7.38006143768145,4.84409946429152,
0.618106722867779));
#158706=CARTESIAN_POINT('Ctrl Pts',(-7.40675952790616,4.94924836941368,
-0.0365648420981692));
#158707=CARTESIAN_POINT('Ctrl Pts',(-7.40677498695308,4.94861077170685,
-0.0325530340490846));
#158708=CARTESIAN_POINT('Ctrl Pts',(-7.406790446,4.947973174,-0.028541226));
#158709=CARTESIAN_POINT('Ctrl Pts',(-7.408345248,4.88384644,0.374948537));
#158710=CARTESIAN_POINT('Ctrl Pts',(-7.366060182,4.818610636,0.776219491));
#158711=CARTESIAN_POINT('Ctrl Pts',(-7.24757376884405,4.94924836941368,
-0.187712921172618));
#158712=CARTESIAN_POINT('Ctrl Pts',(-7.24767118892203,4.94861077170685,
-0.183787245586309));
#158713=CARTESIAN_POINT('Ctrl Pts',(-7.247768609,4.947973174,-0.17986157));
#158714=CARTESIAN_POINT('Ctrl Pts',(-7.257566686,4.88384644,0.214965374));
#158715=CARTESIAN_POINT('Ctrl Pts',(-7.224417148,4.818610636,0.608520231));
#158716=CARTESIAN_POINT('',(-7.27448443441505,4.94797317334249,-0.154439607001196));
#158717=CARTESIAN_POINT('Ctrl Pts',(-7.24769012502909,4.94745154526473,
-0.183024189166083));
#158718=CARTESIAN_POINT('Ctrl Pts',(-7.24772936701454,4.94771235963237,
-0.181442879583041));
#158719=CARTESIAN_POINT('Ctrl Pts',(-7.247768609,4.947973174,-0.17986157));
#158720=CARTESIAN_POINT('Ctrl Pts',(-7.251697857,4.97408817100001,-0.021527137));
#158721=CARTESIAN_POINT('Ctrl Pts',(-7.248708723,5.00031307,0.136827835));
#158722=CARTESIAN_POINT('Ctrl Pts',(-7.30114396216113,4.94745154526473,
-0.132203570485143));
#158723=CARTESIAN_POINT('Ctrl Pts',(-7.30117211108056,4.94771235963237,
-0.130610603242571));
#158724=CARTESIAN_POINT('Ctrl Pts',(-7.30120026,4.947973174,-0.129017636));
#158725=CARTESIAN_POINT('Ctrl Pts',(-7.304018774,4.97408817100001,0.030484063));
#158726=CARTESIAN_POINT('Ctrl Pts',(-7.299868989,5.00031307,0.18995668));
#158727=CARTESIAN_POINT('Origin',(0.196226351021154,5.08925695299974,-0.0184426163327351));
#158728=CARTESIAN_POINT('Ctrl Pts',(-7.291483082,4.94766207,-0.22776056));
#158729=CARTESIAN_POINT('Ctrl Pts',(-7.296488381,4.97393188700001,-0.067521878));
#158730=CARTESIAN_POINT('Ctrl Pts',(-7.294449391,5.00031307,0.092781992));
#158731=CARTESIAN_POINT('Ctrl Pts',(-7.247721555,4.94766207,-0.181747804));
#158732=CARTESIAN_POINT('Ctrl Pts',(-7.251715671,4.97393188700001,-0.022470832));
#158733=CARTESIAN_POINT('Ctrl Pts',(-7.248708723,5.00031307,0.136827835));
#158734=CARTESIAN_POINT('Ctrl Pts',(-7.24776876254565,4.94797287209048,
-0.179859610832122));
#158735=CARTESIAN_POINT('Ctrl Pts',(-7.25298873007889,4.94882769744435,
-0.180031303752704));
#158736=CARTESIAN_POINT('Ctrl Pts',(-7.25820923271784,4.94967947057355,
-0.180201946555563));
#158737=CARTESIAN_POINT('Ctrl Pts',(-7.26343014649147,4.95052852744933,
-0.180373487663704));
#158738=CARTESIAN_POINT('Ctrl Pts',(-7.26827703965157,4.95131675880924,
-0.180532739752471));
#158739=CARTESIAN_POINT('Ctrl Pts',(-7.27312428867693,4.95210264919798,
-0.180692766204615));
#158740=CARTESIAN_POINT('Ctrl Pts',(-7.27797188654918,4.95288622032569,
-0.180853558570527));
#158741=CARTESIAN_POINT('Ctrl Pts',(-7.28281948931899,4.95366979224505,
-0.181014351098888));
#158742=CARTESIAN_POINT('Ctrl Pts',(-7.2876674421591,4.95445104509613,-0.181175909583881));
#158743=CARTESIAN_POINT('Ctrl Pts',(-7.29251573846638,4.95523000034311,
-0.18133822573945));
#158744=CARTESIAN_POINT('Ctrl Pts',(-7.28050636400001,5.000313899,-0.460247214));
#158745=CARTESIAN_POINT('Ctrl Pts',(-7.287548207,4.98224132,-0.348854501));
#158746=CARTESIAN_POINT('Ctrl Pts',(-7.291178906,4.964285714,-0.237298496));
#158747=CARTESIAN_POINT('Ctrl Pts',(-7.292857089,4.955986264,-0.185735018));
#158748=CARTESIAN_POINT('Ctrl Pts',(-7.29380582399999,4.947660853,-0.134152962));
#158749=CARTESIAN_POINT('Ctrl Pts',(-7.232604243,5.000313899,-0.501932126));
#158750=CARTESIAN_POINT('Ctrl Pts',(-7.240283871,4.98224132,-0.391272321));
#158751=CARTESIAN_POINT('Ctrl Pts',(-7.244574478,4.964285714,-0.28042937));
#158752=CARTESIAN_POINT('Ctrl Pts',(-7.246557685,4.955986264,-0.22919548));
#158753=CARTESIAN_POINT('Ctrl Pts',(-7.247816073,4.947660853,-0.177938666));
#158754=CARTESIAN_POINT('Ctrl Pts',(-7.24776873792564,4.94797303320985,
-0.179860602843012));
#158755=CARTESIAN_POINT('Ctrl Pts',(-7.24693594426172,4.95342302542251,
-0.213416168512296));
#158756=CARTESIAN_POINT('Ctrl Pts',(-7.24587078836578,4.95886083283933,
-0.246940673114338));
#158757=CARTESIAN_POINT('Ctrl Pts',(-7.24457447817704,4.96428571406034,
-0.280429370195282));
#158758=CARTESIAN_POINT('Ctrl Pts',(-7.24174375852354,4.97613189122118,
-0.353557797662088));
#158759=CARTESIAN_POINT('Ctrl Pts',(-7.23780069553802,4.98803923920819,
-0.42676819201584));
#158760=CARTESIAN_POINT('Ctrl Pts',(-7.23273737682363,5.00000000046251,
-0.500010033005965));
#158761=CARTESIAN_POINT('Ctrl Pts',(-7.232604243,5.000313899,-0.501932126));
#158762=CARTESIAN_POINT('Ctrl Pts',(-7.240283871,4.98224132,-0.391272321));
#158763=CARTESIAN_POINT('Ctrl Pts',(-7.244574478,4.964285714,-0.28042937));
#158764=CARTESIAN_POINT('Ctrl Pts',(-7.246520483,4.95614194999999,-0.230156553));
#158765=CARTESIAN_POINT('Ctrl Pts',(-7.247768609,4.947973174,-0.17986157));
#158766=CARTESIAN_POINT('Ctrl Pts',(-7.281022233,5.000313899,-0.557571548));
#158767=CARTESIAN_POINT('Ctrl Pts',(-7.289553152,4.98224132,-0.446170941));
#158768=CARTESIAN_POINT('Ctrl Pts',(-7.294671987,4.964285714,-0.334561492));
#158769=CARTESIAN_POINT('Ctrl Pts',(-7.296993635,4.95614194999999,-0.283941029));
#158770=CARTESIAN_POINT('Ctrl Pts',(-7.298612544,4.947973174,-0.233293221));
#158771=CARTESIAN_POINT('',(-7.32342878135728,4.94797317334223,-0.259372492529681));
#158772=CARTESIAN_POINT('Ctrl Pts',(-7.318179135,4.818630405,-1.14263444));
#158773=CARTESIAN_POINT('Ctrl Pts',(-7.319540982,4.820029867,-1.133912278));
#158774=CARTESIAN_POINT('Ctrl Pts',(-7.320882034,4.821428571,-1.125186894));
#158775=CARTESIAN_POINT('Ctrl Pts',(-7.380986662,4.884117105,-0.734123958));
#158776=CARTESIAN_POINT('Ctrl Pts',(-7.399088954,4.947973174,-0.338883407));
#158777=CARTESIAN_POINT('Ctrl Pts',(-7.18507635000001,4.818630405,-0.968079464000001));
#158778=CARTESIAN_POINT('Ctrl Pts',(-7.186230154,4.820029867,-0.95951594));
#158779=CARTESIAN_POINT('Ctrl Pts',(-7.187363542,4.821428571,-0.95094969));
#158780=CARTESIAN_POINT('Ctrl Pts',(-7.238160861,4.884117105,-0.567018973000001));
#158781=CARTESIAN_POINT('Ctrl Pts',(-7.247768609,4.947973174,-0.17986157));
#158782=CARTESIAN_POINT('Ctrl Pts',(-7.18570192502524,4.81939091775255,
-0.96342520897109));
#158783=CARTESIAN_POINT('Ctrl Pts',(-7.20364312653454,4.82234724727576,
-0.965650551686533));
#158784=CARTESIAN_POINT('Ctrl Pts',(-7.22158979302488,4.82527010313215,
-0.96787670764295));
#158785=CARTESIAN_POINT('Ctrl Pts',(-7.23953914972131,4.82816321749835,
-0.970119462776279));
#158786=CARTESIAN_POINT('Ctrl Pts',(-7.25634249050191,4.83087161465345,
-0.972219024305425));
#158787=CARTESIAN_POINT('Ctrl Pts',(-7.27314885172646,4.83355328553458,
-0.974329074620028));
#158788=CARTESIAN_POINT('Ctrl Pts',(-7.28995801424419,4.83620904388172,
-0.976449177968326));
#158789=CARTESIAN_POINT('Ctrl Pts',(-7.30676735723456,4.83886483074258,
-0.978569304079248));
#158790=CARTESIAN_POINT('Ctrl Pts',(-7.32357954629048,4.84149471142377,
-0.98069948922502));
#158791=CARTESIAN_POINT('Ctrl Pts',(-7.34039437668646,4.84409946433426,
-0.982839325059756));
#158792=CARTESIAN_POINT('Ctrl Pts',(-7.22573324546067,4.94924836941368,
-1.62794433293449));
#158793=CARTESIAN_POINT('Ctrl Pts',(-7.22661076323034,4.94861077170684,
-1.62402964196724));
#158794=CARTESIAN_POINT('Ctrl Pts',(-7.227488281,4.94797317400001,-1.620114951));
#158795=CARTESIAN_POINT('Ctrl Pts',(-7.315745105,4.88384644,-1.226392791));
#158796=CARTESIAN_POINT('Ctrl Pts',(-7.360710034,4.818610636,-0.825413289));
#158797=CARTESIAN_POINT('Ctrl Pts',(-7.03777679268802,4.94924836941368,
-1.74133842106059));
#158798=CARTESIAN_POINT('Ctrl Pts',(-7.03871583934401,4.94861077170684,
-1.73752546803029));
#158799=CARTESIAN_POINT('Ctrl Pts',(-7.03965488600001,4.94797317400001,
-1.733712515));
#158800=CARTESIAN_POINT('Ctrl Pts',(-7.134100011,4.88384644,-1.350222703));
#158801=CARTESIAN_POINT('Ctrl Pts',(-7.186328152,4.818610636,-0.958742768));
#158802=CARTESIAN_POINT('',(-7.071211081057,4.94797317334255,-1.71462801588899));
#158803=CARTESIAN_POINT('Ctrl Pts',(-7.03889836730892,4.94745154526473,
-1.73678432215825));
#158804=CARTESIAN_POINT('Ctrl Pts',(-7.03927662665446,4.94771235963237,
-1.73524841857913));
#158805=CARTESIAN_POINT('Ctrl Pts',(-7.039654886,4.947973174,-1.733712515));
#158806=CARTESIAN_POINT('Ctrl Pts',(-7.077529493,4.974088171,-1.579924525));
#158807=CARTESIAN_POINT('Ctrl Pts',(-7.108651881,5.00031307,-1.424629229));
#158808=CARTESIAN_POINT('Ctrl Pts',(-7.1020274146377,4.94745154526474,-1.69864285574175));
#158809=CARTESIAN_POINT('Ctrl Pts',(-7.10239734631886,4.94771235963237,
-1.69709318237087));
#158810=CARTESIAN_POINT('Ctrl Pts',(-7.102767278,4.947973174,-1.695543509));
#158811=CARTESIAN_POINT('Ctrl Pts',(-7.139808047,4.974088171,-1.540376768));
#158812=CARTESIAN_POINT('Ctrl Pts',(-7.17003718,5.00031307,-1.383740452));
#158813=CARTESIAN_POINT('Origin',(0.195603365251878,5.0892570054678,0.0241714225221729));
#158814=CARTESIAN_POINT('Ctrl Pts',(-7.07205047200001,4.94766207,-1.789888972));
#158815=CARTESIAN_POINT('Ctrl Pts',(-7.11138533,4.973931887,-1.634472573));
#158816=CARTESIAN_POINT('Ctrl Pts',(-7.143854603,5.00031307,-1.477478196));
#158817=CARTESIAN_POINT('Ctrl Pts',(-7.039203447,4.94766207,-1.735544534));
#158818=CARTESIAN_POINT('Ctrl Pts',(-7.077344024,4.973931887,-1.580849986));
#158819=CARTESIAN_POINT('Ctrl Pts',(-7.108651881,5.00031307,-1.424629229));
#158820=CARTESIAN_POINT('Ctrl Pts',(-7.03965545684652,4.94797287211985,
-1.73371063429946));
#158821=CARTESIAN_POINT('Ctrl Pts',(-7.04471647548854,4.94882769743596,
-1.73500045180656));
#158822=CARTESIAN_POINT('Ctrl Pts',(-7.04977824253012,4.94967947055132,
-1.73628935882992));
#158823=CARTESIAN_POINT('Ctrl Pts',(-7.05484021799868,4.95052852741816,
-1.73757923153099));
#158824=CARTESIAN_POINT('Ctrl Pts',(-7.05953955902984,4.9513167587711,-1.73877669914946));
#158825=CARTESIAN_POINT('Ctrl Pts',(-7.06423908115425,4.95210264915737,
-1.73997499952157));
#158826=CARTESIAN_POINT('Ctrl Pts',(-7.06893877932178,4.95288622028444,
-1.74117412288784));
#158827=CARTESIAN_POINT('Ctrl Pts',(-7.07363848223743,4.95366979220316,
-1.74237324746559));
#158828=CARTESIAN_POINT('Ctrl Pts',(-7.07833836238181,4.95445104505539,
-1.74357319534238));
#158829=CARTESIAN_POINT('Ctrl Pts',(-7.08303841496067,4.95523000028386,
-1.74477395697837));
#158830=CARTESIAN_POINT('Ctrl Pts',(-7.011352625,5.000313899,-2.014580548));
#158831=CARTESIAN_POINT('Ctrl Pts',(-7.042175974,4.98224132,-1.907305922));
#158832=CARTESIAN_POINT('Ctrl Pts',(-7.069703033,4.964285714,-1.799138528));
#158833=CARTESIAN_POINT('Ctrl Pts',(-7.082426605,4.955986264,-1.749141335));
#158834=CARTESIAN_POINT('Ctrl Pts',(-7.094441776,4.947660853,-1.698969189));
#158835=CARTESIAN_POINT('Ctrl Pts',(-6.955609405,5.000313899,-2.04499335));
#158836=CARTESIAN_POINT('Ctrl Pts',(-6.986898075,4.98224132,-1.938571603));
#158837=CARTESIAN_POINT('Ctrl Pts',(-7.014916327,4.964285714,-1.831242452));
#158838=CARTESIAN_POINT('Ctrl Pts',(-7.02786694,4.955986264,-1.781632713));
#158839=CARTESIAN_POINT('Ctrl Pts',(-7.040114608,4.947660853,-1.73184477));
#158840=CARTESIAN_POINT('Ctrl Pts',(-7.03965488655287,4.94797317390935,
-1.73371251515132));
#158841=CARTESIAN_POINT('Ctrl Pts',(-7.02688358239494,4.9566446859759,-1.78556977598731));
#158842=CARTESIAN_POINT('Ctrl Pts',(-7.01355081990285,4.96527388717983,
-1.83724103979854));
#158843=CARTESIAN_POINT('Ctrl Pts',(-6.98571435793737,4.98260138847449,
-1.9404003540024));
#158844=CARTESIAN_POINT('Ctrl Pts',(-6.97121825042533,4.99129055630127,
-1.99185191186361));
#158845=CARTESIAN_POINT('Ctrl Pts',(-6.95615261950568,5.0000000003956,-2.04314481393163));
#158846=CARTESIAN_POINT('Ctrl Pts',(-6.955609405,5.000313899,-2.04499335));
#158847=CARTESIAN_POINT('Ctrl Pts',(-6.986898075,4.98224132,-1.938571603));
#158848=CARTESIAN_POINT('Ctrl Pts',(-7.014916327,4.964285714,-1.831242452));
#158849=CARTESIAN_POINT('Ctrl Pts',(-7.02762400500001,4.95614194999999,
-1.782563319));
#158850=CARTESIAN_POINT('Ctrl Pts',(-7.039654886,4.947973174,-1.733712515));
#158851=CARTESIAN_POINT('Ctrl Pts',(-6.990934579,5.000313899,-2.10974039));
#158852=CARTESIAN_POINT('Ctrl Pts',(-7.023213887,4.98224132,-2.002778163));
#158853=CARTESIAN_POINT('Ctrl Pts',(-7.052205779,4.964285714,-1.894878478));
#158854=CARTESIAN_POINT('Ctrl Pts',(-7.065355051,4.95614194999999,-1.845940579));
#158855=CARTESIAN_POINT('Ctrl Pts',(-7.077823892,4.947973174,-1.796824907));
#158856=CARTESIAN_POINT('',(-7.09645366749441,4.94797317334227,-1.82762921640457));
#158857=CARTESIAN_POINT('Ctrl Pts',(-6.901451545,4.818630405,-2.689112472));
#158858=CARTESIAN_POINT('Ctrl Pts',(-6.90465656,4.820029867,-2.680886986));
#158859=CARTESIAN_POINT('Ctrl Pts',(-6.907841959,4.821428571,-2.672653884));
#158860=CARTESIAN_POINT('Ctrl Pts',(-7.050608345,4.884117105,-2.3036545));
#158861=CARTESIAN_POINT('Ctrl Pts',(-7.153252451,4.947973174,-1.92154591));
#158862=CARTESIAN_POINT('Ctrl Pts',(-6.808984789,4.818630405,-2.49002533));
#158863=CARTESIAN_POINT('Ctrl Pts',(-6.811952522,4.820029867,-2.48191005));
#158864=CARTESIAN_POINT('Ctrl Pts',(-6.814900903,4.821428571,-2.47378772));
#158865=CARTESIAN_POINT('Ctrl Pts',(-6.94704436400001,4.884117105,-2.109753011));
#158866=CARTESIAN_POINT('Ctrl Pts',(-7.039654886,4.947973174,-1.733712515));
#158867=CARTESIAN_POINT('Ctrl Pts',(-6.81059626604813,4.81939091775241,
-2.48561436902601));
#158868=CARTESIAN_POINT('Ctrl Pts',(-6.82763962922413,4.82234724736873,
-2.49164451250913));
#158869=CARTESIAN_POINT('Ctrl Pts',(-6.84468815497496,4.82527010319989,
-2.49767662485868));
#158870=CARTESIAN_POINT('Ctrl Pts',(-6.86173573966136,4.82816321756086,
-2.50372552673113));
#158871=CARTESIAN_POINT('Ctrl Pts',(-6.87769488401649,4.83087161470757,
-2.5093882232332));
#158872=CARTESIAN_POINT('Ctrl Pts',(-6.89365472341908,4.83355328558158,
-2.51506181260813));
#158873=CARTESIAN_POINT('Ctrl Pts',(-6.90961513751605,4.83620904392258,
-2.52074582218012));
#158874=CARTESIAN_POINT('Ctrl Pts',(-6.925575722973,4.8388648307773,-2.52642989277884));
#158875=CARTESIAN_POINT('Ctrl Pts',(-6.94153692555988,4.84149471145331,
-2.5321243990602));
#158876=CARTESIAN_POINT('Ctrl Pts',(-6.9574986329725,4.84409946433526,-2.5378288981618));
#158877=CARTESIAN_POINT('Ctrl Pts',(-6.7068397085662,4.94924836941368,-3.14320295556554));
#158878=CARTESIAN_POINT('Ctrl Pts',(-6.7085382532831,4.94861077170684,-3.13956842828277));
#158879=CARTESIAN_POINT('Ctrl Pts',(-6.71023679800001,4.94797317400001,
-3.135933901));
#158880=CARTESIAN_POINT('Ctrl Pts',(-6.881068851,4.88384644,-2.770389355));
#158881=CARTESIAN_POINT('Ctrl Pts',(-7.011181266,4.818610636,-2.388450661));
#158882=CARTESIAN_POINT('Ctrl Pts',(-6.49890119506649,4.94924836941368,
-3.21354087208441));
#158883=CARTESIAN_POINT('Ctrl Pts',(-6.50063795953325,4.94861077170684,
-3.21001893104221));
#158884=CARTESIAN_POINT('Ctrl Pts',(-6.502374724,4.94797317400001,-3.20649699));
#158885=CARTESIAN_POINT('Ctrl Pts',(-6.67705074900001,4.88384644,-2.852275866));
#158886=CARTESIAN_POINT('Ctrl Pts',(-6.812214438,4.818610636,-2.481176021));
#158887=CARTESIAN_POINT('',(-6.53729575574303,4.94797317334255,-3.19464232459535));
#158888=CARTESIAN_POINT('Ctrl Pts',(-6.50097554455138,4.94745154526473,
-3.20933435087155));
#158889=CARTESIAN_POINT('Ctrl Pts',(-6.50167513427568,4.94771235963237,
-3.20791567043577));
#158890=CARTESIAN_POINT('Ctrl Pts',(-6.502374724,4.947973174,-3.20649699));
#158891=CARTESIAN_POINT('Ctrl Pts',(-6.572423716,4.974088171,-3.064446398));
#158892=CARTESIAN_POINT('Ctrl Pts',(-6.636202377,5.00031307,-2.919472213));
#158893=CARTESIAN_POINT('Ctrl Pts',(-6.570827957299,4.94745154526473,-3.18565548897648));
#158894=CARTESIAN_POINT('Ctrl Pts',(-6.5715223741495,4.94771235963237,-3.18422157048824));
#158895=CARTESIAN_POINT('Ctrl Pts',(-6.572216791,4.947973174,-3.182787652));
#158896=CARTESIAN_POINT('Ctrl Pts',(-6.64174783,4.974088171,-3.039211294));
#158897=CARTESIAN_POINT('Ctrl Pts',(-6.704942401,5.00031307,-2.892735418));
#158898=CARTESIAN_POINT('Origin',(0.185833529860157,5.08925709679066,0.0656549302348208));
#158899=CARTESIAN_POINT('Ctrl Pts',(-6.52193664200001,4.94766207,-3.268324166));
#158900=CARTESIAN_POINT('Ctrl Pts',(-6.593761804,4.97393188700001,-3.124997148));
#158901=CARTESIAN_POINT('Ctrl Pts',(-6.659221114,5.00031307,-2.978653146));
#158902=CARTESIAN_POINT('Ctrl Pts',(-6.50154001,4.94766207,-3.208189131));
#158903=CARTESIAN_POINT('Ctrl Pts',(-6.572043636,4.97393188700001,-3.065310352));
#158904=CARTESIAN_POINT('Ctrl Pts',(-6.63620237700001,5.00031307,-2.919472213));
#158905=CARTESIAN_POINT('Ctrl Pts',(-6.50237568605531,4.94797287219492,
-3.20649527578045));
#158906=CARTESIAN_POINT('Ctrl Pts',(-6.50704110849926,4.94882769745278,
-3.20884290710233));
#158907=CARTESIAN_POINT('Ctrl Pts',(-6.51170745733011,4.94967947057386,
-3.21118981052001));
#158908=CARTESIAN_POINT('Ctrl Pts',(-6.5163738021151,4.95052852744416,-3.21353770185232));
#158909=CARTESIAN_POINT('Ctrl Pts',(-6.52070585498803,4.9513167587952,-3.2157173927796));
#158910=CARTESIAN_POINT('Ctrl Pts',(-6.5250379056958,4.95210264917763,-3.2178979359278));
#158911=CARTESIAN_POINT('Ctrl Pts',(-6.52936995141139,4.95288622030084,
-3.22007932067324));
#158912=CARTESIAN_POINT('Ctrl Pts',(-6.53370200150367,4.95366979221571,
-3.22226070762255));
#158913=CARTESIAN_POINT('Ctrl Pts',(-6.53803404769612,4.95445104506405,
-3.22444293672171));
#158914=CARTESIAN_POINT('Ctrl Pts',(-6.54236608731522,4.9552300002817,-3.2266259975922));
#158915=CARTESIAN_POINT('Ctrl Pts',(-6.414355829,5.000313899,-3.474714335));
#158916=CARTESIAN_POINT('Ctrl Pts',(-6.46751942,4.98224132,-3.376573839));
#158917=CARTESIAN_POINT('Ctrl Pts',(-6.517655703,4.964285714,-3.276852842));
#158918=CARTESIAN_POINT('Ctrl Pts',(-6.540829724,4.955986264,-3.230759748));
#158919=CARTESIAN_POINT('Ctrl Pts',(-6.563349515,4.947660853,-3.184343505));
#158920=CARTESIAN_POINT('Ctrl Pts',(-6.353378002,5.000313899,-3.492432958));
#158921=CARTESIAN_POINT('Ctrl Pts',(-6.40681269,4.98224132,-3.395225431));
#158922=CARTESIAN_POINT('Ctrl Pts',(-6.457248486,4.964285714,-3.296428672));
#158923=CARTESIAN_POINT('Ctrl Pts',(-6.480560947,4.955986264,-3.25076278));
#158924=CARTESIAN_POINT('Ctrl Pts',(-6.503225208,4.947660853,-3.204771738));
#158925=CARTESIAN_POINT('Ctrl Pts',(-6.50237524706428,4.94797303335539,
-3.2064961659945));
#158926=CARTESIAN_POINT('Ctrl Pts',(-6.48752980748,4.95342302544615,-3.23660069140457));
#158927=CARTESIAN_POINT('Ctrl Pts',(-6.47248652405784,4.95886083281266,
-3.26657946034516));
#158928=CARTESIAN_POINT('Ctrl Pts',(-6.45724848618829,4.96428571404603,
-3.29642867215033));
#158929=CARTESIAN_POINT('Ctrl Pts',(-6.42397356473944,4.97613189118364,
-3.36160964736261));
#158930=CARTESIAN_POINT('Ctrl Pts',(-6.38965469195533,4.98803923904675,
-3.42639795188724));
#158931=CARTESIAN_POINT('Ctrl Pts',(-6.35430589758882,5.0000000002178,-3.49074441377445));
#158932=CARTESIAN_POINT('Ctrl Pts',(-6.353378002,5.000313899,-3.492432958));
#158933=CARTESIAN_POINT('Ctrl Pts',(-6.40681269,4.98224132,-3.395225431));
#158934=CARTESIAN_POINT('Ctrl Pts',(-6.457248486,4.964285714,-3.296428672));
#158935=CARTESIAN_POINT('Ctrl Pts',(-6.48012364,4.95614195,-3.251619405));
#158936=CARTESIAN_POINT('Ctrl Pts',(-6.502374724,4.947973174,-3.20649699));
#158937=CARTESIAN_POINT('Ctrl Pts',(-6.373958593,5.000313899,-3.563260116));
#158938=CARTESIAN_POINT('Ctrl Pts',(-6.42847694499999,4.98224132,-3.465737703));
#158939=CARTESIAN_POINT('Ctrl Pts',(-6.479986266,4.964285714,-3.366593053));
#158940=CARTESIAN_POINT('Ctrl Pts',(-6.503348317,4.95614195,-3.321626));
#158941=CARTESIAN_POINT('Ctrl Pts',(-6.526084062,4.947973174,-3.276339057));
#158942=CARTESIAN_POINT('',(-6.5376562666786,4.94797317334228,-3.31042803009703));
#158943=CARTESIAN_POINT('Ctrl Pts',(-6.162019751,4.818630405,-4.109850593));
#158944=CARTESIAN_POINT('Ctrl Pts',(-6.166918071,4.820029867,-4.102506398));
#158945=CARTESIAN_POINT('Ctrl Pts',(-6.171798871,4.821428571,-4.095150548));
#158946=CARTESIAN_POINT('Ctrl Pts',(-6.390551418,4.884117105,-3.765468718));
#158947=CARTESIAN_POINT('Ctrl Pts',(-6.572937813,4.947973174,-3.414359063));
#158948=CARTESIAN_POINT('Ctrl Pts',(-6.114512667,4.818630405,-3.895540379));
#158949=CARTESIAN_POINT('Ctrl Pts',(-6.119155562,4.820029867,-3.888252805));
#158950=CARTESIAN_POINT('Ctrl Pts',(-6.123781072,4.821428571,-3.880954185));
#158951=CARTESIAN_POINT('Ctrl Pts',(-6.331091794,4.884117105,-3.553837343));
#158952=CARTESIAN_POINT('Ctrl Pts',(-6.502374724,4.947973174,-3.20649699));
#158953=CARTESIAN_POINT('Ctrl Pts',(-6.11703469529526,4.81939091801858,
-3.8915789639107));
#158954=CARTESIAN_POINT('Ctrl Pts',(-6.13238329170512,4.82234724732519,
-3.90113194489536));
#158955=CARTESIAN_POINT('Ctrl Pts',(-6.14773650636247,4.82527010323118,
-3.91068795923837));
#158956=CARTESIAN_POINT('Ctrl Pts',(-6.16308519293364,4.82816321759971,
-3.92026016792834));
#158957=CARTESIAN_POINT('Ctrl Pts',(-6.17745390895555,4.83087161473765,
-3.92922121796549));
#158958=CARTESIAN_POINT('Ctrl Pts',(-6.19182096212693,4.83355328560386,
-3.93819305562455));
#158959=CARTESIAN_POINT('Ctrl Pts',(-6.20618633652024,4.83620904393796,
-3.94717519340763));
#158960=CARTESIAN_POINT('Ctrl Pts',(-6.22055186514831,4.83886483078577,
-3.956157427628));
#158961=CARTESIAN_POINT('Ctrl Pts',(-6.23491575311279,4.84149471145579,
-3.9651499862183));
#158962=CARTESIAN_POINT('Ctrl Pts',(-6.24927798597133,4.84409946433865,
-3.97415241254827));
#158963=CARTESIAN_POINT('Ctrl Pts',(-5.87434179975964,4.94924836941368,
-4.51148890129795));
#158964=CARTESIAN_POINT('Ctrl Pts',(-5.87678194937982,4.94861077170684,
-4.50830448414898));
#158965=CARTESIAN_POINT('Ctrl Pts',(-5.879222099,4.94797317400001,-4.505120067));
#158966=CARTESIAN_POINT('Ctrl Pts',(-6.124641466,4.88384644,-4.184845591));
#158967=CARTESIAN_POINT('Ctrl Pts',(-6.333817454,4.818610636,-3.839806735));
#158968=CARTESIAN_POINT('Ctrl Pts',(-5.6561442008214,4.94924836941368,-4.53548172299218));
#158969=CARTESIAN_POINT('Ctrl Pts',(-5.6585974739107,4.94861077170684,-4.53241547599609));
#158970=CARTESIAN_POINT('Ctrl Pts',(-5.661050747,4.94797317400001,-4.529349229));
#158971=CARTESIAN_POINT('Ctrl Pts',(-5.90779001400001,4.88384644,-4.22095978));
#158972=CARTESIAN_POINT('Ctrl Pts',(-6.119569149,4.818610636,-3.887592241));
#158973=CARTESIAN_POINT('',(-5.69770374701121,4.94797317334255,-4.5252787091336));
#158974=CARTESIAN_POINT('Ctrl Pts',(-5.65907433086952,4.94745154526473,
-4.5318194717201));
#158975=CARTESIAN_POINT('Ctrl Pts',(-5.66006253893476,4.94771235963237,
-4.53058435036005));
#158976=CARTESIAN_POINT('Ctrl Pts',(-5.661050747,4.947973174,-4.529349229));
#158977=CARTESIAN_POINT('Ctrl Pts',(-5.759998711,4.974088171,-4.405678164));
#158978=CARTESIAN_POINT('Ctrl Pts',(-5.853451427,5.00031307,-4.277803922));
#158979=CARTESIAN_POINT('Ctrl Pts',(-5.73238388827846,4.94745154526473,
-4.52371041336006));
#158980=CARTESIAN_POINT('Ctrl Pts',(-5.73337032013924,4.94771235963237,
-4.52245929818003));
#158981=CARTESIAN_POINT('Ctrl Pts',(-5.734356752,4.947973174,-4.521208183));
#158982=CARTESIAN_POINT('Ctrl Pts',(-5.833126867,4.974088171,-4.395935678));
#158983=CARTESIAN_POINT('Ctrl Pts',(-5.926331967,5.00031307,-4.266469291));
#158984=CARTESIAN_POINT('Origin',(0.167375319649697,5.08925700133457,0.104068977210618));
#158985=CARTESIAN_POINT('Ctrl Pts',(-5.666864302,4.94766207,-4.593936154));
#158986=CARTESIAN_POINT('Ctrl Pts',(-5.767821305,4.97393188700001,-4.469400329));
#158987=CARTESIAN_POINT('Ctrl Pts',(-5.863209847,5.00031307,-4.340549585));
#158988=CARTESIAN_POINT('Ctrl Pts',(-5.659871788,4.94766207,-4.53082237));
#158989=CARTESIAN_POINT('Ctrl Pts',(-5.75944179200001,4.97393188700001,
-4.406440213));
#158990=CARTESIAN_POINT('Ctrl Pts',(-5.853451427,5.00031307,-4.277803922));
#158991=CARTESIAN_POINT('Ctrl Pts',(-5.66105205514287,4.94797287208707,
-4.52934776177233));
#158992=CARTESIAN_POINT('Ctrl Pts',(-5.66510373101984,4.94882769740976,
-4.53264343487047));
#158993=CARTESIAN_POINT('Ctrl Pts',(-5.66915646832016,4.94967947055303,
-4.5359385960291));
#158994=CARTESIAN_POINT('Ctrl Pts',(-5.67320898930314,4.95052852744299,
-4.53923472113756));
#158995=CARTESIAN_POINT('Ctrl Pts',(-5.67697119202556,4.9513167588072,-4.54229471537536));
#158996=CARTESIAN_POINT('Ctrl Pts',(-5.68073320943725,4.95210264920075,
-4.54535554144628));
#158997=CARTESIAN_POINT('Ctrl Pts',(-5.68449504105515,4.95288622033218,
-4.54841718836571));
#158998=CARTESIAN_POINT('Ctrl Pts',(-5.68825687647365,4.95366979225525,
-4.55147883837835));
#158999=CARTESIAN_POINT('Ctrl Pts',(-5.69201852704637,4.95445104510896,
-4.55454131001399));
#159000=CARTESIAN_POINT('Ctrl Pts',(-5.69577999258466,4.95523000036888,
-4.55760459272089));
#159001=CARTESIAN_POINT('Ctrl Pts',(-5.517430884,5.000313899,-4.772374341));
#159002=CARTESIAN_POINT('Ctrl Pts',(-5.590448845,4.98224132,-4.68795691599999));
#159003=CARTESIAN_POINT('Ctrl Pts',(-5.660850037,4.964285714,-4.601345159));
#159004=CARTESIAN_POINT('Ctrl Pts',(-5.693390914,4.955986264,-4.561311425));
#159005=CARTESIAN_POINT('Ctrl Pts',(-5.725362325,4.947660853,-4.520821458));
#159006=CARTESIAN_POINT('Ctrl Pts',(-5.454069705,5.000313899,-4.776570282));
#159007=CARTESIAN_POINT('Ctrl Pts',(-5.527151864,4.98224132,-4.69312229100001));
#159008=CARTESIAN_POINT('Ctrl Pts',(-5.597646882,4.964285714,-4.607477551));
#159009=CARTESIAN_POINT('Ctrl Pts',(-5.630231128,4.955986264,-4.567890792));
#159010=CARTESIAN_POINT('Ctrl Pts',(-5.662252225,4.947660853,-4.527847142));
#159011=CARTESIAN_POINT('Ctrl Pts',(-5.661050747,4.947973174,-4.529349229));
#159012=CARTESIAN_POINT('Ctrl Pts',(-5.64008185355594,4.95342292106738,
-4.55555740236727));
#159013=CARTESIAN_POINT('Ctrl Pts',(-5.6189455709875,4.95886077964645,-4.58160167016205));
#159014=CARTESIAN_POINT('Ctrl Pts',(-5.59764688175189,4.9642857140632,-4.60747755130143));
#159015=CARTESIAN_POINT('Ctrl Pts',(-5.55113792653855,4.97613189126735,
-4.6639815070346));
#159016=CARTESIAN_POINT('Ctrl Pts',(-5.50369384036136,4.98803923897126,
-4.71987755304588));
#159017=CARTESIAN_POINT('Ctrl Pts',(-5.45533889445123,5.00000000010406,
-4.77512068459171));
#159018=CARTESIAN_POINT('Ctrl Pts',(-5.454069705,5.000313899,-4.776570282));
#159019=CARTESIAN_POINT('Ctrl Pts',(-5.527151864,4.98224132,-4.69312229100001));
#159020=CARTESIAN_POINT('Ctrl Pts',(-5.597646882,4.964285714,-4.607477551));
#159021=CARTESIAN_POINT('Ctrl Pts',(-5.629619895,4.95614195,-4.568633382));
#159022=CARTESIAN_POINT('Ctrl Pts',(-5.661050747,4.947973174,-4.529349229));
#159023=CARTESIAN_POINT('Ctrl Pts',(-5.458943387,5.000313899,-4.85016575900001));
#159024=CARTESIAN_POINT('Ctrl Pts',(-5.533151567,4.98224132,-4.766643201));
#159025=CARTESIAN_POINT('Ctrl Pts',(-5.604769797,4.964285714,-4.680889479));
#159026=CARTESIAN_POINT('Ctrl Pts',(-5.637252244,4.95614195,-4.641995881));
#159027=CARTESIAN_POINT('Ctrl Pts',(-5.669191793,4.947973174,-4.60265523400001));
#159028=CARTESIAN_POINT('',(-5.67316532544793,4.94797317334228,-4.63843490812138));
#159029=CARTESIAN_POINT('Ctrl Pts',(-5.134458762,4.81863040500001,-5.338416669));
#159030=CARTESIAN_POINT('Ctrl Pts',(-5.140821347,4.820029867,-5.33229717100001));
#159031=CARTESIAN_POINT('Ctrl Pts',(-5.147169327,4.821428571,-5.326162524));
#159032=CARTESIAN_POINT('Ctrl Pts',(-5.43167941,4.884117105,-5.051213803));
#159033=CARTESIAN_POINT('Ctrl Pts',(-5.685279909,4.947973174,-4.747520581));
#159034=CARTESIAN_POINT('Ctrl Pts',(-5.134132729,4.81863040500001,-5.118904289));
#159035=CARTESIAN_POINT('Ctrl Pts',(-5.140233688,4.820029867,-5.11278518));
#159036=CARTESIAN_POINT('Ctrl Pts',(-5.146320044,4.821428571,-5.106651545));
#159037=CARTESIAN_POINT('Ctrl Pts',(-5.41910440800001,4.884117105,-4.831748191));
#159038=CARTESIAN_POINT('Ctrl Pts',(-5.661050747,4.947973174,-4.529349229));
#159039=CARTESIAN_POINT('Ctrl Pts',(-5.13744737984433,4.8193909179173,-5.11557765142939));
#159040=CARTESIAN_POINT('Ctrl Pts',(-5.1503835258232,4.82234724732518,-5.1282067840203));
#159041=CARTESIAN_POINT('Ctrl Pts',(-5.16332353063032,4.8252701031319,-5.14083987093192));
#159042=CARTESIAN_POINT('Ctrl Pts',(-5.17625563150039,4.82816321749342,
-5.15348780056849));
#159043=CARTESIAN_POINT('Ctrl Pts',(-5.18836205414139,4.83087161464878,
-5.16532819550913));
#159044=CARTESIAN_POINT('Ctrl Pts',(-5.20046453379271,4.83355328553066,
-5.17717876839553));
#159045=CARTESIAN_POINT('Ctrl Pts',(-5.21256315969593,4.83620904387903,
-5.1890390397041));
#159046=CARTESIAN_POINT('Ctrl Pts',(-5.22466191549681,4.83886483074111,
-5.20089943835123));
#159047=CARTESIAN_POINT('Ctrl Pts',(-5.23675684956082,4.84149471142401,
-5.21276956729307));
#159048=CARTESIAN_POINT('Ctrl Pts',(-5.24884804582745,4.84409946429349,
-5.22464897735641));
#159049=CARTESIAN_POINT('Ctrl Pts',(-4.76716619730484,4.94924836941368,
-5.66882264040786));
#159050=CARTESIAN_POINT('Ctrl Pts',(-4.77023385315243,4.94861077170684,
-5.66623723320393));
#159051=CARTESIAN_POINT('Ctrl Pts',(-4.773301509,4.94797317400001,-5.663651826));
#159052=CARTESIAN_POINT('Ctrl Pts',(-5.08183265400001,4.88384644,-5.403623099));
#159053=CARTESIAN_POINT('Ctrl Pts',(-5.360291378,4.818610636,-5.11161771400001));
#159054=CARTESIAN_POINT('Ctrl Pts',(-4.54891219022449,4.94924836941368,
-5.64534848929436));
#159055=CARTESIAN_POINT('Ctrl Pts',(-4.55196725961225,4.94861077170684,
-5.64288131064718));
#159056=CARTESIAN_POINT('Ctrl Pts',(-4.555022329,4.94797317400001,-5.640414132));
#159057=CARTESIAN_POINT('Ctrl Pts',(-4.862287584,4.88384644,-5.392276306));
#159058=CARTESIAN_POINT('Ctrl Pts',(-5.14077960699999,4.818610636,-5.112228969));
#159059=CARTESIAN_POINT('',(-4.59169344389577,4.94797317334255,-5.64431809002532));
#159060=CARTESIAN_POINT('Ctrl Pts',(-4.55256109121282,4.94745154526473,
-5.6424017507755));
#159061=CARTESIAN_POINT('Ctrl Pts',(-4.55379171010641,4.94771235963237,
-5.64140794138775));
#159062=CARTESIAN_POINT('Ctrl Pts',(-4.55502232900001,4.947973174,-5.640414132));
#159063=CARTESIAN_POINT('Ctrl Pts',(-4.678242568,4.974088171,-5.540905315));
#159064=CARTESIAN_POINT('Ctrl Pts',(-4.796999593,5.00031307,-5.436110273));
#159065=CARTESIAN_POINT('Ctrl Pts',(-4.62589992017682,4.94745154526473,
-5.65024166521513));
#159066=CARTESIAN_POINT('Ctrl Pts',(-4.62713224258841,4.94771235963237,
-5.64923185410757));
#159067=CARTESIAN_POINT('Ctrl Pts',(-4.628364565,4.947973174,-5.648222043));
#159068=CARTESIAN_POINT('Ctrl Pts',(-4.751755375,4.974088171,-5.547110995));
#159069=CARTESIAN_POINT('Ctrl Pts',(-4.870612837,5.00031307,-5.440707802));
#159070=CARTESIAN_POINT('Origin',(0.141090112662756,5.08925706339396,0.137616244610315));
#159071=CARTESIAN_POINT('Ctrl Pts',(-4.546815687,4.94766207,-5.704740794));
#159072=CARTESIAN_POINT('Ctrl Pts',(-4.672183892,4.97393188700001,-5.604819318));
#159073=CARTESIAN_POINT('Ctrl Pts',(-4.793041404,5.00031307,-5.49948675));
#159074=CARTESIAN_POINT('Ctrl Pts',(-4.553554251,4.94766207,-5.641599391));
#159075=CARTESIAN_POINT('Ctrl Pts',(-4.677534851,4.97393188700001,-5.541529827));
#159076=CARTESIAN_POINT('Ctrl Pts',(-4.796999593,5.00031307,-5.436110273));
#159077=CARTESIAN_POINT('Ctrl Pts',(-4.55502392165559,4.94797287218644,
-5.64041298053945));
#159078=CARTESIAN_POINT('Ctrl Pts',(-4.55827239943767,4.9488276974756,-5.64450259314184));
#159079=CARTESIAN_POINT('Ctrl Pts',(-4.56152202378497,4.94967947059951,
-5.64859193398487));
#159080=CARTESIAN_POINT('Ctrl Pts',(-4.56477122964979,4.95052852747181,
-5.65268216973473));
#159081=CARTESIAN_POINT('Ctrl Pts',(-4.56778766590997,4.95131675882528,
-5.65647938540585));
#159082=CARTESIAN_POINT('Ctrl Pts',(-4.57080374237042,4.95210264920943,
-5.66027737362154));
#159083=CARTESIAN_POINT('Ctrl Pts',(-4.57381946092239,4.95288622033308,
-5.66407612355446));
#159084=CARTESIAN_POINT('Ctrl Pts',(-4.57683518252117,4.95366979224837,
-5.66787487732529));
#159085=CARTESIAN_POINT('Ctrl Pts',(-4.57985054697082,4.95445104509583,
-5.67167439377354));
#159086=CARTESIAN_POINT('Ctrl Pts',(-4.58286555616587,4.95523000030221,
-5.67547466231674));
#159087=CARTESIAN_POINT('Ctrl Pts',(-4.362517003,5.000313899,-5.846883427));
#159088=CARTESIAN_POINT('Ctrl Pts',(-4.451975096,4.98224132,-5.780136338));
#159089=CARTESIAN_POINT('Ctrl Pts',(-4.539349314,4.964285714,-5.710683691));
#159090=CARTESIAN_POINT('Ctrl Pts',(-4.579735474,4.955986264,-5.67858125));
#159091=CARTESIAN_POINT('Ctrl Pts',(-4.619663557,4.947660853,-5.645910824));
#159092=CARTESIAN_POINT('Ctrl Pts',(-4.29973517,5.000313899,-5.837360488));
#159093=CARTESIAN_POINT('Ctrl Pts',(-4.38904756,4.98224132,-5.77157397));
#159094=CARTESIAN_POINT('Ctrl Pts',(-4.476305531,4.964285714,-5.703085901));
#159095=CARTESIAN_POINT('Ctrl Pts',(-4.516637959,4.955986264,-5.671429308));
#159096=CARTESIAN_POINT('Ctrl Pts',(-4.556518621,4.947660853,-5.639205445));
#159097=CARTESIAN_POINT('Ctrl Pts',(-4.55502314960303,4.94797303331433,
-5.64041360402221));
#159098=CARTESIAN_POINT('Ctrl Pts',(-4.52890923100112,4.95342302539129,
-5.66150229278074));
#159099=CARTESIAN_POINT('Ctrl Pts',(-4.50266855884138,4.95886083277496,
-5.68239377597682));
#159100=CARTESIAN_POINT('Ctrl Pts',(-4.47630553123975,4.96428571399719,
-5.70308590101651));
#159101=CARTESIAN_POINT('Ctrl Pts',(-4.41873725026119,4.97613189112419,
-5.74827077517629));
#159102=CARTESIAN_POINT('Ctrl Pts',(-4.36038638074774,4.98803923912244,
-5.79266092730607));
#159103=CARTESIAN_POINT('Ctrl Pts',(-4.30128630597296,5.00000000033185,
-5.83621762044319));
#159104=CARTESIAN_POINT('Ctrl Pts',(-4.29973517,5.000313899,-5.837360488));
#159105=CARTESIAN_POINT('Ctrl Pts',(-4.38904756,4.98224132,-5.77157397));
#159106=CARTESIAN_POINT('Ctrl Pts',(-4.476305531,4.964285714,-5.703085901));
#159107=CARTESIAN_POINT('Ctrl Pts',(-4.515881381,4.95614195,-5.672023139));
#159108=CARTESIAN_POINT('Ctrl Pts',(-4.555022329,4.947973174,-5.640414132));
#159109=CARTESIAN_POINT('Ctrl Pts',(-4.288674056,5.000313899,-5.910283042));
#159110=CARTESIAN_POINT('Ctrl Pts',(-4.379102171,4.98224132,-5.844665759));
#159111=CARTESIAN_POINT('Ctrl Pts',(-4.467480522,4.964285714,-5.776312715));
#159112=CARTESIAN_POINT('Ctrl Pts',(-4.507564521,4.95614195,-5.745311193));
#159113=CARTESIAN_POINT('Ctrl Pts',(-4.54721441799999,4.947973174,-5.713756368));
#159114=CARTESIAN_POINT('',(-4.54340347883659,4.94797317334228,-5.74955372499979));
#159115=CARTESIAN_POINT('Ctrl Pts',(-3.866816188,4.818630405,-6.317364314));
#159116=CARTESIAN_POINT('Ctrl Pts',(-3.874345531,4.820029867,-6.312755654));
#159117=CARTESIAN_POINT('Ctrl Pts',(-3.881863866,4.821428571,-6.30812906));
#159118=CARTESIAN_POINT('Ctrl Pts',(-4.218828109,4.884117105,-6.10076974500001));
#159119=CARTESIAN_POINT('Ctrl Pts',(-4.531784635,4.947973174,-5.858693313));
#159120=CARTESIAN_POINT('Ctrl Pts',(-3.91368645,4.818630405,-6.102913924));
#159121=CARTESIAN_POINT('Ctrl Pts',(-3.9209602,4.820029867,-6.098249402));
#159122=CARTESIAN_POINT('Ctrl Pts',(-3.928222811,4.821428571,-6.093567555));
#159123=CARTESIAN_POINT('Ctrl Pts',(-4.253725723,4.884117105,-5.883731863));
#159124=CARTESIAN_POINT('Ctrl Pts',(-4.555022329,4.947973174,-5.640414132));
#159125=CARTESIAN_POINT('Ctrl Pts',(-3.91763873527576,4.81939091791743,
-6.10037761323303));
#159126=CARTESIAN_POINT('Ctrl Pts',(-3.92755755152312,4.8223472472166,-6.11549237277444));
#159127=CARTESIAN_POINT('Ctrl Pts',(-3.93747928571279,4.82527010307455,
-6.13061182384926));
#159128=CARTESIAN_POINT('Ctrl Pts',(-3.94739011022992,4.82816321744659,
-6.14574407138381));
#159129=CARTESIAN_POINT('Ctrl Pts',(-3.95666815648934,4.8308716146068,-6.15991016749337));
#159130=CARTESIAN_POINT('Ctrl Pts',(-3.96594016399411,4.83355328549382,
-6.17408535596271));
#159131=CARTESIAN_POINT('Ctrl Pts',(-3.97520632298064,4.83620904384735,
-6.18826918766501));
#159132=CARTESIAN_POINT('Ctrl Pts',(-3.98447258145384,4.83886483071459,
-6.20245317165289));
#159133=CARTESIAN_POINT('Ctrl Pts',(-3.99373301581997,4.84149471140265,
-6.21664583688259));
#159134=CARTESIAN_POINT('Ctrl Pts',(-4.00298780463037,4.84409946428194,
-6.23084676275461));
#159135=CARTESIAN_POINT('Ctrl Pts',(-3.43708320223719,4.94924836941368,
-6.56108853400832));
#159136=CARTESIAN_POINT('Ctrl Pts',(-3.4406349241186,4.94861077170685,-6.55922302750416));
#159137=CARTESIAN_POINT('Ctrl Pts',(-3.444186646,4.947973174,-6.557357521));
#159138=CARTESIAN_POINT('Ctrl Pts',(-3.801402994,4.88384644,-6.369733196));
#159139=CARTESIAN_POINT('Ctrl Pts',(-4.136124034,4.818610636,-6.14441513));
#159140=CARTESIAN_POINT('Ctrl Pts',(-3.22897810090943,4.94924836941368,
-6.49124503453278));
#159141=CARTESIAN_POINT('Ctrl Pts',(-3.23249211495472,4.94861077170685,
-6.48949228676639));
#159142=CARTESIAN_POINT('Ctrl Pts',(-3.236006129,4.947973174,-6.487739539));
#159143=CARTESIAN_POINT('Ctrl Pts',(-3.589429991,4.88384644,-6.311455985));
#159144=CARTESIAN_POINT('Ctrl Pts',(-3.921612925,4.818610636,-6.097823552));
#159145=CARTESIAN_POINT('',(-3.27098065792544,4.94797317334254,-6.49943543079898));
#159146=CARTESIAN_POINT('Ctrl Pts',(-3.23317515431105,4.94745154526474,
-6.48915159497978));
#159147=CARTESIAN_POINT('Ctrl Pts',(-3.23459064165553,4.94771235963237,
-6.48844556698989));
#159148=CARTESIAN_POINT('Ctrl Pts',(-3.236006129,4.947973174,-6.487739539));
#159149=CARTESIAN_POINT('Ctrl Pts',(-3.377737001,4.974088171,-6.417045892));
#159150=CARTESIAN_POINT('Ctrl Pts',(-3.51624539,5.00031307,-6.34023015));
#159151=CARTESIAN_POINT('Ctrl Pts',(-3.30311401212512,4.94745154526474,
-6.51257389780459));
#159152=CARTESIAN_POINT('Ctrl Pts',(-3.30453460306256,4.94771235963237,
-6.5118526084023));
#159153=CARTESIAN_POINT('Ctrl Pts',(-3.305955194,4.947973174,-6.511131319));
#159154=CARTESIAN_POINT('Ctrl Pts',(-3.448197082,4.974088171,-6.438909567));
#159155=CARTESIAN_POINT('Ctrl Pts',(-3.587149265,5.00031307,-6.360544862));
#159156=CARTESIAN_POINT('Origin',(0.10820841979828,5.0892568791216,0.164729784140485));
#159157=CARTESIAN_POINT('Ctrl Pts',(-3.214163023,4.94766207,-6.54879809400001));
#159158=CARTESIAN_POINT('Ctrl Pts',(-3.358080353,4.973931887,-6.478163184));
#159159=CARTESIAN_POINT('Ctrl Pts',(-3.498755672,5.00031307,-6.401274026));
#159160=CARTESIAN_POINT('Ctrl Pts',(-3.234317579,4.94766207,-6.488581494));
#159161=CARTESIAN_POINT('Ctrl Pts',(-3.376911579,4.973931887,-6.417503665));
#159162=CARTESIAN_POINT('Ctrl Pts',(-3.51624539,5.00031307,-6.34023015));
#159163=CARTESIAN_POINT('Ctrl Pts',(-3.23600793233001,4.94797287199268,
-6.4877387569128));
#159164=CARTESIAN_POINT('Ctrl Pts',(-3.238301316439,4.94882769736909,-6.49243108356366));
#159165=CARTESIAN_POINT('Ctrl Pts',(-3.2405958789538,4.94967947050675,-6.49712339103697));
#159166=CARTESIAN_POINT('Ctrl Pts',(-3.24288984038026,4.95052852738732,
-6.50181648251531));
#159167=CARTESIAN_POINT('Ctrl Pts',(-3.24501946491259,4.95131675875919,
-6.50617336603982));
#159168=CARTESIAN_POINT('Ctrl Pts',(-3.24714857197188,4.95210264915641,
-6.51053092668283));
#159169=CARTESIAN_POINT('Ctrl Pts',(-3.24927716574165,4.95288622029139,
-6.51488915429613));
#159170=CARTESIAN_POINT('Ctrl Pts',(-3.25140576166195,4.95366979221801,
-6.51924738631258));
#159171=CARTESIAN_POINT('Ctrl Pts',(-3.25353384482793,4.9544510450751,-6.52360628640031));
#159172=CARTESIAN_POINT('Ctrl Pts',(-3.25566141942808,4.95523000031271,
-6.52796584476247));
#159173=CARTESIAN_POINT('Ctrl Pts',(-3.003616676,5.000313899,-6.64799874200001));
#159174=CARTESIAN_POINT('Ctrl Pts',(-3.105331939,4.98224132,-6.602043008));
#159175=CARTESIAN_POINT('Ctrl Pts',(-3.205593663,4.964285714,-6.552997));
#159176=CARTESIAN_POINT('Ctrl Pts',(-3.251936692,4.955986264,-6.530326927));
#159177=CARTESIAN_POINT('Ctrl Pts',(-3.297954455,4.947660853,-6.507003675));
#159178=CARTESIAN_POINT('Ctrl Pts',(-2.944349797,5.000313899,-6.625202206));
#159179=CARTESIAN_POINT('Ctrl Pts',(-3.04571627,4.98224132,-6.580153264));
#159180=CARTESIAN_POINT('Ctrl Pts',(-3.145657109,4.964285714,-6.532024292));
#159181=CARTESIAN_POINT('Ctrl Pts',(-3.191851818,4.955986264,-6.50977809300001));
#159182=CARTESIAN_POINT('Ctrl Pts',(-3.237727271,4.947660853,-6.48688077));
#159183=CARTESIAN_POINT('Ctrl Pts',(-3.23600612947942,4.94797317382086,
-6.48773954002634));
#159184=CARTESIAN_POINT('Ctrl Pts',(-3.18821456999116,4.9566446780338,-6.51157739400629));
#159185=CARTESIAN_POINT('Ctrl Pts',(-3.14020122808787,4.96527388257548,
-6.53486694554253));
#159186=CARTESIAN_POINT('Ctrl Pts',(-3.04355614826285,4.9826013876045,-6.58043498550645));
#159187=CARTESIAN_POINT('Ctrl Pts',(-2.99495714815925,4.99129055431876,
-6.60269563274663));
#159188=CARTESIAN_POINT('Ctrl Pts',(-2.94611035073432,5.00000000038334,
-6.62441950656244));
#159189=CARTESIAN_POINT('Ctrl Pts',(-2.944349797,5.000313899,-6.625202206));
#159190=CARTESIAN_POINT('Ctrl Pts',(-3.04571627,4.98224132,-6.580153264));
#159191=CARTESIAN_POINT('Ctrl Pts',(-3.145657109,4.964285714,-6.532024292));
#159192=CARTESIAN_POINT('Ctrl Pts',(-3.190985273,4.95614195,-6.510195399));
#159193=CARTESIAN_POINT('Ctrl Pts',(-3.236006129,4.947973174,-6.487739539));
#159194=CARTESIAN_POINT('Ctrl Pts',(-2.917871093,5.000313899,-6.694042058));
#159195=CARTESIAN_POINT('Ctrl Pts',(-3.020290825,4.98224132,-6.649398243));
#159196=CARTESIAN_POINT('Ctrl Pts',(-3.121296823,4.964285714,-6.601641988));
#159197=CARTESIAN_POINT('Ctrl Pts',(-3.167108091,4.95614195,-6.579982139));
#159198=CARTESIAN_POINT('Ctrl Pts',(-3.21261435,4.947973174,-6.557688604));
#159199=CARTESIAN_POINT('',(-3.20119713487288,4.94797317334223,-6.59182979976144));
#159200=CARTESIAN_POINT('Ctrl Pts',(-2.418365587,4.818630405,-7.000919025));
#159201=CARTESIAN_POINT('Ctrl Pts',(-2.426709623,4.820029867,-6.998036699));
#159202=CARTESIAN_POINT('Ctrl Pts',(-2.435046765,4.821428571,-6.995134492));
#159203=CARTESIAN_POINT('Ctrl Pts',(-2.808709094,4.884117105,-6.865060475));
#159204=CARTESIAN_POINT('Ctrl Pts',(-3.166388148,4.947973174,-6.695920057));
#159205=CARTESIAN_POINT('Ctrl Pts',(-2.510240543,4.818630405,-6.801558087));
#159206=CARTESIAN_POINT('Ctrl Pts',(-2.518346971,4.820029867,-6.79856626));
#159207=CARTESIAN_POINT('Ctrl Pts',(-2.526446244,4.821428571,-6.795555119));
#159208=CARTESIAN_POINT('Ctrl Pts',(-2.88944755,4.884117105,-6.660598773));
#159209=CARTESIAN_POINT('Ctrl Pts',(-3.236006129,4.947973174,-6.487739539));
#159210=CARTESIAN_POINT('Ctrl Pts',(-2.51464565778541,4.81939091791719,
-6.79993069839959));
#159211=CARTESIAN_POINT('Ctrl Pts',(-2.5210833505913,4.82234724728871,-6.81682433556511));
#159212=CARTESIAN_POINT('Ctrl Pts',(-2.52752288517145,4.82527010314086,
-6.83372318185064));
#159213=CARTESIAN_POINT('Ctrl Pts',(-2.53394901425799,4.82816321751078,
-6.85063218017267));
#159214=CARTESIAN_POINT('Ctrl Pts',(-2.53996485306458,4.83087161466,-6.86646158647879));
#159215=CARTESIAN_POINT('Ctrl Pts',(-2.54597283970855,4.83355328553621,
-6.88229857441741));
#159216=CARTESIAN_POINT('Ctrl Pts',(-2.55197325652855,4.83620904387925,
-6.89814274625689));
#159217=CARTESIAN_POINT('Ctrl Pts',(-2.55797373777239,4.838864830736,-6.9139870882083));
#159218=CARTESIAN_POINT('Ctrl Pts',(-2.56396666486193,4.84149471141391,
-6.92983865642847));
#159219=CARTESIAN_POINT('Ctrl Pts',(-2.56995230260316,4.84409946428864,
-6.94569707856559));
#159220=CARTESIAN_POINT('Ctrl Pts',(-1.9462860173166,4.94924836941368,-7.14656521854563));
#159221=CARTESIAN_POINT('Ctrl Pts',(-1.9501557306583,4.94861077170684,-7.14550684177282));
#159222=CARTESIAN_POINT('Ctrl Pts',(-1.954025444,4.947973174,-7.144448465));
#159223=CARTESIAN_POINT('Ctrl Pts',(-2.343223955,4.88384644,-7.038001649));
#159224=CARTESIAN_POINT('Ctrl Pts',(-2.718556127,4.818610636,-6.889906523));
#159225=CARTESIAN_POINT('Ctrl Pts',(-1.75806058539699,4.94924836941368,
-7.03361817669735));
#159226=CARTESIAN_POINT('Ctrl Pts',(-1.76186923269849,4.94861077170684,
-7.03266181634868));
#159227=CARTESIAN_POINT('Ctrl Pts',(-1.76567788,4.947973174,-7.031705456));
#159228=CARTESIAN_POINT('Ctrl Pts',(-2.148734641,4.88384644,-6.935518997));
#159229=CARTESIAN_POINT('Ctrl Pts',(-2.519075981,4.818610636,-6.798290683));
#159230=CARTESIAN_POINT('',(-1.79732045262188,4.94797317334248,-7.05064639398859));
#159231=CARTESIAN_POINT('Ctrl Pts',(-1.76260954163828,4.94745154526473,
-7.0324759230231));
#159232=CARTESIAN_POINT('Ctrl Pts',(-1.76414371081914,4.94771235963237,
-7.03209068951155));
#159233=CARTESIAN_POINT('Ctrl Pts',(-1.76567788,4.947973174,-7.031705456));
#159234=CARTESIAN_POINT('Ctrl Pts',(-1.919292207,4.97408817100001,-6.993132535));
#159235=CARTESIAN_POINT('Ctrl Pts',(-2.07107546,5.00031307,-6.947887912));
#159236=CARTESIAN_POINT('Ctrl Pts',(-1.82587816458829,4.94745154526473,
-7.07038541198959));
#159237=CARTESIAN_POINT('Ctrl Pts',(-1.82742059879415,4.94771235963237,
-7.06998637099479));
#159238=CARTESIAN_POINT('Ctrl Pts',(-1.828963033,4.947973174,-7.06958733));
#159239=CARTESIAN_POINT('Ctrl Pts',(-1.983404926,4.97408817100001,-7.029631884));
#159240=CARTESIAN_POINT('Ctrl Pts',(-2.135954579,5.00031307,-6.982969915));
#159241=CARTESIAN_POINT('Origin',(0.0702666180962777,5.08925695913635,0.184140373501591));
#159242=CARTESIAN_POINT('Ctrl Pts',(-1.731219669,4.94766207,-7.086640874));
#159243=CARTESIAN_POINT('Ctrl Pts',(-1.886956709,4.97393188700001,-7.048595341));
#159244=CARTESIAN_POINT('Ctrl Pts',(-2.040872013,5.00031307,-7.003744844));
#159245=CARTESIAN_POINT('Ctrl Pts',(-1.763847811,4.94766207,-7.032164738));
#159246=CARTESIAN_POINT('Ctrl Pts',(-1.918387675,4.97393188700001,-6.993402164));
#159247=CARTESIAN_POINT('Ctrl Pts',(-2.07107546,5.00031307,-6.947887912));
#159248=CARTESIAN_POINT('Ctrl Pts',(-1.76567980883721,4.94797287199132,
-7.03170507974775));
#159249=CARTESIAN_POINT('Ctrl Pts',(-1.76691086312142,4.94882769741292,
-7.03678071229921));
#159250=CARTESIAN_POINT('Ctrl Pts',(-1.76814307271491,4.94967947055106,
-7.04185657940211));
#159251=CARTESIAN_POINT('Ctrl Pts',(-1.76937452674259,4.9505285274352,-7.04693308296692));
#159252=CARTESIAN_POINT('Ctrl Pts',(-1.77051776072215,4.95131675879317,
-7.05164591125135));
#159253=CARTESIAN_POINT('Ctrl Pts',(-1.77166034377292,4.95210264917935,
-7.05635928958518));
#159254=CARTESIAN_POINT('Ctrl Pts',(-1.772802282163,4.95288622030561,-7.06107320895169));
#159255=CARTESIAN_POINT('Ctrl Pts',(-1.77394422170679,4.95366979222352,
-7.06578713308069));
#159256=CARTESIAN_POINT('Ctrl Pts',(-1.77508551687588,4.95445104507422,
-7.07050159943266));
#159257=CARTESIAN_POINT('Ctrl Pts',(-1.77622617387012,4.95523000030894,
-7.07521659934531));
#159258=CARTESIAN_POINT('Ctrl Pts',(-1.504270571,5.000313899,-7.138261025));
#159259=CARTESIAN_POINT('Ctrl Pts',(-1.613486912,4.98224132,-7.11524548600001));
#159260=CARTESIAN_POINT('Ctrl Pts',(-1.721948015,4.964285714,-7.088899452));
#159261=CARTESIAN_POINT('Ctrl Pts',(-1.772080965,4.955986264,-7.07672177400001));
#159262=CARTESIAN_POINT('Ctrl Pts',(-1.822036668,4.947660853,-7.063836266));
#159263=CARTESIAN_POINT('Ctrl Pts',(-1.4512899,5.000313899,-7.103256832));
#159264=CARTESIAN_POINT('Ctrl Pts',(-1.559970672,4.98224132,-7.081051904));
#159265=CARTESIAN_POINT('Ctrl Pts',(-1.667921256,4.964285714,-7.055532488));
#159266=CARTESIAN_POINT('Ctrl Pts',(-1.717818234,4.955986264,-7.043736889));
#159267=CARTESIAN_POINT('Ctrl Pts',(-1.767543392,4.947660853,-7.031236759));
#159268=CARTESIAN_POINT('Ctrl Pts',(-1.7656778802699,4.9479731738047,-7.03170545720505));
#159269=CARTESIAN_POINT('Ctrl Pts',(-1.71387924127078,4.95664467553049,
-7.04471221882473));
#159270=CARTESIAN_POINT('Ctrl Pts',(-1.66198186828356,4.96527387858945,
-7.05713582273003));
#159271=CARTESIAN_POINT('Ctrl Pts',(-1.55780371363979,4.98260085164332,
-7.08086194272409));
#159272=CARTESIAN_POINT('Ctrl Pts',(-1.50554913342956,4.99129108543522,
-7.09215618765466));
#159273=CARTESIAN_POINT('Ctrl Pts',(-1.45317754970485,5.00000000046694,
-7.10287089874499));
#159274=CARTESIAN_POINT('Ctrl Pts',(-1.4512899,5.000313899,-7.103256832));
#159275=CARTESIAN_POINT('Ctrl Pts',(-1.559970672,4.98224132,-7.081051904));
#159276=CARTESIAN_POINT('Ctrl Pts',(-1.667921256,4.964285714,-7.055532488));
#159277=CARTESIAN_POINT('Ctrl Pts',(-1.71688224,4.95614195,-7.04395815700001));
#159278=CARTESIAN_POINT('Ctrl Pts',(-1.76567788,4.947973174,-7.031705456));
#159279=CARTESIAN_POINT('Ctrl Pts',(-1.41063172,5.000313899,-7.16479510800001));
#159280=CARTESIAN_POINT('Ctrl Pts',(-1.520254036,4.98224132,-7.143212256));
#159281=CARTESIAN_POINT('Ctrl Pts',(-1.629164754,4.964285714,-7.118285819));
#159282=CARTESIAN_POINT('Ctrl Pts',(-1.678561207,4.95614195,-7.106980434));
#159283=CARTESIAN_POINT('Ctrl Pts',(-1.727796006,4.947973174,-7.09499061));
#159284=CARTESIAN_POINT('',(-1.70930637157898,4.94797317334222,-7.12587923944055));
#159285=CARTESIAN_POINT('Ctrl Pts',(-0.856834899,4.818630405,-7.357118544));
#159286=CARTESIAN_POINT('Ctrl Pts',(-0.865603471,4.820029867,-7.35609732600001));
#159287=CARTESIAN_POINT('Ctrl Pts',(-0.874369584,4.821428571,-7.35505521));
#159288=CARTESIAN_POINT('Ctrl Pts',(-1.267257964,4.884117105,-7.308348606));
#159289=CARTESIAN_POINT('Ctrl Pts',(-1.652934871,4.947973174,-7.220053021));
#159290=CARTESIAN_POINT('Ctrl Pts',(-0.989418577999999,4.818630405,-7.182168954));
#159291=CARTESIAN_POINT('Ctrl Pts',(-0.997978637,4.820029867,-7.180989716));
#159292=CARTESIAN_POINT('Ctrl Pts',(-1.00653586,4.821428571,-7.179790078));
#159293=CARTESIAN_POINT('Ctrl Pts',(-1.390062022,4.884117105,-7.126023487));
#159294=CARTESIAN_POINT('Ctrl Pts',(-1.76567788,4.947973174,-7.031705456));
#159295=CARTESIAN_POINT('Ctrl Pts',(-0.994070543748172,4.81939091801866,
-7.18152658130227));
#159296=CARTESIAN_POINT('Ctrl Pts',(-0.996726094868206,4.82234724727202,
-7.19940916869544));
#159297=CARTESIAN_POINT('Ctrl Pts',(-0.999382324343524,4.82527010312014,
-7.2172972388855));
#159298=CARTESIAN_POINT('Ctrl Pts',(-1.00202327928225,4.82816321749345,
-7.2351923419871));
#159299=CARTESIAN_POINT('Ctrl Pts',(-1.00449561666861,4.830871614643,-7.25194489303674));
#159300=CARTESIAN_POINT('Ctrl Pts',(-1.0069586556332,4.83355328551821,-7.26870316048359));
#159301=CARTESIAN_POINT('Ctrl Pts',(-1.00941275741717,4.83620904385919,
-7.2854668165887));
#159302=CARTESIAN_POINT('Ctrl Pts',(-1.01186688554976,4.83886483071389,
-7.3022306526779));
#159303=CARTESIAN_POINT('Ctrl Pts',(-1.01431208269721,4.84149471138868,
-7.31899992217128));
#159304=CARTESIAN_POINT('Ctrl Pts',(-1.01674868753842,4.84409946427727,
-7.33577431846203));
#159305=CARTESIAN_POINT('Ctrl Pts',(-0.364482660369833,4.94924836941368,
-7.39787645705584));
#159306=CARTESIAN_POINT('Ctrl Pts',(-0.368489421684916,4.94861077170684,
-7.39767469852792));
#159307=CARTESIAN_POINT('Ctrl Pts',(-0.372496183,4.947973174,-7.39747294));
#159308=CARTESIAN_POINT('Ctrl Pts',(-0.775478368,4.88384644,-7.377180967));
#159309=CARTESIAN_POINT('Ctrl Pts',(-1.173871557,4.818610636,-7.313233544));
#159310=CARTESIAN_POINT('Ctrl Pts',(-0.204938109066286,4.94924836941368,
-7.24710715016634));
#159311=CARTESIAN_POINT('Ctrl Pts',(-0.208863301533143,4.94861077170684,
-7.24699189558318));
#159312=CARTESIAN_POINT('Ctrl Pts',(-0.212788494,4.947973174,-7.246876641));
#159313=CARTESIAN_POINT('Ctrl Pts',(-0.607566848,4.88384644,-7.235284849));
#159314=CARTESIAN_POINT('Ctrl Pts',(-0.998749843,4.818610636,-7.180877297));
#159315=CARTESIAN_POINT('',(-0.239619539500027,4.94797317334248,-7.2721769681318));
#159316=CARTESIAN_POINT('Ctrl Pts',(-0.209626264033116,4.94745154526473,
-7.24696949288303));
#159317=CARTESIAN_POINT('Ctrl Pts',(-0.211207379016558,4.94771235963237,
-7.24692306694152));
#159318=CARTESIAN_POINT('Ctrl Pts',(-0.212788494,4.947973174,-7.246876641));
#159319=CARTESIAN_POINT('Ctrl Pts',(-0.371103442,4.97408817100001,-7.242228073));
#159320=CARTESIAN_POINT('Ctrl Pts',(-0.529064344,5.00031307,-7.230670157));
#159321=CARTESIAN_POINT('Ctrl Pts',(-0.263266283044498,4.94745154526473,
-7.2975935627527));
#159322=CARTESIAN_POINT('Ctrl Pts',(-0.264858438022249,4.94771235963237,
-7.29753542887635));
#159323=CARTESIAN_POINT('Ctrl Pts',(-0.266450593,4.947973174,-7.297477295));
#159324=CARTESIAN_POINT('Ctrl Pts',(-0.425870961,4.97408817100001,-7.291656427));
#159325=CARTESIAN_POINT('Ctrl Pts',(-0.584885032,5.00031307,-7.278879055));
#159326=CARTESIAN_POINT('Origin',(0.0290390952789225,5.08925700087071,0.194940675385882));
#159327=CARTESIAN_POINT('Ctrl Pts',(-0.167326407,4.94766207,-7.293120202));
#159328=CARTESIAN_POINT('Ctrl Pts',(-0.327601066,4.973931887,-7.289443013));
#159329=CARTESIAN_POINT('Ctrl Pts',(-0.487559448,5.00031307,-7.278728336));
#159330=CARTESIAN_POINT('Ctrl Pts',(-0.21090248,4.94766207,-7.246931774));
#159331=CARTESIAN_POINT('Ctrl Pts',(-0.370162096,4.973931887,-7.242296951));
#159332=CARTESIAN_POINT('Ctrl Pts',(-0.529064344,5.00031307,-7.230670157));
#159333=CARTESIAN_POINT('Ctrl Pts',(-0.212790459169118,4.94797287208577,
-7.24687668792547));
#159334=CARTESIAN_POINT('Ctrl Pts',(-0.21290162157793,4.94882769743312,
-7.25209829529905));
#159335=CARTESIAN_POINT('Ctrl Pts',(-0.213013861400536,4.94967947056244,
-7.25732038006634));
#159336=CARTESIAN_POINT('Ctrl Pts',(-0.213125226487645,4.95052852743733,
-7.26254292398658));
#159337=CARTESIAN_POINT('Ctrl Pts',(-0.213228613500719,4.95131675879874,
-7.26739133052561));
#159338=CARTESIAN_POINT('Ctrl Pts',(-0.213331246546994,4.95210264918784,
-7.27224013431917));
#159339=CARTESIAN_POINT('Ctrl Pts',(-0.213433133688945,4.95288622031736,
-7.2770893279135));
#159340=CARTESIAN_POINT('Ctrl Pts',(-0.213535020933834,4.95366979223853,
-7.28193852640701));
#159341=CARTESIAN_POINT('Ctrl Pts',(-0.213636162297835,4.95445104509289,
-7.28678811592523));
#159342=CARTESIAN_POINT('Ctrl Pts',(-0.213736565703542,4.95523000035635,
-7.29163808949555));
#159343=CARTESIAN_POINT('Ctrl Pts',(0.0654135539999999,5.000313899,-7.29474615600001));
#159344=CARTESIAN_POINT('Ctrl Pts',(-0.0461970310000001,4.98224132,-7.29574699200001));
#159345=CARTESIAN_POINT('Ctrl Pts',(-0.157785991,4.964285714,-7.293332845));
#159346=CARTESIAN_POINT('Ctrl Pts',(-0.209364702,4.955986264,-7.292216977));
#159347=CARTESIAN_POINT('Ctrl Pts',(-0.260922472,4.947660853,-7.290371724));
#159348=CARTESIAN_POINT('Ctrl Pts',(0.1096307,5.000313899,-7.249171064));
#159349=CARTESIAN_POINT('Ctrl Pts',(-0.00128258,4.98224132,-7.250848428));
#159350=CARTESIAN_POINT('Ctrl Pts',(-0.112195259,4.964285714,-7.249131826));
#159351=CARTESIAN_POINT('Ctrl Pts',(-0.163461379,4.955986264,-7.248338377));
#159352=CARTESIAN_POINT('Ctrl Pts',(-0.214711149,4.947660853,-7.24681993199999));
#159353=CARTESIAN_POINT('Ctrl Pts',(-0.212789467012575,4.94797303324862,
-7.24687671705583));
#159354=CARTESIAN_POINT('Ctrl Pts',(-0.179238027472989,4.9534230253913,
-7.24786180670163));
#159355=CARTESIAN_POINT('Ctrl Pts',(-0.145705023109152,4.95886083279325,
-7.24861319334356));
#159356=CARTESIAN_POINT('Ctrl Pts',(-0.112195259296336,4.96428571396278,
-7.24913182606086));
#159357=CARTESIAN_POINT('Ctrl Pts',(-0.0390208298553256,4.97613189092785,
-7.25026435090952));
#159358=CARTESIAN_POINT('Ctrl Pts',(0.0342956684092139,4.98803923897761,
-7.25029060206938));
#159359=CARTESIAN_POINT('Ctrl Pts',(0.107704216070518,5.00000000011363,
-7.24919994256545));
#159360=CARTESIAN_POINT('Ctrl Pts',(0.1096307,5.000313899,-7.249171064));
#159361=CARTESIAN_POINT('Ctrl Pts',(-0.00128258,4.98224132,-7.250848428));
#159362=CARTESIAN_POINT('Ctrl Pts',(-0.112195259,4.964285714,-7.249131826));
#159363=CARTESIAN_POINT('Ctrl Pts',(-0.162499702,4.95614195,-7.248353261));
#159364=CARTESIAN_POINT('Ctrl Pts',(-0.212788494,4.947973174,-7.246876641));
#159365=CARTESIAN_POINT('Ctrl Pts',(0.162567224,5.000313899,-7.300530302));
#159366=CARTESIAN_POINT('Ctrl Pts',(0.050868142,4.98224132,-7.30301760200001));
#159367=CARTESIAN_POINT('Ctrl Pts',(-0.060854751,4.964285714,-7.302086516));
#159368=CARTESIAN_POINT('Ctrl Pts',(-0.111526666,4.95614195,-7.301664223));
#159369=CARTESIAN_POINT('Ctrl Pts',(-0.162187841,4.947973174,-7.30053874));
#159370=CARTESIAN_POINT('',(-0.137490340968732,4.94797317334227,-7.32673048557565));
#159371=CARTESIAN_POINT('Ctrl Pts',(0.744760437,4.818630405,-7.369307376));
#159372=CARTESIAN_POINT('Ctrl Pts',(0.735977338000001,4.820029867,-7.370195018));
#159373=CARTESIAN_POINT('Ctrl Pts',(0.727192148,4.821428571,-7.371061721));
#159374=CARTESIAN_POINT('Ctrl Pts',(0.33344874,4.884117105,-7.409906479));
#159375=CARTESIAN_POINT('Ctrl Pts',(-0.062192196,4.947973174,-7.40658433));
#159376=CARTESIAN_POINT('Ctrl Pts',(0.5776675,4.818630405,-7.226949582));
#159377=CARTESIAN_POINT('Ctrl Pts',(0.56905407,4.820029867,-7.227638074));
#159378=CARTESIAN_POINT('Ctrl Pts',(0.560439023,4.821428571,-7.228306033));
#159379=CARTESIAN_POINT('Ctrl Pts',(0.174321262,4.884117105,-7.258243263));
#159380=CARTESIAN_POINT('Ctrl Pts',(-0.212788494,4.947973174,-7.246876641));
#159381=CARTESIAN_POINT('Ctrl Pts',(0.572986203940172,4.8193909179172,-7.22732226363947));
#159382=CARTESIAN_POINT('Ctrl Pts',(0.57423696565771,4.82234724734176,-7.24535763046555));
#159383=CARTESIAN_POINT('Ctrl Pts',(0.575488243539231,4.8252701031345,-7.26339849828819));
#159384=CARTESIAN_POINT('Ctrl Pts',(0.576755950933578,4.82816321749379,
-7.28144295100099));
#159385=CARTESIAN_POINT('Ctrl Pts',(0.577942718779974,4.83087161464669,
-7.29833531621148));
#159386=CARTESIAN_POINT('Ctrl Pts',(0.579139796495352,4.83355328552718,
-7.31523126528801));
#159387=CARTESIAN_POINT('Ctrl Pts',(0.580346760832532,4.83620904387485,
-7.33213055581014));
#159388=CARTESIAN_POINT('Ctrl Pts',(0.581553738128358,4.83886483073622,
-7.34903002777252));
#159389=CARTESIAN_POINT('Ctrl Pts',(0.582770605614413,4.84149471141908,
-7.36593288621209));
#159390=CARTESIAN_POINT('Ctrl Pts',(0.583996966610964,4.84409946429569,
-7.38283890436021));
#159391=CARTESIAN_POINT('Ctrl Pts',(1.23436350016688,4.94924836941368,-7.30327121457896));
#159392=CARTESIAN_POINT('Ctrl Pts',(1.23040704258344,4.94861077170685,-7.30393550828948));
#159393=CARTESIAN_POINT('Ctrl Pts',(1.226450585,4.947973174,-7.304599802));
#159394=CARTESIAN_POINT('Ctrl Pts',(0.828527725,4.88384644,-7.371411501));
#159395=CARTESIAN_POINT('Ctrl Pts',(0.425701942,4.818610636,-7.394601894));
#159396=CARTESIAN_POINT('Ctrl Pts',(1.35776704393169,4.94924836941368,-7.12172944830898));
#159397=CARTESIAN_POINT('Ctrl Pts',(1.35390884396585,4.94861077170685,-7.12246068865449));
#159398=CARTESIAN_POINT('Ctrl Pts',(1.350050644,4.947973174,-7.123191929));
#159399=CARTESIAN_POINT('Ctrl Pts',(0.962010097,4.88384644,-7.196736822));
#159400=CARTESIAN_POINT('Ctrl Pts',(0.568276727,4.818610636,-7.227694069));
#159401=CARTESIAN_POINT('',(1.32928571593438,4.94797317334254,-7.15366863026892));
#159402=CARTESIAN_POINT('Ctrl Pts',(1.35315890319367,4.94745154526474,-7.12260282408957));
#159403=CARTESIAN_POINT('Ctrl Pts',(1.35160477359683,4.94771235963237,-7.12289737654479));
#159404=CARTESIAN_POINT('Ctrl Pts',(1.350050644,4.947973174,-7.123191929));
#159405=CARTESIAN_POINT('Ctrl Pts',(1.194437707,4.974088171,-7.152685076));
#159406=CARTESIAN_POINT('Ctrl Pts',(1.037685233,5.00031307,-7.175354302));
#159407=CARTESIAN_POINT('Ctrl Pts',(1.31165563666942,4.94745154526474,-7.18357434997128));
#159408=CARTESIAN_POINT('Ctrl Pts',(1.31008820833471,4.94771235963237,-7.18385984148564));
#159409=CARTESIAN_POINT('Ctrl Pts',(1.30852078,4.947973174,-7.184145333));
#159410=CARTESIAN_POINT('Ctrl Pts',(1.151576258,4.974088171,-7.21273122));
#159411=CARTESIAN_POINT('Ctrl Pts',(0.99353309,5.00031307,-7.2344359));
#159412=CARTESIAN_POINT('Origin',(-0.0135462464901456,5.08925699491388,
0.196625289502568));
#159413=CARTESIAN_POINT('Ctrl Pts',(1.404390852,4.94766207,-7.158581336));
#159414=CARTESIAN_POINT('Ctrl Pts',(1.247072838,4.97393188700001,-7.189444432));
#159415=CARTESIAN_POINT('Ctrl Pts',(1.088550856,5.00031307,-7.213366582));
#159416=CARTESIAN_POINT('Ctrl Pts',(1.351904417,4.94766207,-7.122840336));
#159417=CARTESIAN_POINT('Ctrl Pts',(1.195371852,4.97393188700001,-7.152549982));
#159418=CARTESIAN_POINT('Ctrl Pts',(1.037685233,5.00031307,-7.175354302));
#159419=CARTESIAN_POINT('Ctrl Pts',(1.35004873535491,4.94797287208564,-7.12319239739961));
#159420=CARTESIAN_POINT('Ctrl Pts',(1.35106266313749,4.94882769744714,-7.12831582295565));
#159421=CARTESIAN_POINT('Ctrl Pts',(1.35207564124165,4.94967947059234,-7.13343994654348));
#159422=CARTESIAN_POINT('Ctrl Pts',(1.35308957235425,4.95052852748342,-7.13856433053091));
#159423=CARTESIAN_POINT('Ctrl Pts',(1.35403086651912,4.95131675884083,-7.14332160909344));
#159424=CARTESIAN_POINT('Ctrl Pts',(1.35497298243889,4.95210264922691,-7.14807911356628));
#159425=CARTESIAN_POINT('Ctrl Pts',(1.35591591063016,4.95288622035062,-7.1528368383776));
#159426=CARTESIAN_POINT('Ctrl Pts',(1.35685883977408,4.95366979226598,-7.15759456799571));
#159427=CARTESIAN_POINT('Ctrl Pts',(1.35780258142974,4.95445104511169,-7.16235251915265));
#159428=CARTESIAN_POINT('Ctrl Pts',(1.35874712633804,4.95523000034704,-7.16711068663691));
#159429=CARTESIAN_POINT('Ctrl Pts',(1.632039014,5.000313899,-7.110137064));
#159430=CARTESIAN_POINT('Ctrl Pts',(1.523252973,4.98224132,-7.13510747800001));
#159431=CARTESIAN_POINT('Ctrl Pts',(1.41375393,4.964285714,-7.1567381));
#159432=CARTESIAN_POINT('Ctrl Pts',(1.363141222,4.955986264,-7.16673621900001));
#159433=CARTESIAN_POINT('Ctrl Pts',(1.312392169,4.947660853,-7.176017503));
#159434=CARTESIAN_POINT('Ctrl Pts',(1.665425089,5.000313899,-7.056122113));
#159435=CARTESIAN_POINT('Ctrl Pts',(1.557465485,4.98224132,-7.081603338));
#159436=CARTESIAN_POINT('Ctrl Pts',(1.448776863,4.964285714,-7.103769816));
#159437=CARTESIAN_POINT('Ctrl Pts',(1.398538749,4.955986264,-7.114015618));
#159438=CARTESIAN_POINT('Ctrl Pts',(1.34816075,4.947660853,-7.123549859));
#159439=CARTESIAN_POINT('Ctrl Pts',(1.35004971036774,4.94797303321381,-7.12319221260434));
#159440=CARTESIAN_POINT('Ctrl Pts',(1.38302850103403,4.95342302536017,-7.11694170312311));
#159441=CARTESIAN_POINT('Ctrl Pts',(1.41593904815349,4.95886083277475,-7.1104669176639));
#159442=CARTESIAN_POINT('Ctrl Pts',(1.44877686326084,4.96428571408279,-7.10376981626125));
#159443=CARTESIAN_POINT('Ctrl Pts',(1.52048397699665,4.97613189137991,-7.08914552447998));
#159444=CARTESIAN_POINT('Ctrl Pts',(1.59209201781199,4.9880392390861,-7.07341028179112));
#159445=CARTESIAN_POINT('Ctrl Pts',(1.66354985423409,5.0000000002771,-7.05656445327241));
#159446=CARTESIAN_POINT('Ctrl Pts',(1.665425089,5.000313899,-7.056122113));
#159447=CARTESIAN_POINT('Ctrl Pts',(1.557465485,4.98224132,-7.081603338));
#159448=CARTESIAN_POINT('Ctrl Pts',(1.448776863,4.964285714,-7.103769816));
#159449=CARTESIAN_POINT('Ctrl Pts',(1.399481142,4.95614195,-7.113823422));
#159450=CARTESIAN_POINT('Ctrl Pts',(1.350050644,4.947973174,-7.123191929));
#159451=CARTESIAN_POINT('Ctrl Pts',(1.728164706,5.000313899,-7.094900813));
#159452=CARTESIAN_POINT('Ctrl Pts',(1.619611782,4.98224132,-7.121341962));
#159453=CARTESIAN_POINT('Ctrl Pts',(1.510300752,4.964285714,-7.144449764));
#159454=CARTESIAN_POINT('Ctrl Pts',(1.460722737,4.95614195,-7.154930307));
#159455=CARTESIAN_POINT('Ctrl Pts',(1.411004048,4.947973174,-7.164721793));
#159456=CARTESIAN_POINT('',(1.44075458445333,4.94797317334226,-7.18499195770727));
#159457=CARTESIAN_POINT('Ctrl Pts',(2.311531602,4.818630405,-7.036915586));
#159458=CARTESIAN_POINT('Ctrl Pts',(2.303144664,4.820029867,-7.039670582));
#159459=CARTESIAN_POINT('Ctrl Pts',(2.294751182,4.821428571,-7.042405578));
#159460=CARTESIAN_POINT('Ctrl Pts',(1.918563751,4.884117105,-7.164985361));
#159461=CARTESIAN_POINT('Ctrl Pts',(1.531458517,4.947973174,-7.246791988));
#159462=CARTESIAN_POINT('Ctrl Pts',(2.117742488,4.818630405,-6.93380608));
#159463=CARTESIAN_POINT('Ctrl Pts',(2.10947844,4.820029867,-6.936330109));
#159464=CARTESIAN_POINT('Ctrl Pts',(2.1012084,4.821428571,-6.938834431));
#159465=CARTESIAN_POINT('Ctrl Pts',(1.730553477,4.884117105,-7.05107565));
#159466=CARTESIAN_POINT('Ctrl Pts',(1.350050644,4.947973174,-7.123191929));
#159467=CARTESIAN_POINT('Ctrl Pts',(2.11325075290604,4.81939091791738,-6.93517638941566));
#159468=CARTESIAN_POINT('Ctrl Pts',(2.11834934301391,4.8223472472358,-6.95252122234189));
#159469=CARTESIAN_POINT('Ctrl Pts',(2.1234496207869,4.82527010317062,-6.96987131670068));
#159470=CARTESIAN_POINT('Ctrl Pts',(2.12856671375808,4.82816321752733,-6.98722138055105));
#159471=CARTESIAN_POINT('Ctrl Pts',(2.13335709474407,4.83087161467446,-7.00346369165283));
#159472=CARTESIAN_POINT('Ctrl Pts',(2.13815831498521,4.83355328554903,-7.01970728651488));
#159473=CARTESIAN_POINT('Ctrl Pts',(2.14296990901817,4.83620904389083,-7.03595201936947));
#159474=CARTESIAN_POINT('Ctrl Pts',(2.14778155471109,4.83886483074633,-7.05219692663661));
#159475=CARTESIAN_POINT('Ctrl Pts',(2.15260358736129,4.84149471142336,-7.06844301510797));
#159476=CARTESIAN_POINT('Ctrl Pts',(2.15743557083302,4.84409946430342,-7.08469014864696));
#159477=CARTESIAN_POINT('Ctrl Pts',(2.77549219559838,4.94924836941368,-6.86717312735757));
#159478=CARTESIAN_POINT('Ctrl Pts',(2.77177104129919,4.94861077170685,-6.86867241167878));
#159479=CARTESIAN_POINT('Ctrl Pts',(2.768049887,4.947973174,-6.870171696));
#159480=CARTESIAN_POINT('Ctrl Pts',(2.393792782,4.88384644,-7.020963027));
#159481=CARTESIAN_POINT('Ctrl Pts',(2.005370091,4.818610636,-7.130206877));
#159482=CARTESIAN_POINT('Ctrl Pts',(2.85698451967887,4.94924836941368,-6.66334759239431));
#159483=CARTESIAN_POINT('Ctrl Pts',(2.85337371733943,4.94861077170685,-6.66489113569716));
#159484=CARTESIAN_POINT('Ctrl Pts',(2.849762915,4.947973174,-6.666434679));
#159485=CARTESIAN_POINT('Ctrl Pts',(2.486604518,4.88384644,-6.821677381));
#159486=CARTESIAN_POINT('Ctrl Pts',(2.108731308,4.818610636,-6.93655190100001));
#159487=CARTESIAN_POINT('',(2.83603504918524,4.94797317334254,-6.70066269744023));
#159488=CARTESIAN_POINT('Ctrl Pts',(2.85267186467479,4.94745154526474,-6.66519116319149));
#159489=CARTESIAN_POINT('Ctrl Pts',(2.8512173898374,4.94771235963237,-6.66581292109574));
#159490=CARTESIAN_POINT('Ctrl Pts',(2.849762915,4.947973174,-6.66643467899999));
#159491=CARTESIAN_POINT('Ctrl Pts',(2.704128277,4.974088171,-6.728690474));
#159492=CARTESIAN_POINT('Ctrl Pts',(2.555913802,5.00031307,-6.784526854));
#159493=CARTESIAN_POINT('Ctrl Pts',(2.82524599699793,4.94745154526474,-6.73365918371558));
#159494=CARTESIAN_POINT('Ctrl Pts',(2.82377658649896,4.94771235963237,-6.73427495135779));
#159495=CARTESIAN_POINT('Ctrl Pts',(2.822307176,4.947973174,-6.734890719));
#159496=CARTESIAN_POINT('Ctrl Pts',(2.67517705,4.974088171,-6.796546717));
#159497=CARTESIAN_POINT('Ctrl Pts',(2.525494709,5.00031307,-6.851718563));
#159498=CARTESIAN_POINT('Origin',(-0.0554978882862017,5.08925696267246,
0.189115584010757));
#159499=CARTESIAN_POINT('Ctrl Pts',(2.910440355,4.94766207,-6.68931516300001));
#159500=CARTESIAN_POINT('Ctrl Pts',(2.763435003,4.973931887,-6.75327541900001));
#159501=CARTESIAN_POINT('Ctrl Pts',(2.613761731,5.00031307,-6.810715823));
#159502=CARTESIAN_POINT('Ctrl Pts',(2.851497765,4.94766207,-6.665692799));
#159503=CARTESIAN_POINT('Ctrl Pts',(2.705011541,4.973931887,-6.728357725));
#159504=CARTESIAN_POINT('Ctrl Pts',(2.555913802,5.00031307,-6.784526854));
#159505=CARTESIAN_POINT('Ctrl Pts',(2.84976115133646,4.94797287201019,-6.66643554643429));
#159506=CARTESIAN_POINT('Ctrl Pts',(2.85185275935425,4.94882769742881,-6.67122122457105));
#159507=CARTESIAN_POINT('Ctrl Pts',(2.85394358965563,4.94967947057215,-6.67600778869325));
#159508=CARTESIAN_POINT('Ctrl Pts',(2.85603540668187,4.95052852746016,-6.68079440224708));
#159509=CARTESIAN_POINT('Ctrl Pts',(2.85797736816239,4.95131675881625,-6.68523810789968));
#159510=CARTESIAN_POINT('Ctrl Pts',(2.85992018076595,4.95210264919987,-6.68968185751783));
#159511=CARTESIAN_POINT('Ctrl Pts',(2.8618638340298,4.95288622032081,-6.69412564770306));
#159512=CARTESIAN_POINT('Ctrl Pts',(2.86380748925736,4.9536697922334,-6.69856944237792));
#159513=CARTESIAN_POINT('Ctrl Pts',(2.86575198563786,4.95445104507607,-6.70301327874052));
#159514=CARTESIAN_POINT('Ctrl Pts',(2.86769731302196,4.9552300003156,-6.70745715373435));
#159515=CARTESIAN_POINT('Ctrl Pts',(3.122352143,5.000313899,-6.593065866));
#159516=CARTESIAN_POINT('Ctrl Pts',(3.02147736,4.98224132,-6.640838268));
#159517=CARTESIAN_POINT('Ctrl Pts',(2.919188289,4.964285714,-6.685502236));
#159518=CARTESIAN_POINT('Ctrl Pts',(2.871908178,4.955986264,-6.70614684));
#159519=CARTESIAN_POINT('Ctrl Pts',(2.824340811,4.947660853,-6.72612067900001));
#159520=CARTESIAN_POINT('Ctrl Pts',(3.143346053,5.000313899,-6.533136734));
#159521=CARTESIAN_POINT('Ctrl Pts',(3.043388194,4.98224132,-6.581230346));
#159522=CARTESIAN_POINT('Ctrl Pts',(2.94200579,4.964285714,-6.626243425));
#159523=CARTESIAN_POINT('Ctrl Pts',(2.895144759,4.955986264,-6.647049396));
#159524=CARTESIAN_POINT('Ctrl Pts',(2.84799415,4.947660853,-6.667190512));
#159525=CARTESIAN_POINT('Ctrl Pts',(2.84976291533748,4.94797317387187,-6.66643467973655));
#159526=CARTESIAN_POINT('Ctrl Pts',(2.89887082684445,4.95664467876409,-6.64544206388029));
#159527=CARTESIAN_POINT('Ctrl Pts',(2.94770441222799,4.96527388208562,-6.62392545570605));
#159528=CARTESIAN_POINT('Ctrl Pts',(3.04499834694427,4.98260085372362,-6.57976772645109));
#159529=CARTESIAN_POINT('Ctrl Pts',(3.0934328535996,4.99129108975406,-6.55713586568035));
#159530=CARTESIAN_POINT('Ctrl Pts',(3.14160975151107,5.00000000050473,-6.53397185204522));
#159531=CARTESIAN_POINT('Ctrl Pts',(3.143346053,5.000313899,-6.533136734));
#159532=CARTESIAN_POINT('Ctrl Pts',(3.043388194,4.98224132,-6.581230346));
#159533=CARTESIAN_POINT('Ctrl Pts',(2.94200579,4.964285714,-6.626243425));
#159534=CARTESIAN_POINT('Ctrl Pts',(2.896023804,4.95614195,-6.646659106));
#159535=CARTESIAN_POINT('Ctrl Pts',(2.849762915,4.947973174,-6.66643467900001));
#159536=CARTESIAN_POINT('Ctrl Pts',(3.212955126,5.000313899,-6.557521647));
#159537=CARTESIAN_POINT('Ctrl Pts',(3.112624175,4.98224132,-6.606680287));
#159538=CARTESIAN_POINT('Ctrl Pts',(3.01083627,4.964285714,-6.652746481));
#159539=CARTESIAN_POINT('Ctrl Pts',(2.964670369,4.95614195,-6.673639803));
#159540=CARTESIAN_POINT('Ctrl Pts',(2.918218955,4.947973174,-6.693890418));
#159541=CARTESIAN_POINT('',(2.95163142719041,4.94797317334227,-6.70729119137599));
#159542=CARTESIAN_POINT('Ctrl Pts',(3.770218119,4.818630405,-6.375485444));
#159543=CARTESIAN_POINT('Ctrl Pts',(3.762619505,4.820029867,-6.379978973));
#159544=CARTESIAN_POINT('Ctrl Pts',(3.755010202,4.821428571,-6.384454377));
#159545=CARTESIAN_POINT('Ctrl Pts',(3.413968854,4.884117105,-6.585037491));
#159546=CARTESIAN_POINT('Ctrl Pts',(3.053499932,4.947973174,-6.748147707));
#159547=CARTESIAN_POINT('Ctrl Pts',(3.558794191,4.818630405,-6.316445512));
#159548=CARTESIAN_POINT('Ctrl Pts',(3.551265944,4.820029867,-6.320687056));
#159549=CARTESIAN_POINT('Ctrl Pts',(3.543727607,4.821428571,-6.324910643));
#159550=CARTESIAN_POINT('Ctrl Pts',(3.205866935,4.884117105,-6.514207577));
#159551=CARTESIAN_POINT('Ctrl Pts',(2.849762915,4.947973174,-6.666434679));
#159552=CARTESIAN_POINT('Ctrl Pts',(3.55470204599044,4.8193909179173,-6.31874937381797));
#159553=CARTESIAN_POINT('Ctrl Pts',(3.5634100609705,4.82234724728643,-6.3345926481873));
#159554=CARTESIAN_POINT('Ctrl Pts',(3.57212085391211,4.82527010311282,-6.35044069837409));
#159555=CARTESIAN_POINT('Ctrl Pts',(3.58084806296071,4.82816321747262,-6.3662851036461));
#159556=CARTESIAN_POINT('Ctrl Pts',(3.58901806429448,4.8308716146299,-6.38111788827223));
#159557=CARTESIAN_POINT('Ctrl Pts',(3.59719892743765,4.83355328551375,-6.39594959652601));
#159558=CARTESIAN_POINT('Ctrl Pts',(3.60539016647409,4.83620904386399,-6.41078018610813));
#159559=CARTESIAN_POINT('Ctrl Pts',(3.61358149345627,4.83886483072794,-6.42561093491979));
#159560=CARTESIAN_POINT('Ctrl Pts',(3.62178321847861,4.84149471141258,-6.44044060443103));
#159561=CARTESIAN_POINT('Ctrl Pts',(3.62999488635505,4.84409946430512,-6.45526915547616));
#159562=CARTESIAN_POINT('Ctrl Pts',(4.18684196093688,4.94924836941368,-6.10997365687233));
#159563=CARTESIAN_POINT('Ctrl Pts',(4.18353010696844,4.94861077170685,-6.11223782693617));
#159564=CARTESIAN_POINT('Ctrl Pts',(4.180218253,4.947973174,-6.114501997));
#159565=CARTESIAN_POINT('Ctrl Pts',(3.84712675,4.88384644,-6.342222125));
#159566=CARTESIAN_POINT('Ctrl Pts',(3.491269364,4.818610636,-6.532411311));
#159567=CARTESIAN_POINT('Ctrl Pts',(4.22261257419805,4.94924836941368,-5.89339500821419));
#159568=CARTESIAN_POINT('Ctrl Pts',(4.21941800659902,4.94861077170685,-5.8956786801071));
#159569=CARTESIAN_POINT('Ctrl Pts',(4.216223439,4.947973174,-5.897962352));
#159570=CARTESIAN_POINT('Ctrl Pts',(3.894928076,4.88384644,-6.127643887));
#159571=CARTESIAN_POINT('Ctrl Pts',(3.550583958,4.818610636,-6.321064274));
#159572=CARTESIAN_POINT('',(4.21017453526411,4.94797317334248,-5.93434122418425));
#159573=CARTESIAN_POINT('Ctrl Pts',(4.21879705989843,4.94745154526473,-5.89612257069493));
#159574=CARTESIAN_POINT('Ctrl Pts',(4.21751024944921,4.94771235963237,-5.89704246134746));
#159575=CARTESIAN_POINT('Ctrl Pts',(4.216223439,4.947973174,-5.897962352));
#159576=CARTESIAN_POINT('Ctrl Pts',(4.087376814,4.97408817100001,-5.990069784));
#159577=CARTESIAN_POINT('Ctrl Pts',(3.954630682,5.00031307,-6.076462471));
#159578=CARTESIAN_POINT('Ctrl Pts',(4.20673099430623,4.94745154526473,-5.96888559868221));
#159579=CARTESIAN_POINT('Ctrl Pts',(4.20542830965312,4.94771235963237,-5.9698028498411));
#159580=CARTESIAN_POINT('Ctrl Pts',(4.204125625,4.947973174,-5.970720101));
#159581=CARTESIAN_POINT('Ctrl Pts',(4.073689537,4.97408817100001,-6.062563244));
#159582=CARTESIAN_POINT('Ctrl Pts',(3.939367001,5.00031307,-6.148622482));
#159583=CARTESIAN_POINT('Origin',(-0.0948540586112023,5.08925688855765,
0.172762876232048));
#159584=CARTESIAN_POINT('Ctrl Pts',(4.280400903,4.94766207,-5.907264047));
#159585=CARTESIAN_POINT('Ctrl Pts',(4.150582018,4.973931887,-6.001330754));
#159586=CARTESIAN_POINT('Ctrl Pts',(4.016756013,5.00031307,-6.089603562));
#159587=CARTESIAN_POINT('Ctrl Pts',(4.217758247,4.94766207,-5.89686487600001));
#159588=CARTESIAN_POINT('Ctrl Pts',(4.088167896,4.973931887,-5.989554938));
#159589=CARTESIAN_POINT('Ctrl Pts',(3.954630682,5.00031307,-6.076462471));
#159590=CARTESIAN_POINT('Ctrl Pts',(4.21622190306857,4.94797287210893,-5.89796357864352));
#159591=CARTESIAN_POINT('Ctrl Pts',(4.21929338956627,4.94882769744785,-5.90218773665338));
#159592=CARTESIAN_POINT('Ctrl Pts',(4.22236430733007,4.94967947058069,-5.9064129267227));
#159593=CARTESIAN_POINT('Ctrl Pts',(4.22543619933326,4.95052852745714,-5.91063795296052));
#159594=CARTESIAN_POINT('Ctrl Pts',(4.22828802432798,4.95131675882064,-5.91456030290507));
#159595=CARTESIAN_POINT('Ctrl Pts',(4.23114068995999,4.95210264921027,-5.91848251282697));
#159596=CARTESIAN_POINT('Ctrl Pts',(4.23399418529024,4.95288622033926,-5.92240458167081));
#159597=CARTESIAN_POINT('Ctrl Pts',(4.2368476835034,4.9536697922599,-5.92632665447713));
#159598=CARTESIAN_POINT('Ctrl Pts',(4.23970201213683,4.95445104511264,-5.93024858719394));
#159599=CARTESIAN_POINT('Ctrl Pts',(4.24255716059392,4.95523000035748,-5.9341703789812));
#159600=CARTESIAN_POINT('Ctrl Pts',(4.466667556,5.000313899,-5.767710235));
#159601=CARTESIAN_POINT('Ctrl Pts',(4.378420824,4.98224132,-5.836050841));
#159602=CARTESIAN_POINT('Ctrl Pts',(4.288124647,4.964285714,-5.901659717));
#159603=CARTESIAN_POINT('Ctrl Pts',(4.246387899,4.955986264,-5.931985488));
#159604=CARTESIAN_POINT('Ctrl Pts',(4.204226416,4.947660853,-5.961717928));
#159605=CARTESIAN_POINT('Ctrl Pts',(4.474287649,5.000313899,-5.704669143));
#159606=CARTESIAN_POINT('Ctrl Pts',(4.387005454,4.98224132,-5.773126338));
#159607=CARTESIAN_POINT('Ctrl Pts',(4.297669796,4.964285714,-5.838881257));
#159608=CARTESIAN_POINT('Ctrl Pts',(4.256377018,4.955986264,-5.869274531));
#159609=CARTESIAN_POINT('Ctrl Pts',(4.214658508,4.947660853,-5.899080747));
#159610=CARTESIAN_POINT('Ctrl Pts',(4.21622343934038,4.94797317391062,-5.89796235245119));
#159611=CARTESIAN_POINT('Ctrl Pts',(4.25967046514281,4.95664468310041,-5.86690376849364));
#159612=CARTESIAN_POINT('Ctrl Pts',(4.30273688556295,4.96527388072572,-5.83539245009048));
#159613=CARTESIAN_POINT('Ctrl Pts',(4.38826353175028,4.98260085161193,-5.77135178628772));
#159614=CARTESIAN_POINT('Ctrl Pts',(4.43070047526962,4.99129108540162,-5.73883706723313));
#159615=CARTESIAN_POINT('Ctrl Pts',(4.47277146646463,5.00000000040085,-5.70585799033773));
#159616=CARTESIAN_POINT('Ctrl Pts',(4.474287649,5.000313899,-5.704669143));
#159617=CARTESIAN_POINT('Ctrl Pts',(4.387005454,4.98224132,-5.773126338));
#159618=CARTESIAN_POINT('Ctrl Pts',(4.297669796,4.964285714,-5.838881257));
#159619=CARTESIAN_POINT('Ctrl Pts',(4.25715161,4.95614195,-5.868704398));
#159620=CARTESIAN_POINT('Ctrl Pts',(4.216223439,4.947973174,-5.897962352));
#159621=CARTESIAN_POINT('Ctrl Pts',(4.547511336,5.000313899,-5.713520057));
#159622=CARTESIAN_POINT('Ctrl Pts',(4.460093721,4.98224132,-5.783097584));
#159623=CARTESIAN_POINT('Ctrl Pts',(4.370588431,4.964285714,-5.849968167));
#159624=CARTESIAN_POINT('Ctrl Pts',(4.32999331,4.95614195,-5.880297318));
#159625=CARTESIAN_POINT('Ctrl Pts',(4.288981187,4.947973174,-5.910060166));
#159626=CARTESIAN_POINT('',(4.32449326475501,4.94797317334227,-5.91596494312064));
#159627=CARTESIAN_POINT('Ctrl Pts',(5.052613427,4.818630405,-5.415944688));
#159628=CARTESIAN_POINT('Ctrl Pts',(5.046158441,4.820029867,-5.421966639));
#159629=CARTESIAN_POINT('Ctrl Pts',(5.039689118,4.821428571,-5.427973185));
#159630=CARTESIAN_POINT('Ctrl Pts',(4.749740568,4.884117105,-5.697180586));
#159631=CARTESIAN_POINT('Ctrl Pts',(4.432763084,4.947973174,-5.933967539));
#159632=CARTESIAN_POINT('Ctrl Pts',(4.833440632,4.818630405,-5.403734972));
#159633=CARTESIAN_POINT('Ctrl Pts',(4.827000198,4.820029867,-5.409495702));
#159634=CARTESIAN_POINT('Ctrl Pts',(4.82054605,4.821428571,-5.415241063));
#159635=CARTESIAN_POINT('Ctrl Pts',(4.531277618,4.884117105,-5.672742398));
#159636=CARTESIAN_POINT('Ctrl Pts',(4.216223439,4.947973174,-5.897962352));
#159637=CARTESIAN_POINT('Ctrl Pts',(4.82993942163252,4.81939091791738,-5.4068646610732));
#159638=CARTESIAN_POINT('Ctrl Pts',(4.84184968410277,4.82234724721574,-5.42046556271523));
#159639=CARTESIAN_POINT('Ctrl Pts',(4.8537636861635,4.82527010310443,-5.43407053107029));
#159640=CARTESIAN_POINT('Ctrl Pts',(4.86569293671696,4.82816321746756,-5.44766841099453));
#159641=CARTESIAN_POINT('Ctrl Pts',(4.87686053821621,4.83087161462581,-5.46039810457822));
#159642=CARTESIAN_POINT('Ctrl Pts',(4.8880385161992,4.83355328551165,-5.47312441198141));
#159643=CARTESIAN_POINT('Ctrl Pts',(4.89922638701532,4.8362090438646,-5.48584739635302));
#159644=CARTESIAN_POINT('Ctrl Pts',(4.9104143779507,4.83886483073126,-5.49857051732573));
#159645=CARTESIAN_POINT('Ctrl Pts',(4.92161229181196,4.84149471141935,-5.51129034895669));
#159646=CARTESIAN_POINT('Ctrl Pts',(4.93281967559905,4.84409946430769,-5.52400695080939));
#159647=CARTESIAN_POINT('Ctrl Pts',(5.40241964904355,4.94924836941368,-5.06707860853674));
#159648=CARTESIAN_POINT('Ctrl Pts',(5.39967195402178,4.94861077170685,-5.07000179426837));
#159649=CARTESIAN_POINT('Ctrl Pts',(5.396924259,4.947973174,-5.07292498));
#159650=CARTESIAN_POINT('Ctrl Pts',(5.120573347,4.88384644,-5.36692596499999));
#159651=CARTESIAN_POINT('Ctrl Pts',(4.81392076200001,4.818610636,-5.629167453));
#159652=CARTESIAN_POINT('Ctrl Pts',(5.39079595785796,4.94924836941368,-4.84787382396709));
#159653=CARTESIAN_POINT('Ctrl Pts',(5.38816699942898,4.94861077170685,-4.85079084248354));
#159654=CARTESIAN_POINT('Ctrl Pts',(5.385538041,4.947973174,-4.853707861));
#159655=CARTESIAN_POINT('Ctrl Pts',(5.121129126,4.88384644,-5.147088575));
#159656=CARTESIAN_POINT('Ctrl Pts',(4.826415248,4.818610636,-5.410010708));
#159657=CARTESIAN_POINT('',(5.3874509396897,4.94797317334254,-4.89053655053701));
#159658=CARTESIAN_POINT('Ctrl Pts',(5.38765599348884,4.94745154526474,-4.8513578403444));
#159659=CARTESIAN_POINT('Ctrl Pts',(5.38659701724442,4.94771235963237,-4.8525328506722));
#159660=CARTESIAN_POINT('Ctrl Pts',(5.385538041,4.947973174,-4.853707861));
#159661=CARTESIAN_POINT('Ctrl Pts',(5.279504153,4.974088171,-4.971360088));
#159662=CARTESIAN_POINT('Ctrl Pts',(5.168433427,5.00031307,-5.084269457));
#159663=CARTESIAN_POINT('Ctrl Pts',(5.39151392645153,4.94745154526474,-4.92501355593251));
#159664=CARTESIAN_POINT('Ctrl Pts',(5.39043887972577,4.94771235963237,-4.92618940096626));
#159665=CARTESIAN_POINT('Ctrl Pts',(5.389363833,4.947973174,-4.927365246));
#159666=CARTESIAN_POINT('Ctrl Pts',(5.281720829,4.974088171,-5.045101051));
#159667=CARTESIAN_POINT('Ctrl Pts',(5.169038872,5.00031307,-5.15802364600001));
#159668=CARTESIAN_POINT('Origin',(-0.129776799267178,5.08925709704122,0.148334366254367));
#159669=CARTESIAN_POINT('Ctrl Pts',(5.450214661,4.94766207,-4.84899583));
#159670=CARTESIAN_POINT('Ctrl Pts',(5.343652431,4.97393188700001,-4.968770532));
#159671=CARTESIAN_POINT('Ctrl Pts',(5.231931248,5.00031307,-5.083748206));
#159672=CARTESIAN_POINT('Ctrl Pts',(5.386801042,4.94766207,-4.852306105));
#159673=CARTESIAN_POINT('Ctrl Pts',(5.28016606400001,4.97393188700001,-4.97068722));
#159674=CARTESIAN_POINT('Ctrl Pts',(5.168433427,5.00031307,-5.084269457));
#159675=CARTESIAN_POINT('Ctrl Pts',(5.38553680511737,4.94797287199671,-4.85370938913422));
#159676=CARTESIAN_POINT('Ctrl Pts',(5.38944455129704,4.94882769741461,-4.85717450974945));
#159677=CARTESIAN_POINT('Ctrl Pts',(5.39335196362416,4.94967947056355,-4.86064076076593));
#159678=CARTESIAN_POINT('Ctrl Pts',(5.39726029218899,4.95052852745504,-4.86410664233588));
#159679=CARTESIAN_POINT('Ctrl Pts',(5.40088863229767,4.95131675882372,-4.86732423187668));
#159680=CARTESIAN_POINT('Ctrl Pts',(5.40451776328343,4.95210264921743,-4.87054150394423));
#159681=CARTESIAN_POINT('Ctrl Pts',(5.40814767425038,4.95288622034999,-4.87375845986201));
#159682=CARTESIAN_POINT('Ctrl Pts',(5.41177758888466,4.95366979227421,-4.87697541902991));
#159683=CARTESIAN_POINT('Ctrl Pts',(5.41540828441786,4.95445104513005,-4.88019206285825));
#159684=CARTESIAN_POINT('Ctrl Pts',(5.4190397503672,4.95523000038511,-4.88340839283606));
#159685=CARTESIAN_POINT('Ctrl Pts',(5.602126559,5.000313899,-4.672662884));
#159686=CARTESIAN_POINT('Ctrl Pts',(5.530634197,4.98224132,-4.758376164));
#159687=CARTESIAN_POINT('Ctrl Pts',(5.456553063,4.964285714,-4.84186215));
#159688=CARTESIAN_POINT('Ctrl Pts',(5.422311241,4.955986264,-4.880451088));
#159689=CARTESIAN_POINT('Ctrl Pts',(5.387527066,4.947660853,-4.918551872));
#159690=CARTESIAN_POINT('Ctrl Pts',(5.596016527,5.000313899,-4.609457563));
#159691=CARTESIAN_POINT('Ctrl Pts',(5.52549121500001,4.98224132,-4.695077359));
#159692=CARTESIAN_POINT('Ctrl Pts',(5.452379538,4.964285714,-4.77849949));
#159693=CARTESIAN_POINT('Ctrl Pts',(5.418585819,4.955986264,-4.817058913));
#159694=CARTESIAN_POINT('Ctrl Pts',(5.38425012,4.947660853,-4.855136522));
#159695=CARTESIAN_POINT('Ctrl Pts',(5.38553746950781,4.94797303313041,-4.85370865194204));
#159696=CARTESIAN_POINT('Ctrl Pts',(5.4080090089543,4.9534230252675,-4.82877475100876));
#159697=CARTESIAN_POINT('Ctrl Pts',(5.43029049427791,4.95886083271017,-4.80370360501776));
#159698=CARTESIAN_POINT('Ctrl Pts',(5.45237953810033,4.96428571402229,-4.77849949004151));
#159699=CARTESIAN_POINT('Ctrl Pts',(5.5006148297591,4.97613189137016,-4.72346189605064));
#159700=CARTESIAN_POINT('Ctrl Pts',(5.54809893169663,4.98803923916643,-4.66759983832208));
#159701=CARTESIAN_POINT('Ctrl Pts',(5.59479135902996,5.00000000040303,-4.61094455025893));
#159702=CARTESIAN_POINT('Ctrl Pts',(5.596016527,5.000313899,-4.609457563));
#159703=CARTESIAN_POINT('Ctrl Pts',(5.52549121500001,4.98224132,-4.695077359));
#159704=CARTESIAN_POINT('Ctrl Pts',(5.452379538,4.964285714,-4.77849949));
#159705=CARTESIAN_POINT('Ctrl Pts',(5.419219739,4.95614195,-4.816335595));
#159706=CARTESIAN_POINT('Ctrl Pts',(5.385538041,4.947973174,-4.853707861));
#159707=CARTESIAN_POINT('Ctrl Pts',(5.66943097000001,5.000313899,-4.60236062));
#159708=CARTESIAN_POINT('Ctrl Pts',(5.599014242,4.98224132,-4.68910366600001));
#159709=CARTESIAN_POINT('Ctrl Pts',(5.525976735,4.964285714,-4.773651843));
#159710=CARTESIAN_POINT('Ctrl Pts',(5.492850576,4.95614195,-4.811998667));
#159711=CARTESIAN_POINT('Ctrl Pts',(5.459195426,4.947973174,-4.84988207));
#159712=CARTESIAN_POINT('',(5.49514660316742,4.94797317334227,-4.84801474947653));
#159713=CARTESIAN_POINT('Ctrl Pts',(6.098754147,4.81863040500001,-4.203160378));
#159714=CARTESIAN_POINT('Ctrl Pts',(6.09374461600001,4.820029867,-4.21042917));
#159715=CARTESIAN_POINT('Ctrl Pts',(6.088717772,4.821428571,-4.217686));
#159716=CARTESIAN_POINT('Ctrl Pts',(5.863419691,4.884117105,-4.542929849));
#159717=CARTESIAN_POINT('Ctrl Pts',(5.60475516,4.947973174,-4.842321644));
#159718=CARTESIAN_POINT('Ctrl Pts',(5.882080762,4.81863040500001,-4.238351791));
#159719=CARTESIAN_POINT('Ctrl Pts',(5.877029288,4.820029867,-4.245362341));
#159720=CARTESIAN_POINT('Ctrl Pts',(5.871961118,4.821428571,-4.25236083));
#159721=CARTESIAN_POINT('Ctrl Pts',(5.64481079600001,4.884117105,-4.566026089));
#159722=CARTESIAN_POINT('Ctrl Pts',(5.385538041,4.947973174,-4.853707861));
#159723=CARTESIAN_POINT('Ctrl Pts',(5.87933419858875,4.8193909179172,-4.24216096606972));
#159724=CARTESIAN_POINT('Ctrl Pts',(5.89388979747093,4.82234724725715,-4.2528835319381));
#159725=CARTESIAN_POINT('Ctrl Pts',(5.90844992258693,4.82527010309212,-4.26360926566706));
#159726=CARTESIAN_POINT('Ctrl Pts',(5.92302341609072,4.82816321745518,-4.27432479842803));
#159727=CARTESIAN_POINT('Ctrl Pts',(5.93666643311167,4.8308716146208,-4.2843561746254));
#159728=CARTESIAN_POINT('Ctrl Pts',(5.95031885609539,4.83355328551246,-4.2943820131668));
#159729=CARTESIAN_POINT('Ctrl Pts',(5.96398022627268,4.83620904386994,-4.30440247969684));
#159730=CARTESIAN_POINT('Ctrl Pts',(5.97764174312615,4.83886483074115,-4.31442305381226));
#159731=CARTESIAN_POINT('Ctrl Pts',(5.99131224380473,4.84149471143251,-4.32443828234945));
#159732=CARTESIAN_POINT('Ctrl Pts',(6.00499129873184,4.84409946432866,-4.33444832088375));
#159733=CARTESIAN_POINT('Ctrl Pts',(6.36538619882948,4.94924836941368,-3.78725259602702));
#159734=CARTESIAN_POINT('Ctrl Pts',(6.36333114191474,4.94861077170685,-3.79069811251351));
#159735=CARTESIAN_POINT('Ctrl Pts',(6.361276085,4.947973174,-3.794143629));
#159736=CARTESIAN_POINT('Ctrl Pts',(6.154587625,4.88384644,-4.140678312));
#159737=CARTESIAN_POINT('Ctrl Pts',(5.911478575,4.818610636,-4.462709981));
#159738=CARTESIAN_POINT('Ctrl Pts',(6.30691171418917,4.94924836941368,-3.57567144780525));
#159739=CARTESIAN_POINT('Ctrl Pts',(6.30497129209459,4.94861077170685,-3.57908541640263));
#159740=CARTESIAN_POINT('Ctrl Pts',(6.30303087000001,4.947973174,-3.582499385));
#159741=CARTESIAN_POINT('Ctrl Pts',(6.107871869,4.88384644,-3.925861122));
#159742=CARTESIAN_POINT('Ctrl Pts',(5.876568725,4.818610636,-4.245991053));
#159743=CARTESIAN_POINT('',(6.31281612599007,4.94797317334248,-3.61805582352771));
#159744=CARTESIAN_POINT('Ctrl Pts',(6.30459412094996,4.94745154526473,-3.57974900934041));
#159745=CARTESIAN_POINT('Ctrl Pts',(6.30381249547498,4.94771235963237,-3.5811241971702));
#159746=CARTESIAN_POINT('Ctrl Pts',(6.30303087,4.947973174,-3.582499385));
#159747=CARTESIAN_POINT('Ctrl Pts',(6.224767747,4.97408817100001,-3.72019512));
#159748=CARTESIAN_POINT('Ctrl Pts',(6.140565969,5.00031307,-3.854341653));
#159749=CARTESIAN_POINT('Ctrl Pts',(6.32419565962129,4.94745154526473,-3.65085335360889));
#159750=CARTESIAN_POINT('Ctrl Pts',(6.32339851881065,4.94771235963237,-3.65223281130444));
#159751=CARTESIAN_POINT('Ctrl Pts',(6.322601378,4.947973174,-3.653612269));
#159752=CARTESIAN_POINT('Ctrl Pts',(6.242784725,4.97408817100001,-3.79173554));
#159753=CARTESIAN_POINT('Ctrl Pts',(6.157012229,5.00031307,-3.926241358));
#159754=CARTESIAN_POINT('Origin',(-0.158628913824926,5.08925704202097,0.116967444023323));
#159755=CARTESIAN_POINT('Ctrl Pts',(6.365182439,4.94766207,-3.563993958));
#159756=CARTESIAN_POINT('Ctrl Pts',(6.286859595,4.973931887,-3.703876123));
#159757=CARTESIAN_POINT('Ctrl Pts',(6.202467193,5.00031307,-3.840182435));
#159758=CARTESIAN_POINT('Ctrl Pts',(6.303963006,4.94766207,-3.580858894));
#159759=CARTESIAN_POINT('Ctrl Pts',(6.225269536,4.973931887,-3.719395692));
#159760=CARTESIAN_POINT('Ctrl Pts',(6.140565969,5.00031307,-3.854341653));
#159761=CARTESIAN_POINT('Ctrl Pts',(6.30302999118404,4.94797287209564,-3.58250114338846));
#159762=CARTESIAN_POINT('Ctrl Pts',(6.3075912746304,4.94882769739619,-3.58504520174211));
#159763=CARTESIAN_POINT('Ctrl Pts',(6.31215247530727,4.94967947051464,-3.58759043548581));
#159764=CARTESIAN_POINT('Ctrl Pts',(6.31671449138878,4.95052852737955,-3.59013511146802));
#159765=CARTESIAN_POINT('Ctrl Pts',(6.32094968965551,4.95131675874445,-3.59249748966149));
#159766=CARTESIAN_POINT('Ctrl Pts',(6.3251855920701,4.95210264913791,-3.59485938779982));
#159767=CARTESIAN_POINT('Ctrl Pts',(6.32942218826612,4.95288622027104,-3.59722080950912));
#159768=CARTESIAN_POINT('Ctrl Pts',(6.3336587887424,4.95366979219581,-3.59958223360419));
#159769=CARTESIAN_POINT('Ctrl Pts',(6.33789608407051,4.95445104505298,-3.60194318186425));
#159770=CARTESIAN_POINT('Ctrl Pts',(6.34213406430118,4.9552300003035,-3.6043036579765));
#159771=CARTESIAN_POINT('Ctrl Pts',(6.475636351,5.000313899,-3.35912701));
#159772=CARTESIAN_POINT('Ctrl Pts',(6.424241261,4.98224132,-3.458205105));
#159773=CARTESIAN_POINT('Ctrl Pts',(6.369839123,4.964285714,-3.555664489));
#159774=CARTESIAN_POINT('Ctrl Pts',(6.344693336,4.955986264,-3.600712219));
#159775=CARTESIAN_POINT('Ctrl Pts',(6.318912939,4.947660853,-3.645399798));
#159776=CARTESIAN_POINT('Ctrl Pts',(6.45608189200001,5.000313899,-3.298712871));
#159777=CARTESIAN_POINT('Ctrl Pts',(6.405611147,4.98224132,-3.397491781));
#159778=CARTESIAN_POINT('Ctrl Pts',(6.352142073,4.964285714,-3.494680397));
#159779=CARTESIAN_POINT('Ctrl Pts',(6.327427568,4.955986264,-3.539602974));
#159780=CARTESIAN_POINT('Ctrl Pts',(6.30208017899999,4.947660853,-3.58417151));
#159781=CARTESIAN_POINT('Ctrl Pts',(6.3030308705642,4.94797317389881,-3.58249938530178));
#159782=CARTESIAN_POINT('Ctrl Pts',(6.32942116704821,4.95664468470342,-3.536068436542));
#159783=CARTESIAN_POINT('Ctrl Pts',(6.35527594017604,4.96527388511,-3.48938640217459));
#159784=CARTESIAN_POINT('Ctrl Pts',(6.40600783802618,4.98260085337293,-3.39535297841428));
#159785=CARTESIAN_POINT('Ctrl Pts',(6.43086999418703,4.99129108928458,-3.3480245972018));
#159786=CARTESIAN_POINT('Ctrl Pts',(6.45520502561423,5.00000000025075,-3.30042846896562));
#159787=CARTESIAN_POINT('Ctrl Pts',(6.45608189200001,5.000313899,-3.298712871));
#159788=CARTESIAN_POINT('Ctrl Pts',(6.405611147,4.98224132,-3.397491781));
#159789=CARTESIAN_POINT('Ctrl Pts',(6.352142073,4.964285714,-3.494680397));
#159790=CARTESIAN_POINT('Ctrl Pts',(6.327891176,4.95614195,-3.538760292));
#159791=CARTESIAN_POINT('Ctrl Pts',(6.30303087,4.947973174,-3.582499385));
#159792=CARTESIAN_POINT('Ctrl Pts',(6.526254313,5.000313899,-3.275999914));
#159793=CARTESIAN_POINT('Ctrl Pts',(6.476131079,4.98224132,-3.375852472));
#159794=CARTESIAN_POINT('Ctrl Pts',(6.422976508,4.964285714,-3.474124865));
#159795=CARTESIAN_POINT('Ctrl Pts',(6.39886825300001,4.95614195,-3.518696306));
#159796=CARTESIAN_POINT('Ctrl Pts',(6.374143754,4.947973174,-3.562928878));
#159797=CARTESIAN_POINT('',(6.40885299445509,4.94797317334227,-3.5533767744738));
#159798=CARTESIAN_POINT('Ctrl Pts',(6.859723901,4.818630405,-2.793840961));
#159799=CARTESIAN_POINT('Ctrl Pts',(6.856394065,4.820029867,-2.802016714));
#159800=CARTESIAN_POINT('Ctrl Pts',(6.853044751,4.821428571,-2.810184506));
#159801=CARTESIAN_POINT('Ctrl Pts',(6.702931827,4.884117105,-3.176256762));
#159802=CARTESIAN_POINT('Ctrl Pts',(6.514675115,4.947973174,-3.524254171));
#159803=CARTESIAN_POINT('Ctrl Pts',(6.655681333,4.818630405,-2.874787991));
#159804=CARTESIAN_POINT('Ctrl Pts',(6.652255021,4.820029867,-2.882720556));
#159805=CARTESIAN_POINT('Ctrl Pts',(6.64880981,4.821428571,-2.890644931));
#159806=CARTESIAN_POINT('Ctrl Pts',(6.494398894,4.884117105,-3.245807475));
#159807=CARTESIAN_POINT('Ctrl Pts',(6.30303087,4.947973174,-3.582499385));
#159808=CARTESIAN_POINT('Ctrl Pts',(6.6538178429181,4.81939091791731,-2.87909853968817));
#159809=CARTESIAN_POINT('Ctrl Pts',(6.67033817410486,4.8223472472397,-2.88644139503092));
#159810=CARTESIAN_POINT('Ctrl Pts',(6.68686360748816,4.82527010311368,-2.89378637035384));
#159811=CARTESIAN_POINT('Ctrl Pts',(6.7033999037213,4.8281632174832,-2.90111850959978));
#159812=CARTESIAN_POINT('Ctrl Pts',(6.71888040393875,4.83087161463545,-2.90798251237229));
#159813=CARTESIAN_POINT('Ctrl Pts',(6.73436889977429,4.83355328551508,-2.91483908496541));
#159814=CARTESIAN_POINT('Ctrl Pts',(6.74986497879421,4.8362090438618,-2.92168848777077));
#159815=CARTESIAN_POINT('Ctrl Pts',(6.7653612241887,4.83886483072222,-2.92853796411515));
#159816=CARTESIAN_POINT('Ctrl Pts',(6.78086509422502,4.84149471140405,-2.93538028861221));
#159817=CARTESIAN_POINT('Ctrl Pts',(6.79637620263612,4.84409946426182,-2.9422157054656));
#159818=CARTESIAN_POINT('Ctrl Pts',(7.03071436425429,4.94924836941368,-2.33033886258751));
#159819=CARTESIAN_POINT('Ctrl Pts',(7.02944803762714,4.94861077170685,-2.33414560129375));
#159820=CARTESIAN_POINT('Ctrl Pts',(7.028181711,4.947973174,-2.33795234));
#159821=CARTESIAN_POINT('Ctrl Pts',(6.900820226,4.88384644,-2.720817143));
#159822=CARTESIAN_POINT('Ctrl Pts',(6.73262222,4.818610636,-3.08758115));
#159823=CARTESIAN_POINT('Ctrl Pts',(6.92812328853911,4.94924836941368,-2.13627464941378));
#159824=CARTESIAN_POINT('Ctrl Pts',(6.92696213476956,4.94861077170685,-2.14002593470689));
#159825=CARTESIAN_POINT('Ctrl Pts',(6.92580098100001,4.947973174,-2.14377722));
#159826=CARTESIAN_POINT('Ctrl Pts',(6.809017313,4.88384644,-2.521064766));
#159827=CARTESIAN_POINT('Ctrl Pts',(6.651940379,4.818610636,-2.883433576));
#159828=CARTESIAN_POINT('',(6.9430010461971,4.94797317334248,-2.17639882768109));
#159829=CARTESIAN_POINT('Ctrl Pts',(6.92673643454702,4.94745154526473,-2.1407550938548));
#159830=CARTESIAN_POINT('Ctrl Pts',(6.92626870777351,4.94771235963237,-2.1422661569274));
#159831=CARTESIAN_POINT('Ctrl Pts',(6.925800981,4.947973174,-2.14377722));
#159832=CARTESIAN_POINT('Ctrl Pts',(6.878968119,4.97408817100001,-2.295077963));
#159833=CARTESIAN_POINT('Ctrl Pts',(6.825572471,5.00031307,-2.444189118));
#159834=CARTESIAN_POINT('Ctrl Pts',(6.96116503193408,4.94745154526473,-2.20598330608988));
#159835=CARTESIAN_POINT('Ctrl Pts',(6.96068307046704,4.94771235963237,-2.20750187454494));
#159836=CARTESIAN_POINT('Ctrl Pts',(6.960201109,4.947973174,-2.209020443));
#159837=CARTESIAN_POINT('Ctrl Pts',(6.911942946,4.97408817100001,-2.36107269));
#159838=CARTESIAN_POINT('Ctrl Pts',(6.857090538,5.00031307,-2.510872388));
#159839=CARTESIAN_POINT('Origin',(-0.180064974145001,5.08925699270593,0.080132333575427));
#159840=CARTESIAN_POINT('Ctrl Pts',(6.982521361,4.94766207,-2.112343688));
#159841=CARTESIAN_POINT('Ctrl Pts',(6.936100192,4.973931887,-2.265792583));
#159842=CARTESIAN_POINT('Ctrl Pts',(6.882982665,5.00031307,-2.417054001));
#159843=CARTESIAN_POINT('Ctrl Pts',(6.926358667,4.94766207,-2.1419747));
#159844=CARTESIAN_POINT('Ctrl Pts',(6.879286323,4.973931887,-2.294189355));
#159845=CARTESIAN_POINT('Ctrl Pts',(6.825572471,5.00031307,-2.444189118));
#159846=CARTESIAN_POINT('Ctrl Pts',(6.92580050069003,4.94797287203559,-2.1437791256559));
#159847=CARTESIAN_POINT('Ctrl Pts',(6.93080204135417,4.94882769742158,-2.14528316368062));
#159848=CARTESIAN_POINT('Ctrl Pts',(6.93580375378228,4.94967947055423,-2.14678836796916));
#159849=CARTESIAN_POINT('Ctrl Pts',(6.94080614265597,4.95052852743683,-2.14829285226673));
#159850=CARTESIAN_POINT('Ctrl Pts',(6.94545016576042,4.95131675879576,-2.14968955692418));
#159851=CARTESIAN_POINT('Ctrl Pts',(6.95009477335998,4.95210264918661,-2.1510856413952));
#159852=CARTESIAN_POINT('Ctrl Pts',(6.95473995609888,4.95288622031847,-2.15248111144501));
#159853=CARTESIAN_POINT('Ctrl Pts',(6.95938514353082,4.95366979224198,-2.15387658290467));
#159854=CARTESIAN_POINT('Ctrl Pts',(6.96403090727515,4.95445104509922,-2.15527144029312));
#159855=CARTESIAN_POINT('Ctrl Pts',(6.96867723835465,4.95523000034217,-2.1566656893329));
#159856=CARTESIAN_POINT('Ctrl Pts',(7.04635258300001,5.000313899,-1.88852209));
#159857=CARTESIAN_POINT('Ctrl Pts',(7.017457945,4.98224132,-1.99633222));
#159858=CARTESIAN_POINT('Ctrl Pts',(6.985278584,4.964285714,-2.103207909));
#159859=CARTESIAN_POINT('Ctrl Pts',(6.970404623,4.955986264,-2.152608049));
#159860=CARTESIAN_POINT('Ctrl Pts',(6.954833465,4.947660853,-2.20179288));
#159861=CARTESIAN_POINT('Ctrl Pts',(7.014268043,5.000313899,-1.833724031));
#159862=CARTESIAN_POINT('Ctrl Pts',(6.986211822,4.98224132,-1.941043263));
#159863=CARTESIAN_POINT('Ctrl Pts',(6.954885505,4.964285714,-2.047453934));
#159864=CARTESIAN_POINT('Ctrl Pts',(6.940405838,4.955986264,-2.096639133));
#159865=CARTESIAN_POINT('Ctrl Pts',(6.925231974,4.947660853,-2.145614621));
#159866=CARTESIAN_POINT('Ctrl Pts',(6.92580079412434,4.94797303316317,-2.14377817766412));
#159867=CARTESIAN_POINT('Ctrl Pts',(6.93572593790158,4.95342302531133,-2.11171322693376));
#159868=CARTESIAN_POINT('Ctrl Pts',(6.94542096528859,4.9588608327439,-2.07960351790515));
#159869=CARTESIAN_POINT('Ctrl Pts',(6.95488550519347,4.96428571402583,-2.04745393411916));
#159870=CARTESIAN_POINT('Ctrl Pts',(6.97555298415225,4.97613189126264,-1.97724969495794));
#159871=CARTESIAN_POINT('Ctrl Pts',(6.99519251853477,4.98803923908107,-1.9066126073206));
#159872=CARTESIAN_POINT('Ctrl Pts',(7.01378048014667,5.00000000026952,-1.83558801947581));
#159873=CARTESIAN_POINT('Ctrl Pts',(7.014268043,5.000313899,-1.833724031));
#159874=CARTESIAN_POINT('Ctrl Pts',(6.986211822,4.98224132,-1.941043263));
#159875=CARTESIAN_POINT('Ctrl Pts',(6.954885505,4.964285714,-2.047453934));
#159876=CARTESIAN_POINT('Ctrl Pts',(6.940677455,4.95614195,-2.095716491));
#159877=CARTESIAN_POINT('Ctrl Pts',(6.925800981,4.947973174,-2.14377722));
#159878=CARTESIAN_POINT('Ctrl Pts',(7.077917257,5.000313899,-1.796457094));
#159879=CARTESIAN_POINT('Ctrl Pts',(7.050431225,4.98224132,-1.904750168));
#159880=CARTESIAN_POINT('Ctrl Pts',(7.019645038,4.964285714,-2.012151669));
#159881=CARTESIAN_POINT('Ctrl Pts',(7.005681963,4.95614195,-2.060863616));
#159882=CARTESIAN_POINT('Ctrl Pts',(6.991044205,4.947973174,-2.109377092));
#159883=CARTESIAN_POINT('',(7.02288854215139,4.94797317334226,-2.09258685113586));
#159884=CARTESIAN_POINT('Ctrl Pts',(7.299940589,4.81863040500001,-1.253884645));
#159885=CARTESIAN_POINT('Ctrl Pts',(7.298446148,4.820029867,-1.262585069));
#159886=CARTESIAN_POINT('Ctrl Pts',(7.296930973,4.821428571,-1.271281907));
#159887=CARTESIAN_POINT('Ctrl Pts',(7.22902232,4.884117105,-1.661065438));
#159888=CARTESIAN_POINT('Ctrl Pts',(7.11997610100001,4.947973174,-2.04139649));
#159889=CARTESIAN_POINT('Ctrl Pts',(7.118069642,4.81863040500001,-1.376802299));
#159890=CARTESIAN_POINT('Ctrl Pts',(7.116428702,4.820029867,-1.385285961));
#159891=CARTESIAN_POINT('Ctrl Pts',(7.114767544,4.821428571,-1.393765687));
#159892=CARTESIAN_POINT('Ctrl Pts',(7.040316119,4.884117105,-1.77381851));
#159893=CARTESIAN_POINT('Ctrl Pts',(6.925800981,4.947973174,-2.14377722));
#159894=CARTESIAN_POINT('Ctrl Pts',(7.11717635922453,4.81939091801856,-1.381412664868));
#159895=CARTESIAN_POINT('Ctrl Pts',(7.13488895149142,4.82234724724486,-1.38503246517534));
#159896=CARTESIAN_POINT('Ctrl Pts',(7.15260698192933,4.82527010311933,-1.38865323946183));
#159897=CARTESIAN_POINT('Ctrl Pts',(7.17033286187557,4.82816321748676,-1.39225914256787));
#159898=CARTESIAN_POINT('Ctrl Pts',(7.18692699429999,4.8308716146483,-1.39563481891414));
#159899=CARTESIAN_POINT('Ctrl Pts',(7.20352733814408,4.83355328553553,-1.39900151995689));
#159900=CARTESIAN_POINT('Ctrl Pts',(7.22013354659239,4.8362090438886,-1.40235958866371));
#159901=CARTESIAN_POINT('Ctrl Pts',(7.23673993333435,4.83886483075539,-1.40571769342466));
#159902=CARTESIAN_POINT('Ctrl Pts',(7.25335222902539,4.84149471144234,-1.40906717445856));
#159903=CARTESIAN_POINT('Ctrl Pts',(7.26997010912512,4.84409946433572,-1.41240835333832));
#159904=CARTESIAN_POINT('Ctrl Pts',(7.36729414063743,4.94924836941368,-0.764461072856926));
#159905=CARTESIAN_POINT('Ctrl Pts',(7.36687575631872,4.94861077170684,-0.768451034928463));
#159906=CARTESIAN_POINT('Ctrl Pts',(7.366457372,4.947973174,-0.772440997000001));
#159907=CARTESIAN_POINT('Ctrl Pts',(7.324378143,4.88384644,-1.173733589));
#159908=CARTESIAN_POINT('Ctrl Pts',(7.238955932,4.818610636,-1.568080456));
#159909=CARTESIAN_POINT('Ctrl Pts',(7.22538351839981,4.94924836941368,-0.596988021858047));
#159910=CARTESIAN_POINT('Ctrl Pts',(7.2250559271999,4.94861077170684,-0.600901217929023));
#159911=CARTESIAN_POINT('Ctrl Pts',(7.224728336,4.947973174,-0.604814414));
#159912=CARTESIAN_POINT('Ctrl Pts',(7.191780674,4.88384644,-0.998386224));
#159913=CARTESIAN_POINT('Ctrl Pts',(7.116274695,4.818610636,-1.38604995));
#159914=CARTESIAN_POINT('',(7.24853895434816,4.94797317334248,-0.632975841513029));
#159915=CARTESIAN_POINT('Ctrl Pts',(7.2249922513874,4.94745154526473,-0.601661848617231));
#159916=CARTESIAN_POINT('Ctrl Pts',(7.2248602936937,4.94771235963237,-0.603238131308616));
#159917=CARTESIAN_POINT('Ctrl Pts',(7.224728336,4.947973174,-0.604814414));
#159918=CARTESIAN_POINT('Ctrl Pts',(7.211515587,4.97408817100001,-0.762645510999999));
#159919=CARTESIAN_POINT('Ctrl Pts',(7.19142279,5.00031307,-0.919749016));
#159920=CARTESIAN_POINT('Ctrl Pts',(7.27263806430311,4.94745154526473,-0.657963931735703));
#159921=CARTESIAN_POINT('Ctrl Pts',(7.27249381815156,4.94771235963237,-0.659550604367851));
#159922=CARTESIAN_POINT('Ctrl Pts',(7.272349572,4.947973174,-0.661137277));
#159923=CARTESIAN_POINT('Ctrl Pts',(7.257906396,4.97408817100001,-0.820008705));
#159924=CARTESIAN_POINT('Ctrl Pts',(7.236538914,5.00031307,-0.978097815));
#159925=CARTESIAN_POINT('Origin',(-0.19308164471352,5.08925706922526,0.0395503117135843));
#159926=CARTESIAN_POINT('Ctrl Pts',(7.273365344,4.94766207,-0.561922576));
#159927=CARTESIAN_POINT('Ctrl Pts',(7.261016453,4.973931887,-0.7217631));
#159928=CARTESIAN_POINT('Ctrl Pts',(7.241657518,5.00031307,-0.880906808));
#159929=CARTESIAN_POINT('Ctrl Pts',(7.224885495,4.94766207,-0.602934150000001));
#159930=CARTESIAN_POINT('Ctrl Pts',(7.211635327,4.973931887,-0.761709274));
#159931=CARTESIAN_POINT('Ctrl Pts',(7.19142279,5.00031307,-0.919749016));
#159932=CARTESIAN_POINT('Ctrl Pts',(7.22472827651318,4.94797287212304,-0.604816378418453));
#159933=CARTESIAN_POINT('Ctrl Pts',(7.22993620750882,4.94882769746256,-0.605210069807342));
#159934=CARTESIAN_POINT('Ctrl Pts',(7.23514455707306,4.94967947060204,-0.605604862983575));
#159935=CARTESIAN_POINT('Ctrl Pts',(7.24035341250809,4.95052852749047,-0.605998807567377));
#159936=CARTESIAN_POINT('Ctrl Pts',(7.24518911107269,4.95131675884529,-0.606364530379651));
#159937=CARTESIAN_POINT('Ctrl Pts',(7.25002524716207,4.95210264923163,-0.606729521840045));
#159938=CARTESIAN_POINT('Ctrl Pts',(7.25486181286332,4.95288622035671,-0.607093789592621));
#159939=CARTESIAN_POINT('Ctrl Pts',(7.25969838345099,4.95366979227343,-0.607458057713219));
#159940=CARTESIAN_POINT('Ctrl Pts',(7.26453538487142,4.95445104512166,-0.60782160221566));
#159941=CARTESIAN_POINT('Ctrl Pts',(7.26937280966497,4.9552300003664,-0.60818443062782));
#159942=CARTESIAN_POINT('Ctrl Pts',(7.287589201,5.000313899,-0.329611976));
#159943=CARTESIAN_POINT('Ctrl Pts',(7.282546094,4.98224132,-0.441113058));
#159944=CARTESIAN_POINT('Ctrl Pts',(7.274094183,4.964285714,-0.552407665));
#159945=CARTESIAN_POINT('Ctrl Pts',(7.27018753600001,4.955986264,-0.603850319));
#159946=CARTESIAN_POINT('Ctrl Pts',(7.265553708,4.947660853,-0.655232575));
#159947=CARTESIAN_POINT('Ctrl Pts',(7.244474816,5.000313899,-0.282992293));
#159948=CARTESIAN_POINT('Ctrl Pts',(7.240144997,4.98224132,-0.393833719));
#159949=CARTESIAN_POINT('Ctrl Pts',(7.23242622,4.964285714,-0.5044908));
#159950=CARTESIAN_POINT('Ctrl Pts',(7.228858443,4.955986264,-0.555638777));
#159951=CARTESIAN_POINT('Ctrl Pts',(7.22456761900001,4.947660853,-0.606731178));
#159952=CARTESIAN_POINT('Ctrl Pts',(7.22472835929903,4.94797303325467,-0.604815389485618));
#159953=CARTESIAN_POINT('Ctrl Pts',(7.22752844201957,4.95342302547636,-0.571366486962385));
#159954=CARTESIAN_POINT('Ctrl Pts',(7.23009416642667,4.95886083287659,-0.537923340666376));
#159955=CARTESIAN_POINT('Ctrl Pts',(7.23242622053074,4.96428571409676,-0.504490799966201));
#159956=CARTESIAN_POINT('Ctrl Pts',(7.2375186690733,4.97613189123871,-0.431484999790809));
#159957=CARTESIAN_POINT('Ctrl Pts',(7.24151415645778,4.98803923915467,-0.358277448234716));
#159958=CARTESIAN_POINT('Ctrl Pts',(7.24439935455547,5.00000000038041,-0.28491751337921));
#159959=CARTESIAN_POINT('Ctrl Pts',(7.244474816,5.000313899,-0.282992293));
#159960=CARTESIAN_POINT('Ctrl Pts',(7.240144997,4.98224132,-0.393833719));
#159961=CARTESIAN_POINT('Ctrl Pts',(7.23242622,4.964285714,-0.5044908));
#159962=CARTESIAN_POINT('Ctrl Pts',(7.22892537,4.95614195,-0.554679316000001));
#159963=CARTESIAN_POINT('Ctrl Pts',(7.224728336,4.947973174,-0.604814414));
#159964=CARTESIAN_POINT('Ctrl Pts',(7.298624658,5.000313899,-0.232913937));
#159965=CARTESIAN_POINT('Ctrl Pts',(7.295061043,4.98224132,-0.344583863));
#159966=CARTESIAN_POINT('Ctrl Pts',(7.288082768,4.964285714,-0.456092497));
#159967=CARTESIAN_POINT('Ctrl Pts',(7.28491777100001,4.95614195,-0.506667235));
#159968=CARTESIAN_POINT('Ctrl Pts',(7.281051199,4.947973174,-0.557193178));
#159969=CARTESIAN_POINT('',(7.3085416277938,4.94797317334222,-0.533949891478464));
#159970=CARTESIAN_POINT('Ctrl Pts',(7.398820169,4.818630405,0.344701923));
#159971=CARTESIAN_POINT('Ctrl Pts',(7.399231002,4.820029867,0.335883649));
#159972=CARTESIAN_POINT('Ctrl Pts',(7.399620813,4.821428571,0.327064421));
#159973=CARTESIAN_POINT('Ctrl Pts',(7.417091764,4.884117105,-0.068204541));
#159974=CARTESIAN_POINT('Ctrl Pts',(7.392354919,4.947973174,-0.463085377));
#159975=CARTESIAN_POINT('Ctrl Pts',(7.247624926,4.818630405,0.185561138));
#159976=CARTESIAN_POINT('Ctrl Pts',(7.247846087,4.820029867,0.176923066));
#159977=CARTESIAN_POINT('Ctrl Pts',(7.248046656,4.821428571,0.168284491));
#159978=CARTESIAN_POINT('Ctrl Pts',(7.257035987,4.884117105,-0.218887764));
#159979=CARTESIAN_POINT('Ctrl Pts',(7.224728336,4.947973174,-0.604814414));
#159980=CARTESIAN_POINT('Ctrl Pts',(7.2477436202233,4.81939091791719,0.180866530341205));
#159981=CARTESIAN_POINT('Ctrl Pts',(7.26582025148185,4.82234724725628,0.181139042606722));
#159982=CARTESIAN_POINT('Ctrl Pts',(7.28390240363902,4.82527010311953,0.181411772860868));
#159983=CARTESIAN_POINT('Ctrl Pts',(7.30198902492249,4.82816321747991,0.181700714026033));
#159984=CARTESIAN_POINT('Ctrl Pts',(7.31892086638338,4.83087161463771,0.181971207111691));
#159985=CARTESIAN_POINT('Ctrl Pts',(7.33585684461923,4.83355328552332,0.182251800924294));
#159986=CARTESIAN_POINT('Ctrl Pts',(7.35279669465095,4.83620904387642,0.182542085962254));
#159987=CARTESIAN_POINT('Ctrl Pts',(7.3697367265584,4.83886483074323,0.182832374116876));
#159988=CARTESIAN_POINT('Ctrl Pts',(7.38668067542047,4.84149471143185,0.183132354622081));
#159989=CARTESIAN_POINT('Ctrl Pts',(7.40362829344876,4.84409946433362,0.183441643659611));
#159990=CARTESIAN_POINT('Ctrl Pts',(7.3593874306487,4.94924836941369,0.837162067481764));
#159991=CARTESIAN_POINT('Ctrl Pts',(7.35983655182435,4.94861077170684,0.833175448240883));
#159992=CARTESIAN_POINT('Ctrl Pts',(7.360285673,4.947973174,0.829188829));
#159993=CARTESIAN_POINT('Ctrl Pts',(7.405456278,4.88384644,0.428232444));
#159994=CARTESIAN_POINT('Ctrl Pts',(7.406804111,4.818610636,0.024741937));
#159995=CARTESIAN_POINT('Ctrl Pts',(7.18479284462102,4.94924836941369,0.970213102287845));
#159996=CARTESIAN_POINT('Ctrl Pts',(7.18531413381051,4.94861077170684,0.966320972143923));
#159997=CARTESIAN_POINT('Ctrl Pts',(7.185835423,4.947973174,0.962428842));
#159998=CARTESIAN_POINT('Ctrl Pts',(7.238264365,4.88384644,0.570975749));
#159999=CARTESIAN_POINT('Ctrl Pts',(7.24785991500001,4.818610636,0.176143831));
#160000=CARTESIAN_POINT('',(7.21514323698324,4.94797317334286,0.940044391966286));
#160001=CARTESIAN_POINT('Ctrl Pts',(7.18541545982678,4.94745154526474,0.965564436160455));
#160002=CARTESIAN_POINT('Ctrl Pts',(7.18562544141339,4.94771235963236,0.963996639080227));
#160003=CARTESIAN_POINT('Ctrl Pts',(7.185835423,4.947973174,0.962428842));
#160004=CARTESIAN_POINT('Ctrl Pts',(7.206860601,4.97408817100001,0.805447398));
#160005=CARTESIAN_POINT('Ctrl Pts',(7.221010173,5.00031307,0.647697528));
#160006=CARTESIAN_POINT('Ctrl Pts',(7.24405062408982,4.94745154526474,0.920821105528827));
#160007=CARTESIAN_POINT('Ctrl Pts',(7.2442508380449,4.94771235963236,0.919240519764414));
#160008=CARTESIAN_POINT('Ctrl Pts',(7.244451052,4.947973174,0.917659934));
#160009=CARTESIAN_POINT('Ctrl Pts',(7.26449821,4.97408817100001,0.759397976));
#160010=CARTESIAN_POINT('Ctrl Pts',(7.277614774,5.00031307,0.600411524));
#160011=CARTESIAN_POINT('Origin',(-0.197070757240472,5.08925702468576,-0.00288134842447038));
#160012=CARTESIAN_POINT('Ctrl Pts',(7.224114848,4.94766207,1.014773411));
#160013=CARTESIAN_POINT('Ctrl Pts',(7.246415654,4.973931887,0.856015224000001));
#160014=CARTESIAN_POINT('Ctrl Pts',(7.26172051400001,5.00031307,0.696430608));
#160015=CARTESIAN_POINT('Ctrl Pts',(7.185584706,4.94766207,0.96429893));
#160016=CARTESIAN_POINT('Ctrl Pts',(7.206776278,4.973931887,0.806387487000001));
#160017=CARTESIAN_POINT('Ctrl Pts',(7.221010173,5.00031307,0.647697528));
#160018=CARTESIAN_POINT('Ctrl Pts',(7.18583578693528,4.94797287209165,0.962426910232247));
#160019=CARTESIAN_POINT('Ctrl Pts',(7.19100659134204,4.94882769740662,0.963161974412689));
#160020=CARTESIAN_POINT('Ctrl Pts',(7.19617804139228,4.94967947052024,0.963896052513582));
#160021=CARTESIAN_POINT('Ctrl Pts',(7.20134980306533,4.95052852738558,0.964631068107125));
#160022=CARTESIAN_POINT('Ctrl Pts',(7.20615106539685,4.95131675874708,0.965313427988624));
#160023=CARTESIAN_POINT('Ctrl Pts',(7.21095259780624,4.95210264914231,0.965996596171963));
#160024=CARTESIAN_POINT('Ctrl Pts',(7.21575439420849,4.95288622027866,0.96668056348834));
#160025=CARTESIAN_POINT('Ctrl Pts',(7.22055619546201,4.95366979220666,0.967364531495733));
#160026=CARTESIAN_POINT('Ctrl Pts',(7.22535826191999,4.9544510450685,0.968049298811043));
#160027=CARTESIAN_POINT('Ctrl Pts',(7.23016058785084,4.95523000031898,0.968734856467267));
#160028=CARTESIAN_POINT('Ctrl Pts',(7.188066246,5.000313899,1.244710427));
#160029=CARTESIAN_POINT('Ctrl Pts',(7.20711048100001,4.98224132,1.13473206));
#160030=CARTESIAN_POINT('Ctrl Pts',(7.222781222,4.964285714,1.024222548));
#160031=CARTESIAN_POINT('Ctrl Pts',(7.230024561,4.955986264,0.973142781));
#160032=CARTESIAN_POINT('Ctrl Pts',(7.236544735,4.947660853,0.921965678));
#160033=CARTESIAN_POINT('Ctrl Pts',(7.135937999,5.000313899,1.28097185));
#160034=CARTESIAN_POINT('Ctrl Pts',(7.155537038,4.98224132,1.171791051));
#160035=CARTESIAN_POINT('Ctrl Pts',(7.171786724,4.964285714,1.062061763));
#160036=CARTESIAN_POINT('Ctrl Pts',(7.179297663,4.955986264,1.01134263));
#160037=CARTESIAN_POINT('Ctrl Pts',(7.186090511,4.947660853,0.960522341));
#160038=CARTESIAN_POINT('Ctrl Pts',(7.18583565516621,4.94797303325765,0.962427894050688));
#160039=CARTESIAN_POINT('Ctrl Pts',(7.1813797480107,4.95342302539181,0.995696714765073));
#160040=CARTESIAN_POINT('Ctrl Pts',(7.17669620014671,4.95886083279384,1.02890953346614));
#160041=CARTESIAN_POINT('Ctrl Pts',(7.17178672409145,4.96428571393831,1.06206176259658));
#160042=CARTESIAN_POINT('Ctrl Pts',(7.16106602474189,4.97613189084492,1.13445545159152));
#160043=CARTESIAN_POINT('Ctrl Pts',(7.14923064057945,4.98803923896588,1.20681036385963));
#160044=CARTESIAN_POINT('Ctrl Pts',(7.13627816756702,5.00000000009595,1.27907541649019));
#160045=CARTESIAN_POINT('Ctrl Pts',(7.135937999,5.000313899,1.28097185));
#160046=CARTESIAN_POINT('Ctrl Pts',(7.155537038,4.98224132,1.171791051));
#160047=CARTESIAN_POINT('Ctrl Pts',(7.171786724,4.964285714,1.062061763));
#160048=CARTESIAN_POINT('Ctrl Pts',(7.179156768,4.95614195,1.012294047));
#160049=CARTESIAN_POINT('Ctrl Pts',(7.185835423,4.947973174,0.962428842));
#160050=CARTESIAN_POINT('Ctrl Pts',(7.178056481,5.000313899,1.341520017));
#160051=CARTESIAN_POINT('Ctrl Pts',(7.198581915,4.98224132,1.2316948));
#160052=CARTESIAN_POINT('Ctrl Pts',(7.215737847,4.964285714,1.121293053));
#160053=CARTESIAN_POINT('Ctrl Pts',(7.22351892000001,4.95614195,1.071220344));
#160054=CARTESIAN_POINT('Ctrl Pts',(7.23060433,4.947973174,1.021044471));
#160055=CARTESIAN_POINT('',(7.25245542892245,4.94797317334225,1.04965397099054));
#160056=CARTESIAN_POINT('Ctrl Pts',(7.15173914100001,4.818630405,1.927170612));
#160057=CARTESIAN_POINT('Ctrl Pts',(7.154036037,4.820029867,1.918646822));
#160058=CARTESIAN_POINT('Ctrl Pts',(7.156312608,4.821428571,1.91011758));
#160059=CARTESIAN_POINT('Ctrl Pts',(7.258346241,4.884117105,1.527845525));
#160060=CARTESIAN_POINT('Ctrl Pts',(7.319075436,4.947973174,1.136879092));
#160061=CARTESIAN_POINT('Ctrl Pts',(7.038289323,4.818630405,1.739247943));
#160062=CARTESIAN_POINT('Ctrl Pts',(7.040362243,4.820029867,1.730859367));
#160063=CARTESIAN_POINT('Ctrl Pts',(7.042415162,4.821428571,1.722465874));
#160064=CARTESIAN_POINT('Ctrl Pts',(7.134424917,4.884117105,1.346277931));
#160065=CARTESIAN_POINT('Ctrl Pts',(7.185835423,4.947973174,0.962428842));
#160066=CARTESIAN_POINT('Ctrl Pts',(7.03941444436566,4.81939091775252,1.73468860817442));
#160067=CARTESIAN_POINT('Ctrl Pts',(7.05700987218026,4.82234724734587,1.73884069106666));
#160068=CARTESIAN_POINT('Ctrl Pts',(7.0746106448554,4.82527010316785,1.74299417296875));
#160069=CARTESIAN_POINT('Ctrl Pts',(7.09221229723318,4.82816321752951,1.74716444778148));
#160070=CARTESIAN_POINT('Ctrl Pts',(7.10869013359083,4.83087161467271,1.75106846227147));
#160071=CARTESIAN_POINT('Ctrl Pts',(7.12516983864926,4.83355328554229,1.75498323062839));
#160072=CARTESIAN_POINT('Ctrl Pts',(7.1416512416553,4.8362090438783,1.7589082959611));
#160073=CARTESIAN_POINT('Ctrl Pts',(7.15813282161496,4.83886483072803,1.76283340343552));
#160074=CARTESIAN_POINT('Ctrl Pts',(7.17461614338329,4.84149471139851,1.76676881869245));
#160075=CARTESIAN_POINT('Ctrl Pts',(7.19110104734923,4.84409946426157,1.77071411358907));
#160076=CARTESIAN_POINT('Ctrl Pts',(7.0073639444683,4.94924836941368,2.39964043902942));
#160077=CARTESIAN_POINT('Ctrl Pts',(7.00865957073415,4.94861077170684,2.39584357251471));
#160078=CARTESIAN_POINT('Ctrl Pts',(7.009955197,4.947973174,2.392046706));
#160079=CARTESIAN_POINT('Ctrl Pts',(7.140263509,4.88384644,2.010174804));
#160080=CARTESIAN_POINT('Ctrl Pts',(7.228318362,4.818610636,1.616407425));
#160081=CARTESIAN_POINT('Ctrl Pts',(6.80824924266725,4.94924836941368,2.49204813906551));
#160082=CARTESIAN_POINT('Ctrl Pts',(6.80959503733362,4.94861077170684,2.48835906653275));
#160083=CARTESIAN_POINT('Ctrl Pts',(6.810940832,4.947973174,2.484669994));
#160084=CARTESIAN_POINT('Ctrl Pts',(6.94629485800001,4.88384644,2.11363953));
#160085=CARTESIAN_POINT('Ctrl Pts',(7.040543261,4.818610636,1.730101323));
#160086=CARTESIAN_POINT('',(6.84437544064191,4.94797317334249,2.46910919426462));
#160087=CARTESIAN_POINT('Ctrl Pts',(6.80985662727826,4.94745154526473,2.48764200003715));
#160088=CARTESIAN_POINT('Ctrl Pts',(6.81039872963913,4.94771235963237,2.48615599701857));
#160089=CARTESIAN_POINT('Ctrl Pts',(6.810940832,4.947973174,2.484669994));
#160090=CARTESIAN_POINT('Ctrl Pts',(6.865220823,4.97408817100001,2.335878481));
#160091=CARTESIAN_POINT('Ctrl Pts',(6.912951145,5.00031307,2.184858455));
#160092=CARTESIAN_POINT('Ctrl Pts',(6.87673942742404,4.94745154526473,2.45654957195124));
#160093=CARTESIAN_POINT('Ctrl Pts',(6.87727473971202,4.94771235963237,2.45504897947562));
#160094=CARTESIAN_POINT('Ctrl Pts',(6.877810052,4.947973174,2.453548387));
#160095=CARTESIAN_POINT('Ctrl Pts',(6.931410162,4.97408817100001,2.303296051));
#160096=CARTESIAN_POINT('Ctrl Pts',(6.978397455,5.00031307,2.150846288));
#160097=CARTESIAN_POINT('Origin',(-0.191843328106668,5.08925706687508,-0.0451781557118802));
#160098=CARTESIAN_POINT('Ctrl Pts',(6.83707277,4.94766207,2.544019722));
#160099=CARTESIAN_POINT('Ctrl Pts',(6.892980514,4.973931887,2.393767227));
#160100=CARTESIAN_POINT('Ctrl Pts',(6.942233529,5.00031307,2.241203703));
#160101=CARTESIAN_POINT('Ctrl Pts',(6.810293963,4.94766207,2.486442465));
#160102=CARTESIAN_POINT('Ctrl Pts',(6.86493638100001,4.973931887,2.336778465));
#160103=CARTESIAN_POINT('Ctrl Pts',(6.912951145,5.00031307,2.184858455));
#160104=CARTESIAN_POINT('Ctrl Pts',(6.81094160271618,4.94797287204861,2.48466818632));
#160105=CARTESIAN_POINT('Ctrl Pts',(6.81583349962326,4.94882769745355,2.48649763558292));
#160106=CARTESIAN_POINT('Ctrl Pts',(6.82072623906249,4.94967947058637,2.48832626024999));
#160107=CARTESIAN_POINT('Ctrl Pts',(6.82561908128822,4.95052852746818,2.49015586746808));
#160108=CARTESIAN_POINT('Ctrl Pts',(6.83016140554712,4.95131675882604,2.49185440358831));
#160109=CARTESIAN_POINT('Ctrl Pts',(6.8347038197908,4.95210264921486,2.49355378715903));
#160110=CARTESIAN_POINT('Ctrl Pts',(6.83924632006457,4.95288622034428,2.49525400793252));
#160111=CARTESIAN_POINT('Ctrl Pts',(6.84378882492764,4.95366979226534,2.49695423042375));
#160112=CARTESIAN_POINT('Ctrl Pts',(6.84833141696647,4.95445104511974,2.49865529054903));
#160113=CARTESIAN_POINT('Ctrl Pts',(6.85287409254451,4.95523000036724,2.50035717833961));
#160114=CARTESIAN_POINT('Ctrl Pts',(6.752437304,5.000313899,2.760831554));
#160115=CARTESIAN_POINT('Ctrl Pts',(6.794678393,4.98224132,2.657518367));
#160116=CARTESIAN_POINT('Ctrl Pts',(6.833739039,4.964285714,2.552961253));
#160117=CARTESIAN_POINT('Ctrl Pts',(6.851793672,4.955986264,2.504632806));
#160118=CARTESIAN_POINT('Ctrl Pts',(6.86916297300001,4.947660853,2.45605384));
#160119=CARTESIAN_POINT('Ctrl Pts',(6.693732651,5.000313899,2.785039173));
#160120=CARTESIAN_POINT('Ctrl Pts',(6.73634412,4.98224132,2.682624175));
#160121=CARTESIAN_POINT('Ctrl Pts',(6.775802451,4.964285714,2.578953498));
#160122=CARTESIAN_POINT('Ctrl Pts',(6.794040902,4.955986264,2.531034781));
#160123=CARTESIAN_POINT('Ctrl Pts',(6.811599798,4.947660853,2.482862903));
#160124=CARTESIAN_POINT('Ctrl Pts',(6.81094126263909,4.94797303316575,2.4846691185281));
#160125=CARTESIAN_POINT('Ctrl Pts',(6.79943771959581,4.95342302528782,2.51620224415172));
#160126=CARTESIAN_POINT('Ctrl Pts',(6.78772389566368,4.95886083271677,2.54763174148845));
#160127=CARTESIAN_POINT('Ctrl Pts',(6.77580245123129,4.96428571398709,2.57895349783444));
#160128=CARTESIAN_POINT('Ctrl Pts',(6.74976989148222,4.97613189122178,2.64735003178943));
#160129=CARTESIAN_POINT('Ctrl Pts',(6.72265704507204,4.98803923914334,2.71546906758587));
#160130=CARTESIAN_POINT('Ctrl Pts',(6.69447254313508,5.00000000036334,2.78326020476335));
#160131=CARTESIAN_POINT('Ctrl Pts',(6.693732651,5.000313899,2.785039173));
#160132=CARTESIAN_POINT('Ctrl Pts',(6.73634412,4.98224132,2.682624175));
#160133=CARTESIAN_POINT('Ctrl Pts',(6.775802451,4.964285714,2.578953498));
#160134=CARTESIAN_POINT('Ctrl Pts',(6.793698776,4.95614194999999,2.531933665));
#160135=CARTESIAN_POINT('Ctrl Pts',(6.81094083200001,4.947973174,2.484669994));
#160136=CARTESIAN_POINT('Ctrl Pts',(6.72185036,5.000313899,2.853225986));
#160137=CARTESIAN_POINT('Ctrl Pts',(6.76550509700001,4.98224132,2.750380783));
#160138=CARTESIAN_POINT('Ctrl Pts',(6.805993045,4.964285714,2.646248186));
#160139=CARTESIAN_POINT('Ctrl Pts',(6.824356353,4.95614194999999,2.59901885));
#160140=CARTESIAN_POINT('Ctrl Pts',(6.84206244,4.947973174,2.551539214));
#160141=CARTESIAN_POINT('',(6.85725247507841,4.94797317334239,2.58417718027227));
#160142=CARTESIAN_POINT('Ctrl Pts',(6.570250739,4.818630405,3.419526946));
#160143=CARTESIAN_POINT('Ctrl Pts',(6.574326298,4.820029867,3.411696201));
#160144=CARTESIAN_POINT('Ctrl Pts',(6.578383179,4.821428571,3.403855764));
#160145=CARTESIAN_POINT('Ctrl Pts',(6.760208514,4.884117105,3.052455232));
#160146=CARTESIAN_POINT('Ctrl Pts',(6.903564121,4.947973174,2.683684359));
#160147=CARTESIAN_POINT('Ctrl Pts',(6.499851134,4.818630405,3.211609446));
#160148=CARTESIAN_POINT('Ctrl Pts',(6.503678886,4.820029867,3.203862607));
#160149=CARTESIAN_POINT('Ctrl Pts',(6.507488162,4.821428571,3.196106666));
#160150=CARTESIAN_POINT('Ctrl Pts',(6.678216068,4.884117105,2.848493166));
#160151=CARTESIAN_POINT('Ctrl Pts',(6.810940832,4.947973174,2.484669994));
#160152=CARTESIAN_POINT('Ctrl Pts',(6.5019300724108,4.81939091791719,3.2073985743076));
#160153=CARTESIAN_POINT('Ctrl Pts',(6.51822155404743,4.82234724730935,3.21523608098732));
#160154=CARTESIAN_POINT('Ctrl Pts',(6.53451795468387,4.82527010309894,3.22307610241689));
#160155=CARTESIAN_POINT('Ctrl Pts',(6.55081160437425,4.8281632174668,3.23093271345656));
#160156=CARTESIAN_POINT('Ctrl Pts',(6.56606495036695,4.83087161462078,3.2382877019825));
#160157=CARTESIAN_POINT('Ctrl Pts',(6.58131780960935,4.83355328550247,3.24565359466761));
#160158=CARTESIAN_POINT('Ctrl Pts',(6.59657011355836,4.8362090438514,3.25302990859615));
#160159=CARTESIAN_POINT('Ctrl Pts',(6.61182258126467,4.83886483071405,3.26040630172093));
#160160=CARTESIAN_POINT('Ctrl Pts',(6.62707453419009,4.84149471139827,3.26779313607204));
#160161=CARTESIAN_POINT('Ctrl Pts',(6.64232590857355,4.8440994642892,3.2751899592442));
#160162=CARTESIAN_POINT('Ctrl Pts',(6.32768390839934,4.94924836941368,3.8499142910946));
#160163=CARTESIAN_POINT('Ctrl Pts',(6.32976545769967,4.94861077170685,3.8464847145473));
#160164=CARTESIAN_POINT('Ctrl Pts',(6.331847007,4.947973174,3.843055138));
#160165=CARTESIAN_POINT('Ctrl Pts',(6.541199953,4.88384644,3.498123623));
#160166=CARTESIAN_POINT('Ctrl Pts',(6.71184448,4.818610636,3.132491498));
#160167=CARTESIAN_POINT('Ctrl Pts',(6.11335947344275,4.94924836941368,3.89735777600251));
#160168=CARTESIAN_POINT('Ctrl Pts',(6.11546684572137,4.94861077170685,3.89404425800126));
#160169=CARTESIAN_POINT('Ctrl Pts',(6.117574218,4.947973174,3.89073074));
#160170=CARTESIAN_POINT('Ctrl Pts',(6.329524324,4.88384644,3.557471876));
#160171=CARTESIAN_POINT('Ctrl Pts',(6.50401862899999,4.818610636,3.2031612));
#160172=CARTESIAN_POINT('',(6.15357225586438,4.94797317334249,3.88272119488466));
#160173=CARTESIAN_POINT('Ctrl Pts',(6.11587646793651,4.94745154526473,3.89340019023023));
#160174=CARTESIAN_POINT('Ctrl Pts',(6.11672534296826,4.94771235963237,3.89206546511511));
#160175=CARTESIAN_POINT('Ctrl Pts',(6.117574218,4.947973174,3.89073074));
#160176=CARTESIAN_POINT('Ctrl Pts',(6.20257095,4.97408817100001,3.757086483));
#160177=CARTESIAN_POINT('Ctrl Pts',(6.281650205,5.00031307,3.619857829));
#160178=CARTESIAN_POINT('Ctrl Pts',(6.18787953798209,4.94745154526473,3.87741250926571));
#160179=CARTESIAN_POINT('Ctrl Pts',(6.18872491799105,4.94771235963237,3.87606207613285));
#160180=CARTESIAN_POINT('Ctrl Pts',(6.189570298,4.947973174,3.874711643));
#160181=CARTESIAN_POINT('Ctrl Pts',(6.274217078,4.97408817100001,3.739494563));
#160182=CARTESIAN_POINT('Ctrl Pts',(6.352878027,5.00031307,3.60070987));
#160183=CARTESIAN_POINT('Origin',(-0.177646785006003,5.08925693465323,-0.0853629412040702));
#160184=CARTESIAN_POINT('Ctrl Pts',(6.130336769,4.94766207,3.954310498));
#160185=CARTESIAN_POINT('Ctrl Pts',(6.217237265,4.973931887,3.819589334));
#160186=CARTESIAN_POINT('Ctrl Pts',(6.29813542,5.00031307,3.681180604));
#160187=CARTESIAN_POINT('Ctrl Pts',(6.116561444,4.94766207,3.892322713));
#160188=CARTESIAN_POINT('Ctrl Pts',(6.202099688,4.973931887,3.757904278));
#160189=CARTESIAN_POINT('Ctrl Pts',(6.281650205,5.00031307,3.619857829));
#160190=CARTESIAN_POINT('Ctrl Pts',(6.11757535950015,4.94797287221035,3.89072913977308));
#160191=CARTESIAN_POINT('Ctrl Pts',(6.12195960931022,4.94882769747571,3.89356743017046));
#160192=CARTESIAN_POINT('Ctrl Pts',(6.12634485893963,4.94967947060649,3.8964050970286));
#160193=CARTESIAN_POINT('Ctrl Pts',(6.13072999775624,4.95052852749173,3.89924374556819));
#160194=CARTESIAN_POINT('Ctrl Pts',(6.13480098985002,4.95131675883662,3.90187903631836));
#160195=CARTESIAN_POINT('Ctrl Pts',(6.1388718876706,4.95210264921789,3.90451517405683));
#160196=CARTESIAN_POINT('Ctrl Pts',(6.14294268953924,4.9528862203413,3.90715214791331));
#160197=CARTESIAN_POINT('Ctrl Pts',(6.14701349552063,4.95366979225636,3.90978912443392));
#160198=CARTESIAN_POINT('Ctrl Pts',(6.15108420657628,4.95445104510628,3.91242693774001));
#160199=CARTESIAN_POINT('Ctrl Pts',(6.15515482124631,4.95523000034099,3.91506557728136));
#160200=CARTESIAN_POINT('Ctrl Pts',(6.001071897,5.000313899,4.147859266));
#160201=CARTESIAN_POINT('Ctrl Pts',(6.064534695,4.98224132,4.05604207));
#160202=CARTESIAN_POINT('Ctrl Pts',(6.125158813,4.964285714,3.962326327));
#160203=CARTESIAN_POINT('Ctrl Pts',(6.153180527,4.955986264,3.919008985));
#160204=CARTESIAN_POINT('Ctrl Pts',(6.180586785,4.947660853,3.875299654));
#160205=CARTESIAN_POINT('Ctrl Pts',(5.93853580499999,5.000313899,4.158881159));
#160206=CARTESIAN_POINT('Ctrl Pts',(6.002167238,4.98224132,4.068020773));
#160207=CARTESIAN_POINT('Ctrl Pts',(6.062989186,4.964285714,3.975256234));
#160208=CARTESIAN_POINT('Ctrl Pts',(6.091102341,4.955986264,3.932378558));
#160209=CARTESIAN_POINT('Ctrl Pts',(6.118606248,4.947660853,3.889107555));
#160210=CARTESIAN_POINT('Ctrl Pts',(6.11757421810585,4.94797317397983,3.8907307400712));
#160211=CARTESIAN_POINT('Ctrl Pts',(6.08891330775294,4.95664469842826,3.93579560534761));
#160212=CARTESIAN_POINT('Ctrl Pts',(6.05977978348553,4.96527389211456,3.98050483093599));
#160213=CARTESIAN_POINT('Ctrl Pts',(6.00046157189516,4.98260138557519,4.06937581674763));
#160214=CARTESIAN_POINT('Ctrl Pts',(5.97029573984605,4.99129055034349,4.1135054048051));
#160215=CARTESIAN_POINT('Ctrl Pts',(5.93964082487683,5.00000000023931,4.15730283636664));
#160216=CARTESIAN_POINT('Ctrl Pts',(5.93853580499999,5.000313899,4.158881159));
#160217=CARTESIAN_POINT('Ctrl Pts',(6.002167238,4.98224132,4.068020773));
#160218=CARTESIAN_POINT('Ctrl Pts',(6.062989186,4.964285714,3.975256234));
#160219=CARTESIAN_POINT('Ctrl Pts',(6.090574979,4.95614194999999,3.93318288));
#160220=CARTESIAN_POINT('Ctrl Pts',(6.117574218,4.947973174,3.89073074));
#160221=CARTESIAN_POINT('Ctrl Pts',(5.951337988,5.000313899,4.231518279));
#160222=CARTESIAN_POINT('Ctrl Pts',(6.01608078,4.98224132,4.140462018));
#160223=CARTESIAN_POINT('Ctrl Pts',(6.078007573,4.964285714,4.047467695));
#160224=CARTESIAN_POINT('Ctrl Pts',(6.106094468,4.95614194999999,4.005290123));
#160225=CARTESIAN_POINT('Ctrl Pts',(6.133593314,4.947973174,3.96272682));
#160226=CARTESIAN_POINT('',(6.14141201680087,4.94797317334243,3.99786713737824));
#160227=CARTESIAN_POINT('Ctrl Pts',(5.681544715,4.818630405,4.75199));
#160228=CARTESIAN_POINT('Ctrl Pts',(5.687208368,4.820029867,4.745218458));
#160229=CARTESIAN_POINT('Ctrl Pts',(5.692855864,4.821428571,4.738433436));
#160230=CARTESIAN_POINT('Ctrl Pts',(5.945970951,4.884117105,4.434335525));
#160231=CARTESIAN_POINT('Ctrl Pts',(6.16524982,4.947973174,4.105003528));
#160232=CARTESIAN_POINT('Ctrl Pts',(5.65748713,4.818630405,4.533799662));
#160233=CARTESIAN_POINT('Ctrl Pts',(5.662890733,4.820029867,4.52705679300001));
#160234=CARTESIAN_POINT('Ctrl Pts',(5.668278248,4.821428571,4.520301063));
#160235=CARTESIAN_POINT('Ctrl Pts',(5.90974125700001,4.884117105,4.217516027));
#160236=CARTESIAN_POINT('Ctrl Pts',(6.11757421800001,4.947973174,3.89073074));
#160237=CARTESIAN_POINT('Ctrl Pts',(5.6604226771306,4.81939091801856,4.53013414802792));
#160238=CARTESIAN_POINT('Ctrl Pts',(5.67464844079712,4.82234724726659,4.54129060488698));
#160239=CARTESIAN_POINT('Ctrl Pts',(5.68887846756111,4.82527010310083,4.55245057562458));
#160240=CARTESIAN_POINT('Ctrl Pts',(5.70310224161804,4.8281632174612,4.56362615650414));
#160241=CARTESIAN_POINT('Ctrl Pts',(5.71641786775918,4.8308716146174,4.57408820801779));
#160242=CARTESIAN_POINT('Ctrl Pts',(5.72973067446047,4.83355328549926,4.58456080411798));
#160243=CARTESIAN_POINT('Ctrl Pts',(5.7430406985932,4.83620904384686,4.59504345844529));
#160244=CARTESIAN_POINT('Ctrl Pts',(5.75635086562983,4.83886483070819,4.60552622532028));
#160245=CARTESIAN_POINT('Ctrl Pts',(5.7696582853675,4.84149471138958,4.61601907864709));
#160246=CARTESIAN_POINT('Ctrl Pts',(5.78296299265857,4.84409946425117,4.62652156278843));
#160247=CARTESIAN_POINT('Ctrl Pts',(5.35212840517261,4.94924836941368,5.12017042975023));
#160248=CARTESIAN_POINT('Ctrl Pts',(5.35489854658631,4.94861077170684,5.11726850637511));
#160249=CARTESIAN_POINT('Ctrl Pts',(5.357668688,4.94797317400001,5.114366583));
#160250=CARTESIAN_POINT('Ctrl Pts',(5.636277158,4.88384644,4.82250407099999));
#160251=CARTESIAN_POINT('Ctrl Pts',(5.88153221,4.818610636,4.50210375));
#160252=CARTESIAN_POINT('Ctrl Pts',(5.13261580896174,4.94924836941368,5.12043129408338));
#160253=CARTESIAN_POINT('Ctrl Pts',(5.13538622048087,4.94861077170684,5.11764826704169));
#160254=CARTESIAN_POINT('Ctrl Pts',(5.138156632,4.94797317400001,5.11486524));
#160255=CARTESIAN_POINT('Ctrl Pts',(5.416792268,4.88384644,4.834960791));
#160256=CARTESIAN_POINT('Ctrl Pts',(5.663373315,4.818610636,4.526444819));
#160257=CARTESIAN_POINT('',(5.175034871687,4.94797317334255,5.11478146784614));
#160258=CARTESIAN_POINT('Ctrl Pts',(5.13592472148641,4.94745154526473,5.11710731389588));
#160259=CARTESIAN_POINT('Ctrl Pts',(5.13704067674321,4.94771235963237,5.11598627694794));
#160260=CARTESIAN_POINT('Ctrl Pts',(5.138156632,4.947973174,5.11486524));
#160261=CARTESIAN_POINT('Ctrl Pts',(5.249895753,4.974088171,5.002617296));
#160262=CARTESIAN_POINT('Ctrl Pts',(5.356626283,5.00031307,4.885596675));
#160263=CARTESIAN_POINT('Ctrl Pts',(5.20968127961232,4.94745154526473,5.11697194808294));
#160264=CARTESIAN_POINT('Ctrl Pts',(5.21079719830616,4.94771235963237,5.11583481904147));
#160265=CARTESIAN_POINT('Ctrl Pts',(5.211913117,4.947973174,5.11469769));
#160266=CARTESIAN_POINT('Ctrl Pts',(5.323648577,4.974088171,5.000838466));
#160267=CARTESIAN_POINT('Ctrl Pts',(5.430305083,5.00031307,4.88220826));
#160268=CARTESIAN_POINT('Origin',(-0.155143030563726,5.08925727759442,-0.121555994973399));
#160269=CARTESIAN_POINT('Ctrl Pts',(5.136953033,4.94766207,5.17970211));
#160270=CARTESIAN_POINT('Ctrl Pts',(5.250782913,4.97393188700001,5.06681169));
#160271=CARTESIAN_POINT('Ctrl Pts',(5.359543499,5.00031307,4.949029591));
#160272=CARTESIAN_POINT('Ctrl Pts',(5.136825309,4.94766207,5.116202277));
#160273=CARTESIAN_POINT('Ctrl Pts',(5.249259707,4.97393188700001,5.003314665));
#160274=CARTESIAN_POINT('Ctrl Pts',(5.356626283,5.00031307,4.885596675));
#160275=CARTESIAN_POINT('Ctrl Pts',(5.13815809084062,4.94797287201475,5.11486392257979));
#160276=CARTESIAN_POINT('Ctrl Pts',(5.14182969055117,4.94882769741438,5.11857833976555));
#160277=CARTESIAN_POINT('Ctrl Pts',(5.1455024010555,4.94967947055841,5.12229236245135));
#160278=CARTESIAN_POINT('Ctrl Pts',(5.14917479227229,4.95052852744747,5.12600732004938));
#160279=CARTESIAN_POINT('Ctrl Pts',(5.15258409735191,4.95131675881877,5.12945614210069));
#160280=CARTESIAN_POINT('Ctrl Pts',(5.15599312825447,4.95210264921763,5.13290577107319));
#160281=CARTESIAN_POINT('Ctrl Pts',(5.15940188569591,4.95288622035444,5.13635619600154));
#160282=CARTESIAN_POINT('Ctrl Pts',(5.16281064658125,4.9536697922829,5.13980662441589));
#160283=CARTESIAN_POINT('Ctrl Pts',(5.1662191348642,4.95445104514204,5.14325784965854));
#160284=CARTESIAN_POINT('Ctrl Pts',(5.1696273514169,4.95523000038884,5.14670986113548));
#160285=CARTESIAN_POINT('Ctrl Pts',(4.969103039,5.000313899,5.340937689));
#160286=CARTESIAN_POINT('Ctrl Pts',(5.050820094,4.98224132,5.264909753));
#160287=CARTESIAN_POINT('Ctrl Pts',(5.130172969,4.964285714,5.186417426));
#160288=CARTESIAN_POINT('Ctrl Pts',(5.16685149900001,4.955986264,5.150136659));
#160289=CARTESIAN_POINT('Ctrl Pts',(5.203013228,4.947660853,5.113340763));
#160290=CARTESIAN_POINT('Ctrl Pts',(4.905659624,5.000313899,5.338258485));
#160291=CARTESIAN_POINT('Ctrl Pts',(4.987335687,4.98224132,5.263201242));
#160292=CARTESIAN_POINT('Ctrl Pts',(5.066677286,4.964285714,5.185680407));
#160293=CARTESIAN_POINT('Ctrl Pts',(5.103350603,4.955986264,5.149848684));
#160294=CARTESIAN_POINT('Ctrl Pts',(5.139513471,4.947660853,5.113501861));
#160295=CARTESIAN_POINT('Ctrl Pts',(5.1381573905858,4.9479730331745,5.11486462602031));
#160296=CARTESIAN_POINT('Ctrl Pts',(5.11447664210774,4.95342302529756,5.13865310318677));
#160297=CARTESIAN_POINT('Ctrl Pts',(5.09064856021101,4.95886083272451,5.16225923533607));
#160298=CARTESIAN_POINT('Ctrl Pts',(5.06667728621878,4.96428571397019,5.1856804068723));
#160299=CARTESIAN_POINT('Ctrl Pts',(5.01433181580533,4.97613189117016,5.23682463158556));
#160300=CARTESIAN_POINT('Ctrl Pts',(4.96112242201154,4.98803923912007,5.28726340536358));
#160301=CARTESIAN_POINT('Ctrl Pts',(4.90707810144186,5.00000000032828,5.3369546096604));
#160302=CARTESIAN_POINT('Ctrl Pts',(4.905659624,5.000313899,5.338258485));
#160303=CARTESIAN_POINT('Ctrl Pts',(4.987335687,4.98224132,5.263201242));
#160304=CARTESIAN_POINT('Ctrl Pts',(5.066677286,4.964285714,5.185680407));
#160305=CARTESIAN_POINT('Ctrl Pts',(5.102662666,4.95614194999999,5.150520834));
#160306=CARTESIAN_POINT('Ctrl Pts',(5.138156632,4.947973174,5.11486524));
#160307=CARTESIAN_POINT('Ctrl Pts',(4.902547666,5.000313899,5.41194948));
#160308=CARTESIAN_POINT('Ctrl Pts',(4.985351212,4.98224132,5.33693985));
#160309=CARTESIAN_POINT('Ctrl Pts',(5.065821221,4.964285714,5.259432113));
#160310=CARTESIAN_POINT('Ctrl Pts',(5.102318391,4.95614194999999,5.224278481));
#160311=CARTESIAN_POINT('Ctrl Pts',(5.138324182,4.947973174,5.188621724));
#160312=CARTESIAN_POINT('',(5.13840595762541,4.94797317334228,5.22462127032716));
#160313=CARTESIAN_POINT('Ctrl Pts',(4.527175975,4.818630405,5.862255283));
#160314=CARTESIAN_POINT('Ctrl Pts',(4.534162896,4.820029867,5.856859574));
#160315=CARTESIAN_POINT('Ctrl Pts',(4.541136935,4.821428571,5.851447226));
#160316=CARTESIAN_POINT('Ctrl Pts',(4.853706394,4.884117105,5.608871218));
#160317=CARTESIAN_POINT('Ctrl Pts',(5.138655289,4.947973174,5.334377295));
#160318=CARTESIAN_POINT('Ctrl Pts',(4.550585316,4.818630405,5.643994444));
#160319=CARTESIAN_POINT('Ctrl Pts',(4.557312103,4.820029867,5.638570835));
#160320=CARTESIAN_POINT('Ctrl Pts',(4.564025943,4.821428571,5.633131207));
#160321=CARTESIAN_POINT('Ctrl Pts',(4.864933514,4.884117105,5.389332525));
#160322=CARTESIAN_POINT('Ctrl Pts',(5.138156632,4.947973174,5.11486524));
#160323=CARTESIAN_POINT('Ctrl Pts',(4.55424020907722,4.81939091801857,5.64104568384217));
#160324=CARTESIAN_POINT('Ctrl Pts',(4.56573507336455,4.82234724734205,5.65499942765427));
#160325=CARTESIAN_POINT('Ctrl Pts',(4.57723334628362,4.82527010319568,5.66895751963913));
#160326=CARTESIAN_POINT('Ctrl Pts',(4.5887221569022,4.82816321758488,5.68292951270901));
#160327=CARTESIAN_POINT('Ctrl Pts',(4.59947743918297,4.83087161473403,5.69600943320562));
#160328=CARTESIAN_POINT('Ctrl Pts',(4.61022770116185,4.83355328560802,5.7090990456699));
#160329=CARTESIAN_POINT('Ctrl Pts',(4.62097308340232,4.83620904394719,5.72219788303831));
#160330=CARTESIAN_POINT('Ctrl Pts',(4.63171858101127,4.83886483080008,5.73529686104324));
#160331=CARTESIAN_POINT('Ctrl Pts',(4.64245922725937,4.84149471147249,5.74840509909905));
#160332=CARTESIAN_POINT('Ctrl Pts',(4.65319515431945,4.84409946436975,5.76152215993885));
#160333=CARTESIAN_POINT('Ctrl Pts',(4.12631332540522,4.94924836941368,6.15101308899583));
#160334=CARTESIAN_POINT('Ctrl Pts',(4.12964253020261,4.94861077170684,6.14877450949792));
#160335=CARTESIAN_POINT('Ctrl Pts',(4.132971735,4.94797317400001,6.14653593));
#160336=CARTESIAN_POINT('Ctrl Pts',(4.467808307,4.88384644,5.921389587));
#160337=CARTESIAN_POINT('Ctrl Pts',(4.77620603,4.818610636,5.661202634));
#160338=CARTESIAN_POINT('Ctrl Pts',(3.91187673525438,4.94924836941368,6.10407913568029));
#160339=CARTESIAN_POINT('Ctrl Pts',(3.91518064462719,4.94861077170684,6.10195673084015));
#160340=CARTESIAN_POINT('Ctrl Pts',(3.918484554,4.94797317400001,6.099834326));
#160341=CARTESIAN_POINT('Ctrl Pts',(4.250777025,4.88384644,5.886372312));
#160342=CARTESIAN_POINT('Ctrl Pts',(4.557914959,4.818610636,5.638076909));
#160343=CARTESIAN_POINT('',(3.95451860864093,4.94797317334255,6.10768024367488));
#160344=CARTESIAN_POINT('Ctrl Pts',(3.91582284472911,4.94745154526473,6.1015441866602));
#160345=CARTESIAN_POINT('Ctrl Pts',(3.91715369936455,4.94771235963237,6.1006892563301));
#160346=CARTESIAN_POINT('Ctrl Pts',(3.918484554,4.947973174,6.099834326));
#160347=CARTESIAN_POINT('Ctrl Pts',(4.051741265,4.974088171,6.014231285));
#160348=CARTESIAN_POINT('Ctrl Pts',(4.181132469,5.00031307,5.922890449));
#160349=CARTESIAN_POINT('Ctrl Pts',(3.98788411345982,4.94745154526474,6.11726746511525));
#160350=CARTESIAN_POINT('Ctrl Pts',(3.98921839172991,4.94771235963237,6.11639681105762));
#160351=CARTESIAN_POINT('Ctrl Pts',(3.99055267,4.947973174,6.115526157));
#160352=CARTESIAN_POINT('Ctrl Pts',(4.124152185,4.974088171,6.02834872));
#160353=CARTESIAN_POINT('Ctrl Pts',(4.253817109,5.00031307,5.935420018));
#160354=CARTESIAN_POINT('Origin',(-0.125384865003265,5.08925684212034,-0.152065231848668));
#160355=CARTESIAN_POINT('Ctrl Pts',(3.903371084,4.94766207,6.162896608));
#160356=CARTESIAN_POINT('Ctrl Pts',(4.038807786,4.973931887,6.077115563));
#160357=CARTESIAN_POINT('Ctrl Pts',(4.170345281,5.00031307,5.985467455));
#160358=CARTESIAN_POINT('Ctrl Pts',(3.916896932,4.94766207,6.100853909));
#160359=CARTESIAN_POINT('Ctrl Pts',(4.050970176,4.973931887,6.014775618));
#160360=CARTESIAN_POINT('Ctrl Pts',(4.181132469,5.00031307,5.922890449));
#160361=CARTESIAN_POINT('Ctrl Pts',(3.91848626136233,4.94797287209023,6.0998333531052));
#160362=CARTESIAN_POINT('Ctrl Pts',(3.92127353100262,4.94882769745733,6.10425021460731));
#160363=CARTESIAN_POINT('Ctrl Pts',(3.92406197047932,4.94967947057366,6.10866692966534));
#160364=CARTESIAN_POINT('Ctrl Pts',(3.92684989716656,4.95052852744272,6.11308448915988));
#160365=CARTESIAN_POINT('Ctrl Pts',(3.92943809980516,4.95131675879719,6.11718557947632));
#160366=CARTESIAN_POINT('Ctrl Pts',(3.93202586122446,4.95210264918639,6.12128739892803));
#160367=CARTESIAN_POINT('Ctrl Pts',(3.93461318446858,4.95288622031634,6.12538993694027));
#160368=CARTESIAN_POINT('Ctrl Pts',(3.93720051032669,4.95366979223794,6.12949247909733));
#160369=CARTESIAN_POINT('Ctrl Pts',(3.9397873986607,4.95445104509302,6.1335957408516));
#160370=CARTESIAN_POINT('Ctrl Pts',(3.94237385257086,4.95523000032935,6.13769971199802));
#160371=CARTESIAN_POINT('Ctrl Pts',(3.704784445,5.000313899,6.284279802));
#160372=CARTESIAN_POINT('Ctrl Pts',(3.80093476,4.98224132,6.227596108));
#160373=CARTESIAN_POINT('Ctrl Pts',(3.895305939,4.964285714,6.16799741));
#160374=CARTESIAN_POINT('Ctrl Pts',(3.938926237,4.955986264,6.140449667));
#160375=CARTESIAN_POINT('Ctrl Pts',(3.982152555,4.947660853,6.112287742));
#160376=CARTESIAN_POINT('Ctrl Pts',(3.643400252,5.000313899,6.268024777));
#160377=CARTESIAN_POINT('Ctrl Pts',(3.739301863,4.98224132,6.21228027));
#160378=CARTESIAN_POINT('Ctrl Pts',(3.833453187,4.964285714,6.153627927));
#160379=CARTESIAN_POINT('Ctrl Pts',(3.876971864,4.955986264,6.126517609));
#160380=CARTESIAN_POINT('Ctrl Pts',(3.920102756,4.947660853,6.098794502));
#160381=CARTESIAN_POINT('Ctrl Pts',(3.9184854264898,4.94797303320567,6.09983388941806));
#160382=CARTESIAN_POINT('Ctrl Pts',(3.890244500683,4.95342302541711,6.1179755445405));
#160383=CARTESIAN_POINT('Ctrl Pts',(3.86189888534793,4.95886083283601,6.13590744510505));
#160384=CARTESIAN_POINT('Ctrl Pts',(3.83345318681619,4.96428571407458,6.15362792729177));
#160385=CARTESIAN_POINT('Ctrl Pts',(3.77133702917533,4.9761318912024,6.19232369985351));
#160386=CARTESIAN_POINT('Ctrl Pts',(3.70852879586539,4.98803923906917,6.23014479602785));
#160387=CARTESIAN_POINT('Ctrl Pts',(3.64506586129705,5.00000000025158,6.26705631602723));
#160388=CARTESIAN_POINT('Ctrl Pts',(3.643400252,5.000313899,6.268024777));
#160389=CARTESIAN_POINT('Ctrl Pts',(3.739301863,4.98224132,6.21228027));
#160390=CARTESIAN_POINT('Ctrl Pts',(3.833453187,4.964285714,6.153627927));
#160391=CARTESIAN_POINT('Ctrl Pts',(3.876155517,4.95614194999999,6.127026159));
#160392=CARTESIAN_POINT('Ctrl Pts',(3.918484554,4.947973174,6.099834326));
#160393=CARTESIAN_POINT('Ctrl Pts',(3.624519664,5.000313899,6.339323939));
#160394=CARTESIAN_POINT('Ctrl Pts',(3.721512162,4.98224132,6.283868307));
#160395=CARTESIAN_POINT('Ctrl Pts',(3.816762699,4.964285714,6.225471331));
#160396=CARTESIAN_POINT('Ctrl Pts',(3.859963578,4.95614194999999,6.198985384));
#160397=CARTESIAN_POINT('Ctrl Pts',(3.902792722,4.947973174,6.171902443));
#160398=CARTESIAN_POINT('',(3.89513374808462,4.94797317334224,6.20707791914326));
#160399=CARTESIAN_POINT('Ctrl Pts',(3.161121518,4.818630405,6.698408024));
#160400=CARTESIAN_POINT('Ctrl Pts',(3.169105006,4.820029867,6.694640446));
#160401=CARTESIAN_POINT('Ctrl Pts',(3.177079491,4.821428571,6.690853848));
#160402=CARTESIAN_POINT('Ctrl Pts',(3.534487921,4.884117105,6.521142326));
#160403=CARTESIAN_POINT('Ctrl Pts',(3.871782949,4.947973174,6.314321508));
#160404=CARTESIAN_POINT('Ctrl Pts',(3.23090319,4.818630405,6.490282319));
#160405=CARTESIAN_POINT('Ctrl Pts',(3.238638624,4.820029867,6.486431571));
#160406=CARTESIAN_POINT('Ctrl Pts',(3.246364857,4.821428571,6.482562396));
#160407=CARTESIAN_POINT('Ctrl Pts',(3.592646886,4.884117105,6.309149825));
#160408=CARTESIAN_POINT('Ctrl Pts',(3.918484554,4.947973174,6.099834326));
#160409=CARTESIAN_POINT('Ctrl Pts',(3.2351065298675,4.8193909179172,6.4881881934962));
#160410=CARTESIAN_POINT('Ctrl Pts',(3.24333300793021,4.82234724737653,6.50428676221164));
#160411=CARTESIAN_POINT('Ctrl Pts',(3.25156188047758,4.8252701031888,6.52039031048622));
#160412=CARTESIAN_POINT('Ctrl Pts',(3.25977852354582,4.82816321755467,6.53650540076862));
#160413=CARTESIAN_POINT('Ctrl Pts',(3.26747055705677,4.83087161470281,6.55159158784706));
#160414=CARTESIAN_POINT('Ctrl Pts',(3.27515560415933,4.83355328557703,6.56668616107939));
#160415=CARTESIAN_POINT('Ctrl Pts',(3.28283390253395,4.83620904391764,6.58178869453964));
#160416=CARTESIAN_POINT('Ctrl Pts',(3.2905122833471,4.83886483077196,6.59689139014914));
#160417=CARTESIAN_POINT('Ctrl Pts',(3.2981839355909,4.84149471144699,6.61200208641192));
#160418=CARTESIAN_POINT('Ctrl Pts',(3.30584908222536,4.84409946430701,6.62712038446017));
#160419=CARTESIAN_POINT('Ctrl Pts',(2.70755642147094,4.94924836941368,6.89424121325815));
#160420=CARTESIAN_POINT('Ctrl Pts',(2.71128901973547,4.94861077170684,6.89277065112908));
#160421=CARTESIAN_POINT('Ctrl Pts',(2.715021618,4.94797317400001,6.891300089));
#160422=CARTESIAN_POINT('Ctrl Pts',(3.090429706,4.88384644,6.743397508));
#160423=CARTESIAN_POINT('Ctrl Pts',(3.447549765,4.818610636,6.555589976));
#160424=CARTESIAN_POINT('Ctrl Pts',(2.50822265177515,4.94924836941368,6.80230702168493));
#160425=CARTESIAN_POINT('Ctrl Pts',(2.51190557188757,4.94861077170684,6.80094448034247));
#160426=CARTESIAN_POINT('Ctrl Pts',(2.515588492,4.94797317400001,6.799581939));
#160427=CARTESIAN_POINT('Ctrl Pts',(2.886000173,4.88384644,6.662543607));
#160428=CARTESIAN_POINT('Ctrl Pts',(3.239333565,4.818610636,6.486078789));
#160429=CARTESIAN_POINT('',(2.54909345025193,4.94797317334255,6.81499067990194));
#160430=CARTESIAN_POINT('Ctrl Pts',(2.51262144250503,4.94745154526473,6.80067963526152));
#160431=CARTESIAN_POINT('Ctrl Pts',(2.51410496725252,4.94771235963237,6.80013078713076));
#160432=CARTESIAN_POINT('Ctrl Pts',(2.515588492,4.947973174,6.799581939));
#160433=CARTESIAN_POINT('Ctrl Pts',(2.664131859,4.974088171,6.744626503));
#160434=CARTESIAN_POINT('Ctrl Pts',(2.810133548,5.00031307,6.68323645));
#160435=CARTESIAN_POINT('Ctrl Pts',(2.57961791904852,4.94745154526473,6.83152635453666));
#160436=CARTESIAN_POINT('Ctrl Pts',(2.58110816752426,4.94771235963237,6.83096288626833));
#160437=CARTESIAN_POINT('Ctrl Pts',(2.582598416,4.947973174,6.830399418));
#160438=CARTESIAN_POINT('Ctrl Pts',(2.731815021,4.974088171,6.773980087));
#160439=CARTESIAN_POINT('Ctrl Pts',(2.878425375,5.00031307,6.711098133));
#160440=CARTESIAN_POINT('Origin',(-0.089764152265116,5.08925712536846,-0.175464601845655));
#160441=CARTESIAN_POINT('Ctrl Pts',(2.48727184,4.94766207,6.85792091));
#160442=CARTESIAN_POINT('Ctrl Pts',(2.637982497,4.97393188700001,6.803260266));
#160443=CARTESIAN_POINT('Ctrl Pts',(2.786146352,5.00031307,6.742031513));
#160444=CARTESIAN_POINT('Ctrl Pts',(2.513818808,4.94766207,6.800236393));
#160445=CARTESIAN_POINT('Ctrl Pts',(2.663261782,4.97393188700001,6.744992349));
#160446=CARTESIAN_POINT('Ctrl Pts',(2.810133548,5.00031307,6.68323645));
#160447=CARTESIAN_POINT('Ctrl Pts',(2.51559036884464,4.94797287220619,6.79958135590101));
#160448=CARTESIAN_POINT('Ctrl Pts',(2.51736297941983,4.94882769749915,6.80449413410756));
#160449=CARTESIAN_POINT('Ctrl Pts',(2.51913676346908,4.94967947062019,6.80940702092935));
#160450=CARTESIAN_POINT('Ctrl Pts',(2.52090986519437,4.95052852749235,6.81432062220744));
#160451=CARTESIAN_POINT('Ctrl Pts',(2.52255594381641,4.9513167588421,6.81888221836729));
#160452=CARTESIAN_POINT('Ctrl Pts',(2.5242014347969,4.95210264922525,6.82344443176355));
#160453=CARTESIAN_POINT('Ctrl Pts',(2.52584634338302,4.95288622034841,6.82800725272412));
#160454=CARTESIAN_POINT('Ctrl Pts',(2.527491253631,4.95366979226322,6.83257007829454));
#160455=CARTESIAN_POINT('Ctrl Pts',(2.52913558189762,4.95445104511072,6.83713351258166));
#160456=CARTESIAN_POINT('Ctrl Pts',(2.53077933337913,4.95523000032694,6.84169754621404));
#160457=CARTESIAN_POINT('Ctrl Pts',(2.267234248,5.000313899,6.933775975));
#160458=CARTESIAN_POINT('Ctrl Pts',(2.373321941,4.98224132,6.89908699));
#160459=CARTESIAN_POINT('Ctrl Pts',(2.478298732,4.964285714,6.861168691));
#160460=CARTESIAN_POINT('Ctrl Pts',(2.526821163,4.955986264,6.843642074));
#160461=CARTESIAN_POINT('Ctrl Pts',(2.575090855,4.947660853,6.825430939));
#160462=CARTESIAN_POINT('Ctrl Pts',(2.210779533,5.000313899,6.904705197));
#160463=CARTESIAN_POINT('Ctrl Pts',(2.316422439,4.98224132,6.870879977));
#160464=CARTESIAN_POINT('Ctrl Pts',(2.420981077,4.964285714,6.833838645));
#160465=CARTESIAN_POINT('Ctrl Pts',(2.469310228,4.955986264,6.81671738));
#160466=CARTESIAN_POINT('Ctrl Pts',(2.517392394,4.947660853,6.798914291));
#160467=CARTESIAN_POINT('Ctrl Pts',(2.51558943810921,4.94797303333726,6.79958170023568));
#160468=CARTESIAN_POINT('Ctrl Pts',(2.48410885035045,4.95342302538865,6.81122824905784));
#160469=CARTESIAN_POINT('Ctrl Pts',(2.4525711111243,4.95886083276052,6.82264744228887));
#160470=CARTESIAN_POINT('Ctrl Pts',(2.42098107736794,4.96428571399539,6.83383864515312));
#160471=CARTESIAN_POINT('Ctrl Pts',(2.35199871314928,4.97613189113004,6.85827659379836));
#160472=CARTESIAN_POINT('Ctrl Pts',(2.28252848394537,4.9880392390776,6.88171154060857));
#160473=CARTESIAN_POINT('Ctrl Pts',(2.21261439168749,5.00000000026428,6.90411743489196));
#160474=CARTESIAN_POINT('Ctrl Pts',(2.210779533,5.000313899,6.904705197));
#160475=CARTESIAN_POINT('Ctrl Pts',(2.316422439,4.98224132,6.870879977));
#160476=CARTESIAN_POINT('Ctrl Pts',(2.420981077,4.964285714,6.833838645));
#160477=CARTESIAN_POINT('Ctrl Pts',(2.468403645,4.95614194999999,6.81703855));
#160478=CARTESIAN_POINT('Ctrl Pts',(2.515588492,4.947973174,6.799581939));
#160479=CARTESIAN_POINT('Ctrl Pts',(2.177013151,5.000313899,6.970278656));
#160480=CARTESIAN_POINT('Ctrl Pts',(2.283659339,4.98224132,6.936970065));
#160481=CARTESIAN_POINT('Ctrl Pts',(2.389236596,4.964285714,6.900414428));
#160482=CARTESIAN_POINT('Ctrl Pts',(2.437121158,4.95614194999999,6.88383462));
#160483=CARTESIAN_POINT('Ctrl Pts',(2.484771012,4.947973174,6.866591863));
#160484=CARTESIAN_POINT('',(2.4697294127037,4.94797317334223,6.89929850335895));
#160485=CARTESIAN_POINT('Ctrl Pts',(1.647256531,4.818630405,7.221350651));
#160486=CARTESIAN_POINT('Ctrl Pts',(1.655863289,4.820029867,7.219387371));
#160487=CARTESIAN_POINT('Ctrl Pts',(1.664465341,4.821428571,7.21740358));
#160488=CARTESIAN_POINT('Ctrl Pts',(2.050000721,4.884117105,7.128492066));
#160489=CARTESIAN_POINT('Ctrl Pts',(2.423870341,4.947973174,6.999015065));
#160490=CARTESIAN_POINT('Ctrl Pts',(1.760147622,4.818630405,7.033091806));
#160491=CARTESIAN_POINT('Ctrl Pts',(1.768530003,4.820029867,7.030993976));
#160492=CARTESIAN_POINT('Ctrl Pts',(1.776907359,4.821428571,7.028876172));
#160493=CARTESIAN_POINT('Ctrl Pts',(2.152372083,4.884117105,6.933958291));
#160494=CARTESIAN_POINT('Ctrl Pts',(2.515588492,4.947973174,6.799581939));
#160495=CARTESIAN_POINT('Ctrl Pts',(1.76470286479964,4.81939091791719,7.03195023316287));
#160496=CARTESIAN_POINT('Ctrl Pts',(1.76927629608275,4.82234724726155,7.04944087630683));
#160497=CARTESIAN_POINT('Ctrl Pts',(1.77385099516533,4.82527010308462,7.06693689689648));
#160498=CARTESIAN_POINT('Ctrl Pts',(1.77841126959503,4.82816321744559,7.08444156064864));
#160499=CARTESIAN_POINT('Ctrl Pts',(1.78268038335581,4.83087161460903,7.10082860095823));
#160500=CARTESIAN_POINT('Ctrl Pts',(1.78694087127104,4.8335532854988,7.11722232948686));
#160501=CARTESIAN_POINT('Ctrl Pts',(1.79119305702643,4.83620904385498,7.13362238136058));
#160502=CARTESIAN_POINT('Ctrl Pts',(1.79544528843569,4.83886483072488,7.15002260931446));
#160503=CARTESIAN_POINT('Ctrl Pts',(1.79968922868213,4.84149471141551,7.16642920442718));
#160504=CARTESIAN_POINT('Ctrl Pts',(1.80392518127354,4.84409946430028,7.18284182514446));
#160505=CARTESIAN_POINT('Ctrl Pts',(1.16219718885009,4.94924836941368,7.31510228082506));
#160506=CARTESIAN_POINT('Ctrl Pts',(1.16615864842505,4.94861077170684,7.31446849791253));
#160507=CARTESIAN_POINT('Ctrl Pts',(1.170120108,4.94797317400001,7.31383471500001));
#160508=CARTESIAN_POINT('Ctrl Pts',(1.568546046,4.88384644,7.250091656));
#160509=CARTESIAN_POINT('Ctrl Pts',(1.957689904,4.818610636,7.143445216));
#160510=CARTESIAN_POINT('Ctrl Pts',(0.987286864787931,4.94924836941368,
7.18246659083401));
#160511=CARTESIAN_POINT('Ctrl Pts',(0.991176586393966,4.94861077170684,
7.18192762391701));
#160512=CARTESIAN_POINT('Ctrl Pts',(0.995066308,4.94797317400001,7.181388657));
#160513=CARTESIAN_POINT('Ctrl Pts',(1.386277161,4.88384644,7.127181768));
#160514=CARTESIAN_POINT('Ctrl Pts',(1.769284534,4.818610636,7.030798834));
#160515=CARTESIAN_POINT('',(1.02447551553818,4.94797317334255,7.20363972606343));
#160516=CARTESIAN_POINT('Ctrl Pts',(0.991932654222761,4.94745154526474,
7.18182286178785));
#160517=CARTESIAN_POINT('Ctrl Pts',(0.99349948111138,4.94771235963237,7.18160575939393));
#160518=CARTESIAN_POINT('Ctrl Pts',(0.995066308,4.947973174,7.181388657));
#160519=CARTESIAN_POINT('Ctrl Pts',(1.151950608,4.974088171,7.159650482));
#160520=CARTESIAN_POINT('Ctrl Pts',(1.307735906,5.00031307,7.131081741));
#160521=CARTESIAN_POINT('Ctrl Pts',(1.05073165838991,4.94745154526473,7.22635066464237));
#160522=CARTESIAN_POINT('Ctrl Pts',(1.05230819469495,4.94771235963237,7.22612072932119));
#160523=CARTESIAN_POINT('Ctrl Pts',(1.053884731,4.947973174,7.225890794));
#160524=CARTESIAN_POINT('Ctrl Pts',(1.211741222,4.974088171,7.202867675));
#160525=CARTESIAN_POINT('Ctrl Pts',(1.368441669,5.00031307,7.172972758));
#160526=CARTESIAN_POINT('Origin',(-0.0499455387825083,5.08925704570198,
-0.190657335926088));
#160527=CARTESIAN_POINT('Ctrl Pts',(0.95487053,4.94766207,7.23227645200001));
#160528=CARTESIAN_POINT('Ctrl Pts',(1.113808078,4.97393188700001,7.21129208));
#160529=CARTESIAN_POINT('Ctrl Pts',(1.271670316,5.00031307,7.18334567));
#160530=CARTESIAN_POINT('Ctrl Pts',(0.993197311,4.94766207,7.18164738100001));
#160531=CARTESIAN_POINT('Ctrl Pts',(1.151022227,4.97393188700001,7.159820734));
#160532=CARTESIAN_POINT('Ctrl Pts',(1.307735906,5.00031307,7.131081741));
#160533=CARTESIAN_POINT('Ctrl Pts',(0.995068266814636,4.94797287211291,
7.18138849127666));
#160534=CARTESIAN_POINT('Ctrl Pts',(0.995743332761482,4.94882769742648,
7.18656747044334));
#160535=CARTESIAN_POINT('Ctrl Pts',(0.99641952126286,4.94967947057192,7.19174680788969));
#160536=CARTESIAN_POINT('Ctrl Pts',(0.997094889799226,4.95052852746446,
7.19692669639858));
#160537=CARTESIAN_POINT('Ctrl Pts',(0.997721875648572,4.95131675882001,
7.20173550317798));
#160538=CARTESIAN_POINT('Ctrl Pts',(0.998348154901802,4.9521026492053,7.20654478642679));
#160539=CARTESIAN_POINT('Ctrl Pts',(0.998973734766601,4.95288622032942,
7.21135453783823));
#160540=CARTESIAN_POINT('Ctrl Pts',(0.999599315263429,4.95366979224519,
7.21616429410901));
#160541=CARTESIAN_POINT('Ctrl Pts',(1.00022419652744,4.95445104509255,7.22097451975665));
#160542=CARTESIAN_POINT('Ctrl Pts',(1.00084838567572,4.95523000033943,7.22578520694037));
#160543=CARTESIAN_POINT('Ctrl Pts',(0.723670697,5.000313899,7.259056491));
#160544=CARTESIAN_POINT('Ctrl Pts',(0.834735225,4.98224132,7.247984233));
#160545=CARTESIAN_POINT('Ctrl Pts',(0.945409031,4.964285714,7.233519349));
#160546=CARTESIAN_POINT('Ctrl Pts',(0.996564739,4.955986264,7.226833383));
#160547=CARTESIAN_POINT('Ctrl Pts',(1.047620768,4.947660853,7.219424571));
#160548=CARTESIAN_POINT('Ctrl Pts',(0.67478522,5.000313899,7.218529276));
#160549=CARTESIAN_POINT('Ctrl Pts',(0.785229676,4.98224132,7.208204972));
#160550=CARTESIAN_POINT('Ctrl Pts',(0.895306583,4.964285714,7.194506663));
#160551=CARTESIAN_POINT('Ctrl Pts',(0.946186392000001,4.955986264,7.188175023));
#160552=CARTESIAN_POINT('Ctrl Pts',(0.99697156,4.947660853,7.181124404));
#160553=CARTESIAN_POINT('Ctrl Pts',(0.99506728359157,4.94797303328102,7.18138862751167));
#160554=CARTESIAN_POINT('Ctrl Pts',(0.961819030399578,4.95342302542127,
7.18599549061261));
#160555=CARTESIAN_POINT('Ctrl Pts',(0.928563837219034,4.95886083281524,
7.19036802794514));
#160556=CARTESIAN_POINT('Ctrl Pts',(0.895306583038016,4.96428571399449,
7.19450666299911));
#160557=CARTESIAN_POINT('Ctrl Pts',(0.822683552230544,4.97613189103025,
7.20354409641358));
#160558=CARTESIAN_POINT('Ctrl Pts',(0.749799676836577,4.98803923906901,
7.21149710151008));
#160559=CARTESIAN_POINT('Ctrl Pts',(0.676703532269287,5.00000000025134,
7.21834969580106));
#160560=CARTESIAN_POINT('Ctrl Pts',(0.67478522,5.000313899,7.218529276));
#160561=CARTESIAN_POINT('Ctrl Pts',(0.785229676,4.98224132,7.208204972));
#160562=CARTESIAN_POINT('Ctrl Pts',(0.895306583,4.964285714,7.194506663));
#160563=CARTESIAN_POINT('Ctrl Pts',(0.945231961,4.95614194999999,7.188293795));
#160564=CARTESIAN_POINT('Ctrl Pts',(0.995066308,4.947973174,7.181388657));
#160565=CARTESIAN_POINT('Ctrl Pts',(0.627711922,5.000313899,7.275310889));
#160566=CARTESIAN_POINT('Ctrl Pts',(0.739025144,4.98224132,7.265706814));
#160567=CARTESIAN_POINT('Ctrl Pts',(0.849992445,4.964285714,7.252701816));
#160568=CARTESIAN_POINT('Ctrl Pts',(0.900321661,4.95614194999999,7.2468034));
#160569=CARTESIAN_POINT('Ctrl Pts',(0.950564171,4.947973174,7.240207079));
#160570=CARTESIAN_POINT('',(0.928843275000543,4.94797317334227,7.26891555701107));
#160571=CARTESIAN_POINT('Ctrl Pts',(0.056367661,4.818630405,7.406630948));
#160572=CARTESIAN_POINT('Ctrl Pts',(0.065195244,4.820029867,7.406563766));
#160573=CARTESIAN_POINT('Ctrl Pts',(0.074022642,4.821428571,7.406475542));
#160574=CARTESIAN_POINT('Ctrl Pts',(0.469657766,4.884117105,7.402521441));
#160575=CARTESIAN_POINT('Ctrl Pts',(0.86262025,4.947973174,7.35644245600001));
#160576=CARTESIAN_POINT('Ctrl Pts',(0.207089507,4.818630405,7.24704173700001));
#160577=CARTESIAN_POINT('Ctrl Pts',(0.215726884,4.820029867,7.246794918));
#160578=CARTESIAN_POINT('Ctrl Pts',(0.224363648,4.821428571,7.24652751));
#160579=CARTESIAN_POINT('Ctrl Pts',(0.611454754,4.884117105,7.234542573));
#160580=CARTESIAN_POINT('Ctrl Pts',(0.995066308,4.947973174,7.181388657));
#160581=CARTESIAN_POINT('Ctrl Pts',(0.211783655067681,4.81939091801857,
7.24690609670381));
#160582=CARTESIAN_POINT('Ctrl Pts',(0.212490191699886,4.8223472472686,7.26497097077347));
#160583=CARTESIAN_POINT('Ctrl Pts',(0.21319680923074,4.82527010317956,7.2830413693019));
#160584=CARTESIAN_POINT('Ctrl Pts',(0.213887481742358,4.82816321755752,
7.30111710804181));
#160585=CARTESIAN_POINT('Ctrl Pts',(0.214534056753162,4.83087161470481,
7.31803876161052));
#160586=CARTESIAN_POINT('Ctrl Pts',(0.215170769813655,4.8335532855769,7.33496509272996));
#160587=CARTESIAN_POINT('Ctrl Pts',(0.215798015478006,4.8362090439141,7.35189581463962));
#160588=CARTESIAN_POINT('Ctrl Pts',(0.216425267876818,4.83886483076503,
7.36882671832704));
#160589=CARTESIAN_POINT('Ctrl Pts',(0.217043054200761,4.84149471143539,
7.38576205795811));
#160590=CARTESIAN_POINT('Ctrl Pts',(0.21765174428364,4.84409946429302,7.40270156517168));
#160591=CARTESIAN_POINT('Ctrl Pts',(-0.437505093897724,4.94924836941368,
7.39391729643459));
#160592=CARTESIAN_POINT('Ctrl Pts',(-0.433500006448862,4.94861077170685,
7.39414992771729));
#160593=CARTESIAN_POINT('Ctrl Pts',(-0.429494919,4.947973174,7.39438255900001));
#160594=CARTESIAN_POINT('Ctrl Pts',(-0.026681084,4.88384644,7.417779576));
#160595=CARTESIAN_POINT('Ctrl Pts',(0.37629064,4.818610636,7.397280897));
#160596=CARTESIAN_POINT('Ctrl Pts',(-0.5798133580548,4.94924836941368,7.22678200501259));
#160597=CARTESIAN_POINT('Ctrl Pts',(-0.5758987140274,4.94861077170685,7.2270918140063));
#160598=CARTESIAN_POINT('Ctrl Pts',(-0.57198407,4.947973174,7.227401623));
#160599=CARTESIAN_POINT('Ctrl Pts',(-0.178266631,4.88384644,7.25856083000001));
#160600=CARTESIAN_POINT('Ctrl Pts',(0.216505724,4.818610636,7.246766539));
#160601=CARTESIAN_POINT('Ctrl Pts',(0.459542598,0.940053947,7.48590813500001));
#160602=CARTESIAN_POINT('Ctrl Pts',(0.867851637,0.874398499000001,7.460842987));
#160603=CARTESIAN_POINT('Ctrl Pts',(1.271012251,0.809170361000001,7.391517291));
#160604=CARTESIAN_POINT('Ctrl Pts',(0.206665513,0.940053947,7.24705384));
#160605=CARTESIAN_POINT('Ctrl Pts',(0.601946558,0.874398499000001,7.235781541));
#160606=CARTESIAN_POINT('Ctrl Pts',(0.993656627,0.809170361000001,7.18158384400001));
#160607=CARTESIAN_POINT('',(0.988998381141225,0.809946052584885,7.18222682884825));
#160608=CARTESIAN_POINT('Origin',(-0.00457861362387568,0.946423635872504,
-0.198602844994274));
#160609=CARTESIAN_POINT('Ctrl Pts',(1.02255389472722,0.849330499449965,
7.42996524443304));
#160610=CARTESIAN_POINT('Ctrl Pts',(1.01691672373786,0.843074444461056,
7.38864113427304));
#160611=CARTESIAN_POINT('Ctrl Pts',(1.01129781035107,0.836669224966113,
7.34731392216213));
#160612=CARTESIAN_POINT('Ctrl Pts',(1.00011311603077,0.82355155051849,7.2647479618169));
#160613=CARTESIAN_POINT('Ctrl Pts',(0.994541071872439,0.816831759747733,
7.22346300196618));
#160614=CARTESIAN_POINT('Ctrl Pts',(0.988998378925275,0.809946053603692,
7.18222682897598));
#160615=CARTESIAN_POINT('Ctrl Pts',(0.773595447487787,0.809162772000001,
7.46052528797153));
#160616=CARTESIAN_POINT('Ctrl Pts',(1.18052789164326,0.874819703,7.41832972190814));
#160617=CARTESIAN_POINT('Ctrl Pts',(1.58045672673546,0.940053947,7.33212411374811));
#160618=CARTESIAN_POINT('Ctrl Pts',(1.59428862386671,0.942310131784066,
7.3291426155425));
#160619=CARTESIAN_POINT('Ctrl Pts',(1.60812052099803,0.944566316568131,
7.32616111733674));
#160620=CARTESIAN_POINT('Ctrl Pts',(0.984324587,0.809162772000001,7.182868863));
#160621=CARTESIAN_POINT('Ctrl Pts',(1.376112332,0.874819703,7.12917913000001));
#160622=CARTESIAN_POINT('Ctrl Pts',(1.759736143,0.940053947,7.03319477300001));
#160623=CARTESIAN_POINT('Ctrl Pts',(1.77300411626237,0.942310131784066,
7.02987506800317));
#160624=CARTESIAN_POINT('Ctrl Pts',(1.7862720895248,0.944566316568132,7.02655536300634));
#160625=CARTESIAN_POINT('Origin',(-0.0260253471876515,0.803577338089193,
-0.196947453086254));
#160626=CARTESIAN_POINT('Ctrl Pts',(2.058047714,0.940053947,7.212103688));
#160627=CARTESIAN_POINT('Ctrl Pts',(2.451422449,0.874398499000001,7.099850175));
#160628=CARTESIAN_POINT('Ctrl Pts',(2.830254416,0.809170361000001,6.945477661));
#160629=CARTESIAN_POINT('Ctrl Pts',(1.759736143,0.940053947,7.033194773));
#160630=CARTESIAN_POINT('Ctrl Pts',(2.143352525,0.874398499000001,6.937212273));
#160631=CARTESIAN_POINT('Ctrl Pts',(2.514253728,0.809170361000001,6.800075602));
#160632=CARTESIAN_POINT('',(2.50984261151385,0.809946052722277,6.80170493911415));
#160633=CARTESIAN_POINT('Origin',(-0.0471666674626342,0.94642390327405,
-0.192979181616322));
#160634=CARTESIAN_POINT('Ctrl Pts',(2.59587005248641,0.849330499397736,
7.03643792480018));
#160635=CARTESIAN_POINT('Ctrl Pts',(2.58148121593858,0.843074445580346,
6.99729178184802));
#160636=CARTESIAN_POINT('Ctrl Pts',(2.56710953902123,0.836669225428602,
6.95813867299499));
#160637=CARTESIAN_POINT('Ctrl Pts',(2.538437094516,0.823551550486689,6.87990743449499));
#160638=CARTESIAN_POINT('Ctrl Pts',(2.52412027548073,0.816831759701209,
6.84078551863939));
#160639=CARTESIAN_POINT('Ctrl Pts',(2.50984260926868,0.809946053624328,
6.80170493977546));
#160640=CARTESIAN_POINT('Ctrl Pts',(2.35930162164549,0.809162772,7.119802199134));
#160641=CARTESIAN_POINT('Ctrl Pts',(2.74764941145811,0.874819703,6.99111469553932));
#160642=CARTESIAN_POINT('Ctrl Pts',(3.1196964750598,0.940053947,6.82095164824368));
#160643=CARTESIAN_POINT('Ctrl Pts',(3.13256405620265,0.942310131795108,
6.81506640674388));
#160644=CARTESIAN_POINT('Ctrl Pts',(3.14543163734554,0.944566316590221,
6.80918116524396));
#160645=CARTESIAN_POINT('Ctrl Pts',(2.505416106,0.809162772000001,6.803336691));
#160646=CARTESIAN_POINT('Ctrl Pts',(2.876502367,0.874819703,6.66667941000001));
#160647=CARTESIAN_POINT('Ctrl Pts',(3.230523466,0.940053947,6.49047133400001));
#160648=CARTESIAN_POINT('Ctrl Pts',(3.24276760300128,0.942310131795108,
6.48437701976457));
#160649=CARTESIAN_POINT('Ctrl Pts',(3.2550117400026,0.944566316590218,6.47828270552914));
#160650=CARTESIAN_POINT('Origin',(-0.0677547966818837,0.803577340718484,
-0.186748302152657));
#160651=CARTESIAN_POINT('Ctrl Pts',(3.560320807,0.940053947,6.601069288));
#160652=CARTESIAN_POINT('Ctrl Pts',(3.920367472,0.874398499000001,6.406876261));
#160653=CARTESIAN_POINT('Ctrl Pts',(4.257157031,0.809170361000001,6.174675215));
#160654=CARTESIAN_POINT('Ctrl Pts',(3.230523466,0.940053947,6.490471334));
#160655=CARTESIAN_POINT('Ctrl Pts',(3.58453771,0.874398499000001,6.314266669));
#160656=CARTESIAN_POINT('Ctrl Pts',(3.917287119,0.809170361000001,6.100603383));
#160657=CARTESIAN_POINT('',(3.91332939130414,0.809946052687199,6.10314288710069));
#160658=CARTESIAN_POINT('Origin',(-0.0875486649536983,0.94642384785471,
-0.178327848723953));
#160659=CARTESIAN_POINT('Ctrl Pts',(4.04780621107471,0.84933049940968,6.31389458846495));
#160660=CARTESIAN_POINT('Ctrl Pts',(4.02533850999492,0.843074444501961,
6.27875682894537));
#160661=CARTESIAN_POINT('Ctrl Pts',(4.00288607621306,0.836669224983247,
6.24360858740351));
#160662=CARTESIAN_POINT('Ctrl Pts',(3.95806657572774,0.8235515505967,6.17337008284586));
#160663=CARTESIAN_POINT('Ctrl Pts',(3.93567442065259,0.816831759834135,
6.13824050874194));
#160664=CARTESIAN_POINT('Ctrl Pts',(3.91332938911934,0.809946053720409,
6.10314288828895));
#160665=CARTESIAN_POINT('Ctrl Pts',(3.83468947317847,0.809162772000001,
6.44616507150864));
#160666=CARTESIAN_POINT('Ctrl Pts',(4.18629389863323,0.874819703,6.23700291524641));
#160667=CARTESIAN_POINT('Ctrl Pts',(4.51306268385258,0.940053947,5.99083906467152));
#160668=CARTESIAN_POINT('Ctrl Pts',(4.52436427523322,0.942310131810363,
5.9823252672168));
#160669=CARTESIAN_POINT('Ctrl Pts',(4.5356658666138,0.944566316620727,5.97381146976219));
#160670=CARTESIAN_POINT('Ctrl Pts',(3.909357153,0.809162772000001,6.105688057));
#160671=CARTESIAN_POINT('Ctrl Pts',(4.242390347,0.874819703,5.89245317));
#160672=CARTESIAN_POINT('Ctrl Pts',(4.550255102,0.940053947,5.644260669));
#160673=CARTESIAN_POINT('Ctrl Pts',(4.56090288054828,0.942310131810363,
5.6356767088517));
#160674=CARTESIAN_POINT('Ctrl Pts',(4.57155065909668,0.944566316620727,
5.62709274870327));
#160675=CARTESIAN_POINT('Origin',(-0.106316028050865,0.803577351965726,
-0.167816835776771));
#160676=CARTESIAN_POINT('Ctrl Pts',(4.896117256,0.940053947,5.681376225));
#160677=CARTESIAN_POINT('Ctrl Pts',(5.206000469,0.874398499000001,5.414323933));
#160678=CARTESIAN_POINT('Ctrl Pts',(5.484999715,0.809170361000001,5.115151819));
#160679=CARTESIAN_POINT('Ctrl Pts',(4.550255102,0.940053947,5.644260669));
#160680=CARTESIAN_POINT('Ctrl Pts',(4.858113896,0.874398499000001,5.396072974));
#160681=CARTESIAN_POINT('Ctrl Pts',(5.13715251700001,0.809170361000001,
5.115873729));
#160682=CARTESIAN_POINT('',(5.13383323727461,0.809946052692845,5.11920465507359));
#160683=CARTESIAN_POINT('Origin',(-0.123836949338836,0.946423886243637,
-0.155338165371992));
#160684=CARTESIAN_POINT('Ctrl Pts',(5.31047145097424,0.849330499403383,
5.29612055860465));
#160685=CARTESIAN_POINT('Ctrl Pts',(5.28097545619076,0.843074445266492,
5.26663419557828));
#160686=CARTESIAN_POINT('Ctrl Pts',(5.25149211254345,0.836669225282618,
5.23713430764829));
#160687=CARTESIAN_POINT('Ctrl Pts',(5.19262126283321,0.823551550467761,
5.17817280592604));
#160688=CARTESIAN_POINT('Ctrl Pts',(5.16320080379069,0.81683175968613,5.14867819294392));
#160689=CARTESIAN_POINT('Ctrl Pts',(5.13383323576534,0.809946053571207,
5.11920465637222));
#160690=CARTESIAN_POINT('Ctrl Pts',(5.13077150802369,0.809162772000001,
5.47111243079908));
#160691=CARTESIAN_POINT('Ctrl Pts',(5.42919193653831,0.874819703,5.19125581030733));
#160692=CARTESIAN_POINT('Ctrl Pts',(5.69540309763417,0.940053947,4.88060150441881));
#160693=CARTESIAN_POINT('Ctrl Pts',(5.70461024979998,0.942310131934013,
4.8698572461634));
#160694=CARTESIAN_POINT('Ctrl Pts',(5.71381740196581,0.944566316868028,
4.8591129879081));
#160695=CARTESIAN_POINT('Ctrl Pts',(5.130501005,0.809162772000001,5.122544235));
#160696=CARTESIAN_POINT('Ctrl Pts',(5.40990887,0.874819703,4.842702369));
#160697=CARTESIAN_POINT('Ctrl Pts',(5.657221867,0.940053947,4.534130649));
#160698=CARTESIAN_POINT('Ctrl Pts',(5.66577540918279,0.942310131934013,
4.52345841884851));
#160699=CARTESIAN_POINT('Ctrl Pts',(5.67432895136558,0.944566316868028,
4.51278618869704));
#160700=CARTESIAN_POINT('Origin',(-0.139906057813666,0.803577330930769,
-0.141038569020607));
#160701=CARTESIAN_POINT('Ctrl Pts',(6.002976704,0.940053947,4.496028325));
#160702=CARTESIAN_POINT('Ctrl Pts',(6.24820667,0.874398499000001,4.168603835));
#160703=CARTESIAN_POINT('Ctrl Pts',(6.456369908,0.809170361,3.816449609));
#160704=CARTESIAN_POINT('Ctrl Pts',(5.657221867,0.940053947,4.534130649));
#160705=CARTESIAN_POINT('Ctrl Pts',(5.904530075,0.874398499000001,4.225564904));
#160706=CARTESIAN_POINT('Ctrl Pts',(6.116810374,0.809170361,3.891931506));
#160707=CARTESIAN_POINT('',(6.11428474814677,0.809946052705531,3.89589810483794));
#160708=CARTESIAN_POINT('Origin',(-0.154334695472245,0.946423870006678,
-0.125085081308661));
#160709=CARTESIAN_POINT('Ctrl Pts',(6.32482494729746,0.849330499396653,
4.03070581739706));
#160710=CARTESIAN_POINT('Ctrl Pts',(6.28967985561757,0.843074445169154,
4.00824959584534));
#160711=CARTESIAN_POINT('Ctrl Pts',(6.25454421281167,0.836669225267164,
3.98577744660042));
#160712=CARTESIAN_POINT('Ctrl Pts',(6.18437475129884,0.823551550514595,
3.9408499247295));
#160713=CARTESIAN_POINT('Ctrl Pts',(6.14930165691336,0.816831759845914,
3.91836940879918));
#160714=CARTESIAN_POINT('Ctrl Pts',(6.1142847471491,0.809946053730446,3.89589810607854));
#160715=CARTESIAN_POINT('Ctrl Pts',(6.18694436872949,0.809162772000001,
4.24023665216759));
#160716=CARTESIAN_POINT('Ctrl Pts',(6.41822699307587,0.874819703,3.90277135387516));
#160717=CARTESIAN_POINT('Ctrl Pts',(6.6114327918787,0.940053947,3.54215244291957));
#160718=CARTESIAN_POINT('Ctrl Pts',(6.61811498814797,0.942310131982987,
3.5296801136399));
#160719=CARTESIAN_POINT('Ctrl Pts',(6.62479718441722,0.944566316965973,
3.51720778436022));
#160720=CARTESIAN_POINT('Ctrl Pts',(6.111748332,0.809162772000001,3.899875938));
#160721=CARTESIAN_POINT('Ctrl Pts',(6.324466068,0.874819703,3.566512188));
#160722=CARTESIAN_POINT('Ctrl Pts',(6.499663225,0.940053947,3.211989719));
#160723=CARTESIAN_POINT('Ctrl Pts',(6.50572257620033,0.942310131982987,
3.19972824064686));
#160724=CARTESIAN_POINT('Ctrl Pts',(6.5117819274008,0.944566316965973,3.18746676229378));
#160725=CARTESIAN_POINT('Origin',(-0.166954220895447,0.803577360084644,
-0.107665456760575));
#160726=CARTESIAN_POINT('Ctrl Pts',(6.829143632,0.940053947,3.100451136));
#160727=CARTESIAN_POINT('Ctrl Pts',(6.998253672,0.874398499000001,2.727964456));
#160728=CARTESIAN_POINT('Ctrl Pts',(7.125847419,0.809170361,2.339294456));
#160729=CARTESIAN_POINT('Ctrl Pts',(6.499663225,0.940053947,3.211989719));
#160730=CARTESIAN_POINT('Ctrl Pts',(6.674856991,0.874398499000001,2.857474115));
#160731=CARTESIAN_POINT('Ctrl Pts',(6.810452976,0.809170361,2.486006892));
#160732=CARTESIAN_POINT('',(6.80883909887103,0.809946052703242,2.49042368839839));
#160733=CARTESIAN_POINT('Origin',(-0.177616241857739,0.946423877604977,
-0.0889833580990079));
#160734=CARTESIAN_POINT('Ctrl Pts',(7.04343665837362,0.849330499394402,
2.57681975190768));
#160735=CARTESIAN_POINT('Ctrl Pts',(7.00428581770227,0.843074445515644,
2.56244370102973));
#160736=CARTESIAN_POINT('Ctrl Pts',(6.96514077770283,0.83666922543599,2.54805006240474));
#160737=CARTESIAN_POINT('Ctrl Pts',(6.88695374929916,0.823551550542199,
2.51925728103009));
#160738=CARTESIAN_POINT('Ctrl Pts',(6.84786799755061,0.816831759784013,
2.50484202561442));
#160739=CARTESIAN_POINT('Ctrl Pts',(6.80883909801412,0.809946053662277,
2.49042369025996));
#160740=CARTESIAN_POINT('Ctrl Pts',(6.95382258706006,0.809162772,2.81109212166397));
#160741=CARTESIAN_POINT('Ctrl Pts',(7.10715288826951,0.874819703,2.4317976459104));
#160742=CARTESIAN_POINT('Ctrl Pts',(7.21831923755852,0.940053947,2.03807626899816));
#160743=CARTESIAN_POINT('Ctrl Pts',(7.22216402529775,0.942310131745766,
2.02445906260161));
#160744=CARTESIAN_POINT('Ctrl Pts',(7.22600881303697,0.944566316491536,
2.01084185620499));
#160745=CARTESIAN_POINT('Ctrl Pts',(6.807217099,0.809162772000001,2.494853776));
#160746=CARTESIAN_POINT('Ctrl Pts',(6.94329826,0.874819703,2.12355586));
#160747=CARTESIAN_POINT('Ctrl Pts',(7.038187555,0.940053947,1.73965972));
#160748=CARTESIAN_POINT('Ctrl Pts',(7.04146938624059,0.942310131745766,
1.72638232822052));
#160749=CARTESIAN_POINT('Ctrl Pts',(7.04475121748121,0.944566316491536,
1.71310493644103));
#160750=CARTESIAN_POINT('Origin',(-0.186195806700906,0.803577371035635,
-0.0692580764843428));
#160751=CARTESIAN_POINT('Ctrl Pts',(7.335987395,0.940053947,1.559900299));
#160752=CARTESIAN_POINT('Ctrl Pts',(7.42107011,0.874398499000001,1.15976849));
#160753=CARTESIAN_POINT('Ctrl Pts',(7.462128226,0.809170361,0.752756495));
#160754=CARTESIAN_POINT('Ctrl Pts',(7.038187555,0.940053947,1.73965972));
#160755=CARTESIAN_POINT('Ctrl Pts',(7.133075012,0.874398499000001,1.355771012));
#160756=CARTESIAN_POINT('Ctrl Pts',(7.185646366,0.809170361,0.963839358));
#160757=CARTESIAN_POINT('',(7.18501970015274,0.809946052684096,0.968499827292238));
#160758=CARTESIAN_POINT('Origin',(-0.192592153795034,0.946423760555048,
-0.0487206444150247));
#160759=CARTESIAN_POINT('Ctrl Pts',(7.43270510014592,0.849330499432997,
1.00244445911311));
#160760=CARTESIAN_POINT('Ctrl Pts',(7.39137915765184,0.843074445435521,
0.996820785600723));
#160761=CARTESIAN_POINT('Ctrl Pts',(7.35005510021506,0.836669225363939,
0.991178688685446));
#160762=CARTESIAN_POINT('Ctrl Pts',(7.26750644432747,0.823551550483965,
0.979866966386957));
#160763=CARTESIAN_POINT('Ctrl Pts',(7.2262356410549,0.816831759582578,0.974191012744954));
#160764=CARTESIAN_POINT('Ctrl Pts',(7.18501969968291,0.809946053480066,
0.968499829781929));
#160765=CARTESIAN_POINT('Ctrl Pts',(7.39554779057258,0.809162772,1.25050404734931));
#160766=CARTESIAN_POINT('Ctrl Pts',(7.46375621382019,0.874819703,0.84711578386319));
#160767=CARTESIAN_POINT('Ctrl Pts',(7.48768509771001,0.940053947,0.438701914431586));
#160768=CARTESIAN_POINT('Ctrl Pts',(7.48851269958806,0.942310131747133,
0.424576555015612));
#160769=CARTESIAN_POINT('Ctrl Pts',(7.48934030146606,0.94456631649427,0.410451195599633));
#160770=CARTESIAN_POINT('Ctrl Pts',(7.184387961,0.809162772000001,0.973175025));
#160771=CARTESIAN_POINT('Ctrl Pts',(7.237469544,0.874819703,0.581304421));
#160772=CARTESIAN_POINT('Ctrl Pts',(7.24761405700001,0.940053947,0.185985165));
#160773=CARTESIAN_POINT('Ctrl Pts',(7.24796491406668,0.942310131747134,
0.17231269451601));
#160774=CARTESIAN_POINT('Ctrl Pts',(7.24831577113348,0.944566316494269,
0.158640224032027));
#160775=CARTESIAN_POINT('Origin',(-0.196731118555223,0.803577356082231,
-0.0276122899099263));
#160776=CARTESIAN_POINT('Ctrl Pts',(7.49980854,0.940053947,-0.053589743));
#160777=CARTESIAN_POINT('Ctrl Pts',(7.496885558,0.874398499000001,-0.462656961));
#160778=CARTESIAN_POINT('Ctrl Pts',(7.44948821,0.809170361,-0.868979523));
#160779=CARTESIAN_POINT('Ctrl Pts',(7.247614057,0.940053947,0.185985165));
#160780=CARTESIAN_POINT('Ctrl Pts',(7.257758374,0.874398499000001,-0.209326436));
#160781=CARTESIAN_POINT('Ctrl Pts',(7.224846918,0.809170361,-0.603396233));
#160782=CARTESIAN_POINT('',(7.22523676689643,0.809946052675541,-0.598710008135555));
#160783=CARTESIAN_POINT('Origin',(-0.198563384833296,0.946423902094758,
-0.00617996603265752));
#160784=CARTESIAN_POINT('Ctrl Pts',(7.47442851183213,0.849330499401343,
-0.61880402232886));
#160785=CARTESIAN_POINT('Ctrl Pts',(7.43285981681545,0.843074444412867,
-0.615412360954006));
#160786=CARTESIAN_POINT('Ctrl Pts',(7.39128901257921,0.836669224881622,
-0.612039098317023));
#160787=CARTESIAN_POINT('Ctrl Pts',(7.30823861543218,0.823551550480405,
-0.60534083824266));
#160788=CARTESIAN_POINT('Ctrl Pts',(7.26671253872467,0.816831759653862,
-0.602012088542576));
#160789=CARTESIAN_POINT('Ctrl Pts',(7.22523676694034,0.809946053561054,
-0.59871000573749));
#160790=CARTESIAN_POINT('Ctrl Pts',(7.49146539823555,0.809162772000001,
-0.368556206897238));
#160791=CARTESIAN_POINT('Ctrl Pts',(7.47136259378149,0.874819703,-0.777176271136419));
#160792=CARTESIAN_POINT('Ctrl Pts',(7.40693512425472,0.940053947,-1.18118565372789));
#160793=CARTESIAN_POINT('Ctrl Pts',(7.4047068423435,0.942310131931147,-1.19515868116184));
#160794=CARTESIAN_POINT('Ctrl Pts',(7.40247856043215,0.944566316862295,
-1.20913170859578));
#160795=CARTESIAN_POINT('Ctrl Pts',(7.225624826,0.809162772000001,-0.594008309));
#160796=CARTESIAN_POINT('Ctrl Pts',(7.193224795,0.874819703,-0.988128168));
#160797=CARTESIAN_POINT('Ctrl Pts',(7.118150181,0.940053947,-1.376385849));
#160798=CARTESIAN_POINT('Ctrl Pts',(7.11555365803243,0.942310131931147,
-1.38981408968405));
#160799=CARTESIAN_POINT('Ctrl Pts',(7.11295713506485,0.944566316862295,
-1.40324233036812));
#160800=CARTESIAN_POINT('Origin',(-0.198067613676669,0.803577356916781,
0.0153246665703818));
#160801=CARTESIAN_POINT('Ctrl Pts',(7.312946974,0.940053947,-1.664573988));
#160802=CARTESIAN_POINT('Ctrl Pts',(7.222154969,0.874398499000001,-2.063449087));
#160803=CARTESIAN_POINT('Ctrl Pts',(7.088518405,0.809170361,-2.450083024));
#160804=CARTESIAN_POINT('Ctrl Pts',(7.118150181,0.940053947,-1.376385849));
#160805=CARTESIAN_POINT('Ctrl Pts',(7.04307702,0.874398499000001,-1.764636013));
#160806=CARTESIAN_POINT('Ctrl Pts',(6.926221658,0.809170361,-2.142417687));
#160807=CARTESIAN_POINT('',(6.92760979279974,0.809946052722275,-2.13792482936519));
#160808=CARTESIAN_POINT('Origin',(-0.19524961185327,0.946423874648229,0.036649780107621));
#160809=CARTESIAN_POINT('Ctrl Pts',(7.16665595397255,0.849330499387892,
-2.2111179158326));
#160810=CARTESIAN_POINT('Ctrl Pts',(7.12678822298043,0.843074445056534,
-2.19886951017339));
#160811=CARTESIAN_POINT('Ctrl Pts',(7.08691447053379,0.836669225196569,
-2.18663861775412));
#160812=CARTESIAN_POINT('Ctrl Pts',(7.00724567148069,0.823551550493151,
-2.16224357833837));
#160813=CARTESIAN_POINT('Ctrl Pts',(6.96740603447509,0.816831759727534,
-2.15006577416038));
#160814=CARTESIAN_POINT('Ctrl Pts',(6.92760979323707,0.809946053613321,
-2.13792482742635));
#160815=CARTESIAN_POINT('Ctrl Pts',(7.23709041010625,0.809162772000001,
-1.97038318210479));
#160816=CARTESIAN_POINT('Ctrl Pts',(7.1296163636436,0.874819703,-2.36512842791326));
#160817=CARTESIAN_POINT('Ctrl Pts',(6.97984509784344,0.940053947,-2.74584229453887));
#160818=CARTESIAN_POINT('Ctrl Pts',(6.97466512443654,0.942310131771728,
-2.75900962469549));
#160819=CARTESIAN_POINT('Ctrl Pts',(6.96948515102947,0.944566316543458,
-2.77217695485211));
#160820=CARTESIAN_POINT('Ctrl Pts',(6.928999505,0.809162772000001,-2.133416475));
#160821=CARTESIAN_POINT('Ctrl Pts',(6.81263284900001,0.874819703,-2.511356981));
#160822=CARTESIAN_POINT('Ctrl Pts',(6.655849513,0.940053947,-2.874398591));
#160823=CARTESIAN_POINT('Ctrl Pts',(6.65042702086314,0.942310131771728,
-2.88695471032876));
#160824=CARTESIAN_POINT('Ctrl Pts',(6.64500452872626,0.944566316543458,
-2.89951082965752));
#160825=CARTESIAN_POINT('Origin',(-0.190142576295623,0.803577351896187,
0.0575450801711413));
#160826=CARTESIAN_POINT('Ctrl Pts',(6.784140134,0.940053947,-3.197724603));
#160827=CARTESIAN_POINT('Ctrl Pts',(6.609724441,0.874398499000001,-3.567756627));
#160828=CARTESIAN_POINT('Ctrl Pts',(6.396097357,0.809170361,-3.916623367));
#160829=CARTESIAN_POINT('Ctrl Pts',(6.655849513,0.940053947,-2.874398591));
#160830=CARTESIAN_POINT('Ctrl Pts',(6.499069213,0.874398499000001,-3.237433171));
#160831=CARTESIAN_POINT('Ctrl Pts',(6.303733971,0.809170361,-3.581262071));
#160832=CARTESIAN_POINT('',(6.30605548324046,0.809946052678392,-3.5771726618393));
#160833=CARTESIAN_POINT('Origin',(-0.1828060003259,0.946423907519971,0.0777657385988639));
#160834=CARTESIAN_POINT('Ctrl Pts',(6.52377852850538,0.849330499411468,
-3.70004239318147));
#160835=CARTESIAN_POINT('Ctrl Pts',(6.48747592982481,0.843074445384863,
-3.67950996577842));
#160836=CARTESIAN_POINT('Ctrl Pts',(6.45116368279414,0.836669225346678,
-3.65899334610276));
#160837=CARTESIAN_POINT('Ctrl Pts',(6.37860170748226,0.823551550490179,
-3.61804221184952));
#160838=CARTESIAN_POINT('Ctrl Pts',(6.34231136673367,0.816831759681685,
-3.59758477350974));
#160839=CARTESIAN_POINT('Ctrl Pts',(6.30605548418455,0.809946053571847,
-3.57717265986101));
#160840=CARTESIAN_POINT('Ctrl Pts',(6.64431711846076,0.809162772000001,
-3.48007722958917));
#160841=CARTESIAN_POINT('Ctrl Pts',(6.45449719567497,0.874819703,-3.8424898080853));
#160842=CARTESIAN_POINT('Ctrl Pts',(6.22638527100719,0.940053947,-4.18210640003388));
#160843=CARTESIAN_POINT('Ctrl Pts',(6.21849581559411,0.942310131810126,
-4.1938523443269));
#160844=CARTESIAN_POINT('Ctrl Pts',(6.21060636018102,0.944566316620252,
-4.20559828861992));
#160845=CARTESIAN_POINT('Ctrl Pts',(6.308381869,0.809162772000001,-3.573068457));
#160846=CARTESIAN_POINT('Ctrl Pts',(6.113489763,0.874819703,-3.917157533));
#160847=CARTESIAN_POINT('Ctrl Pts',(5.88232872,0.940053947,-4.238007649));
#160848=CARTESIAN_POINT('Ctrl Pts',(5.87433380809593,0.942310131810126,
-4.24910453789851));
#160849=CARTESIAN_POINT('Ctrl Pts',(5.86633889619174,0.944566316620252,
-4.26020142679696));
#160850=CARTESIAN_POINT('Origin',(-0.173326571395247,0.80357735796664,0.0970746776577225));
#160851=CARTESIAN_POINT('Ctrl Pts',(5.938114442,0.940053947,-4.58135317));
#160852=CARTESIAN_POINT('Ctrl Pts',(5.688230544,0.874398499000001,-4.905239832));
#160853=CARTESIAN_POINT('Ctrl Pts',(5.404601906,0.809170361,-5.200026753));
#160854=CARTESIAN_POINT('Ctrl Pts',(5.88232872,0.940053947,-4.238007649));
#160855=CARTESIAN_POINT('Ctrl Pts',(5.651172152,0.874398499000001,-4.55885155200001));
#160856=CARTESIAN_POINT('Ctrl Pts',(5.38649069,0.809170361,-4.85265062));
#160857=CARTESIAN_POINT('',(5.38963702945792,0.809946052688611,-4.84915587636754));
#160858=CARTESIAN_POINT('Origin',(-0.161814908904617,0.946423888559224,
0.115245624273202));
#160859=CARTESIAN_POINT('Ctrl Pts',(5.57585646967174,0.849330499367115,
-5.01595700001293));
#160860=CARTESIAN_POINT('Ctrl Pts',(5.54481647208769,0.84307444565754,-4.98810062512837));
#160861=CARTESIAN_POINT('Ctrl Pts',(5.51376365132296,0.836669225498839,
-4.96025761229804));
#160862=CARTESIAN_POINT('Ctrl Pts',(5.45170141738891,0.823551550511566,
-4.90466521235823));
#160863=CARTESIAN_POINT('Ctrl Pts',(5.42065726996587,0.816831759876436,
-4.87688470765218));
#160864=CARTESIAN_POINT('Ctrl Pts',(5.38963703080557,0.809946053748422,
-4.84915587459674));
#160865=CARTESIAN_POINT('Ctrl Pts',(5.74086294257922,0.809162772000001,
-4.82704673403754));
#160866=CARTESIAN_POINT('Ctrl Pts',(5.47757291233011,0.874819703,-5.14018063457471));
#160867=CARTESIAN_POINT('Ctrl Pts',(5.18178659015694,0.940053947,-5.42281985940062));
#160868=CARTESIAN_POINT('Ctrl Pts',(5.1715565548202,0.942310131857983,-5.43259519057982));
#160869=CARTESIAN_POINT('Ctrl Pts',(5.16132651948343,0.944566316715966,
-5.44237052175898));
#160870=CARTESIAN_POINT('Ctrl Pts',(5.392791307,0.809162772000001,-4.845647729));
#160871=CARTESIAN_POINT('Ctrl Pts',(5.128486691,0.874819703,-5.139796152));
#160872=CARTESIAN_POINT('Ctrl Pts',(4.833756773,0.940053947,-5.403452179));
#160873=CARTESIAN_POINT('Ctrl Pts',(4.8235632743494,0.942310131857983,-5.41257095925034));
#160874=CARTESIAN_POINT('Ctrl Pts',(4.81336977569886,0.944566316715967,
-5.4216897395007));
#160875=CARTESIAN_POINT('Origin',(-0.148406033224281,0.803577342228433,
0.132065168002498));
#160876=CARTESIAN_POINT('Ctrl Pts',(4.814429119,0.940053947,-5.750762755));
#160877=CARTESIAN_POINT('Ctrl Pts',(4.500761309,0.874398499000001,-6.013359475));
#160878=CARTESIAN_POINT('Ctrl Pts',(4.160393277,0.809170361,-6.240282668));
#160879=CARTESIAN_POINT('Ctrl Pts',(4.833756773,0.940053947,-5.403452179));
#160880=CARTESIAN_POINT('Ctrl Pts',(4.539032563,0.874398499000001,-5.667103101));
#160881=CARTESIAN_POINT('Ctrl Pts',(4.217381091,0.809170361,-5.89713462));
#160882=CARTESIAN_POINT('',(4.22120513711784,0.809946052707974,-5.89439795128935));
#160883=CARTESIAN_POINT('Origin',(-0.133257209627604,0.946423898125065,
0.147336455417874));
#160884=CARTESIAN_POINT('Ctrl Pts',(4.3672135600113,0.849330499383033,-6.09733103232013));
#160885=CARTESIAN_POINT('Ctrl Pts',(4.34288755318523,0.843074444573075,
-6.06345323611053));
#160886=CARTESIAN_POINT('Ctrl Pts',(4.3185461571543,0.836669224993378,-6.0295857421921));
#160887=CARTESIAN_POINT('Ctrl Pts',(4.26988562827292,0.8235515505247,-5.96195151866442));
#160888=CARTESIAN_POINT('Ctrl Pts',(4.24553926283837,0.816831759838917,
-5.92814693247654));
#160889=CARTESIAN_POINT('Ctrl Pts',(4.22120513897645,0.809946053714662,
-5.89439794974384));
#160890=CARTESIAN_POINT('Ctrl Pts',(4.56897239579151,0.809162772,-5.94830889693425));
#160891=CARTESIAN_POINT('Ctrl Pts',(4.2445234080415,0.874819703,-6.19752232790785));
#160892=CARTESIAN_POINT('Ctrl Pts',(3.89489332643903,0.940053947,-6.40996828922183));
#160893=CARTESIAN_POINT('Ctrl Pts',(3.88280105600422,0.942310131926778,
-6.41731592362796));
#160894=CARTESIAN_POINT('Ctrl Pts',(3.87070878556934,0.944566316853557,
-6.42466355803407));
#160895=CARTESIAN_POINT('Ctrl Pts',(4.225039818,0.809162772000001,-5.891649899));
#160896=CARTESIAN_POINT('Ctrl Pts',(3.903681281,0.874819703,-6.122103616));
#160897=CARTESIAN_POINT('Ctrl Pts',(3.559163733,0.940053947,-6.316237292));
#160898=CARTESIAN_POINT('Ctrl Pts',(3.54724828413225,0.942310131926778,
-6.32295157956916));
#160899=CARTESIAN_POINT('Ctrl Pts',(3.53533283526452,0.944566316853556,
-6.32966586713822));
#160900=CARTESIAN_POINT('Origin',(-0.116546242053256,0.803577346880212,
0.160880395793309));
#160901=CARTESIAN_POINT('Ctrl Pts',(3.465626441,0.940053947,-6.651273064));
#160902=CARTESIAN_POINT('Ctrl Pts',(3.102841477,0.874398499000001,-6.840301112));
#160903=CARTESIAN_POINT('Ctrl Pts',(2.721649282,0.809170361,-6.988749902));
#160904=CARTESIAN_POINT('Ctrl Pts',(3.559163733,0.940053947,-6.31623729200001));
#160905=CARTESIAN_POINT('Ctrl Pts',(3.214652856,0.874398499000001,-6.51036720800001));
#160906=CARTESIAN_POINT('Ctrl Pts',(2.85107144,0.809170361,-6.66587516));
#160907=CARTESIAN_POINT('',(2.85539438458225,0.809946052650979,-6.66402452877942));
#160908=CARTESIAN_POINT('Origin',(-0.0984686780031424,0.946423832486099,
0.172538085307491));
#160909=CARTESIAN_POINT('Ctrl Pts',(2.9543645978865,0.84933049941643,-6.89360064286475));
#160910=CARTESIAN_POINT('Ctrl Pts',(2.93789004392451,0.843074444415432,
-6.85528551721847));
#160911=CARTESIAN_POINT('Ctrl Pts',(2.92139824653569,0.836669224896916,
-6.81697714634658));
#160912=CARTESIAN_POINT('Ctrl Pts',(2.88841473288365,0.823551550476378,
-6.74046359851006));
#160913=CARTESIAN_POINT('Ctrl Pts',(2.8719045584201,0.816831759630593,-6.70221559503671));
#160914=CARTESIAN_POINT('Ctrl Pts',(2.85539438671172,0.809946053538579,
-6.66402452769881));
#160915=CARTESIAN_POINT('Ctrl Pts',(3.18344177798828,0.809162772,-6.79143474774354));
#160916=CARTESIAN_POINT('Ctrl Pts',(2.81300470637386,0.874819703,-6.9650747653572));
#160917=CARTESIAN_POINT('Ctrl Pts',(2.42587918038149,0.940053947,-7.09739372560097));
#160918=CARTESIAN_POINT('Ctrl Pts',(2.41249009638585,0.94231013191591,-7.10197009567725));
#160919=CARTESIAN_POINT('Ctrl Pts',(2.39910101239022,0.944566316831819,
-7.10654646575353));
#160920=CARTESIAN_POINT('Ctrl Pts',(2.859730162,0.809162772000001,-6.662165068));
#160921=CARTESIAN_POINT('Ctrl Pts',(2.496344072,0.874819703,-6.818148319));
#160922=CARTESIAN_POINT('Ctrl Pts',(2.118148151,0.940053947,-6.933682168));
#160923=CARTESIAN_POINT('Ctrl Pts',(2.10506790541275,0.94231013191591,-6.93767800992912));
#160924=CARTESIAN_POINT('Ctrl Pts',(2.09198765982549,0.94456631683182,-6.94167385185837));
#160925=CARTESIAN_POINT('Origin',(-0.0792369432847576,0.803577312784041,
0.182173122882493));
#160926=CARTESIAN_POINT('Ctrl Pts',(1.954774922,0.940053947,-7.240777238));
#160927=CARTESIAN_POINT('Ctrl Pts',(1.559836226,0.874398499000001,-7.347397871));
#160928=CARTESIAN_POINT('Ctrl Pts',(1.155643991,0.809170361,-7.410430957));
#160929=CARTESIAN_POINT('Ctrl Pts',(2.118148151,0.940053947,-6.933682168));
#160930=CARTESIAN_POINT('Ctrl Pts',(1.739959553,0.874398499000001,-7.04921378));
#160931=CARTESIAN_POINT('Ctrl Pts',(1.351448856,0.809170361,-7.122926785));
#160932=CARTESIAN_POINT('',(1.35606856387977,0.809946052736701,-7.12204872627898));
#160933=CARTESIAN_POINT('Origin',(-0.0590759568677302,0.946423831175772,
0.189672134415341));
#160934=CARTESIAN_POINT('Ctrl Pts',(1.40337283024097,0.849330499423155,
-7.36753314860582));
#160935=CARTESIAN_POINT('Ctrl Pts',(1.39552006198321,0.843074444748845,
-7.32657226924519));
#160936=CARTESIAN_POINT('Ctrl Pts',(1.38764900074009,0.836669225060746,
-7.28561427662802));
#160937=CARTESIAN_POINT('Ctrl Pts',(1.37188477410703,0.823551550508327,
-7.20379909165716));
#160938=CARTESIAN_POINT('Ctrl Pts',(1.36398278850603,0.81683175972654,-7.16289610614498));
#160939=CARTESIAN_POINT('Ctrl Pts',(1.35606856587717,0.809946053612075,
-7.12204872574442));
#160940=CARTESIAN_POINT('Ctrl Pts',(1.64905696119522,0.809162772000001,
-7.31700065792982));
#160941=CARTESIAN_POINT('Ctrl Pts',(1.24995303106729,0.874819703,-7.40694804797127));
#160942=CARTESIAN_POINT('Ctrl Pts',(0.843433619571964,0.940053947,-7.45295291915762));
#160943=CARTESIAN_POINT('Ctrl Pts',(0.829373781529389,0.94231013177134,
-7.45454403884281));
#160944=CARTESIAN_POINT('Ctrl Pts',(0.815313943486812,0.944566316542682,
-7.45613515852813));
#160945=CARTESIAN_POINT('Ctrl Pts',(1.360702703,0.809162772000001,-7.12116480300001));
#160946=CARTESIAN_POINT('Ctrl Pts',(0.97228059,0.874819703,-7.19538398400001));
#160947=CARTESIAN_POINT('Ctrl Pts',(0.578090317,0.940053947,-7.226915773));
#160948=CARTESIAN_POINT('Ctrl Pts',(0.564456893257817,0.94231013177134,
-7.22800632817153));
#160949=CARTESIAN_POINT('Ctrl Pts',(0.550823469515642,0.944566316542682,
-7.22909688334309));
#160950=CARTESIAN_POINT('Origin',(-0.0382226035147889,0.803577363718229,
0.194947726870536));
#160951=CARTESIAN_POINT('Ctrl Pts',(0.3525203,0.940053947,-7.491710715));
#160952=CARTESIAN_POINT('Ctrl Pts',(-0.056105233,0.874398499000001,-7.510938472));
#160953=CARTESIAN_POINT('Ctrl Pts',(-0.464397928,0.809170361,-7.485608497));
#160954=CARTESIAN_POINT('Ctrl Pts',(0.578090316999999,0.940053947,-7.226915773));
#160955=CARTESIAN_POINT('Ctrl Pts',(0.183907677,0.874398499000001,-7.258446951));
#160956=CARTESIAN_POINT('Ctrl Pts',(-0.211365974,0.809170361,-7.246918271));
#160957=CARTESIAN_POINT('',(-0.206665515349642,0.809946052703829,-7.24705384080755));
#160958=CARTESIAN_POINT('Origin',(-0.0169208965170819,0.946423889145898,
0.197937327803924));
#160959=CARTESIAN_POINT('Ctrl Pts',(-0.213239090823349,0.84933049680011,
-7.49696797599282));
#160960=CARTESIAN_POINT('Ctrl Pts',(-0.212102887475241,0.843074442824839,
-7.45527663117971));
#160961=CARTESIAN_POINT('Ctrl Pts',(-0.210985170255643,0.83666922533313,
-7.41358418244774));
#160962=CARTESIAN_POINT('Ctrl Pts',(-0.208792991489413,0.823551550440252,
-7.33029294605962));
#160963=CARTESIAN_POINT('Ctrl Pts',(-0.207717300195503,0.81683175959965,
-7.28864755583171));
#160964=CARTESIAN_POINT('Ctrl Pts',(-0.206665513343767,0.809946053541909,
-7.24705384071953));
#160965=CARTESIAN_POINT('Ctrl Pts',(0.0375640730725487,0.809162772000001,
-7.50043175005473));
#160966=CARTESIAN_POINT('Ctrl Pts',(-0.371545059360011,0.874819703,-7.50248067266858));
#160967=CARTESIAN_POINT('Ctrl Pts',(-0.778449959964432,0.940053947,-7.46002031823397));
#160968=CARTESIAN_POINT('Ctrl Pts',(-0.792523130628518,0.942310131793034,
-7.45855178882197));
#160969=CARTESIAN_POINT('Ctrl Pts',(-0.806596301292605,0.944566316586069,
-7.45708325941005));
#160970=CARTESIAN_POINT('Ctrl Pts',(-0.201949703,0.809162772000001,-7.247186786));
#160971=CARTESIAN_POINT('Ctrl Pts',(-0.597245653,0.874819703,-7.236171492));
#160972=CARTESIAN_POINT('Ctrl Pts',(-0.988998379000001,0.940053947,-7.182226828));
#160973=CARTESIAN_POINT('Ctrl Pts',(-1.0025474981257,0.942310131793034,
-7.18036110344923));
#160974=CARTESIAN_POINT('Ctrl Pts',(-1.0160966172514,0.944566316586069,
-7.17849537889843));
#160975=CARTESIAN_POINT('Origin',(0.00457900919291515,0.803577353390686,
0.198606638624294));
#160976=CARTESIAN_POINT('Ctrl Pts',(-1.266217779,0.940053947,-7.392340126));
#160977=CARTESIAN_POINT('Ctrl Pts',(-1.669423273,0.874398499000001,-7.323275938));
#160978=CARTESIAN_POINT('Ctrl Pts',(-2.062725117,0.809170361,-7.210767303));
#160979=CARTESIAN_POINT('Ctrl Pts',(-0.988998379000001,0.940053947,-7.182226828));
#160980=CARTESIAN_POINT('Ctrl Pts',(-1.380743519,0.874398499000001,-7.128283209));
#160981=CARTESIAN_POINT('Ctrl Pts',(-1.764297565,0.809170361,-7.032051913));
#160982=CARTESIAN_POINT('',(-1.75973614513862,0.809946052657848,-7.03319477389625));
#160983=CARTESIAN_POINT('Origin',(0.0260254480477046,0.946423936792007,
0.196947624644461));
#160984=CARTESIAN_POINT('Ctrl Pts',(-1.81988018914672,0.849330499393605,
-7.27585294610869));
#160985=CARTESIAN_POINT('Ctrl Pts',(-1.80980814109725,0.843074444356029,
-7.23538056476307));
#160986=CARTESIAN_POINT('Ctrl Pts',(-1.79975390841227,0.836669224901153,
-7.19490312626225));
#160987=CARTESIAN_POINT('Ctrl Pts',(-1.77970782869062,0.823551550531388,
-7.11403044988765));
#160988=CARTESIAN_POINT('Ctrl Pts',(-1.76970475880954,0.816831759807746,
-7.07358994854385));
#160989=CARTESIAN_POINT('Ctrl Pts',(-1.75973614281132,0.809946053652001,
-7.03319477430111));
#160990=CARTESIAN_POINT('Ctrl Pts',(-1.57568526882621,0.809162772000001,
-7.33315098852158));
#160991=CARTESIAN_POINT('Ctrl Pts',(-1.97567011476372,0.874819703,-7.24720563828579));
#160992=CARTESIAN_POINT('Ctrl Pts',(-2.36393408428844,0.940053947,-7.11826545847411));
#160993=CARTESIAN_POINT('Ctrl Pts',(-2.37736254142904,0.942310131756794,
-7.11380594686806));
#160994=CARTESIAN_POINT('Ctrl Pts',(-2.39079099856963,0.944566316513591,
-7.10934643526207));
#160995=CARTESIAN_POINT('Ctrl Pts',(-1.755159165,0.809162772000001,-7.03433837));
#160996=CARTESIAN_POINT('Ctrl Pts',(-2.138845352,0.874819703,-6.938603662));
#160997=CARTESIAN_POINT('Ctrl Pts',(-2.509842609,0.940053947,-6.801704939));
#160998=CARTESIAN_POINT('Ctrl Pts',(-2.52267388142274,0.942310131756794,
-6.79697017404961));
#160999=CARTESIAN_POINT('Ctrl Pts',(-2.53550515384552,0.944566316513591,
-6.79223540909921));
#161000=CARTESIAN_POINT('Origin',(0.047166591713389,0.803577351524094,0.192979168030507));
#161001=CARTESIAN_POINT('Ctrl Pts',(-2.825748922,0.940053947,-6.947311928));
#161002=CARTESIAN_POINT('Ctrl Pts',(-3.204680937,0.874398499000001,-6.79318516));
#161003=CARTESIAN_POINT('Ctrl Pts',(-3.564601571,0.809170361,-6.598758644));
#161004=CARTESIAN_POINT('Ctrl Pts',(-2.509842609,0.940053947,-6.801704939));
#161005=CARTESIAN_POINT('Ctrl Pts',(-2.880832682,0.874398499000001,-6.66480886600001));
#161006=CARTESIAN_POINT('Ctrl Pts',(-3.234732564,0.809170361,-6.488374622));
#161007=CARTESIAN_POINT('',(-3.23052346880049,0.809946052708776,-6.49047133375201));
#161008=CARTESIAN_POINT('Origin',(0.0677547936442369,0.946423863393157,
0.18674810450875));
#161009=CARTESIAN_POINT('Ctrl Pts',(-3.34142571289718,0.849330499364931,
-6.71452710196662));
#161010=CARTESIAN_POINT('Ctrl Pts',(-3.32288878222837,0.843074445722822,
-6.6771661432789));
#161011=CARTESIAN_POINT('Ctrl Pts',(-3.30436815677359,0.836669225509062,
-6.63979640280475));
#161012=CARTESIAN_POINT('Ctrl Pts',(-3.2674055064749,0.823551550480611,
-6.56512379521472));
#161013=CARTESIAN_POINT('Ctrl Pts',(-3.24894279036105,0.816831759752248,
-6.52777913445038));
#161014=CARTESIAN_POINT('Ctrl Pts',(-3.23052346667513,0.809946053623409,
-6.49047133463251));
#161015=CARTESIAN_POINT('Ctrl Pts',(-3.11525731968697,0.809162772000001,
-6.82298023806838));
#161016=CARTESIAN_POINT('Ctrl Pts',(-3.48741503215244,0.874819703,-6.65305932401257));
#161017=CARTESIAN_POINT('Ctrl Pts',(-3.83888327807438,0.940053947,-6.4436684167713));
#161018=CARTESIAN_POINT('Ctrl Pts',(-3.85103912327679,0.942310131964536,
-6.43642644403335));
#161019=CARTESIAN_POINT('Ctrl Pts',(-3.86319496847921,0.94456631692907,
-6.4291844712954));
#161020=CARTESIAN_POINT('Ctrl Pts',(-3.226299335,0.809162772000001,-6.49257211000001));
#161021=CARTESIAN_POINT('Ctrl Pts',(-3.58043502,0.874819703,-6.316594438));
#161022=CARTESIAN_POINT('Ctrl Pts',(-3.913329389,0.940053947,-6.103142887));
#161023=CARTESIAN_POINT('Ctrl Pts',(-3.92484283997394,0.942310131964536,
-6.09576047324775));
#161024=CARTESIAN_POINT('Ctrl Pts',(-3.93635629094792,0.944566316929071,
-6.08837805949553));
#161025=CARTESIAN_POINT('Origin',(0.0875487564160587,0.803577348034149,
0.178328165777322));
#161026=CARTESIAN_POINT('Ctrl Pts',(-4.253151186,0.940053947,-6.177435146));
#161027=CARTESIAN_POINT('Ctrl Pts',(-4.590091282,0.874398499000001,-5.945452595));
#161028=CARTESIAN_POINT('Ctrl Pts',(-4.899801218,0.809170361,-5.678199365));
#161029=CARTESIAN_POINT('Ctrl Pts',(-3.913329389,0.940053947,-6.10314288700001));
#161030=CARTESIAN_POINT('Ctrl Pts',(-4.246217311,0.874398499000001,-5.889695469));
#161031=CARTESIAN_POINT('Ctrl Pts',(-4.553915063,0.809170361,-5.641308146));
#161032=CARTESIAN_POINT('',(-4.55025510443955,0.809946052699697,-5.64426066870771));
#161033=CARTESIAN_POINT('Origin',(0.106316175334812,0.946423914870134,0.16781693033121));
#161034=CARTESIAN_POINT('Ctrl Pts',(-4.70672988353109,0.849330499400675,
-5.83923743366635));
#161035=CARTESIAN_POINT('Ctrl Pts',(-4.68059483219139,0.843074445265959,
-5.80673484298954));
#161036=CARTESIAN_POINT('Ctrl Pts',(-4.65447382012871,0.836669225283608,
-5.77422017452406));
#161037=CARTESIAN_POINT('Ctrl Pts',(-4.60232293361958,0.82355155046795,
-5.70923924925526));
#161038=CARTESIAN_POINT('Ctrl Pts',(-4.576263867122,0.81683175966244,-5.67673662375688));
#161039=CARTESIAN_POINT('Ctrl Pts',(-4.55025510290105,0.809946053539602,
-5.64426066976175));
#161040=CARTESIAN_POINT('Ctrl Pts',(-4.50916339980242,0.809162772,-5.99377451447543));
#161041=CARTESIAN_POINT('Ctrl Pts',(-4.83609229828455,0.874819703,-5.74782334932259));
#161042=CARTESIAN_POINT('Ctrl Pts',(-5.13433055676909,0.940053947,-5.46777260226367));
#161043=CARTESIAN_POINT('Ctrl Pts',(-5.14464539279509,0.942310131480023,
-5.45808679753304));
#161044=CARTESIAN_POINT('Ctrl Pts',(-5.15496022882122,0.94456631596005,
-5.44840099280254));
#161045=CARTESIAN_POINT('Ctrl Pts',(-4.546581334,0.809162772000001,-5.647220394));
#161046=CARTESIAN_POINT('Ctrl Pts',(-4.85460752600001,0.874819703,-5.399228277));
#161047=CARTESIAN_POINT('Ctrl Pts',(-5.133833235,0.940053947,-5.119204656));
#161048=CARTESIAN_POINT('Ctrl Pts',(-5.14349050505391,0.942310131480023,
-5.10951978944833));
#161049=CARTESIAN_POINT('Ctrl Pts',(-5.15314777510765,0.944566315960048,
-5.09983492289654));
#161050=CARTESIAN_POINT('Origin',(0.123836934952264,0.803577357315555,0.15533825453458));
#161051=CARTESIAN_POINT('Ctrl Pts',(-5.481680828,0.940053947,-5.118708363));
#161052=CARTESIAN_POINT('Ctrl Pts',(-5.76087406,0.874398499,-4.819717273));
#161053=CARTESIAN_POINT('Ctrl Pts',(-6.00589160500001,0.809170361000001,
-4.492133795));
#161054=CARTESIAN_POINT('Ctrl Pts',(-5.133833235,0.940053947,-5.119204656));
#161055=CARTESIAN_POINT('Ctrl Pts',(-5.413053537,0.874398499,-4.83918645700001));
#161056=CARTESIAN_POINT('Ctrl Pts',(-5.660161555,0.809170361000001,-4.530460371));
#161057=CARTESIAN_POINT('',(-5.65722186906473,0.809946052729482,-4.53413064781464));
#161058=CARTESIAN_POINT('Origin',(0.139906077312995,0.946423851366999,0.141038475290444));
#161059=CARTESIAN_POINT('Ctrl Pts',(-5.85195259570582,0.849330499374381,
-4.69091151222383));
#161060=CARTESIAN_POINT('Ctrl Pts',(-5.81944146920473,0.843074444858608,
-4.66478707599213));
#161061=CARTESIAN_POINT('Ctrl Pts',(-5.78694146035946,0.836669225061311,
-4.63864782873581));
#161062=CARTESIAN_POINT('Ctrl Pts',(-5.72204085546356,0.8235515504247,-4.5863970212619));
#161063=CARTESIAN_POINT('Ctrl Pts',(-5.68960393149267,0.8168317595591,-4.56025621791836));
#161064=CARTESIAN_POINT('Ctrl Pts',(-5.6572218677119,0.809946053455765,
-4.53413064930002));
#161065=CARTESIAN_POINT('Ctrl Pts',(-5.6922260106926,0.809162772,-4.88430655563095));
#161066=CARTESIAN_POINT('Ctrl Pts',(-5.95863926358306,0.874819703,-4.57382554315626));
#161067=CARTESIAN_POINT('Ctrl Pts',(-6.18970224440444,0.940053947,-4.23620981689925));
#161068=CARTESIAN_POINT('Ctrl Pts',(-6.19769376537438,0.94231013198918,
-4.22453307341324));
#161069=CARTESIAN_POINT('Ctrl Pts',(-6.20568528634422,0.944566316978359,
-4.21285632992723));
#161070=CARTESIAN_POINT('Ctrl Pts',(-5.654270243,0.809162772000001,-4.537810928));
#161071=CARTESIAN_POINT('Ctrl Pts',(-5.90178398,0.874819703,-4.229400204));
#161072=CARTESIAN_POINT('Ctrl Pts',(-6.114284746,0.940053947,-3.895898106));
#161073=CARTESIAN_POINT('Ctrl Pts',(-6.12163427607869,0.942310131989179,
-3.88436363604635));
#161074=CARTESIAN_POINT('Ctrl Pts',(-6.12898380615742,0.944566316978361,
-3.87282916609264));
#161075=CARTESIAN_POINT('Origin',(0.154334891428051,0.80357731127327,0.125085317688508));
#161076=CARTESIAN_POINT('Ctrl Pts',(-6.453893166,0.940053947,-3.820636465));
#161077=CARTESIAN_POINT('Ctrl Pts',(-6.66228477,0.874398499000001,-3.468617329));
#161078=CARTESIAN_POINT('Ctrl Pts',(-6.831153176,0.809170361000001,-3.096021041));
#161079=CARTESIAN_POINT('Ctrl Pts',(-6.114284746,0.940053947,-3.895898106));
#161080=CARTESIAN_POINT('Ctrl Pts',(-6.326781397,0.874398499000001,-3.562402465));
#161081=CARTESIAN_POINT('Ctrl Pts',(-6.501745184,0.809170361000001,-3.207773304));
#161082=CARTESIAN_POINT('',(-6.49966322680666,0.80994605270483,-3.21198971733521));
#161083=CARTESIAN_POINT('Origin',(0.16695401651229,0.946423774500962,0.107665247463179));
#161084=CARTESIAN_POINT('Ctrl Pts',(-6.72354450891877,0.849330499373838,
-3.32324378223985));
#161085=CARTESIAN_POINT('Ctrl Pts',(-6.68617749493505,0.843074445191609,
-3.30471905299559));
#161086=CARTESIAN_POINT('Ctrl Pts',(-6.64881815156924,0.83666922520071,
-3.28617746743303));
#161087=CARTESIAN_POINT('Ctrl Pts',(-6.57420250684033,0.823551550405508,
-3.24909996596334));
#161088=CARTESIAN_POINT('Ctrl Pts',(-6.53690444003405,0.816831759514636,
-3.23054329983008));
#161089=CARTESIAN_POINT('Ctrl Pts',(-6.49966322605802,0.809946053424266,
-3.21198971904584));
#161090=CARTESIAN_POINT('Ctrl Pts',(-6.60912646082584,0.809162772000001,
-3.54645385105304));
#161091=CARTESIAN_POINT('Ctrl Pts',(-6.8025668788176,0.874819703,-3.18596073831698));
#161092=CARTESIAN_POINT('Ctrl Pts',(-6.95565033526458,0.940053947,-2.80656656937156));
#161093=CARTESIAN_POINT('Ctrl Pts',(-6.96094486404493,0.942310131896384,
-2.79344488141654));
#161094=CARTESIAN_POINT('Ctrl Pts',(-6.96623939282528,0.944566316792772,
-2.78032319346146));
#161095=CARTESIAN_POINT('Ctrl Pts',(-6.49757176,0.809162772000001,-3.216218467));
#161096=CARTESIAN_POINT('Ctrl Pts',(-6.672999573,0.874819703,-2.861810077));
#161097=CARTESIAN_POINT('Ctrl Pts',(-6.808839097,0.940053947,-2.49042369));
#161098=CARTESIAN_POINT('Ctrl Pts',(-6.81353722889499,0.942310131896384,
-2.47757895837298));
#161099=CARTESIAN_POINT('Ctrl Pts',(-6.81823536078983,0.94456631679277,
-2.46473422674598));
#161100=CARTESIAN_POINT('Origin',(0.177616129434592,0.803577343094904,0.0889833830637288));
#161101=CARTESIAN_POINT('Ctrl Pts',(-7.124328633,0.940053947,-2.343915853));
#161102=CARTESIAN_POINT('Ctrl Pts',(-7.252174449,0.874398499000001,-1.955328694));
#161103=CARTESIAN_POINT('Ctrl Pts',(-7.336997617,0.809170361000001,-1.555141784));
#161104=CARTESIAN_POINT('Ctrl Pts',(-6.808839097,0.940053947,-2.49042369));
#161105=CARTESIAN_POINT('Ctrl Pts',(-6.94467599,0.874398499000001,-2.119044493));
#161106=CARTESIAN_POINT('Ctrl Pts',(-7.039314433,0.809170361000001,-1.735094322));
#161107=CARTESIAN_POINT('',(-7.03818755630073,0.809946052706088,-1.73965971724958));
#161108=CARTESIAN_POINT('Origin',(0.186195892311229,0.946423873731715,0.0692580378799948));
#161109=CARTESIAN_POINT('Ctrl Pts',(-7.28075095342902,0.849330499377566,
-1.80018486679473));
#161110=CARTESIAN_POINT('Ctrl Pts',(-7.24027528502148,0.843074444394666,
-1.79012603746491));
#161111=CARTESIAN_POINT('Ctrl Pts',(-7.19980349267496,0.836669224887264,
-1.78004909903632));
#161112=CARTESIAN_POINT('Ctrl Pts',(-7.11896175544258,0.823551550465569,
-1.75987860727529));
#161113=CARTESIAN_POINT('Ctrl Pts',(-7.07854656259585,0.81683175970302,
-1.74977376760367));
#161114=CARTESIAN_POINT('Ctrl Pts',(-7.03818755564693,0.809946053586523,
-1.73965971925911));
#161115=CARTESIAN_POINT('Ctrl Pts',(-7.21699150217467,0.809162772,-2.04277290610175));
#161116=CARTESIAN_POINT('Ctrl Pts',(-7.32841402766746,0.874819703,-1.64912395008306));
#161117=CARTESIAN_POINT('Ctrl Pts',(-7.39635994642254,0.940053947,-1.24569138826099));
#161118=CARTESIAN_POINT('Ctrl Pts',(-7.3987099168532,0.942310131731566,
-1.23173831192582));
#161119=CARTESIAN_POINT('Ctrl Pts',(-7.40105988728378,0.944566316463135,
-1.21778523559063));
#161120=CARTESIAN_POINT('Ctrl Pts',(-7.037054042,0.809162772000001,-1.744239205));
#161121=CARTESIAN_POINT('Ctrl Pts',(-7.132193124,0.874819703,-1.360404892));
#161122=CARTESIAN_POINT('Ctrl Pts',(-7.185019699,0.940053947,-0.96849983));
#161123=CARTESIAN_POINT('Ctrl Pts',(-7.18684675339088,0.942310131731566,
-0.954945442566497));
#161124=CARTESIAN_POINT('Ctrl Pts',(-7.18867380778176,0.944566316463134,
-0.941391055132988));
#161125=CARTESIAN_POINT('Origin',(0.192592437819522,0.80357736821388,0.0487207840258531));
#161126=CARTESIAN_POINT('Ctrl Pts',(-7.461638412,0.940053947,-0.75759634));
#161127=CARTESIAN_POINT('Ctrl Pts',(-7.50296051,0.874398499000001,-0.350611062));
#161128=CARTESIAN_POINT('Ctrl Pts',(-7.499772204,0.809170361000001,0.058454175));
#161129=CARTESIAN_POINT('Ctrl Pts',(-7.18501969900001,0.940053947,-0.96849983));
#161130=CARTESIAN_POINT('Ctrl Pts',(-7.237845252,0.874398499000001,-0.576602356));
#161131=CARTESIAN_POINT('Ctrl Pts',(-7.247733164,0.809170361000001,-0.181284259));
#161132=CARTESIAN_POINT('',(-7.247614058022,0.809946052668477,-0.185985163060946));
#161133=CARTESIAN_POINT('Origin',(0.196730823848642,0.946423822056388,0.0276121826915415));
#161134=CARTESIAN_POINT('Ctrl Pts',(-7.49751757546059,0.84933049942428,
-0.192951307212126));
#161135=CARTESIAN_POINT('Ctrl Pts',(-7.45582586103834,0.84307444538524,
-0.191828720249307));
#161136=CARTESIAN_POINT('Ctrl Pts',(-7.41413402924456,0.836669225354686,
-0.190687614096639));
#161137=CARTESIAN_POINT('Ctrl Pts',(-7.33084626478269,0.823551550492759,
-0.188367281286457));
#161138=CARTESIAN_POINT('Ctrl Pts',(-7.28920371489587,0.816831759718861,
-0.187186759113356));
#161139=CARTESIAN_POINT('Ctrl Pts',(-7.24761405780495,0.809946053597453,
-0.185985165250054));
#161140=CARTESIAN_POINT('Ctrl Pts',(-7.48739804276063,0.809162772000001,
-0.443574171164248));
#161141=CARTESIAN_POINT('Ctrl Pts',(-7.51159268225307,0.874819703,-0.0351759592752993));
#161142=CARTESIAN_POINT('Ctrl Pts',(-7.49122398729508,0.940053947,0.373430937495418));
#161143=CARTESIAN_POINT('Ctrl Pts',(-7.49051951773755,0.942310131753154,
0.387562972972483));
#161144=CARTESIAN_POINT('Ctrl Pts',(-7.48981504818013,0.944566316506309,
0.401695008449552));
#161145=CARTESIAN_POINT('Ctrl Pts',(-7.24749149900001,0.809162772000001,
-0.190701257));
#161146=CARTESIAN_POINT('Ctrl Pts',(-7.25789325,0.874819703,0.204611314));
#161147=CARTESIAN_POINT('Ctrl Pts',(-7.225236766,0.940053947,0.598710006));
#161148=CARTESIAN_POINT('Ctrl Pts',(-7.22410731225338,0.942310131753154,
0.612340262221383));
#161149=CARTESIAN_POINT('Ctrl Pts',(-7.22297785850692,0.944566316506312,
0.625970518442767));
#161150=CARTESIAN_POINT('Origin',(0.198563202851664,0.80357734792354,0.00618004660839541));
#161151=CARTESIAN_POINT('Ctrl Pts',(-7.450050271,0.940053947,0.864147535));
#161152=CARTESIAN_POINT('Ctrl Pts',(-7.402916477,0.874398499000001,1.270500754));
#161153=CARTESIAN_POINT('Ctrl Pts',(-7.311865778,0.809170361000001,1.669316881));
#161154=CARTESIAN_POINT('Ctrl Pts',(-7.225236766,0.940053947,0.598710006));
#161155=CARTESIAN_POINT('Ctrl Pts',(-7.192580914,0.874398499000001,0.992801067));
#161156=CARTESIAN_POINT('Ctrl Pts',(-7.11725594700001,0.809170361000001,
1.381002455));
#161157=CARTESIAN_POINT('',(-7.11815018152856,0.809946052682178,1.3763858514358));
#161158=CARTESIAN_POINT('Origin',(0.19806736417516,0.946423835782391,-0.0153247141242421));
#161159=CARTESIAN_POINT('Ctrl Pts',(-7.36370860838713,0.849330499437629,
1.42330444072714));
#161160=CARTESIAN_POINT('Ctrl Pts',(-7.32275029711717,0.843074444948691,
1.41543829550887));
#161161=CARTESIAN_POINT('Ctrl Pts',(-7.28178789480018,0.836669225164592,
1.40759021220572));
#161162=CARTESIAN_POINT('Ctrl Pts',(-7.19994855029583,0.823551550483622,
1.39195189002707));
#161163=CARTESIAN_POINT('Ctrl Pts',(-7.15902580303483,0.81683175974397,
1.38415289520237));
#161164=CARTESIAN_POINT('Ctrl Pts',(-7.11815018169161,0.809946053567181,
1.37638584979312));
#161165=CARTESIAN_POINT('Ctrl Pts',(-7.40770217163706,0.809162772000001,
1.17636559945578));
#161166=CARTESIAN_POINT('Ctrl Pts',(-7.34353761129164,0.874819703,1.58041682072337));
#161167=CARTESIAN_POINT('Ctrl Pts',(-7.23580672022556,0.940053947,1.97509204848353));
#161168=CARTESIAN_POINT('Ctrl Pts',(-7.23208075077751,0.942310131811108,
1.98874224506117));
#161169=CARTESIAN_POINT('Ctrl Pts',(-7.22835478132945,0.944566316622219,
2.00239244163875));
#161170=CARTESIAN_POINT('Ctrl Pts',(-7.11904430900001,0.809162772000001,
1.371753671));
#161171=CARTESIAN_POINT('Ctrl Pts',(-7.044222355,0.874819703,1.760060122));
#161172=CARTESIAN_POINT('Ctrl Pts',(-6.927609792,0.940053947,2.137924827));
#161173=CARTESIAN_POINT('Ctrl Pts',(-6.92357664196574,0.942310131811108,
2.15099361657736));
#161174=CARTESIAN_POINT('Ctrl Pts',(-6.91954349193137,0.944566316622219,
2.1640624061548));
#161175=CARTESIAN_POINT('Origin',(0.195249511379292,0.803577352408136,-0.0366496854475287));
#161176=CARTESIAN_POINT('Ctrl Pts',(-7.090106059,0.940053947,2.445484832));
#161177=CARTESIAN_POINT('Ctrl Pts',(-6.95672029700001,0.874398499000001,
2.832205366));
#161178=CARTESIAN_POINT('Ctrl Pts',(-6.782064634,0.809170361000001,3.202124185));
#161179=CARTESIAN_POINT('Ctrl Pts',(-6.927609792,0.940053947,2.137924827));
#161180=CARTESIAN_POINT('Ctrl Pts',(-6.810999487,0.874398499000001,2.515782215));
#161181=CARTESIAN_POINT('Ctrl Pts',(-6.653983753,0.809170361000001,2.87871503));
#161182=CARTESIAN_POINT('',(-6.655849513603,0.809946052668528,2.8743985932961));
#161183=CARTESIAN_POINT('Origin',(0.190142419849683,0.946423866384608,-0.0575450923149956));
#161184=CARTESIAN_POINT('Ctrl Pts',(-6.885580810478,0.849330499379893,2.97300805530621));
#161185=CARTESIAN_POINT('Ctrl Pts',(-6.84727107633071,0.843074445841034,
2.9565209924128));
#161186=CARTESIAN_POINT('Ctrl Pts',(-6.80895345511024,0.83666922557787,
2.940050685833));
#161187=CARTESIAN_POINT('Ctrl Pts',(-6.73238924394341,0.823551550535741,
2.90718493774205));
#161188=CARTESIAN_POINT('Ctrl Pts',(-6.694099800825,0.816831759741263,2.89077109770459));
#161189=CARTESIAN_POINT('Ctrl Pts',(-6.65584951439853,0.809946053640974,
2.87439859102855));
#161190=CARTESIAN_POINT('Ctrl Pts',(-6.9816303808209,0.809162772000001,
2.74129982289529));
#161191=CARTESIAN_POINT('Ctrl Pts',(-6.83210688278208,0.874819703,3.12211106708376));
#161192=CARTESIAN_POINT('Ctrl Pts',(-6.64205117335252,0.940053947,3.48440004939027));
#161193=CARTESIAN_POINT('Ctrl Pts',(-6.63547792639119,0.942310131765159,
3.4969301383795));
#161194=CARTESIAN_POINT('Ctrl Pts',(-6.62890467942987,0.944566316530321,
3.50946022736874));
#161195=CARTESIAN_POINT('Ctrl Pts',(-6.657718518,0.809162772000001,2.870066921));
#161196=CARTESIAN_POINT('Ctrl Pts',(-6.501171452,0.874819703,3.233210475));
#161197=CARTESIAN_POINT('Ctrl Pts',(-6.306055484,0.940053947,3.577172659));
#161198=CARTESIAN_POINT('Ctrl Pts',(-6.29930722346308,0.942310131765159,
3.58906889925277));
#161199=CARTESIAN_POINT('Ctrl Pts',(-6.2925589629262,0.944566316530321,
3.60096513950554));
#161200=CARTESIAN_POINT('Origin',(0.182806037430469,0.803577345213135,-0.077765686486444));
#161201=CARTESIAN_POINT('Ctrl Pts',(-6.398636369,0.940053947,3.912473977));
#161202=CARTESIAN_POINT('Ctrl Pts',(-6.185235608,0.874398499000001,4.261479203));
#161203=CARTESIAN_POINT('Ctrl Pts',(-5.935141687,0.809170361000001,4.585203721));
#161204=CARTESIAN_POINT('Ctrl Pts',(-6.306055484,0.940053947,3.577172659));
#161205=CARTESIAN_POINT('Ctrl Pts',(-6.110943294,0.874398499000001,3.921128183));
#161206=CARTESIAN_POINT('Ctrl Pts',(-5.879578673,0.809170361000001,4.241822088));
#161207=CARTESIAN_POINT('',(-5.88232871960182,0.809946052669728,4.23800765141649));
#161208=CARTESIAN_POINT('Origin',(0.173326479965217,0.946423872780383,-0.0970747065690575));
#161209=CARTESIAN_POINT('Ctrl Pts',(-6.0854909077331,0.8493304994229,4.38369711687508));
#161210=CARTESIAN_POINT('Ctrl Pts',(-6.05162106171033,0.843074445266074,
4.35936004959652));
#161211=CARTESIAN_POINT('Ctrl Pts',(-6.01773991588643,0.836669225298237,
4.33503765500536));
#161212=CARTESIAN_POINT('Ctrl Pts',(-5.95003089877634,0.82355155048126,
4.28648124866588));
#161213=CARTESIAN_POINT('Ctrl Pts',(-5.91616513215529,0.816831759747061,
4.26222005696166));
#161214=CARTESIAN_POINT('Ctrl Pts',(-5.8823287207792,0.809946053616843,
4.23800764950177));
#161215=CARTESIAN_POINT('Ctrl Pts',(-6.2291053126731,0.809162772000001,
4.17805391238259));
#161216=CARTESIAN_POINT('Ctrl Pts',(-6.00121443024314,0.874819703,4.51781886922408));
#161217=CARTESIAN_POINT('Ctrl Pts',(-5.73772069546419,0.940053947,4.83078137711899));
#161218=CARTESIAN_POINT('Ctrl Pts',(-5.72860752855345,0.942310131779373,
4.84160546587255));
#161219=CARTESIAN_POINT('Ctrl Pts',(-5.71949436164269,0.944566316558748,
4.85242955462612));
#161220=CARTESIAN_POINT('Ctrl Pts',(-5.88508521,0.809162772000001,4.234179032));
#161221=CARTESIAN_POINT('Ctrl Pts',(-5.65413299700001,0.874819703,4.5551795));
#161222=CARTESIAN_POINT('Ctrl Pts',(-5.38963702999999,0.940053947,4.849155874));
#161223=CARTESIAN_POINT('Ctrl Pts',(-5.38048919998988,0.942310131779373,
4.85932331030102));
#161224=CARTESIAN_POINT('Ctrl Pts',(-5.37134136997988,0.944566316558748,
4.86949074660191));
#161225=CARTESIAN_POINT('Origin',(0.161815073416527,0.803577351637582,-0.115245659545124));
#161226=CARTESIAN_POINT('Ctrl Pts',(-5.407973553,0.940053947,5.196520186));
#161227=CARTESIAN_POINT('Ctrl Pts',(-5.124536177,0.874398499000001,5.491491009));
#161228=CARTESIAN_POINT('Ctrl Pts',(-4.81069811,0.809170361000001,5.753884227));
#161229=CARTESIAN_POINT('Ctrl Pts',(-5.38963703,0.940053947,4.849155874));
#161230=CARTESIAN_POINT('Ctrl Pts',(-5.125146184,0.874398499000001,5.143126555));
#161231=CARTESIAN_POINT('Ctrl Pts',(-4.830251029,0.809170361000001,5.406586261));
#161232=CARTESIAN_POINT('',(-4.83375677212873,0.809946052702061,5.40345218124008));
#161233=CARTESIAN_POINT('Origin',(0.148405984167564,0.946423872553155,-0.132065222751626));
#161234=CARTESIAN_POINT('Ctrl Pts',(-5.00085021302196,0.849330499383347,
5.58940937375437));
#161235=CARTESIAN_POINT('Ctrl Pts',(-4.9730039753034,0.84307444525625,5.55836027797521));
#161236=CARTESIAN_POINT('Ctrl Pts',(-4.94514354752411,0.836669225265375,
5.52732308242854));
#161237=CARTESIAN_POINT('Ctrl Pts',(-4.88945572164077,0.823551550481411,
5.46534646060306));
#161238=CARTESIAN_POINT('Ctrl Pts',(-4.86159715640179,0.816831759647414,
5.43437234271068));
#161239=CARTESIAN_POINT('Ctrl Pts',(-4.83375677361857,0.809946053577941,
5.40345217970358));
#161240=CARTESIAN_POINT('Ctrl Pts',(-5.1853142030829,0.809162772,5.4194468453736));
#161241=CARTESIAN_POINT('Ctrl Pts',(-4.88971186043539,0.874819703,5.7022784826116));
#161242=CARTESIAN_POINT('Ctrl Pts',(-4.56510077445979,0.940053947,5.95128073642129));
#161243=CARTESIAN_POINT('Ctrl Pts',(-4.55387380829232,0.942310131960985,
5.95989270317139));
#161244=CARTESIAN_POINT('Ctrl Pts',(-4.54264684212497,0.944566316921971,
5.96850466992152));
#161245=CARTESIAN_POINT('Ctrl Pts',(-4.837271857,0.809162772000001,5.400305637));
#161246=CARTESIAN_POINT('Ctrl Pts',(-4.54271356700001,0.874819703,5.664153394));
#161247=CARTESIAN_POINT('Ctrl Pts',(-4.221205138,0.940053947,5.894397949));
#161248=CARTESIAN_POINT('Ctrl Pts',(-4.21008548001271,0.942310131960985,
5.90236116387744));
#161249=CARTESIAN_POINT('Ctrl Pts',(-4.19896582202542,0.944566316921971,
5.91032437875497));
#161250=CARTESIAN_POINT('Origin',(0.133257403895742,0.803577328187921,-0.147336580872585));
#161251=CARTESIAN_POINT('Ctrl Pts',(-4.164439905,0.940053947,6.237582888));
#161252=CARTESIAN_POINT('Ctrl Pts',(-3.824219129,0.874398499000001,6.464726799));
#161253=CARTESIAN_POINT('Ctrl Pts',(-3.461311636,0.809170361000001,6.653519501));
#161254=CARTESIAN_POINT('Ctrl Pts',(-4.221205138,0.940053947,5.894397949));
#161255=CARTESIAN_POINT('Ctrl Pts',(-3.899702935,0.874398499000001,6.124638046));
#161256=CARTESIAN_POINT('Ctrl Pts',(-3.555066216,0.809170361000001,6.318544469));
#161257=CARTESIAN_POINT('',(-3.55916373151898,0.809946052669262,6.31623729403005));
#161258=CARTESIAN_POINT('Origin',(0.116546246060481,0.946423908382474,-0.160880525506759));
#161259=CARTESIAN_POINT('Ctrl Pts',(-3.68237532007637,0.849330499360679,
6.53376706035624));
#161260=CARTESIAN_POINT('Ctrl Pts',(-3.66185475181377,0.84307444585648,
6.49745776082882));
#161261=CARTESIAN_POINT('Ctrl Pts',(-3.64131776402704,0.836669225572331,
6.46115702750206));
#161262=CARTESIAN_POINT('Ctrl Pts',(-3.60025502958651,0.82355155050574,
6.38865814675778));
#161263=CARTESIAN_POINT('Ctrl Pts',(-3.57970630226656,0.816831759753065,
6.35241941900083));
#161264=CARTESIAN_POINT('Ctrl Pts',(-3.55916373330938,0.809946053662904,
6.31623729282445));
#161265=CARTESIAN_POINT('Ctrl Pts',(-3.89906356435541,0.809162772,6.40743246670616));
#161266=CARTESIAN_POINT('Ctrl Pts',(-3.54957179938179,0.874819703,6.62010589188594));
#161267=CARTESIAN_POINT('Ctrl Pts',(-3.17902181502426,0.940053947,6.79350482401382));
#161268=CARTESIAN_POINT('Ctrl Pts',(-3.16620601068798,0.942310131974825,
6.79950198196843));
#161269=CARTESIAN_POINT('Ctrl Pts',(-3.15339020635174,0.94456631694965,
6.80549913992302));
#161270=CARTESIAN_POINT('Ctrl Pts',(-3.563273049,0.809162772000001,6.313919953));
#161271=CARTESIAN_POINT('Ctrl Pts',(-3.2188819,0.874819703,6.508277771));
#161272=CARTESIAN_POINT('Ctrl Pts',(-2.855394386,0.940053947,6.664024527));
#161273=CARTESIAN_POINT('Ctrl Pts',(-2.84282284355026,0.942310131974825,
6.66941116857376));
#161274=CARTESIAN_POINT('Ctrl Pts',(-2.83025130110046,0.944566316949653,
6.67479781014762));
#161275=CARTESIAN_POINT('Origin',(0.0984688995454319,0.803577314516454,
-0.172538347558309));
#161276=CARTESIAN_POINT('Ctrl Pts',(-2.726181675,0.940053947,6.986983146));
#161277=CARTESIAN_POINT('Ctrl Pts',(-2.345085845,0.874398499000001,7.135679149));
#161278=CARTESIAN_POINT('Ctrl Pts',(-1.950078078,0.809170361000001,7.24204359900001));
#161279=CARTESIAN_POINT('Ctrl Pts',(-2.855394386,0.940053947,6.664024527));
#161280=CARTESIAN_POINT('Ctrl Pts',(-2.491913911,0.874398499000001,6.819768268));
#161281=CARTESIAN_POINT('Ctrl Pts',(-2.113650457,0.809170361000001,6.93505456));
#161282=CARTESIAN_POINT('',(-2.11814814972717,0.809946052719587,6.93368216984298));
#161283=CARTESIAN_POINT('Origin',(0.0792368644578836,0.946423905641289,
-0.182173114611933));
#161284=CARTESIAN_POINT('Ctrl Pts',(-2.19171665082089,0.849330499388496,
7.17261306095222));
#161285=CARTESIAN_POINT('Ctrl Pts',(-2.17948126560287,0.843074444602531,
7.13274132886931));
#161286=CARTESIAN_POINT('Ctrl Pts',(-2.16722800712273,0.836669224998938,
7.09287444566833));
#161287=CARTESIAN_POINT('Ctrl Pts',(-2.14271041383307,0.82355155055306,
7.0132432779999));
#161288=CARTESIAN_POINT('Ctrl Pts',(-2.13043235937359,0.816831759769418,
6.97343442234686));
#161289=CARTESIAN_POINT('Ctrl Pts',(-2.11814815162338,0.809946053689787,
6.93368216908896));
#161290=CARTESIAN_POINT('Ctrl Pts',(-2.43049704742019,0.809162772000001,
7.0958136667112));
#161291=CARTESIAN_POINT('Ctrl Pts',(-2.04345770500201,0.874819703,7.22838450695476));
#161292=CARTESIAN_POINT('Ctrl Pts',(-1.64429532972973,0.940053947,7.3180721746251));
#161293=CARTESIAN_POINT('Ctrl Pts',(-1.63048994008922,0.94231013198164,
7.32117410325077));
#161294=CARTESIAN_POINT('Ctrl Pts',(-1.61668455044872,0.944566316963281,
7.32427603187633));
#161295=CARTESIAN_POINT('Ctrl Pts',(-2.122659554,0.809162772000001,6.932302389));
#161296=CARTESIAN_POINT('Ctrl Pts',(-1.744538893,0.874819703,7.04808231200001));
#161297=CARTESIAN_POINT('Ctrl Pts',(-1.356068566,0.940053947,7.122048725));
#161298=CARTESIAN_POINT('Ctrl Pts',(-1.34263297046233,0.942310131981639,
7.1246069198977));
#161299=CARTESIAN_POINT('Ctrl Pts',(-1.32919737492467,0.94456631696328,
7.12716511479539));
#161300=CARTESIAN_POINT('Origin',(0.0590761169157883,0.803577364487472,
-0.189672464537588));
#161301=CARTESIAN_POINT('Ctrl Pts',(-1.16045022,0.940053947,7.409679837));
#161302=CARTESIAN_POINT('Ctrl Pts',(-0.756298953000001,0.874398499000001,
7.47297507200001));
#161303=CARTESIAN_POINT('Ctrl Pts',(-0.347661035,0.809170361000001,7.491937787));
#161304=CARTESIAN_POINT('Ctrl Pts',(-1.356068566,0.940053947,7.122048725));
#161305=CARTESIAN_POINT('Ctrl Pts',(-0.967605761,0.874398499000001,7.196013706));
#161306=CARTESIAN_POINT('Ctrl Pts',(-0.573402753,0.809170361000001,7.227289207));
#161307=CARTESIAN_POINT('',(-0.578090314703847,0.809946052713699,7.22691577389676));
#161308=CARTESIAN_POINT('Origin',(0.0382225075640378,0.946423838787555,
-0.194947625922174));
#161309=CARTESIAN_POINT('Ctrl Pts',(-0.598575746204804,0.849330499425487,
7.47607564640176));
#161310=CARTESIAN_POINT('Ctrl Pts',(-0.595197661092526,0.843074444324486,
7.43450584510454));
#161311=CARTESIAN_POINT('Ctrl Pts',(-0.591801078470085,0.83666922486761,
7.39293694026594));
#161312=CARTESIAN_POINT('Ctrl Pts',(-0.584975040072362,0.823551550502395,
7.30989694812043));
#161313=CARTESIAN_POINT('Ctrl Pts',(-0.581541766932348,0.816831759718931,
7.26837938286832));
#161314=CARTESIAN_POINT('Ctrl Pts',(-0.578090316529954,0.809946053577953,
7.22691577360123));
#161315=CARTESIAN_POINT('Ctrl Pts',(-0.848283189425136,0.809162772000001,
7.45240250623194));
#161316=CARTESIAN_POINT('Ctrl Pts',(-0.441793800398221,0.874819703,7.49867189599368));
#161317=CARTESIAN_POINT('Ctrl Pts',(-0.032683421404803,0.940053947,7.50045460502934));
#161318=CARTESIAN_POINT('Ctrl Pts',(-0.0185339724271852,0.942310131771804,
7.50051626161846));
#161319=CARTESIAN_POINT('Ctrl Pts',(-0.00438452344956661,0.944566316543609,
7.50057791820755));
#161320=CARTESIAN_POINT('Ctrl Pts',(-0.582792857,0.809162772000001,7.226538071));
#161321=CARTESIAN_POINT('Ctrl Pts',(-0.188623186,0.874819703,7.25832635800001));
#161322=CARTESIAN_POINT('Ctrl Pts',(0.206665513,0.940053947,7.24705384000001));
#161323=CARTESIAN_POINT('Ctrl Pts',(0.220336926792266,0.942310131771804,
7.24666396986597));
#161324=CARTESIAN_POINT('Ctrl Pts',(0.234008340584527,0.944566316543609,
7.24627409973195));
#161325=CARTESIAN_POINT('Origin',(0.0169207711628139,0.803576816201109,
-0.197933668297665));
#161326=CARTESIAN_POINT('Ctrl Pts',(0.201949703,0.940837228,7.247186786));
#161327=CARTESIAN_POINT('Ctrl Pts',(0.597245653,0.875180297,7.236171492));
#161328=CARTESIAN_POINT('Ctrl Pts',(0.988998379000001,0.809946053,7.182226828));
#161329=CARTESIAN_POINT('Ctrl Pts',(1.0025474970505,0.807689868386007,7.18036110359729));
#161330=CARTESIAN_POINT('Ctrl Pts',(1.016096615101,0.805433683772012,7.17849537919455));
#161331=CARTESIAN_POINT('Ctrl Pts',(-0.0375640730680385,0.940837228,7.50043175004996));
#161332=CARTESIAN_POINT('Ctrl Pts',(0.371545059364261,0.875180297,7.50248067266357));
#161333=CARTESIAN_POINT('Ctrl Pts',(0.778449959968396,0.809946053,7.46002031822874));
#161334=CARTESIAN_POINT('Ctrl Pts',(0.792523129515691,0.807689868386006,
7.45855178893327));
#161335=CARTESIAN_POINT('Ctrl Pts',(0.806596299062982,0.805433683772012,
7.45708325963789));
#161336=CARTESIAN_POINT('',(0.213239091069717,0.900669500237862,7.49696799323959));
#161337=CARTESIAN_POINT('',(0.778885076486235,0.809946052263419,7.4594462526428));
#161338=CARTESIAN_POINT('Origin',(0.0019124482713892,0.946416032070669,
-0.191459090284092));
#161339=CARTESIAN_POINT('',(0.883941732031841,0.809946053334084,7.32083652775467));
#161340=CARTESIAN_POINT('Ctrl Pts',(0.213239091291757,0.900669500620797,
7.49696799318031));
#161341=CARTESIAN_POINT('Ctrl Pts',(0.212102887926396,0.90692555462208,
7.45527664792096));
#161342=CARTESIAN_POINT('Ctrl Pts',(0.210985170232026,0.913330774802257,
7.41358418156647));
#161343=CARTESIAN_POINT('Ctrl Pts',(0.208792991462068,0.926448449729418,
7.3302929450039));
#161344=CARTESIAN_POINT('Ctrl Pts',(0.207717300174009,0.933168240538447,
7.28864755498878));
#161345=CARTESIAN_POINT('Ctrl Pts',(0.206665513330684,0.940053946543812,
7.24705384020173));
#161346=CARTESIAN_POINT('Ctrl Pts',(0.988998379000001,0.809946053,7.182226828));
#161347=CARTESIAN_POINT('Ctrl Pts',(1.380743519,0.875601501,7.128283209));
#161348=CARTESIAN_POINT('Ctrl Pts',(1.764297565,0.940829639,7.032051913));
#161349=CARTESIAN_POINT('Ctrl Pts',(1.266217779,0.809946053,7.392340126));
#161350=CARTESIAN_POINT('Ctrl Pts',(1.669423273,0.875601501,7.323275938));
#161351=CARTESIAN_POINT('Ctrl Pts',(2.062725117,0.940829639,7.210767303));
#161352=CARTESIAN_POINT('',(1.26621779070058,0.809946052007887,7.39234012253307));
#161353=CARTESIAN_POINT('',(1.81988019092492,0.90066950060491,7.27585294567191));
#161354=CARTESIAN_POINT('Origin',(-0.0314977611305134,0.803573282467146,
-0.190000801682366));
#161355=CARTESIAN_POINT('Ctrl Pts',(1.75973614606893,0.940053944097848,
7.03319478750167));
#161356=CARTESIAN_POINT('Ctrl Pts',(1.76970476259936,0.933168237615819,
7.07358996388049));
#161357=CARTESIAN_POINT('Ctrl Pts',(1.77970782974647,0.926448448759319,
7.11403045415623));
#161358=CARTESIAN_POINT('Ctrl Pts',(1.79975390956644,0.913330774361959,
7.19490313090962));
#161359=CARTESIAN_POINT('Ctrl Pts',(1.80980814175334,0.906925555236439,
7.23538056739943));
#161360=CARTESIAN_POINT('Ctrl Pts',(1.81988018914809,0.900669500605544,
7.27585294611419));
#161361=CARTESIAN_POINT('',(1.12760809690174,0.809946050061996,7.28728347422995));
#161362=CARTESIAN_POINT('Origin',(3.62231945827407E-13,0.714028547999755,
1.57773100140091E-12));
#161363=CARTESIAN_POINT('',(2.00688844721255,0.749999999457025,7.22650665628683));
#161364=CARTESIAN_POINT('',(1.81501009314308,0.714243089266212,7.24021154783803));
#161365=CARTESIAN_POINT('Origin',(1.418460290385,0.473618757495434,-0.336301876236789));
#161366=CARTESIAN_POINT('',(1.6362104624896,0.750000000179527,7.31934527981378));
#161367=CARTESIAN_POINT('Origin',(0.,0.750000000000029,0.));
#161368=CARTESIAN_POINT('Origin',(-1.44669394436553,0.692075205405702,0.130173868264863));
#161369=CARTESIAN_POINT('Ctrl Pts',(1.755159165,0.940837228,7.03433837));
#161370=CARTESIAN_POINT('Ctrl Pts',(2.138845352,0.875180297,6.938603662));
#161371=CARTESIAN_POINT('Ctrl Pts',(2.509842609,0.809946053,6.801704939));
#161372=CARTESIAN_POINT('Ctrl Pts',(2.52267388045516,0.807689868413341,
6.79697017440664));
#161373=CARTESIAN_POINT('Ctrl Pts',(2.53550515191036,0.80543368382668,6.79223540981329));
#161374=CARTESIAN_POINT('Ctrl Pts',(1.57568526882813,0.940837228000001,
7.33315098851839));
#161375=CARTESIAN_POINT('Ctrl Pts',(1.97567011476546,0.875180297,7.2472056382825));
#161376=CARTESIAN_POINT('Ctrl Pts',(2.36393408428999,0.809946053,7.11826545847073));
#161377=CARTESIAN_POINT('Ctrl Pts',(2.37736254041797,0.807689868413341,
7.11380594720096));
#161378=CARTESIAN_POINT('Ctrl Pts',(2.39079099654594,0.80543368382668,7.10934643593125));
#161379=CARTESIAN_POINT('',(2.36423562280412,0.809946052264267,7.11761127582573));
#161380=CARTESIAN_POINT('Origin',(-0.0392902992667366,0.94641605726145,
-0.187394038683174));
#161381=CARTESIAN_POINT('',(2.43703911643165,0.809946053334091,6.9596580948236));
#161382=CARTESIAN_POINT('Origin',(1.50704101975485E-14,0.901573517999972,
-2.42861286636753E-14));
#161383=CARTESIAN_POINT('Origin',(-0.0598766578396351,0.803569475455572,
-0.183507600577532));
#161384=CARTESIAN_POINT('Origin',(-0.0100119907423271,0.946349155189795,
-0.187382485778542));
#161385=CARTESIAN_POINT('Ctrl Pts',(2.509842609,0.809946053,6.801704939));
#161386=CARTESIAN_POINT('Ctrl Pts',(2.880832682,0.875601501,6.66480886600001));
#161387=CARTESIAN_POINT('Ctrl Pts',(3.234732564,0.940829639,6.488374622));
#161388=CARTESIAN_POINT('Ctrl Pts',(2.825748922,0.809946053,6.947311928));
#161389=CARTESIAN_POINT('Ctrl Pts',(3.204680937,0.875601501,6.79318516));
#161390=CARTESIAN_POINT('Ctrl Pts',(3.564601571,0.940829639,6.598758644));
#161391=CARTESIAN_POINT('',(2.82574893270958,0.809946052007888,6.94731192209775));
#161392=CARTESIAN_POINT('',(3.34142571447524,0.900669500630793,6.7145271012109));
#161393=CARTESIAN_POINT('Origin',(-0.0716058869392666,0.803573306649502,
-0.178787532532706));
#161394=CARTESIAN_POINT('Ctrl Pts',(3.23052347273381,0.940053944111675,
6.49047134690417));
#161395=CARTESIAN_POINT('Ctrl Pts',(3.24894279738607,0.933168237661529,
6.52777914866813));
#161396=CARTESIAN_POINT('Ctrl Pts',(3.26740550839828,0.926448448819339,
6.56512379910516));
#161397=CARTESIAN_POINT('Ctrl Pts',(3.30436815694365,0.913330774448048,
6.63979640314351));
#161398=CARTESIAN_POINT('Ctrl Pts',(3.32288877927613,0.906925555273596,
6.67716613732868));
#161399=CARTESIAN_POINT('Ctrl Pts',(3.34142571288598,0.90066950063885,6.71452710194404));
#161400=CARTESIAN_POINT('',(2.66779578238773,0.809946050061996,6.87450842694637));
#161401=CARTESIAN_POINT('Origin',(-3.44385978068296E-12,0.714028548,-7.08114122893733E-12));
#161402=CARTESIAN_POINT('',(3.51345383299265,0.750000000485261,6.62613325171387));
#161403=CARTESIAN_POINT('',(3.32900763030012,0.714243089209672,6.68076590610822));
#161404=CARTESIAN_POINT('Origin',(1.31300551899894,0.473612695239739,-0.633360103017074));
#161405=CARTESIAN_POINT('',(3.17139964474746,0.750000001078249,6.79648617292802));
#161406=CARTESIAN_POINT('Origin',(0.,0.750000001663587,0.));
#161407=CARTESIAN_POINT('Origin',(-1.38488278791584,0.692074389599663,0.438133504989625));
#161408=CARTESIAN_POINT('Ctrl Pts',(3.226299335,0.940837228,6.49257211000001));
#161409=CARTESIAN_POINT('Ctrl Pts',(3.58043502,0.875180297,6.316594438));
#161410=CARTESIAN_POINT('Ctrl Pts',(3.913329389,0.809946053,6.103142887));
#161411=CARTESIAN_POINT('Ctrl Pts',(3.92484283829835,0.807689868363815,
6.09576047432214));
#161412=CARTESIAN_POINT('Ctrl Pts',(3.93635628759674,0.805433683727629,
6.0883780616443));
#161413=CARTESIAN_POINT('Ctrl Pts',(3.11525731968877,0.940837228,6.82298023806302));
#161414=CARTESIAN_POINT('Ctrl Pts',(3.48741503215394,0.875180297,6.65305932400711));
#161415=CARTESIAN_POINT('Ctrl Pts',(3.83888327807559,0.809946053,6.44366841676578));
#161416=CARTESIAN_POINT('Ctrl Pts',(3.8510391215089,0.807689868363815,6.43642644508177));
#161417=CARTESIAN_POINT('Ctrl Pts',(3.86319496494222,0.805433683727626,
6.42918447339777));
#161418=CARTESIAN_POINT('',(3.83903713685176,0.809946052264257,6.44296470667385));
#161419=CARTESIAN_POINT('Origin',(-0.0786558313566327,0.946416059587553,
-0.17456648136527));
#161420=CARTESIAN_POINT('',(3.87618326074108,0.809946053334091,6.27305378442417));
#161421=CARTESIAN_POINT('Origin',(-3.5301622736128E-13,0.901573518000111,
-7.81926606796546E-13));
#161422=CARTESIAN_POINT('Origin',(-0.0979259484658586,0.803569487859856,
-0.166346363162171));
#161423=CARTESIAN_POINT('Origin',(-0.0500596334563524,0.946349154708691,
-0.180849358721544));
#161424=CARTESIAN_POINT('Ctrl Pts',(3.913329389,0.809946053,6.10314288700001));
#161425=CARTESIAN_POINT('Ctrl Pts',(4.246217311,0.875601501,5.889695469));
#161426=CARTESIAN_POINT('Ctrl Pts',(4.553915063,0.940829639,5.641308146));
#161427=CARTESIAN_POINT('Ctrl Pts',(4.253151186,0.809946053,6.177435146));
#161428=CARTESIAN_POINT('Ctrl Pts',(4.590091282,0.875601501,5.945452595));
#161429=CARTESIAN_POINT('Ctrl Pts',(4.899801218,0.940829639,5.678199365));
#161430=CARTESIAN_POINT('',(4.25315119522186,0.809946052117954,6.17743513791709));
#161431=CARTESIAN_POINT('',(4.706729884842,0.900669500619148,5.83923743243706));
#161432=CARTESIAN_POINT('Origin',(-0.108365671154418,0.803573282975787,
-0.159214253083495));
#161433=CARTESIAN_POINT('Ctrl Pts',(4.55025511129989,0.940053944236844,
5.64426068024899));
#161434=CARTESIAN_POINT('Ctrl Pts',(4.57626387687572,0.933168237793891,
5.67673663592812));
#161435=CARTESIAN_POINT('Ctrl Pts',(4.60232293632015,0.926448448835655,
5.7092392526236));
#161436=CARTESIAN_POINT('Ctrl Pts',(4.65447382124695,0.913330774452229,
5.77422017591404));
#161437=CARTESIAN_POINT('Ctrl Pts',(4.6805948299349,0.90692555527452,5.80673484018321));
#161438=CARTESIAN_POINT('Ctrl Pts',(4.70672988344559,0.900669500619791,
5.83923743356002));
#161439=CARTESIAN_POINT('',(4.08324030258406,0.809946050061996,6.14028900646922));
#161440=CARTESIAN_POINT('Origin',(-6.76672259891653E-12,0.714028548000489,
-8.63588714428154E-12));
#161441=CARTESIAN_POINT('',(4.85573401221774,0.749999999448248,5.7159292241174));
#161442=CARTESIAN_POINT('',(4.6873444694292,0.714243089225114,5.80893507623871));
#161443=CARTESIAN_POINT('Origin',(1.14615087329816,0.473617861364629,-0.900814468059661));
#161444=CARTESIAN_POINT('',(4.55829771058855,0.750000000258868,5.95583092318158));
#161445=CARTESIAN_POINT('Origin',(0.,0.750000000000029,0.));
#161446=CARTESIAN_POINT('Origin',(-1.25832425134463,0.692075148191809,0.725594522822336));
#161447=CARTESIAN_POINT('Ctrl Pts',(4.546581334,0.940837228,5.647220394));
#161448=CARTESIAN_POINT('Ctrl Pts',(4.85460752600001,0.875180297,5.399228277));
#161449=CARTESIAN_POINT('Ctrl Pts',(5.133833235,0.809946053,5.119204656));
#161450=CARTESIAN_POINT('Ctrl Pts',(5.14349050550429,0.807689868414757,
5.10951978899666));
#161451=CARTESIAN_POINT('Ctrl Pts',(5.15314777600842,0.805433683829514,
5.0998349219932));
#161452=CARTESIAN_POINT('Ctrl Pts',(4.50916339980159,0.940837228,5.99377451448312));
#161453=CARTESIAN_POINT('Ctrl Pts',(4.83609229828414,0.875180297,5.74782334933033));
#161454=CARTESIAN_POINT('Ctrl Pts',(5.1343305567691,0.809946053,5.4677726022714));
#161455=CARTESIAN_POINT('Ctrl Pts',(5.14464539327617,0.807689868414757,
5.45808679708906));
#161456=CARTESIAN_POINT('Ctrl Pts',(5.15496022978334,0.805433683829514,
5.44840099190685));
#161457=CARTESIAN_POINT('',(5.13432954268828,0.809946052265052,5.46705226768057));
#161458=CARTESIAN_POINT('Origin',(-0.11434362939921,0.946416045952697,-0.153576652678157));
#161459=CARTESIAN_POINT('',(5.1340813834691,0.809946053334091,5.29312845107504));
#161460=CARTESIAN_POINT('Origin',(6.66133814775094E-13,0.901573517999972,
8.30065183254902E-13));
#161461=CARTESIAN_POINT('Origin',(-0.131395602648939,0.803569504711666,
-0.141405634131786));
#161462=CARTESIAN_POINT('Origin',(-0.0877662100594562,0.946349440318976,
-0.165859511884162));
#161463=CARTESIAN_POINT('Ctrl Pts',(5.133833235,0.809946053,5.119204656));
#161464=CARTESIAN_POINT('Ctrl Pts',(5.413053537,0.875601501,4.839186457));
#161465=CARTESIAN_POINT('Ctrl Pts',(5.660161555,0.940829639,4.530460371));
#161466=CARTESIAN_POINT('Ctrl Pts',(5.481680828,0.809946053,5.118708363));
#161467=CARTESIAN_POINT('Ctrl Pts',(5.76087406,0.875601501,4.819717273));
#161468=CARTESIAN_POINT('Ctrl Pts',(6.00589160500001,0.940829639,4.492133795));
#161469=CARTESIAN_POINT('',(5.48168083522909,0.809946052117951,5.11870835314386));
#161470=CARTESIAN_POINT('',(5.85195259677292,0.900669500639929,4.69091151073651));
#161471=CARTESIAN_POINT('Origin',(-0.140058776189231,0.803573323345158,
-0.132196708794412));
#161472=CARTESIAN_POINT('Ctrl Pts',(5.65722187832807,0.940053944286819,
4.53413065786505));
#161473=CARTESIAN_POINT('Ctrl Pts',(5.68960394382895,0.933168237856532,
4.56025622786481));
#161474=CARTESIAN_POINT('Ctrl Pts',(5.72204085889477,0.926448448864469,
4.5863970240271));
#161475=CARTESIAN_POINT('Ctrl Pts',(5.78694146272018,0.913330774478859,
4.63864783063363));
#161476=CARTESIAN_POINT('Ctrl Pts',(5.81944146835668,0.906925555304823,
4.66478707531063));
#161477=CARTESIAN_POINT('Ctrl Pts',(5.85195259562809,0.900669500640576,
4.69091151216137));
#161478=CARTESIAN_POINT('',(5.30775704407508,0.809946050061996,5.11895649646111));
#161479=CARTESIAN_POINT('Origin',(3.37230243729891E-12,0.714028547998777,
2.2963402013243E-12));
#161480=CARTESIAN_POINT('',(5.97096547083895,0.749999999471665,4.53845469731977));
#161481=CARTESIAN_POINT('',(5.82650629090568,0.714243089334641,4.66548489856268));
#161482=CARTESIAN_POINT('Origin',(0.925704659898806,0.473619308971619,-1.12614361973372));
#161483=CARTESIAN_POINT('',(5.73205483888752,0.750000000168396,4.83668763995693));
#161484=CARTESIAN_POINT('Origin',(0.,0.750000000000029,0.));
#161485=CARTESIAN_POINT('Origin',(-1.07292362222049,0.692075011843041,0.979133253777728));
#161486=CARTESIAN_POINT('Ctrl Pts',(5.654270243,0.940837228,4.537810928));
#161487=CARTESIAN_POINT('Ctrl Pts',(5.90178398,0.875180297,4.229400204));
#161488=CARTESIAN_POINT('Ctrl Pts',(6.114284746,0.809946053,3.895898106));
#161489=CARTESIAN_POINT('Ctrl Pts',(6.12163427499651,0.807689868343035,
3.88436363774475));
#161490=CARTESIAN_POINT('Ctrl Pts',(6.12898380399303,0.805433683686068,
3.87282916948945));
#161491=CARTESIAN_POINT('Ctrl Pts',(5.69222601069185,0.940837228000001,
4.88430655562403));
#161492=CARTESIAN_POINT('Ctrl Pts',(5.95863926358193,0.875180297000001,
4.57382554314938));
#161493=CARTESIAN_POINT('Ctrl Pts',(6.18970224440294,0.809946053,4.23620981689245));
#161494=CARTESIAN_POINT('Ctrl Pts',(6.19769376419614,0.807689868343035,
4.2245330751258));
#161495=CARTESIAN_POINT('Ctrl Pts',(6.20568528398925,0.805433683686067,
4.21285633335913));
#161496=CARTESIAN_POINT('',(6.18954640337577,0.80994605226505,4.23550654132665));
#161497=CARTESIAN_POINT('Origin',(-0.144684598915065,0.946416036811265,
-0.125405476138852));
#161498=CARTESIAN_POINT('',(6.15191556712846,0.809946053334099,4.0657023142925));
#161499=CARTESIAN_POINT('Origin',(2.28983498828939E-13,0.901573518000056,
2.2291196666302E-13));
#161500=CARTESIAN_POINT('Origin',(-0.158721396605581,0.803569456127978,
-0.109853265678252));
#161501=CARTESIAN_POINT('Origin',(-0.121369578731334,0.946349488399566,
-0.143115011248638));
#161502=CARTESIAN_POINT('Ctrl Pts',(6.114284746,0.809946053,3.895898106));
#161503=CARTESIAN_POINT('Ctrl Pts',(6.326781397,0.875601501000001,3.562402465));
#161504=CARTESIAN_POINT('Ctrl Pts',(6.501745184,0.940829639,3.207773304));
#161505=CARTESIAN_POINT('Ctrl Pts',(6.453893166,0.809946053,3.820636465));
#161506=CARTESIAN_POINT('Ctrl Pts',(6.66228477,0.875601501000001,3.468617329));
#161507=CARTESIAN_POINT('Ctrl Pts',(6.831153176,0.940829639,3.096021041));
#161508=CARTESIAN_POINT('',(6.45389317097018,0.809946052117965,3.82063645379648));
#161509=CARTESIAN_POINT('',(6.7235445095841,0.900669500649203,3.32324378054198));
#161510=CARTESIAN_POINT('Origin',(-0.165202437510702,0.803573330537153,
-0.0989974117660164));
#161511=CARTESIAN_POINT('Ctrl Pts',(6.49966323789617,0.940053944386922,
3.21198972494361));
#161512=CARTESIAN_POINT('Ctrl Pts',(6.53690445380191,0.933168237977147,
3.23054330668388));
#161513=CARTESIAN_POINT('Ctrl Pts',(6.57420251069174,0.9264484489006,3.24909996787951));
#161514=CARTESIAN_POINT('Ctrl Pts',(6.64881815322706,0.913330774524643,
3.28617746825447));
#161515=CARTESIAN_POINT('Ctrl Pts',(6.68617749184471,0.906925555326163,
3.3047190514635));
#161516=CARTESIAN_POINT('Ctrl Pts',(6.72354450877726,0.900669500649855,
3.3232437821697));
#161517=CARTESIAN_POINT('',(6.28408896547809,0.809946050062004,3.85826727006272));
#161518=CARTESIAN_POINT('Origin',(-5.95443833129039E-12,0.714028548,-2.89200087488783E-12));
#161519=CARTESIAN_POINT('',(6.80700121913307,0.749999998604196,3.14876707365042));
#161520=CARTESIAN_POINT('',(6.69322715423015,0.714243089177093,3.30388183145284));
#161521=CARTESIAN_POINT('Origin',(0.661978250407972,0.47361279085057,-1.29881298243699));
#161522=CARTESIAN_POINT('',(6.63778745394538,0.749999999337654,3.49138621564948));
#161523=CARTESIAN_POINT('Origin',(0.,0.749999998746365,0.));
#161524=CARTESIAN_POINT('Origin',(-0.837356842110112,0.692075333990243,
1.18688780490404));
#161525=CARTESIAN_POINT('Ctrl Pts',(6.49757176,0.940837228,3.216218467));
#161526=CARTESIAN_POINT('Ctrl Pts',(6.672999573,0.875180297,2.861810077));
#161527=CARTESIAN_POINT('Ctrl Pts',(6.808839097,0.809946053,2.49042369));
#161528=CARTESIAN_POINT('Ctrl Pts',(6.81353722819479,0.807689868439873,
2.47757896028733));
#161529=CARTESIAN_POINT('Ctrl Pts',(6.81823535938943,0.805433683879746,
2.46473423057468));
#161530=CARTESIAN_POINT('Ctrl Pts',(6.60912646082343,0.940837228000001,
3.5464538510459));
#161531=CARTESIAN_POINT('Ctrl Pts',(6.80256687881479,0.875180297,3.18596073830997));
#161532=CARTESIAN_POINT('Ctrl Pts',(6.9556503352614,0.809946053,2.80656656936472));
#161533=CARTESIAN_POINT('Ctrl Pts',(6.96094486325265,0.807689868439873,
2.79344488336533));
#161534=CARTESIAN_POINT('Ctrl Pts',(6.96623939124391,0.805433683879747,
2.78032319736588));
#161535=CARTESIAN_POINT('',(6.95534695426759,0.809946052265058,2.80591323721172));
#161536=CARTESIAN_POINT('Origin',(-0.168260697371486,0.946416079492337,
-0.0913707898677996));
#161537=CARTESIAN_POINT('',(6.88209301623501,0.809946053334099,2.64816845608985));
#161538=CARTESIAN_POINT('Origin',(4.74880551548651E-13,0.901573518000028,
1.86049092798513E-13));
#161539=CARTESIAN_POINT('Origin',(-0.178625726215517,0.803569088508976,
-0.0731646177719986));
#161540=CARTESIAN_POINT('Origin',(-0.149297058360928,0.946349510647673,
-0.113677938552454));
#161541=CARTESIAN_POINT('Ctrl Pts',(6.808839097,0.809946053,2.49042369));
#161542=CARTESIAN_POINT('Ctrl Pts',(6.94467599,0.875601501000001,2.119044493));
#161543=CARTESIAN_POINT('Ctrl Pts',(7.039314433,0.940829639,1.735094322));
#161544=CARTESIAN_POINT('Ctrl Pts',(7.124328633,0.809946053,2.343915853));
#161545=CARTESIAN_POINT('Ctrl Pts',(7.252174449,0.875601501000001,1.955328694));
#161546=CARTESIAN_POINT('Ctrl Pts',(7.336997617,0.940829639,1.555141784));
#161547=CARTESIAN_POINT('',(7.12432863543045,0.809946052007898,2.34391584102206));
#161548=CARTESIAN_POINT('',(7.28075095350219,0.900669500656451,1.80018486554858));
#161549=CARTESIAN_POINT('Origin',(-0.182621433654452,0.803573323859441,
-0.0611692180826484));
#161550=CARTESIAN_POINT('Ctrl Pts',(7.03818756905568,0.940053944125792,
1.73965972261936));
#161551=CARTESIAN_POINT('Ctrl Pts',(7.07854657807296,0.93316823769528,1.7497737714771));
#161552=CARTESIAN_POINT('Ctrl Pts',(7.11896175957167,0.926448448847887,
1.75987860830767));
#161553=CARTESIAN_POINT('Ctrl Pts',(7.19980349681002,0.913330774458309,
1.78004910006589));
#161554=CARTESIAN_POINT('Ctrl Pts',(7.24027528686602,0.906925555320786,
1.79012603792324));
#161555=CARTESIAN_POINT('Ctrl Pts',(7.28075095320631,0.900669500656858,
1.80018486673939));
#161556=CARTESIAN_POINT('',(6.96658387093794,0.809946050062004,2.41716975438613));
#161557=CARTESIAN_POINT('Origin',(1.87913920535188E-12,0.714028547999755,
3.01625044385467E-13));
#161558=CARTESIAN_POINT('',(7.32474915823918,0.749999999442343,1.61184659974827));
#161559=CARTESIAN_POINT('',(7.24698015457827,0.714243089244742,1.78779292270851));
#161560=CARTESIAN_POINT('Origin',(0.367293486184526,0.473617512480871,-1.41075299706784));
#161561=CARTESIAN_POINT('',(7.23314450366846,0.750000000163903,1.98283145817019));
#161562=CARTESIAN_POINT('Origin',(0.,0.750000000000029,0.));
#161563=CARTESIAN_POINT('Origin',(-0.56263078148524,0.692074923964662,1.33914628784326));
#161564=CARTESIAN_POINT('Ctrl Pts',(7.037054042,0.940837228,1.744239205));
#161565=CARTESIAN_POINT('Ctrl Pts',(7.132193124,0.875180297,1.360404892));
#161566=CARTESIAN_POINT('Ctrl Pts',(7.185019699,0.809946053,0.96849983));
#161567=CARTESIAN_POINT('Ctrl Pts',(7.18684675325495,0.807689868436296,
0.95494544357495));
#161568=CARTESIAN_POINT('Ctrl Pts',(7.1886738075099,0.805433683872588,0.941391057149892));
#161569=CARTESIAN_POINT('Ctrl Pts',(7.21699150217313,0.940837228,2.04277290609919));
#161570=CARTESIAN_POINT('Ctrl Pts',(7.32841402766577,0.875180297,1.64912395008058));
#161571=CARTESIAN_POINT('Ctrl Pts',(7.39635994642072,0.809946053,1.24569138825861));
#161572=CARTESIAN_POINT('Ctrl Pts',(7.39870991667655,0.807689868436296,
1.23173831296156));
#161573=CARTESIAN_POINT('Ctrl Pts',(7.40105988693226,0.805433683872588,
1.21778523766448));
#161574=CARTESIAN_POINT('',(7.39592321120424,0.809946052265051,1.2451185486005));
#161575=CARTESIAN_POINT('Origin',(-0.183968858291761,0.946416066937409,
-0.0530635107189836));
#161576=CARTESIAN_POINT('',(7.2904714443072,0.809946053334099,1.10680918397649));
#161577=CARTESIAN_POINT('Origin',(-5.77229236631283E-13,0.901573518000083,
-6.7762635780344E-14));
#161578=CARTESIAN_POINT('Origin',(-0.190178238047356,0.80356947493056,-0.0330548264754186));
#161579=CARTESIAN_POINT('Origin',(-0.170244477781741,0.946349173716153,
-0.0789258546339719));
#161580=CARTESIAN_POINT('Ctrl Pts',(7.18501969900001,0.809946053,0.96849983));
#161581=CARTESIAN_POINT('Ctrl Pts',(7.237845252,0.875601501000001,0.576602356));
#161582=CARTESIAN_POINT('Ctrl Pts',(7.247733164,0.940829639,0.181284259));
#161583=CARTESIAN_POINT('Ctrl Pts',(7.461638412,0.809946053,0.75759634));
#161584=CARTESIAN_POINT('Ctrl Pts',(7.50296051,0.875601501000001,0.350611062));
#161585=CARTESIAN_POINT('Ctrl Pts',(7.499772204,0.940829639,-0.058454175));
#161586=CARTESIAN_POINT('Ctrl Pts',(7.24761407171315,0.940053944099865,
0.185985165651885));
#161587=CARTESIAN_POINT('Ctrl Pts',(7.28920373107082,0.933168237642109,
0.187186759575636));
#161588=CARTESIAN_POINT('Ctrl Pts',(7.33084626931037,0.926448448776613,
0.188367281414812));
#161589=CARTESIAN_POINT('Ctrl Pts',(7.41413403095609,0.913330774393281,
0.1906876141421));
#161590=CARTESIAN_POINT('Ctrl Pts',(7.45582585695214,0.906925555228153,
0.191828720139254));
#161591=CARTESIAN_POINT('Ctrl Pts',(7.4975175753614,0.900669500590605,0.192951307209456));
#161592=CARTESIAN_POINT('',(7.32332905762014,0.809946050062004,0.863048067009758));
#161593=CARTESIAN_POINT('Origin',(4.06966127464159E-12,0.714028547998533,
5.3952271795131E-13));
#161594=CARTESIAN_POINT('',(7.46187241744399,0.7142430893127,0.188108803996591));
#161595=CARTESIAN_POINT('Origin',(0.0554340383527208,0.473613023976932,
-1.4567289021525));
#161596=CARTESIAN_POINT('Origin',(-0.261598757446677,0.692074811532284,
1.42878662012929));
#161597=CARTESIAN_POINT('Ctrl Pts',(7.24749149900001,0.940837228,0.190701257));
#161598=CARTESIAN_POINT('Ctrl Pts',(7.25789325,0.875180297,-0.204611314));
#161599=CARTESIAN_POINT('Ctrl Pts',(7.225236766,0.809946053,-0.598710006));
#161600=CARTESIAN_POINT('Ctrl Pts',(7.22474524731287,0.808964200515023,
-0.604641657174902));
#161601=CARTESIAN_POINT('Ctrl Pts',(7.22425372862578,0.807982348030045,
-0.610573308349804));
#161602=CARTESIAN_POINT('Ctrl Pts',(7.48711801034727,0.940837228000001,
0.443279003673952));
#161603=CARTESIAN_POINT('Ctrl Pts',(7.51129655000436,0.875180297,0.0348960660811571));
#161604=CARTESIAN_POINT('Ctrl Pts',(7.49091351204778,0.809946053,-0.37369389589682));
#161605=CARTESIAN_POINT('Ctrl Pts',(7.49060672323194,0.808964200515023,
-0.379843657814883));
#161606=CARTESIAN_POINT('Ctrl Pts',(7.49029993441611,0.807982348030045,
-0.385993419732945));
#161607=CARTESIAN_POINT('',(7.35795553086503,0.809946053334099,-0.486303255542236));
#161608=CARTESIAN_POINT('Ctrl Pts',(7.225236766,0.809946053,-0.598710006));
#161609=CARTESIAN_POINT('Ctrl Pts',(7.192580914,0.875601501000001,-0.992801067));
#161610=CARTESIAN_POINT('Ctrl Pts',(7.11725594700001,0.940829639,-1.381002455));
#161611=CARTESIAN_POINT('Ctrl Pts',(7.450050271,0.809946053,-0.864147535));
#161612=CARTESIAN_POINT('Ctrl Pts',(7.402916477,0.875601501000001,-1.270500754));
#161613=CARTESIAN_POINT('Ctrl Pts',(7.311865778,0.940829639,-1.669316881));
#161614=CARTESIAN_POINT('',(7.45005026817131,0.809946052007895,-0.864147546869791));
#161615=CARTESIAN_POINT('',(7.36370860794726,0.900669500577546,-1.42330444245839));
#161616=CARTESIAN_POINT('Origin',(-0.191427337976096,0.803573322522903,
0.0211651271455665));
#161617=CARTESIAN_POINT('Ctrl Pts',(7.11815019508415,0.940053944176777,
-1.37638585233793));
#161618=CARTESIAN_POINT('Ctrl Pts',(7.15902581858686,0.933168237674186,
-1.38415289816254));
#161619=CARTESIAN_POINT('Ctrl Pts',(7.19994855461074,0.926448448807835,
-1.3919518908494));
#161620=CARTESIAN_POINT('Ctrl Pts',(7.28178789774418,0.913330774380453,
-1.40759021277047));
#161621=CARTESIAN_POINT('Ctrl Pts',(7.32275029601023,0.906925555220636,
-1.41543829529631));
#161622=CARTESIAN_POINT('Ctrl Pts',(7.36370860828366,0.900669500578175,
-1.42330444070726));
#161623=CARTESIAN_POINT('',(7.3376435167032,0.809946050062004,-0.731428788525407));
#161624=CARTESIAN_POINT('Origin',(1.30971622436249E-13,0.714028547998533,
8.56519716263548E-15));
#161625=CARTESIAN_POINT('',(7.32455911184973,0.749999999450591,-1.61270998931781));
#161626=CARTESIAN_POINT('',(7.32785581902563,0.714243089095246,-1.42037107428952));
#161627=CARTESIAN_POINT('Origin',(-0.259012497022776,0.473616870185757,
-1.43458741474906));
#161628=CARTESIAN_POINT('',(7.3971934782476,0.750000000283857,-1.23754945340732));
#161629=CARTESIAN_POINT('Origin',(0.,0.750000000000029,0.));
#161630=CARTESIAN_POINT('Origin',(0.0516617329994917,0.69207504842183,1.45161927898567));
#161631=CARTESIAN_POINT('Ctrl Pts',(7.11904430900001,0.940837228,-1.371753671));
#161632=CARTESIAN_POINT('Ctrl Pts',(7.044222355,0.875180297,-1.760060122));
#161633=CARTESIAN_POINT('Ctrl Pts',(6.927609792,0.809946053,-2.137924827));
#161634=CARTESIAN_POINT('Ctrl Pts',(6.92357664226118,0.807689868354167,
-2.15099361562003));
#161635=CARTESIAN_POINT('Ctrl Pts',(6.91954349252227,0.805433683708332,
-2.16406240424011));
#161636=CARTESIAN_POINT('Ctrl Pts',(7.40770217163526,0.940837228000001,
-1.17636559945699));
#161637=CARTESIAN_POINT('Ctrl Pts',(7.34353761128978,0.875180297,-1.58041682072448));
#161638=CARTESIAN_POINT('Ctrl Pts',(7.23580672022365,0.809946053,-1.97509204848454));
#161639=CARTESIAN_POINT('Ctrl Pts',(7.23208075104854,0.807689868354167,
-1.98874224406225));
#161640=CARTESIAN_POINT('Ctrl Pts',(7.2283547818734,0.80543368370833,-2.00239243963988));
#161641=CARTESIAN_POINT('',(7.23516982194198,0.809946052264276,-1.97542856151036));
#161642=CARTESIAN_POINT('Origin',(-0.18924613883507,0.946416062892984,0.0290873232071368));
#161643=CARTESIAN_POINT('',(7.08138979442916,0.809946053334099,-2.05667669546547));
#161644=CARTESIAN_POINT('Origin',(1.14708589848966E-12,0.901573517999861,
-2.58528008029169E-13));
#161645=CARTESIAN_POINT('Origin',(-0.186480273030153,0.803569488776888,
0.0498539794532992));
#161646=CARTESIAN_POINT('Origin',(-0.187649829682202,0.946349141882412,
-0.000147355372646651));
#161647=CARTESIAN_POINT('Ctrl Pts',(6.927609792,0.809946053,-2.137924827));
#161648=CARTESIAN_POINT('Ctrl Pts',(6.810999487,0.875601501,-2.515782215));
#161649=CARTESIAN_POINT('Ctrl Pts',(6.653983753,0.940829639,-2.87871503));
#161650=CARTESIAN_POINT('Ctrl Pts',(7.090106059,0.809946053,-2.445484832));
#161651=CARTESIAN_POINT('Ctrl Pts',(6.956720297,0.875601501,-2.832205366));
#161652=CARTESIAN_POINT('Ctrl Pts',(6.782064634,0.940829639,-3.202124185));
#161653=CARTESIAN_POINT('',(7.09010605367899,0.809946052117973,-2.44548484305816));
#161654=CARTESIAN_POINT('',(6.88558080984488,0.900669500611653,-2.97300805691043));
#161655=CARTESIAN_POINT('Origin',(-0.182401896597097,0.803573307003854,
0.0618214724472022));
#161656=CARTESIAN_POINT('Ctrl Pts',(6.65584952666731,0.940053944150437,
-2.87439859628003));
#161657=CARTESIAN_POINT('Ctrl Pts',(6.6940998150624,0.933168237732746,-2.89077110380397));
#161658=CARTESIAN_POINT('Ctrl Pts',(6.73238924787852,0.926448448773642,
-2.90718493942895));
#161659=CARTESIAN_POINT('Ctrl Pts',(6.80895345513282,0.913330774434679,
-2.94005068584498));
#161660=CARTESIAN_POINT('Ctrl Pts',(6.84727106960049,0.906925555258089,
-2.95652098951638));
#161661=CARTESIAN_POINT('Ctrl Pts',(6.88558081045313,0.900669500624169,
-2.97300805529551));
#161662=CARTESIAN_POINT('',(7.00885791987027,0.809946050062004,-2.29170484671772));
#161663=CARTESIAN_POINT('Origin',(1.46397650946373E-11,0.714028547998777,
-6.56484415439973E-12));
#161664=CARTESIAN_POINT('',(6.80663001399836,0.749999999460468,-3.14956942225839));
#161665=CARTESIAN_POINT('',(6.85119682732554,0.7142430892164,-2.96243597874438));
#161666=CARTESIAN_POINT('Origin',(-0.561351999888413,0.473617915787033,
-1.34536704192595));
#161667=CARTESIAN_POINT('',(6.95821465439766,0.750000000203561,-2.79879417363605));
#161668=CARTESIAN_POINT('Origin',(0.,0.750000000000029,0.));
#161669=CARTESIAN_POINT('Origin',(0.362509541410632,0.692075069548214,1.40657521275727));
#161670=CARTESIAN_POINT('Ctrl Pts',(6.657718518,0.940837228,-2.870066921));
#161671=CARTESIAN_POINT('Ctrl Pts',(6.501171452,0.875180297,-3.233210475));
#161672=CARTESIAN_POINT('Ctrl Pts',(6.306055484,0.809946053,-3.577172659));
#161673=CARTESIAN_POINT('Ctrl Pts',(6.2993072239509,0.807689868397938,-3.5890688983928));
#161674=CARTESIAN_POINT('Ctrl Pts',(6.29255896390185,0.805433683795875,
-3.60096513778561));
#161675=CARTESIAN_POINT('Ctrl Pts',(6.98163038081954,0.940837228000001,
-2.74129982289584));
#161676=CARTESIAN_POINT('Ctrl Pts',(6.83210688278068,0.875180297,-3.12211106708423));
#161677=CARTESIAN_POINT('Ctrl Pts',(6.6420511733511,0.809946053,-3.48440004939066));
#161678=CARTESIAN_POINT('Ctrl Pts',(6.63547792686494,0.807689868397938,
-3.4969301374741));
#161679=CARTESIAN_POINT('Ctrl Pts',(6.62890468037882,0.805433683795875,
-3.50946022555754));
#161680=CARTESIAN_POINT('',(6.6413568236661,0.80994605226505,-3.48459178218603));
#161681=CARTESIAN_POINT('Origin',(-0.178568867614937,0.946416037059252,
0.0690896628819765));
#161682=CARTESIAN_POINT('',(6.47370614201999,0.809946053334099,-3.53088221829681));
#161683=CARTESIAN_POINT('Origin',(-1.32836450172924E-12,0.901573518000083,
6.05635333550403E-13));
#161684=CARTESIAN_POINT('Origin',(-0.171403251577942,0.803569519200059,
0.0887761307562095));
#161685=CARTESIAN_POINT('Origin',(-0.183294010153269,0.946349438276496,
0.0401950578583943));
#161686=CARTESIAN_POINT('Ctrl Pts',(6.306055484,0.809946053,-3.577172659));
#161687=CARTESIAN_POINT('Ctrl Pts',(6.110943294,0.875601501000001,-3.921128183));
#161688=CARTESIAN_POINT('Ctrl Pts',(5.879578673,0.940829639,-4.241822088));
#161689=CARTESIAN_POINT('Ctrl Pts',(6.398636369,0.809946053,-3.912473977));
#161690=CARTESIAN_POINT('Ctrl Pts',(6.185235608,0.875601501,-4.261479203));
#161691=CARTESIAN_POINT('Ctrl Pts',(5.935141687,0.940829639,-4.585203721));
#161692=CARTESIAN_POINT('',(6.39863636144931,0.809946052007894,-3.91247398658227));
#161693=CARTESIAN_POINT('',(6.0854909065751,0.900669500598591,-4.38369711823371));
#161694=CARTESIAN_POINT('Origin',(-0.164847907856605,0.80357330245582,0.0995873118686996));
#161695=CARTESIAN_POINT('Ctrl Pts',(5.8823287320493,0.940053944089694,-4.23800765756635));
#161696=CARTESIAN_POINT('Ctrl Pts',(5.9161651452579,0.933168237624726,-4.26222006634371));
#161697=CARTESIAN_POINT('Ctrl Pts',(5.95003090244124,0.926448448791528,
-4.2864812512914));
#161698=CARTESIAN_POINT('Ctrl Pts',(6.01773991754674,0.913330774397287,
-4.33503765619876));
#161699=CARTESIAN_POINT('Ctrl Pts',(6.05162105897944,0.906925555238692,
-4.35936004763431));
#161700=CARTESIAN_POINT('Ctrl Pts',(6.08549090761331,0.900669500599227,
-4.383697116789));
#161701=CARTESIAN_POINT('',(6.35234591730059,0.809946050062004,-3.74482333360496));
#161702=CARTESIAN_POINT('Origin',(8.25164589435268E-12,0.714028547998533,
-6.10449191196238E-12));
#161703=CARTESIAN_POINT('',(5.97043046128455,0.749999999462928,-4.53915849030982));
#161704=CARTESIAN_POINT('',(6.05418348661255,0.714243089235877,-4.36598066940676));
#161705=CARTESIAN_POINT('Origin',(-0.837442198376062,0.473618072624967,
-1.19323890730608));
#161706=CARTESIAN_POINT('',(6.19387744755386,0.750000000332207,-4.22917038787356));
#161707=CARTESIAN_POINT('Origin',(0.,0.750000000000029,0.));
#161708=CARTESIAN_POINT('Origin',(0.656406169991699,0.692075080705617,1.29576162756753));
#161709=CARTESIAN_POINT('Ctrl Pts',(5.88508521,0.940837228,-4.234179032));
#161710=CARTESIAN_POINT('Ctrl Pts',(5.65413299700001,0.875180297,-4.5551795));
#161711=CARTESIAN_POINT('Ctrl Pts',(5.38963702999999,0.809946053,-4.849155874));
#161712=CARTESIAN_POINT('Ctrl Pts',(5.38048920064803,0.807689868382952,
-4.85932330956951));
#161713=CARTESIAN_POINT('Ctrl Pts',(5.37134137129619,0.805433683765901,
-4.86949074513889));
#161714=CARTESIAN_POINT('Ctrl Pts',(6.2291053126719,0.940837228,-4.17805391238279));
#161715=CARTESIAN_POINT('Ctrl Pts',(6.00121443024192,0.875180297,-4.51781886922421));
#161716=CARTESIAN_POINT('Ctrl Pts',(5.73772069546297,0.809946053,-4.83078137711905));
#161717=CARTESIAN_POINT('Ctrl Pts',(5.7286075292079,0.807689868382952,-4.84160546509385));
#161718=CARTESIAN_POINT('Ctrl Pts',(5.7194943629528,0.805433683765901,-4.85242955306867));
#161719=CARTESIAN_POINT('',(5.73700136409408,0.809946052264276,-4.83081936142431));
#161720=CARTESIAN_POINT('Origin',(-0.159541768734545,0.946416043065824,
0.105861393742597));
#161721=CARTESIAN_POINT('',(5.56331918515664,0.809946053334099,-4.83998761354413));
#161722=CARTESIAN_POINT('Origin',(1.38777878078145E-14,0.901573518000056,
-3.03576608295941E-15));
#161723=CARTESIAN_POINT('Origin',(-0.14831164317236,0.803569412242196,0.1235471652116));
#161724=CARTESIAN_POINT('Origin',(-0.170368230555993,0.94634918625941,0.0786583648630335));
#161725=CARTESIAN_POINT('Ctrl Pts',(5.38963703,0.809946053,-4.849155874));
#161726=CARTESIAN_POINT('Ctrl Pts',(5.125146184,0.875601501000001,-5.143126555));
#161727=CARTESIAN_POINT('Ctrl Pts',(4.830251029,0.940829639,-5.406586261));
#161728=CARTESIAN_POINT('Ctrl Pts',(5.407973553,0.809946053,-5.196520186));
#161729=CARTESIAN_POINT('Ctrl Pts',(5.124536177,0.875601501000001,-5.491491009));
#161730=CARTESIAN_POINT('Ctrl Pts',(4.81069811,0.940829639,-5.753884227));
#161731=CARTESIAN_POINT('',(5.40797354355034,0.8099460520079,-5.19652019377016));
#161732=CARTESIAN_POINT('',(5.00085021158662,0.900669500636843,-5.58940937485491));
#161733=CARTESIAN_POINT('Origin',(-0.13958530168794,0.803573298460263,0.132696195845124));
#161734=CARTESIAN_POINT('Ctrl Pts',(4.83375678258189,0.940053944205177,
-5.40345218965847));
#161735=CARTESIAN_POINT('Ctrl Pts',(4.8615971667985,0.933168237817763,-5.43437235426476));
#161736=CARTESIAN_POINT('Ctrl Pts',(4.88945572450934,0.926448448826654,
-5.46534646379243));
#161737=CARTESIAN_POINT('Ctrl Pts',(4.94514354866678,0.913330774481685,
-5.5273230837034));
#161738=CARTESIAN_POINT('Ctrl Pts',(4.97300397282262,0.906925555301418,
-5.55836027520916));
#161739=CARTESIAN_POINT('Ctrl Pts',(5.00085021292921,0.900669500637492,
-5.58940937365095));
#161740=CARTESIAN_POINT('',(5.39880527916107,0.809946050062004,-5.02283804326252));
#161741=CARTESIAN_POINT('Origin',(1.91383367487141E-12,0.714028548001467,
-1.57773100140091E-12));
#161742=CARTESIAN_POINT('',(4.85506021197657,0.750000000749204,-5.71650155683177));
#161743=CARTESIAN_POINT('',(4.97408325374587,0.714243089138568,-5.5653769574538));
#161744=CARTESIAN_POINT('Origin',(-1.0743706025104,0.473612770293792,-0.985320519253279));
#161745=CARTESIAN_POINT('',(5.13992141815109,0.750000001354628,-5.46179529301488));
#161746=CARTESIAN_POINT('Origin',(0.,0.750000002055273,0.));
#161747=CARTESIAN_POINT('Origin',(0.91961459177966,0.692074279456245,1.12435267143665));
#161748=CARTESIAN_POINT('Ctrl Pts',(4.837271857,0.940837228,-5.400305637));
#161749=CARTESIAN_POINT('Ctrl Pts',(4.54271356700001,0.875180297,-5.664153394));
#161750=CARTESIAN_POINT('Ctrl Pts',(4.221205138,0.809946053,-5.894397949));
#161751=CARTESIAN_POINT('Ctrl Pts',(4.21008548164904,0.807689868371028,
-5.9023611627056));
#161752=CARTESIAN_POINT('Ctrl Pts',(4.19896582529809,0.805433683742054,
-5.9103243764113));
#161753=CARTESIAN_POINT('Ctrl Pts',(5.1853142030758,0.940837228000001,-5.41944684537321));
#161754=CARTESIAN_POINT('Ctrl Pts',(4.8897118604283,0.875180297,-5.70227848261083));
#161755=CARTESIAN_POINT('Ctrl Pts',(4.56510077445277,0.809946053,-5.95128073642013));
#161756=CARTESIAN_POINT('Ctrl Pts',(4.55387380993742,0.807689868371028,
-5.9598927019029));
#161757=CARTESIAN_POINT('Ctrl Pts',(4.54264684542219,0.805433683742056,
-5.96850466738573));
#161758=CARTESIAN_POINT('',(4.56439009325036,0.809946052265046,-5.95116319851744));
#161759=CARTESIAN_POINT('Origin',(-0.133054682399875,0.946416046548661,
0.137683166548233));
#161760=CARTESIAN_POINT('',(4.39279760585611,0.809946053334099,-5.92278056671925));
#161761=CARTESIAN_POINT('Origin',(-2.0643209364124E-13,0.901573518000139,
2.51534904016637E-13));
#161762=CARTESIAN_POINT('Origin',(-0.118285670479293,0.803569491232197,
0.152541959866282));
#161763=CARTESIAN_POINT('Origin',(-0.14947577587879,0.946349162772959,0.113443387801616));
#161764=CARTESIAN_POINT('Ctrl Pts',(4.221205138,0.809946053,-5.894397949));
#161765=CARTESIAN_POINT('Ctrl Pts',(3.899702935,0.875601501000001,-6.124638046));
#161766=CARTESIAN_POINT('Ctrl Pts',(3.555066216,0.940829639,-6.318544469));
#161767=CARTESIAN_POINT('Ctrl Pts',(4.164439905,0.809946053,-6.237582888));
#161768=CARTESIAN_POINT('Ctrl Pts',(3.824219129,0.875601501000001,-6.464726799));
#161769=CARTESIAN_POINT('Ctrl Pts',(3.461311636,0.940829639,-6.653519501));
#161770=CARTESIAN_POINT('',(4.16443989410765,0.809946052117949,-6.23758289353459));
#161771=CARTESIAN_POINT('',(3.68237531859818,0.900669500629599,-6.53376706126185));
#161772=CARTESIAN_POINT('Origin',(-0.107796101370615,0.803573316163276,
0.159600559105972));
#161773=CARTESIAN_POINT('Ctrl Pts',(3.55916373987558,0.940053944136155,
-6.31623730438967));
#161774=CARTESIAN_POINT('Ctrl Pts',(3.57970630987706,0.933168237731745,
-6.35241943241517));
#161775=CARTESIAN_POINT('Ctrl Pts',(3.60025503167879,0.926448448810044,
-6.38865815044762));
#161776=CARTESIAN_POINT('Ctrl Pts',(3.64131776395972,0.913330774465002,
-6.46115702738743));
#161777=CARTESIAN_POINT('Ctrl Pts',(3.66185474806907,0.906925555285222,
-6.49745775420293));
#161778=CARTESIAN_POINT('Ctrl Pts',(3.68237532006268,0.900669500643497,
-6.53376706033201));
#161779=CARTESIAN_POINT('',(4.1928225065985,0.809946050062004,-6.06599042879995));
#161780=CARTESIAN_POINT('Origin',(1.32012456521835E-12,0.714028548,-2.06258621293642E-12));
#161781=CARTESIAN_POINT('',(3.51267275150287,0.749999999475252,-6.62654735398287));
#161782=CARTESIAN_POINT('',(3.66140041731029,0.714243089203531,-6.50454240349333));
#161783=CARTESIAN_POINT('Origin',(-1.26107012722738,0.473618310017934,-0.731321202018131));
#161784=CARTESIAN_POINT('',(3.84562836831758,0.750000000182253,-6.43903272670087));
#161785=CARTESIAN_POINT('Origin',(0.,0.750000000000029,0.));
#161786=CARTESIAN_POINT('Origin',(1.13981441991433,0.692074972328244,0.900383294543275));
#161787=CARTESIAN_POINT('Ctrl Pts',(3.563273049,0.940837228,-6.313919953));
#161788=CARTESIAN_POINT('Ctrl Pts',(3.2188819,0.875180297,-6.508277771));
#161789=CARTESIAN_POINT('Ctrl Pts',(2.855394386,0.809946053,-6.664024527));
#161790=CARTESIAN_POINT('Ctrl Pts',(2.84282284542823,0.807689868362209,
-6.6694111677691));
#161791=CARTESIAN_POINT('Ctrl Pts',(2.83025130485638,0.805433683724415,
-6.67479780853829));
#161792=CARTESIAN_POINT('Ctrl Pts',(3.89906356434784,0.940837228,-6.40743246670405));
#161793=CARTESIAN_POINT('Ctrl Pts',(3.54957179937433,0.875180297,-6.62010589188342));
#161794=CARTESIAN_POINT('Ctrl Pts',(3.17902181501696,0.809946053,-6.7935048240109));
#161795=CARTESIAN_POINT('Ctrl Pts',(3.16620601259514,0.807689868362209,
-6.79950198106963));
#161796=CARTESIAN_POINT('Ctrl Pts',(3.15339021017337,0.805433683724414,
-6.80549913812837));
#161797=CARTESIAN_POINT('',(3.17835301629486,0.809946052265058,-6.79323725863071));
#161798=CARTESIAN_POINT('Origin',(-0.100346118795918,0.946416093894335,
0.163066990765337));
#161799=CARTESIAN_POINT('',(3.01687369313244,0.809946053334099,-6.72863088383735));
#161800=CARTESIAN_POINT('Origin',(5.75277672720809E-13,0.901573517999806,
-9.22872889219661E-13));
#161801=CARTESIAN_POINT('Origin',(-0.0827278906056161,0.803569457020606,
0.174402821713849));
#161802=CARTESIAN_POINT('Origin',(-0.121594340985359,0.946349478271723,
0.14292426058979));
#161803=CARTESIAN_POINT('Ctrl Pts',(2.855394386,0.809946053,-6.664024527));
#161804=CARTESIAN_POINT('Ctrl Pts',(2.491913911,0.875601501000001,-6.819768268));
#161805=CARTESIAN_POINT('Ctrl Pts',(2.113650457,0.940829639,-6.93505456));
#161806=CARTESIAN_POINT('Ctrl Pts',(2.726181675,0.809946053,-6.986983146));
#161807=CARTESIAN_POINT('Ctrl Pts',(2.345085845,0.875601501,-7.135679149));
#161808=CARTESIAN_POINT('Ctrl Pts',(1.950078078,0.940829639,-7.24204359900001));
#161809=CARTESIAN_POINT('',(2.7261816631742,0.80994605211795,-6.98698314906222));
#161810=CARTESIAN_POINT('',(2.19171664906142,0.900669500617564,-7.1726130614454));
#161811=CARTESIAN_POINT('Origin',(-0.0709664804698285,0.803573343433978,
0.179042142867073));
#161812=CARTESIAN_POINT('Ctrl Pts',(2.11814815554889,0.940053944109833,
-6.9336821817921));
#161813=CARTESIAN_POINT('Ctrl Pts',(2.13043236392346,0.933168237714838,
-6.97343443708677));
#161814=CARTESIAN_POINT('Ctrl Pts',(2.14271041508717,0.926448448760565,
-7.01324328206604));
#161815=CARTESIAN_POINT('Ctrl Pts',(2.16722800824216,0.913330774417522,
-7.09287444931125));
#161816=CARTESIAN_POINT('Ctrl Pts',(2.17948126585138,0.906925555270505,
-7.13274132967918));
#161817=CARTESIAN_POINT('Ctrl Pts',(2.19171665080781,0.900669500618194,
-7.17261306090959));
#161818=CARTESIAN_POINT('',(2.7907880137327,0.809946050062004,-6.82550384335576));
#161819=CARTESIAN_POINT('Origin',(4.21732961053412E-12,0.714028547999755,
-1.32797418894715E-11));
#161820=CARTESIAN_POINT('',(2.00603661220003,0.749999999425987,-7.2267431670167));
#161821=CARTESIAN_POINT('',(2.17751456677922,0.714243089251923,-7.13956267616647));
#161822=CARTESIAN_POINT('Origin',(-1.3887988617426,0.473616821962798,-0.443132249548737));
#161823=CARTESIAN_POINT('',(2.3715180151596,0.750000000306954,-7.11518814286577));
#161824=CARTESIAN_POINT('Origin',(0.,0.750000000000029,0.));
#161825=CARTESIAN_POINT('Origin',(1.30672170332859,0.692075255289197,0.634308337555363));
#161826=CARTESIAN_POINT('Ctrl Pts',(2.122659554,0.940837228,-6.932302389));
#161827=CARTESIAN_POINT('Ctrl Pts',(1.744538893,0.875180297,-7.04808231200001));
#161828=CARTESIAN_POINT('Ctrl Pts',(1.356068566,0.809946053,-7.122048725));
#161829=CARTESIAN_POINT('Ctrl Pts',(1.34263297247409,0.807689868356189,
-7.12460691951465));
#161830=CARTESIAN_POINT('Ctrl Pts',(1.32919737894819,0.805433683712374,
-7.12716511402929));
#161831=CARTESIAN_POINT('Ctrl Pts',(2.43049704741223,0.940837228,-7.09581366670697));
#161832=CARTESIAN_POINT('Ctrl Pts',(2.04345770499428,0.875180297,-7.2283845069501));
#161833=CARTESIAN_POINT('Ctrl Pts',(1.64429532972229,0.809946053,-7.31807217462003));
#161834=CARTESIAN_POINT('Ctrl Pts',(1.63048994214892,0.807689868356189,
-7.32117410278123));
#161835=CARTESIAN_POINT('Ctrl Pts',(1.61668455457555,0.805433683712374,
-7.32427603094229));
#161836=CARTESIAN_POINT('',(1.64369968581408,0.809946052265051,-7.31766709281447));
#161837=CARTESIAN_POINT('Origin',(-0.0629454776259189,0.946416037296776,
0.180825992163296));
#161838=CARTESIAN_POINT('',(1.49988411999609,0.809946053334099,-7.2198578984163));
#161839=CARTESIAN_POINT('Origin',(-4.83228908276789E-13,0.901573518000167,
1.90602741922952E-12));
#161840=CARTESIAN_POINT('Origin',(-0.0433024034837949,0.803569395438105,
0.188109806131513));
#161841=CARTESIAN_POINT('Origin',(-0.0880268758334116,0.94634945669678,
0.165721505977623));
#161842=CARTESIAN_POINT('Ctrl Pts',(1.356068566,0.809946053,-7.122048725));
#161843=CARTESIAN_POINT('Ctrl Pts',(0.967605761,0.875601501000001,-7.196013706));
#161844=CARTESIAN_POINT('Ctrl Pts',(0.573402753,0.940829639,-7.227289207));
#161845=CARTESIAN_POINT('Ctrl Pts',(1.16045022,0.809946053,-7.409679837));
#161846=CARTESIAN_POINT('Ctrl Pts',(0.756298953000001,0.875601501000001,
-7.47297507200001));
#161847=CARTESIAN_POINT('Ctrl Pts',(0.347661035,0.940829639,-7.491937787));
#161848=CARTESIAN_POINT('',(1.16045020779686,0.809946052007894,-7.40967983745501));
#161849=CARTESIAN_POINT('',(0.598575744401869,0.900669500572252,-7.47607564655911));
#161850=CARTESIAN_POINT('Origin',(-0.0308185621163465,0.803573345307439,
0.190111958624054));
#161851=CARTESIAN_POINT('Ctrl Pts',(0.578090317678941,0.940053944129792,
-7.22691578740449));
#161852=CARTESIAN_POINT('Ctrl Pts',(0.581541768262509,0.933168237656136,
-7.26837939890857));
#161853=CARTESIAN_POINT('Ctrl Pts',(0.584975040441821,0.926448448774479,
-7.30989695258816));
#161854=CARTESIAN_POINT('Ctrl Pts',(0.591801078877184,0.913330774363199,
-7.39293694524516));
#161855=CARTESIAN_POINT('Ctrl Pts',(0.595197661337425,0.906925555221954,
-7.43450584811815));
#161856=CARTESIAN_POINT('Ctrl Pts',(0.598575746205688,0.900669500572879,
-7.47607564641263));
#161857=CARTESIAN_POINT('',(1.25825937515092,0.809946050062004,-7.265864284091));
#161858=CARTESIAN_POINT('Origin',(5.75901088969988E-13,0.714028548000245,
-1.11187101192733E-11));
#161859=CARTESIAN_POINT('',(0.405600432040824,0.74999999933706,-7.48902450137263));
#161860=CARTESIAN_POINT('',(0.5918105554394,0.714243089348684,-7.44074493336252));
#161861=CARTESIAN_POINT('Origin',(-1.45159130690835,0.473612960585341,-0.134218633737058));
#161862=CARTESIAN_POINT('',(0.786518113978562,0.750000000212775,-7.45864526972393));
#161863=CARTESIAN_POINT('Origin',(0.,0.750000000000029,0.));
#161864=CARTESIAN_POINT('Origin',(1.41252863802681,0.69207492570701,0.338569540540863));
#161865=CARTESIAN_POINT('Ctrl Pts',(0.582792857,0.940837228,-7.226538071));
#161866=CARTESIAN_POINT('Ctrl Pts',(0.188623186,0.875180297,-7.25832635800001));
#161867=CARTESIAN_POINT('Ctrl Pts',(-0.206665513,0.809946053,-7.24705384000001));
#161868=CARTESIAN_POINT('Ctrl Pts',(-0.220336925761674,0.807689868398275,
-7.24666396989535));
#161869=CARTESIAN_POINT('Ctrl Pts',(-0.234008338523342,0.805433683796549,
-7.24627409979073));
#161870=CARTESIAN_POINT('Ctrl Pts',(0.848283189422318,0.940837228,-7.45240250622955));
#161871=CARTESIAN_POINT('Ctrl Pts',(0.441793800395535,0.875180297,-7.49867189599113));
#161872=CARTESIAN_POINT('Ctrl Pts',(0.0326834214022629,0.809946053,-7.50045460502665));
#161873=CARTESIAN_POINT('Ctrl Pts',(0.0185339734912782,0.807689868398275,
-7.50051626161112));
#161874=CARTESIAN_POINT('Ctrl Pts',(0.00438452558029279,0.805433683796549,
-7.50057791819554));
#161875=CARTESIAN_POINT('',(0.0321887839317885,0.809946052265054,-7.49993094798273));
#161876=CARTESIAN_POINT('Origin',(-0.0226016246518017,0.946416076947056,
0.190129940226492));
#161877=CARTESIAN_POINT('',(-0.0872383680465476,0.809946053334099,-7.37349238247579));
#161878=CARTESIAN_POINT('Origin',(-1.08545578124744E-13,0.901573518000028,
1.85615411929518E-13));
#161879=CARTESIAN_POINT('Origin',(-0.00185196880873136,0.803569459122582,
0.193020748408552));
#161880=CARTESIAN_POINT('Origin',(-0.0503436538305299,0.946349183241457,
0.180770695181811));
#161881=CARTESIAN_POINT('Ctrl Pts',(-0.206665513,0.809946053,-7.24705384));
#161882=CARTESIAN_POINT('Ctrl Pts',(-0.601946558,0.875601501000001,-7.235781541));
#161883=CARTESIAN_POINT('Ctrl Pts',(-0.993656627,0.940829639,-7.18158384400001));
#161884=CARTESIAN_POINT('Ctrl Pts',(-0.459542598,0.809946053,-7.48590813500001));
#161885=CARTESIAN_POINT('Ctrl Pts',(-0.867851637,0.875601501000001,-7.460842987));
#161886=CARTESIAN_POINT('Ctrl Pts',(-1.271012251,0.940829639,-7.391517291));
#161887=CARTESIAN_POINT('',(-0.459542610028098,0.809946052117958,-7.48590813281646));
#161888=CARTESIAN_POINT('',(-1.0225538965043,0.900669500589206,-7.42996524392277));
#161889=CARTESIAN_POINT('Origin',(0.0107703977697209,0.803573338426796,
0.192292192038651));
#161890=CARTESIAN_POINT('Ctrl Pts',(-0.988998380749854,0.940053944129632,
-7.18222684255033));
#161891=CARTESIAN_POINT('Ctrl Pts',(-0.994541073994604,0.933168237660314,
-7.22346301771727));
#161892=CARTESIAN_POINT('Ctrl Pts',(-1.00011311661772,0.926448448773653,
-7.26474796616579));
#161893=CARTESIAN_POINT('Ctrl Pts',(-1.01129781094299,0.913330774359142,
-7.34731392651569));
#161894=CARTESIAN_POINT('Ctrl Pts',(-1.01691672399893,0.906925555249925,
-7.38864113618631));
#161895=CARTESIAN_POINT('Ctrl Pts',(-1.02255389469136,0.900669500589833,
-7.42996524417017));
#161896=CARTESIAN_POINT('',(-0.333104073596248,0.809946050062004,-7.36648098668171));
#161897=CARTESIAN_POINT('Origin',(4.5102810375397E-14,0.714028548000489,
-7.69349861595714E-13));
#161898=CARTESIAN_POINT('',(-1.21380115554419,0.749999993612532,-7.40112736975039));
#161899=CARTESIAN_POINT('',(-1.02156586106537,0.71424308919482,-7.39400622708004));
#161900=CARTESIAN_POINT('Origin',(-1.44650614712913,0.47361195078468,0.180945298525509));
#161901=CARTESIAN_POINT('',(-0.83525852122216,0.749999995259856,-7.45334442616223));
#161902=CARTESIAN_POINT('Origin',(0.,0.749999992945671,0.));
#161903=CARTESIAN_POINT('Origin',(1.45228896547467,0.692075656665917,0.0270087042234279));
#161904=CARTESIAN_POINT('Ctrl Pts',(-0.984324587,0.940837228,-7.182868863));
#161905=CARTESIAN_POINT('Ctrl Pts',(-1.376112332,0.875180297,-7.12917913000001));
#161906=CARTESIAN_POINT('Ctrl Pts',(-1.759736143,0.809946053,-7.03319477300001));
#161907=CARTESIAN_POINT('Ctrl Pts',(-1.77300411522825,0.807689868391784,
-7.02987506826191));
#161908=CARTESIAN_POINT('Ctrl Pts',(-1.78627208745656,0.805433683783566,
-7.02655536352382));
#161909=CARTESIAN_POINT('Ctrl Pts',(-0.773595447491138,0.940837228,-7.46052528796711));
#161910=CARTESIAN_POINT('Ctrl Pts',(-1.18052789164637,0.875180297000001,
-7.41832972190354));
#161911=CARTESIAN_POINT('Ctrl Pts',(-1.58045672673831,0.809946053,-7.33212411374335));
#161912=CARTESIAN_POINT('Ctrl Pts',(-1.59428862279148,0.807689868391784,
-7.32914261577011));
#161913=CARTESIAN_POINT('Ctrl Pts',(-1.60812051884472,0.805433683783564,
-7.32616111779673));
#161914=CARTESIAN_POINT('',(-1.58082722719252,0.809946052264272,-7.33150636799885));
#161915=CARTESIAN_POINT('Origin',(0.0187991128872561,0.946416066667061,
0.190543491964065));
#161916=CARTESIAN_POINT('',(-1.6702816869935,0.809946053334099,-7.1823505580364));
#161917=CARTESIAN_POINT('Origin',(1.48020701598583E-13,0.901573518000111,
3.93348548177741E-13));
#161918=CARTESIAN_POINT('Origin',(0.039683511241196,0.803566823389688,0.18890083934363));
#161919=CARTESIAN_POINT('Origin',(-0.0103065067715735,0.946349447599535,
0.18736394721752));
#161920=CARTESIAN_POINT('Ctrl Pts',(-1.759736143,0.809946053,-7.033194773));
#161921=CARTESIAN_POINT('Ctrl Pts',(-2.143352525,0.875601501000001,-6.937212273));
#161922=CARTESIAN_POINT('Ctrl Pts',(-2.514253728,0.940829639,-6.800075602));
#161923=CARTESIAN_POINT('Ctrl Pts',(-2.058047714,0.809946053,-7.212103688));
#161924=CARTESIAN_POINT('Ctrl Pts',(-2.451422449,0.875601501000001,-7.099850175));
#161925=CARTESIAN_POINT('Ctrl Pts',(-2.830254416,0.940829639,-6.945477661));
#161926=CARTESIAN_POINT('',(-2.05804772526778,0.809946052007895,-7.21210368328908));
#161927=CARTESIAN_POINT('',(-2.59587005412185,0.900669500603544,-7.03643792418539));
#161928=CARTESIAN_POINT('Origin',(0.0518557822968624,0.803573351669035,
0.185481350724109));
#161929=CARTESIAN_POINT('Ctrl Pts',(-2.50984261394196,0.940053944121885,
-6.80170495256707));
#161930=CARTESIAN_POINT('Ctrl Pts',(-2.52412028091269,0.933168237719441,
-6.84078553349327));
#161931=CARTESIAN_POINT('Ctrl Pts',(-2.53843709602442,0.92644844880531,
-6.87990743861688));
#161932=CARTESIAN_POINT('Ctrl Pts',(-2.56710953932711,0.913330774449358,
-6.95813867382332));
#161933=CARTESIAN_POINT('Ctrl Pts',(-2.58148121400414,0.906925555260774,
-6.9972917765852));
#161934=CARTESIAN_POINT('Ctrl Pts',(-2.59587005247871,0.900669500605613,
-7.03643792477924));
#161935=CARTESIAN_POINT('',(-1.90889194599726,0.809946050062004,-7.12264922581068));
#161936=CARTESIAN_POINT('Origin',(7.51352105532455E-13,0.714028548000978,
1.77202003071031E-12));
#161937=CARTESIAN_POINT('',(-2.77644680466804,0.750000002949537,-6.96716175156718));
#161938=CARTESIAN_POINT('',(-2.58717499223844,0.714243089251773,-7.00153200770937));
#161939=CARTESIAN_POINT('Origin',(-1.37378926289037,0.473612105092906,0.487673478742248));
#161940=CARTESIAN_POINT('',(-2.41797933832242,0.750000003586779,-7.09953350177321));
#161941=CARTESIAN_POINT('Origin',(0.,0.750000005151019,0.));
#161942=CARTESIAN_POINT('Origin',(1.42412805266309,0.692072907189111,-0.28584551893436));
#161943=CARTESIAN_POINT('Ctrl Pts',(-2.505416106,0.940837228,-6.803336691));
#161944=CARTESIAN_POINT('Ctrl Pts',(-2.876502367,0.875180297,-6.66667941000001));
#161945=CARTESIAN_POINT('Ctrl Pts',(-3.230523466,0.809946053,-6.49047133400001));
#161946=CARTESIAN_POINT('Ctrl Pts',(-3.2427676021491,0.807689868361921,
-6.48437702018873));
#161947=CARTESIAN_POINT('Ctrl Pts',(-3.25501173829825,0.805433683723839,
-6.47828270637748));
#161948=CARTESIAN_POINT('Ctrl Pts',(-2.35930162164529,0.940837228000001,
-7.11980219913443));
#161949=CARTESIAN_POINT('Ctrl Pts',(-2.74764941145793,0.875180297,-6.99111469553976));
#161950=CARTESIAN_POINT('Ctrl Pts',(-3.11969647505965,0.809946053,-6.82095164824412));
#161951=CARTESIAN_POINT('Ctrl Pts',(-3.13256405530693,0.807689868361921,
-6.81506640715394));
#161952=CARTESIAN_POINT('Ctrl Pts',(-3.14543163555424,0.805433683723839,
-6.8091811660636));
#161953=CARTESIAN_POINT('',(-3.11992551634625,0.809946052264273,-6.82026869839655));
#161954=CARTESIAN_POINT('Origin',(0.0593207810513757,0.946416086011058,
0.182047336412849));
#161955=CARTESIAN_POINT('',(-3.17522449034723,0.809946053334099,-6.6553700036187));
#161956=CARTESIAN_POINT('Origin',(1.27068494615301E-13,0.901573517999972,
7.12103986888479E-13));
#161957=CARTESIAN_POINT('Origin',(0.0793673685408737,0.803569481651845,
0.175960361352385));
#161958=CARTESIAN_POINT('Origin',(0.030212969465585,0.94634916292647,0.185201735070449));
#161959=CARTESIAN_POINT('Ctrl Pts',(-3.230523466,0.809946053,-6.490471334));
#161960=CARTESIAN_POINT('Ctrl Pts',(-3.58453771,0.875601501000001,-6.314266669));
#161961=CARTESIAN_POINT('Ctrl Pts',(-3.917287119,0.940829639,-6.100603383));
#161962=CARTESIAN_POINT('Ctrl Pts',(-3.560320807,0.809946053,-6.601069288));
#161963=CARTESIAN_POINT('Ctrl Pts',(-3.920367472,0.875601501000001,-6.406876261));
#161964=CARTESIAN_POINT('Ctrl Pts',(-4.257157031,0.940829639,-6.174675215));
#161965=CARTESIAN_POINT('',(-3.56032081704273,0.809946052117963,-6.60106928096141));
#161966=CARTESIAN_POINT('',(-4.04780621259384,0.90066950059267,-6.3138945874699));
#161967=CARTESIAN_POINT('Origin',(0.0905162729336373,0.803573320004725,
0.169997196395875));
#161968=CARTESIAN_POINT('Ctrl Pts',(-3.91332939641532,0.940053944031305,
-6.10314289974884));
#161969=CARTESIAN_POINT('Ctrl Pts',(-3.93567442913333,0.93316823759177,
-6.13824052205359));
#161970=CARTESIAN_POINT('Ctrl Pts',(-3.958066578088,0.926448448694993,-6.17337008654871));
#161971=CARTESIAN_POINT('Ctrl Pts',(-4.00288607856968,0.913330774344538,
-6.24360859109266));
#161972=CARTESIAN_POINT('Ctrl Pts',(-4.02533851098805,0.906925555221556,
-6.27875683049853));
#161973=CARTESIAN_POINT('Ctrl Pts',(-4.04780621106401,0.900669500593302,
-6.31389458844821));
#161974=CARTESIAN_POINT('',(-3.39542215258008,0.809946050062012,-6.54577030265895));
#161975=CARTESIAN_POINT('Origin',(-4.97171748214953E-12,0.714028548000734,
-7.79931674799172E-12));
#161976=CARTESIAN_POINT('',(-4.2092688339877,0.749999999449173,-6.20741939744525));
#161977=CARTESIAN_POINT('',(-4.0318106961935,0.71424308931512,-6.28167393347094));
#161978=CARTESIAN_POINT('Origin',(-1.23682663949029,0.473618831716048,0.771614155931688));
#161979=CARTESIAN_POINT('',(-3.88763818141073,0.750000000078679,-6.41375626069604));
#161980=CARTESIAN_POINT('Origin',(0.,0.750000000000029,0.));
#161981=CARTESIAN_POINT('Origin',(1.32939781459024,0.692075009954695,-0.585293017614466));
#161982=CARTESIAN_POINT('Ctrl Pts',(-3.909357153,0.940837228,-6.105688057));
#161983=CARTESIAN_POINT('Ctrl Pts',(-4.242390347,0.875180297,-5.89245317));
#161984=CARTESIAN_POINT('Ctrl Pts',(-4.550255102,0.809946053,-5.644260669));
#161985=CARTESIAN_POINT('Ctrl Pts',(-4.56090287975081,0.807689868358617,
-5.63567670949461));
#161986=CARTESIAN_POINT('Ctrl Pts',(-4.57155065750173,0.805433683717232,
-5.62709274998908));
#161987=CARTESIAN_POINT('Ctrl Pts',(-3.83468947317919,0.940837228,-6.44616507150536));
#161988=CARTESIAN_POINT('Ctrl Pts',(-4.18629389863377,0.875180297,-6.2370029152431));
#161989=CARTESIAN_POINT('Ctrl Pts',(-4.51306268385293,0.809946053,-5.99083906466819));
#161990=CARTESIAN_POINT('Ctrl Pts',(-4.52436427438713,0.807689868358617,
-5.98232526785112));
#161991=CARTESIAN_POINT('Ctrl Pts',(-4.53566586492127,0.805433683717232,
-5.97381147103415));
#161992=CARTESIAN_POINT('',(-4.51313955625589,0.809946052264272,-5.99012284469398));
#161993=CARTESIAN_POINT('Origin',(0.0970686782388863,0.94641608406807,0.165038954722597));
#161994=CARTESIAN_POINT('',(-4.53169732561459,0.809946053334099,-5.8171917447422));
#161995=CARTESIAN_POINT('Origin',(-1.98625837999344E-13,0.901573518000194,
-1.70436581514721E-13));
#161996=CARTESIAN_POINT('Origin',(0.115336598673815,0.803569483310559,0.154782889231857));
#161997=CARTESIAN_POINT('Origin',(0.0693193576764495,0.946349490873314,
0.174376799761953));
#161998=CARTESIAN_POINT('Ctrl Pts',(-4.550255102,0.809946053,-5.644260669));
#161999=CARTESIAN_POINT('Ctrl Pts',(-4.858113896,0.875601501000001,-5.396072974));
#162000=CARTESIAN_POINT('Ctrl Pts',(-5.13715251700001,0.940829639,-5.115873729));
#162001=CARTESIAN_POINT('Ctrl Pts',(-4.896117256,0.809946053,-5.681376225));
#162002=CARTESIAN_POINT('Ctrl Pts',(-5.206000469,0.875601501000001,-5.414323933));
#162003=CARTESIAN_POINT('Ctrl Pts',(-5.484999715,0.940829639,-5.115151819));
#162004=CARTESIAN_POINT('',(-4.89611726426675,0.809946052007887,-5.68137621598616));
#162005=CARTESIAN_POINT('',(-4.72318619291123,0.809946050061974,-5.66281843539706));
#162006=CARTESIAN_POINT('',(-5.31047145213963,0.900669500617274,-5.29612055723789));
#162007=CARTESIAN_POINT('Origin',(0.124944554358871,0.80357329647491,0.146564579444741));
#162008=CARTESIAN_POINT('Ctrl Pts',(-5.13383324548517,0.940053944149821,
-5.11920466612712));
#162009=CARTESIAN_POINT('Ctrl Pts',(-5.16320081509185,0.933168237703474,
-5.14867820427879));
#162010=CARTESIAN_POINT('Ctrl Pts',(-5.19262126598659,0.926448448811985,
-5.17817280908736));
#162011=CARTESIAN_POINT('Ctrl Pts',(-5.2514921139098,0.913330774430546,
-5.23713430901364));
#162012=CARTESIAN_POINT('Ctrl Pts',(-5.28097545369162,0.906925555263916,
-5.2666341930799));
#162013=CARTESIAN_POINT('Ctrl Pts',(-5.31047145087381,0.900669500617917,
-5.29612055850425));
#162014=CARTESIAN_POINT('Origin',(6.80922332407796E-12,0.714028548,6.68866004249757E-12));
#162015=CARTESIAN_POINT('',(-5.44527015389778,0.75000000074245,-5.15742500300344));
#162016=CARTESIAN_POINT('',(-5.28792341382218,0.714243089165336,-5.26809176682636));
#162017=CARTESIAN_POINT('Origin',(-1.0420408579184,0.473612704232346,1.01945056925008));
#162018=CARTESIAN_POINT('',(-5.17551536390861,0.750000001358042,-5.42807891669345));
#162019=CARTESIAN_POINT('Origin',(0.,0.750000002043061,0.));
#162020=CARTESIAN_POINT('Origin',(1.17249077617713,0.692074247261673,-0.857394588708109));
#162021=CARTESIAN_POINT('Ctrl Pts',(-5.130501005,0.940837228,-5.122544235));
#162022=CARTESIAN_POINT('Ctrl Pts',(-5.40990887,0.875180297,-4.842702369));
#162023=CARTESIAN_POINT('Ctrl Pts',(-5.657221867,0.809946053,-4.534130649));
#162024=CARTESIAN_POINT('Ctrl Pts',(-5.66577540788212,0.807689868409067,
-4.52345842047135));
#162025=CARTESIAN_POINT('Ctrl Pts',(-5.67432894876434,0.805433683818132,
-4.51278619194269));
#162026=CARTESIAN_POINT('Ctrl Pts',(-5.13077150802368,0.940837228,-5.47111243078886));
#162027=CARTESIAN_POINT('Ctrl Pts',(-5.42919193653774,0.875180297000001,
-5.19125581029712));
#162028=CARTESIAN_POINT('Ctrl Pts',(-5.69540309763305,0.809946053,-4.88060150440865));
#162029=CARTESIAN_POINT('Ctrl Pts',(-5.70461024839882,0.807689868409067,
-4.86985724778707));
#162030=CARTESIAN_POINT('Ctrl Pts',(-5.71381739916451,0.805433683818133,
-4.85911299116537));
#162031=CARTESIAN_POINT('',(-5.6953242076193,0.809946052265042,-4.87988550210847));
#162032=CARTESIAN_POINT('Origin',(0.130277874055508,0.946416059068594,0.140313630459598));
#162033=CARTESIAN_POINT('',(-5.67627303080642,0.809946053334091,-4.70700806542456));
#162034=CARTESIAN_POINT('Origin',(-3.98552718605671E-13,0.901573518000056,
-3.54750950837257E-13));
#162035=CARTESIAN_POINT('Origin',(0.14591442777288,0.803569496728868,0.126370695433855));
#162036=CARTESIAN_POINT('Origin',(0.105184722484503,0.946349189289516,0.155398444855144));
#162037=CARTESIAN_POINT('Ctrl Pts',(-5.657221867,0.809946053,-4.534130649));
#162038=CARTESIAN_POINT('Ctrl Pts',(-5.904530075,0.875601501,-4.225564904));
#162039=CARTESIAN_POINT('Ctrl Pts',(-6.116810374,0.940829639,-3.891931506));
#162040=CARTESIAN_POINT('Ctrl Pts',(-6.002976704,0.809946053,-4.496028325));
#162041=CARTESIAN_POINT('Ctrl Pts',(-6.24820667,0.875601501,-4.168603835));
#162042=CARTESIAN_POINT('Ctrl Pts',(-6.456369908,0.940829639,-3.816449609));
#162043=CARTESIAN_POINT('',(-6.00297671011313,0.809946052117936,-4.49602831442525));
#162044=CARTESIAN_POINT('',(-6.3248249481419,0.900669500625308,-4.03070581579533));
#162045=CARTESIAN_POINT('Origin',(0.153530836917978,0.803573322659294,0.116278825060671));
#162046=CARTESIAN_POINT('Ctrl Pts',(-6.11428475835875,0.940053944065295,
-3.89589811327206));
#162047=CARTESIAN_POINT('Ctrl Pts',(-6.149301669923,0.933168237633643,-3.91836941714209));
#162048=CARTESIAN_POINT('Ctrl Pts',(-6.18437475489027,0.926448448797304,
-3.94084992703146));
#162049=CARTESIAN_POINT('Ctrl Pts',(-6.2545442145559,0.913330774423472,
-3.98577744771472));
#162050=CARTESIAN_POINT('Ctrl Pts',(-6.28967985315877,0.906925555268892,
-4.00824959427422));
#162051=CARTESIAN_POINT('Ctrl Pts',(-6.32482494717043,0.900669500625957,
-4.0307058173159));
#162052=CARTESIAN_POINT('',(-5.83009929659162,0.809946050061996,-4.51507947267794));
#162053=CARTESIAN_POINT('Origin',(-7.43242273282263E-12,0.714028547999266,
-4.59875193481452E-12));
#162054=CARTESIAN_POINT('',(-6.42665668287943,0.749999999391371,-3.8662751550363));
#162055=CARTESIAN_POINT('',(-6.29677870903883,0.714243089259356,-4.00817948512182));
#162056=CARTESIAN_POINT('Origin',(-0.798522356592828,0.473612937660149,
1.21962839912454));
#162057=CARTESIAN_POINT('',(-6.22139120767294,0.750000000236834,-4.18859062748345));
#162058=CARTESIAN_POINT('Origin',(0.,0.750000000000029,0.));
#162059=CARTESIAN_POINT('Origin',(0.960772761012999,0.692075178873913,-1.08939629753758));
#162060=CARTESIAN_POINT('Ctrl Pts',(-6.111748332,0.940837228,-3.899875938));
#162061=CARTESIAN_POINT('Ctrl Pts',(-6.324466068,0.875180297,-3.566512188));
#162062=CARTESIAN_POINT('Ctrl Pts',(-6.499663225,0.809946053,-3.211989719));
#162063=CARTESIAN_POINT('Ctrl Pts',(-6.50572257530016,0.807689868352189,
-3.1997282424684));
#162064=CARTESIAN_POINT('Ctrl Pts',(-6.51178192560047,0.805433683704377,
-3.18746676593687));
#162065=CARTESIAN_POINT('Ctrl Pts',(-6.18694436872785,0.940837228,-4.24023665216015));
#162066=CARTESIAN_POINT('Ctrl Pts',(-6.41822699307382,0.875180297000001,
-3.90277135386781));
#162067=CARTESIAN_POINT('Ctrl Pts',(-6.61143279187626,0.809946053,-3.54215244291236));
#162068=CARTESIAN_POINT('Ctrl Pts',(-6.61811498715281,0.807689868352189,
-3.52968011548556));
#162069=CARTESIAN_POINT('Ctrl Pts',(-6.62479718242936,0.805433683704377,
-3.51720778805875));
#162070=CARTESIAN_POINT('',(-6.6112018269334,0.809946052265044,-3.54147013934983));
#162071=CARTESIAN_POINT('Origin',(0.157395165769212,0.946416051811995,0.109027188938045));
#162072=CARTESIAN_POINT('',(-6.55543251743721,0.809946053334091,-3.37672992068055));
#162073=CARTESIAN_POINT('Origin',(1.56125112837913E-14,0.901573518000056,
-2.27682456221956E-14));
#162074=CARTESIAN_POINT('Origin',(0.169668356951714,0.803569306176809,0.0920486297458446));
#162075=CARTESIAN_POINT('Origin',(0.136131335377041,0.946349429981463,0.129153532124544));
#162076=CARTESIAN_POINT('Ctrl Pts',(-6.499663225,0.809946053,-3.211989719));
#162077=CARTESIAN_POINT('Ctrl Pts',(-6.674856991,0.875601501,-2.857474115));
#162078=CARTESIAN_POINT('Ctrl Pts',(-6.810452976,0.940829639,-2.486006892));
#162079=CARTESIAN_POINT('Ctrl Pts',(-6.829143632,0.809946053,-3.100451136));
#162080=CARTESIAN_POINT('Ctrl Pts',(-6.998253672,0.875601501,-2.727964456));
#162081=CARTESIAN_POINT('Ctrl Pts',(-7.125847419,0.940829639,-2.339294456));
#162082=CARTESIAN_POINT('',(-6.8291436357368,0.809946052117954,-3.10045112431753));
#162083=CARTESIAN_POINT('',(-7.04343665893579,0.900669500612243,-2.57681975023539));
#162084=CARTESIAN_POINT('Origin',(0.174937395336665,0.803573296031086,0.0805555129405777));
#162085=CARTESIAN_POINT('Ctrl Pts',(-6.8088391104413,0.940053944145248,
-2.49042369485089));
#162086=CARTESIAN_POINT('Ctrl Pts',(-6.8478680119646,0.933168237710336,
-2.50484203093422));
#162087=CARTESIAN_POINT('Ctrl Pts',(-6.88695375326514,0.92644844877595,
-2.51925728249278));
#162088=CARTESIAN_POINT('Ctrl Pts',(-6.96514077864709,0.913330774422057,
-2.54805006275026));
#162089=CARTESIAN_POINT('Ctrl Pts',(-7.00428581293043,0.906925555246983,
-2.56244369927751));
#162090=CARTESIAN_POINT('Ctrl Pts',(-7.04343665832799,0.90066950061289,
-2.57681975189093));
#162091=CARTESIAN_POINT('',(-6.66440343625349,0.809946050061996,-3.15622041112841));
#162092=CARTESIAN_POINT('Origin',(-5.22889023746309E-12,0.714028547999755,
-2.12872254545804E-12));
#162093=CARTESIAN_POINT('',(-7.10753989224886,0.749999998867154,-2.39434257513311));
#162094=CARTESIAN_POINT('',(-7.01120363025577,0.714243089287394,-2.56084918553649));
#162095=CARTESIAN_POINT('Origin',(-0.517668238337649,0.473612986217688,
1.36277345844869));
#162096=CARTESIAN_POINT('',(-6.97636171019226,0.749999999742988,-2.75324849672299));
#162097=CARTESIAN_POINT('Origin',(0.,0.749999999161366,0.));
#162098=CARTESIAN_POINT('Origin',(0.704122757021434,0.69207529282193,-1.27046448369264));
#162099=CARTESIAN_POINT('Ctrl Pts',(-6.807217099,0.940837228,-2.494853776));
#162100=CARTESIAN_POINT('Ctrl Pts',(-6.94329826,0.875180297,-2.12355586));
#162101=CARTESIAN_POINT('Ctrl Pts',(-7.038187555,0.809946053,-1.73965972));
#162102=CARTESIAN_POINT('Ctrl Pts',(-7.04146938600978,0.807689868412916,
-1.72638232915434));
#162103=CARTESIAN_POINT('Ctrl Pts',(-7.04475121701958,0.80543368382583,
-1.71310493830869));
#162104=CARTESIAN_POINT('Ctrl Pts',(-6.95382258706004,0.940837228000001,
-2.81109212166392));
#162105=CARTESIAN_POINT('Ctrl Pts',(-7.10715288826948,0.875180297,-2.43179764591034));
#162106=CARTESIAN_POINT('Ctrl Pts',(-7.21831923755849,0.809946053,-2.03807626899811));
#162107=CARTESIAN_POINT('Ctrl Pts',(-7.22216402502731,0.807689868412915,
-2.02445906355928));
#162108=CARTESIAN_POINT('Ctrl Pts',(-7.22600881249612,0.805433683825832,
-2.01084185812038));
#162109=CARTESIAN_POINT('',(-7.2179469973611,0.809946052265047,-2.03745956795825));
#162110=CARTESIAN_POINT('Origin',(0.177153184908597,0.946416038992782,0.0726429565010295));
#162111=CARTESIAN_POINT('',(-7.12806726602417,0.809946053334091,-1.88855963752162));
#162112=CARTESIAN_POINT('Origin',(-3.76001313417973E-13,0.901573517999806,
-6.46184494801361E-14));
#162113=CARTESIAN_POINT('Origin',(0.185488957796006,0.803569127013547,0.0534228253417359));
#162114=CARTESIAN_POINT('Origin',(0.160712844055243,0.946349502133253,0.0968698011685543));
#162115=CARTESIAN_POINT('Ctrl Pts',(-7.038187555,0.809946053,-1.73965972));
#162116=CARTESIAN_POINT('Ctrl Pts',(-7.133075012,0.875601501,-1.355771012));
#162117=CARTESIAN_POINT('Ctrl Pts',(-7.185646366,0.940829639,-0.963839358));
#162118=CARTESIAN_POINT('Ctrl Pts',(-7.335987395,0.809946053,-1.559900299));
#162119=CARTESIAN_POINT('Ctrl Pts',(-7.42107011,0.875601501,-1.15976849));
#162120=CARTESIAN_POINT('Ctrl Pts',(-7.462128226,0.940829639,-0.752756495));
#162121=CARTESIAN_POINT('',(-7.33598739610994,0.809946052007895,-1.5599002868475));
#162122=CARTESIAN_POINT('',(-7.43270510030618,0.900669500577752,-1.00244445737222));
#162123=CARTESIAN_POINT('Origin',(0.188164822724248,0.803573315666638,0.0410658480750598));
#162124=CARTESIAN_POINT('Ctrl Pts',(-7.18501971321784,0.940053944258733,
-0.968499831650855));
#162125=CARTESIAN_POINT('Ctrl Pts',(-7.22623565673749,0.933168237835753,
-0.974191014905439));
#162126=CARTESIAN_POINT('Ctrl Pts',(-7.26750644861614,0.926448448817741,
-0.979866966976774));
#162127=CARTESIAN_POINT('Ctrl Pts',(-7.35005510155544,0.913330774439853,
-0.991178688866976));
#162128=CARTESIAN_POINT('Ctrl Pts',(-7.39137915317629,0.906925555242182,
-0.996820784991662));
#162129=CARTESIAN_POINT('Ctrl Pts',(-7.43270510007076,0.900669500578381,
-1.00244445910288));
#162130=CARTESIAN_POINT('',(-7.18708747905281,0.809946050061996,-1.6497799918444));
#162131=CARTESIAN_POINT('Origin',(1.55084278752327E-12,0.714028547998288,
3.34855840972148E-13));
#162132=CARTESIAN_POINT('',(-7.45608243706208,0.749999999447828,-0.810453196812189));
#162133=CARTESIAN_POINT('',(-7.39779246228466,0.714243089163989,-0.99377642309357));
#162134=CARTESIAN_POINT('Origin',(-0.212611893476207,0.47361691107108,1.44219440505136));
#162135=CARTESIAN_POINT('',(-7.40512529159642,0.750000000292744,-1.18916753241498));
#162136=CARTESIAN_POINT('Origin',(0.,0.750000000000029,0.));
#162137=CARTESIAN_POINT('Origin',(0.414546568407169,0.692075061657456,-1.39212726711968));
#162138=CARTESIAN_POINT('Ctrl Pts',(-7.184387961,0.940837228,-0.973175025));
#162139=CARTESIAN_POINT('Ctrl Pts',(-7.237469544,0.875180297,-0.581304421));
#162140=CARTESIAN_POINT('Ctrl Pts',(-7.24761405700001,0.809946053,-0.185985165));
#162141=CARTESIAN_POINT('Ctrl Pts',(-7.24796491404188,0.807689868412287,
-0.172312695482098));
#162142=CARTESIAN_POINT('Ctrl Pts',(-7.2483157710839,0.805433683824573,
-0.158640225964204));
#162143=CARTESIAN_POINT('Ctrl Pts',(-7.3955477905724,0.940837228,-1.25050404734907));
#162144=CARTESIAN_POINT('Ctrl Pts',(-7.46375621382,0.875180297000001,-0.847115783862962));
#162145=CARTESIAN_POINT('Ctrl Pts',(-7.4876850977098,0.809946053,-0.438701914431369));
#162146=CARTESIAN_POINT('Ctrl Pts',(-7.48851269952937,0.807689868412287,
-0.424576556013486));
#162147=CARTESIAN_POINT('Ctrl Pts',(-7.48934030134893,0.805433683824576,
-0.410451197595596));
#162148=CARTESIAN_POINT('',(-7.48718898778801,0.809946052265052,-0.438179652160465));
#162149=CARTESIAN_POINT('Origin',(0.188627531184321,0.946416067397882,0.0328619060441109));
#162150=CARTESIAN_POINT('',(-7.36740151108662,0.809946053334091,-0.312082404455189));
#162151=CARTESIAN_POINT('Origin',(-4.90926743701436E-13,0.901573517999861,
-5.01443504774546E-14));
#162152=CARTESIAN_POINT('Origin',(0.192637052573005,0.803569461496135,0.0122991578322531));
#162153=CARTESIAN_POINT('Origin',(0.177779897331626,0.946349182381831,0.0600565242311453));
#162154=CARTESIAN_POINT('Ctrl Pts',(-7.247614057,0.809946053,-0.185985165));
#162155=CARTESIAN_POINT('Ctrl Pts',(-7.257758374,0.875601501,0.209326436));
#162156=CARTESIAN_POINT('Ctrl Pts',(-7.224846918,0.940829639,0.603396233));
#162157=CARTESIAN_POINT('Ctrl Pts',(-7.49980854,0.809946053,0.053589743));
#162158=CARTESIAN_POINT('Ctrl Pts',(-7.496885558,0.875601501,0.462656961));
#162159=CARTESIAN_POINT('Ctrl Pts',(-7.44948821,0.940829639,0.868979523));
#162160=CARTESIAN_POINT('',(-7.49980853848092,0.809946052117954,0.0535897551571855));
#162161=CARTESIAN_POINT('',(-7.47442851167214,0.90066950059978,0.618804024144828));
#162162=CARTESIAN_POINT('Origin',(0.19259339066803,0.803573308386867,-0.000344107343095319));
#162163=CARTESIAN_POINT('Ctrl Pts',(-7.22523678067821,0.940053944158219,
0.598710006831233));
#162164=CARTESIAN_POINT('Ctrl Pts',(-7.26671255469412,0.933168237733409,
0.602012089818992));
#162165=CARTESIAN_POINT('Ctrl Pts',(-7.30823861989039,0.926448448798157,
0.605340838600035));
#162166=CARTESIAN_POINT('Ctrl Pts',(-7.3912890171494,0.913330774413794,
0.612039098687823));
#162167=CARTESIAN_POINT('Ctrl Pts',(-7.43285981896345,0.906925555263889,
0.615412361129273));
#162168=CARTESIAN_POINT('Ctrl Pts',(-7.47442851182048,0.900669500600411,
0.618804022327912));
#162169=CARTESIAN_POINT('',(-7.37371129866262,0.809946050061996,-0.0661976928859446));
#162170=CARTESIAN_POINT('Origin',(8.59208537651313E-12,0.714028548000978,
-4.4278816724308E-13));
#162171=CARTESIAN_POINT('',(-7.45598684901459,0.749999993899794,0.811332053920997));
#162172=CARTESIAN_POINT('',(-7.43846874078927,0.714243089245729,0.619764219404089));
#162173=CARTESIAN_POINT('Origin',(0.102370559289628,0.473612122600343,1.45418114526299));
#162174=CARTESIAN_POINT('',(-7.48763343938384,0.749999995439564,0.4305176098096));
#162175=CARTESIAN_POINT('Origin',(0.,0.749999993327366,0.));
#162176=CARTESIAN_POINT('Origin',(0.105594438791012,0.69207569376148,-1.44869683082552));
#162177=CARTESIAN_POINT('Ctrl Pts',(-7.225624826,0.940837228,0.594008309));
#162178=CARTESIAN_POINT('Ctrl Pts',(-7.193224795,0.875180297,0.988128168));
#162179=CARTESIAN_POINT('Ctrl Pts',(-7.118150181,0.809946053,1.376385849));
#162180=CARTESIAN_POINT('Ctrl Pts',(-7.11555365842227,0.807689868407598,
1.38981408766792));
#162181=CARTESIAN_POINT('Ctrl Pts',(-7.11295713584455,0.805433683815197,
1.40324232633587));
#162182=CARTESIAN_POINT('Ctrl Pts',(-7.49146539822841,0.940837228000001,
0.368556206903295));
#162183=CARTESIAN_POINT('Ctrl Pts',(-7.47136259377401,0.875180297,0.777176271142086));
#162184=CARTESIAN_POINT('Ctrl Pts',(-7.40693512424696,0.809946053,1.18118565373313));
#162185=CARTESIAN_POINT('Ctrl Pts',(-7.40470684267029,0.807689868407598,
1.19515867906914));
#162186=CARTESIAN_POINT('Ctrl Pts',(-7.40247856109349,0.805433683815198,
1.20913170440515));
#162187=CARTESIAN_POINT('',(-7.40633834297572,0.809946052264265,1.18158905489033));
#162188=CARTESIAN_POINT('Origin',(0.191281854905171,0.946416077062279,-0.00845573081088166));
#162189=CARTESIAN_POINT('',(-7.26224424964502,0.809946053334091,1.27898745451562));
#162190=CARTESIAN_POINT('Origin',(1.35958952429682E-12,0.901573518000083,
-9.95975220699497E-14));
#162191=CARTESIAN_POINT('Origin',(0.190772156346956,0.803567066281397,-0.0293984664076719));
#162192=CARTESIAN_POINT('Origin',(0.186530734540632,0.946349387717187,0.0204350879223742));
#162193=CARTESIAN_POINT('Ctrl Pts',(-7.118150181,0.809946053,1.376385849));
#162194=CARTESIAN_POINT('Ctrl Pts',(-7.04307702,0.875601501,1.764636013));
#162195=CARTESIAN_POINT('Ctrl Pts',(-6.926221658,0.940829639,2.142417687));
#162196=CARTESIAN_POINT('Ctrl Pts',(-7.312946974,0.809946053,1.664573988));
#162197=CARTESIAN_POINT('Ctrl Pts',(-7.222154969,0.875601501,2.063449087));
#162198=CARTESIAN_POINT('Ctrl Pts',(-7.088518405,0.940829639,2.450083024));
#162199=CARTESIAN_POINT('',(-7.31294696989878,0.809946052117947,1.66457399951245));
#162200=CARTESIAN_POINT('',(-7.16665595331403,0.900669500631217,2.21111791752741));
#162201=CARTESIAN_POINT('Origin',(0.188016845196407,0.803573325729783,-0.0417380006118342));
#162202=CARTESIAN_POINT('Ctrl Pts',(-6.92760980580542,0.940053944212052,
2.13792483126068));
#162203=CARTESIAN_POINT('Ctrl Pts',(-6.96740604904775,0.933168237787557,
2.15006577861116));
#162204=CARTESIAN_POINT('Ctrl Pts',(-7.00724567548623,0.926448448831224,
2.16224357956276));
#162205=CARTESIAN_POINT('Ctrl Pts',(-7.08691447273129,0.913330774457708,
2.18663861842916));
#162206=CARTESIAN_POINT('Ctrl Pts',(-7.12678822078421,0.90692555528841,
2.1988695094987));
#162207=CARTESIAN_POINT('Ctrl Pts',(-7.1666559538467,0.900669500631857,
2.21111791579394));
#162208=CARTESIAN_POINT('',(-7.21554857376483,0.809946050061996,1.52047993622552));
#162209=CARTESIAN_POINT('Origin',(6.07066480418084E-12,0.714028547999755,
-1.82102596890665E-12));
#162210=CARTESIAN_POINT('',(-7.10725761130664,0.749999998991949,2.39518035554988));
#162211=CARTESIAN_POINT('',(-7.13133048835984,0.714243089300439,2.20432537570086));
#162212=CARTESIAN_POINT('Origin',(0.412603354274212,0.473613015875695,1.39817395588609));
#162213=CARTESIAN_POINT('',(-7.22002817973684,0.749999999822909,2.03007218619174));
#162214=CARTESIAN_POINT('Origin',(0.,0.749999999379636,0.));
#162215=CARTESIAN_POINT('Origin',(-0.208305057603325,0.692075220411731,
-1.43752493983075));
#162216=CARTESIAN_POINT('Ctrl Pts',(-6.928999505,0.940837228,2.133416475));
#162217=CARTESIAN_POINT('Ctrl Pts',(-6.81263284900001,0.875180297,2.511356981));
#162218=CARTESIAN_POINT('Ctrl Pts',(-6.655849513,0.809946053,2.874398591));
#162219=CARTESIAN_POINT('Ctrl Pts',(-6.65042702125904,0.807689868393002,
2.88695470941201));
#162220=CARTESIAN_POINT('Ctrl Pts',(-6.64500452951808,0.805433683786001,
2.89951082782398));
#162221=CARTESIAN_POINT('Ctrl Pts',(-7.23709041010449,0.940837228,1.97038318210572));
#162222=CARTESIAN_POINT('Ctrl Pts',(-7.12961636364179,0.875180297,2.3651284279141));
#162223=CARTESIAN_POINT('Ctrl Pts',(-6.97984509784159,0.809946053,2.74584229453961));
#162224=CARTESIAN_POINT('Ctrl Pts',(-6.97466512481288,0.807689868393001,
2.75900962373485));
#162225=CARTESIAN_POINT('Ctrl Pts',(-6.96948515178403,0.805433683786001,
2.77217695293011));
#162226=CARTESIAN_POINT('',(-6.97917554963226,0.809946052264273,2.7461079740992));
#162227=CARTESIAN_POINT('Origin',(0.184991985497199,0.946416080281647,-0.0493779501458091));
#162228=CARTESIAN_POINT('',(-6.81751251872002,0.809946053334091,2.81025328239219));
#162229=CARTESIAN_POINT('Origin',(-1.13407547241984E-12,0.901573518,4.45823933326039E-13));
#162230=CARTESIAN_POINT('Origin',(0.179996582079746,0.803569217500806,-0.0697236045505898));
#162231=CARTESIAN_POINT('Origin',(0.186565303897439,0.946349423399718,-0.0201418751128665));
#162232=CARTESIAN_POINT('Ctrl Pts',(-6.655849513,0.809946053,2.874398591));
#162233=CARTESIAN_POINT('Ctrl Pts',(-6.499069213,0.875601501,3.237433171));
#162234=CARTESIAN_POINT('Ctrl Pts',(-6.303733971,0.940829639,3.581262071));
#162235=CARTESIAN_POINT('Ctrl Pts',(-6.784140134,0.809946053,3.197724603));
#162236=CARTESIAN_POINT('Ctrl Pts',(-6.609724441,0.875601501,3.567756627));
#162237=CARTESIAN_POINT('Ctrl Pts',(-6.396097357,0.940829639,3.916623367));
#162238=CARTESIAN_POINT('',(-6.78414012751564,0.809946052117958,3.19772461340661));
#162239=CARTESIAN_POINT('',(-6.52377852755123,0.900669500602261,3.70004239467368));
#162240=CARTESIAN_POINT('Origin',(0.174648437993212,0.803573303207944,-0.0811801132144108));
#162241=CARTESIAN_POINT('Ctrl Pts',(-6.30605549606934,0.940053944170996,
3.57717266655217));
#162242=CARTESIAN_POINT('Ctrl Pts',(-6.3423113804959,0.933168237742285,
3.59758478126356));
#162243=CARTESIAN_POINT('Ctrl Pts',(-6.37860171123587,0.92644844881477,
3.61804221396549));
#162244=CARTESIAN_POINT('Ctrl Pts',(-6.45116368405659,0.913330774441575,
3.65899334681766));
#162245=CARTESIAN_POINT('Ctrl Pts',(-6.48747592609581,0.906925555257983,
3.67950996366937));
#162246=CARTESIAN_POINT('Ctrl Pts',(-6.523778528422,0.900669500602901,3.70004239313431));
#162247=CARTESIAN_POINT('',(-6.71999481604169,0.809946050061996,3.03606161350816));
#162248=CARTESIAN_POINT('Origin',(1.29674916637956E-11,0.714028548000978,
-7.12841244365769E-12));
#162249=CARTESIAN_POINT('',(-6.42620090260971,0.749999999423274,3.86703266739492));
#162250=CARTESIAN_POINT('',(-6.49073914757855,0.714243089136802,3.68581472836303));
#162251=CARTESIAN_POINT('Origin',(0.703519225223311,0.473616182160146,1.27678862258471));
#162252=CARTESIAN_POINT('',(-6.61482242335707,0.750000000270831,3.53470286042756));
#162253=CARTESIAN_POINT('Origin',(0.,0.750000000000029,0.));
#162254=CARTESIAN_POINT('Origin',(-0.512460977771081,0.692075222204829,
-1.35913646868323));
#162255=CARTESIAN_POINT('Ctrl Pts',(-6.308381869,0.940837228,3.573068457));
#162256=CARTESIAN_POINT('Ctrl Pts',(-6.113489763,0.875180297,3.917157533));
#162257=CARTESIAN_POINT('Ctrl Pts',(-5.88232872,0.809946053,4.238007649));
#162258=CARTESIAN_POINT('Ctrl Pts',(-5.87433380866454,0.807689868350337,
4.24910453710929));
#162259=CARTESIAN_POINT('Ctrl Pts',(-5.86633889732895,0.805433683700671,
4.26020142521853));
#162260=CARTESIAN_POINT('Ctrl Pts',(-6.64431711846015,0.940837228,3.48007722958934));
#162261=CARTESIAN_POINT('Ctrl Pts',(-6.45449719567435,0.875180297,3.84248980808543));
#162262=CARTESIAN_POINT('Ctrl Pts',(-6.22638527100657,0.809946053,4.18210640003399));
#162263=CARTESIAN_POINT('Ctrl Pts',(-6.21849581615458,0.807689868350337,
4.19385234349162));
#162264=CARTESIAN_POINT('Ctrl Pts',(-6.21060636130262,0.805433683700673,
4.20559828694927));
#162265=CARTESIAN_POINT('',(-6.22567426167375,0.809946052265036,4.18222193646299));
#162266=CARTESIAN_POINT('Origin',(0.170052079903854,0.946416046042726,-0.0879912919240844));
#162267=CARTESIAN_POINT('',(-6.05400147933149,0.809946053334091,4.21011478918027));
#162268=CARTESIAN_POINT('Origin',(1.12713657851593E-12,0.901573518000139,
-5.95226992694542E-13));
#162269=CARTESIAN_POINT('Origin',(0.160800309337056,0.803569514372434,-0.106787821028391));
#162270=CARTESIAN_POINT('Origin',(0.177873690556483,0.946349453047268,-0.0597770055129204));
#162271=CARTESIAN_POINT('Ctrl Pts',(-5.88232872,0.809946053,4.238007649));
#162272=CARTESIAN_POINT('Ctrl Pts',(-5.651172152,0.875601501,4.55885155200001));
#162273=CARTESIAN_POINT('Ctrl Pts',(-5.38649069,0.940829639,4.85265062));
#162274=CARTESIAN_POINT('Ctrl Pts',(-5.938114442,0.809946053,4.58135317));
#162275=CARTESIAN_POINT('Ctrl Pts',(-5.688230544,0.875601501,4.905239832));
#162276=CARTESIAN_POINT('Ctrl Pts',(-5.404601906,0.940829639,5.200026753));
#162277=CARTESIAN_POINT('',(-5.93811443344712,0.809946052007899,4.58135317874226));
#162278=CARTESIAN_POINT('',(-5.57585646849975,0.900669500631655,5.01595700132481));
#162279=CARTESIAN_POINT('Origin',(0.153113955462107,0.803573294511166,-0.116826443349924));
#162280=CARTESIAN_POINT('Ctrl Pts',(-5.3896370410399,0.940053943979818,
4.84915588374515));
#162281=CARTESIAN_POINT('Ctrl Pts',(-5.42065728185389,0.933168237522385,
4.8768847182855));
#162282=CARTESIAN_POINT('Ctrl Pts',(-5.45170142069717,0.926448448772325,
4.9046652153187));
#162283=CARTESIAN_POINT('Ctrl Pts',(-5.5137636518489,0.913330774406861,
4.96025761277208));
#162284=CARTESIAN_POINT('Ctrl Pts',(-5.54481646756075,0.906925555254912,
4.98810062106575));
#162285=CARTESIAN_POINT('Ctrl Pts',(-5.57585646965406,0.900669500636448,
5.01595699999707));
#162286=CARTESIAN_POINT('',(-5.9102215701673,0.809946050061996,4.40968042401888));
#162287=CARTESIAN_POINT('Origin',(3.37403716077489E-12,0.714028547998533,
-2.77989437025283E-12));
#162288=CARTESIAN_POINT('',(-5.44466217806886,0.750000000797388,5.15806683544274));
#162289=CARTESIAN_POINT('',(-5.54664805887057,0.714243089237145,4.99495947994093));
#162290=CARTESIAN_POINT('Origin',(0.961541774337511,0.473612790912695,1.09570374294362));
#162291=CARTESIAN_POINT('',(-5.70031492472452,0.750000001422546,4.87405475630863));
#162292=CARTESIAN_POINT('Origin',(0.,0.750000002126994,0.));
#162293=CARTESIAN_POINT('Origin',(-0.792659925892832,0.692074230931837,
-1.21718943245041));
#162294=CARTESIAN_POINT('Ctrl Pts',(-5.392791307,0.940837228,4.845647729));
#162295=CARTESIAN_POINT('Ctrl Pts',(-5.128486691,0.875180297,5.139796152));
#162296=CARTESIAN_POINT('Ctrl Pts',(-4.833756773,0.809946053,5.403452179));
#162297=CARTESIAN_POINT('Ctrl Pts',(-4.82356327583318,0.807689868470432,
5.412570957923));
#162298=CARTESIAN_POINT('Ctrl Pts',(-4.81336977866643,0.805433683940862,
5.421689736846));
#162299=CARTESIAN_POINT('Ctrl Pts',(-5.74086294257407,0.940837228000001,
4.82704673403782));
#162300=CARTESIAN_POINT('Ctrl Pts',(-5.47757291232495,0.875180297000001,
5.1401806345747));
#162301=CARTESIAN_POINT('Ctrl Pts',(-5.18178659015179,0.809946053,5.42281985940034));
#162302=CARTESIAN_POINT('Ctrl Pts',(-5.17155655630415,0.807689868470432,
5.43259518915661));
#162303=CARTESIAN_POINT('Ctrl Pts',(-5.16132652245651,0.805433683940861,
5.44237051891284));
#162304=CARTESIAN_POINT('',(-5.18106736691782,0.809946052265036,5.42277984867541));
#162305=CARTESIAN_POINT('Origin',(0.147161080574969,0.946416070009224,-0.122490500035624));
#162306=CARTESIAN_POINT('',(-5.0074120594976,0.809946053334091,5.4131160078898));
#162307=CARTESIAN_POINT('Origin',(3.17020715234761E-13,0.901573518000139,
-3.02275565688959E-13));
#162308=CARTESIAN_POINT('Origin',(0.134085142685041,0.803569523315697,-0.138858993640414));
#162309=CARTESIAN_POINT('Origin',(0.160865042239952,0.946349178674713,-0.0966172917225144));
#162310=CARTESIAN_POINT('Ctrl Pts',(-4.833756773,0.809946053,5.403452179));
#162311=CARTESIAN_POINT('Ctrl Pts',(-4.539032563,0.875601501,5.667103101));
#162312=CARTESIAN_POINT('Ctrl Pts',(-4.217381091,0.940829639,5.89713462));
#162313=CARTESIAN_POINT('Ctrl Pts',(-4.814429119,0.809946053,5.750762755));
#162314=CARTESIAN_POINT('Ctrl Pts',(-4.500761309,0.875601501,6.013359475));
#162315=CARTESIAN_POINT('Ctrl Pts',(-4.160393277,0.940829639,6.240282668));
#162316=CARTESIAN_POINT('',(-4.81442910876821,0.809946052117945,5.75076276168269));
#162317=CARTESIAN_POINT('',(-4.36721355850133,0.90066950062204,6.09733103335733));
#162318=CARTESIAN_POINT('Origin',(0.124420020444259,0.803573308344962,-0.147010115980704));
#162319=CARTESIAN_POINT('Ctrl Pts',(-4.22120514702725,0.94005394400724,
5.89439796090951));
#162320=CARTESIAN_POINT('Ctrl Pts',(-4.24553927219527,0.933168237550762,
5.92814694546217));
#162321=CARTESIAN_POINT('Ctrl Pts',(-4.26988563088799,0.926448448753514,
5.96195152229541));
#162322=CARTESIAN_POINT('Ctrl Pts',(-4.31854615956295,0.913330774374134,
6.02958574554369));
#162323=CARTESIAN_POINT('Ctrl Pts',(-4.34288755386442,0.906925555252343,
6.06345323705642));
#162324=CARTESIAN_POINT('Ctrl Pts',(-4.36721355998907,0.900669500622685,
6.09733103228917));
#162325=CARTESIAN_POINT('',(-4.82409293229943,0.809946050061996,5.57710747885074));
#162326=CARTESIAN_POINT('Origin',(-1.24032728532342E-13,0.714028548000245,
3.13984949151802E-13));
#162327=CARTESIAN_POINT('',(-4.20853710845448,0.749999998091708,6.20791551735464));
#162328=CARTESIAN_POINT('',(-4.34320187174526,0.714243089326984,6.0705454777832));
#162329=CARTESIAN_POINT('Origin',(1.17460218335671,0.47361248030911,0.863386897244571));
#162330=CARTESIAN_POINT('',(-4.51926702152341,0.749999998623412,5.98550127963007));
#162331=CARTESIAN_POINT('Origin',(0.,0.749999997908146,0.));
#162332=CARTESIAN_POINT('Origin',(-1.03578289774064,0.692075300936382,-1.018343469197));
#162333=CARTESIAN_POINT('Ctrl Pts',(-4.225039818,0.940837228,5.891649899));
#162334=CARTESIAN_POINT('Ctrl Pts',(-3.903681281,0.875180297,6.122103616));
#162335=CARTESIAN_POINT('Ctrl Pts',(-3.559163733,0.809946053,6.316237292));
#162336=CARTESIAN_POINT('Ctrl Pts',(-3.54724828593257,0.807689868414112,
6.32295157855468));
#162337=CARTESIAN_POINT('Ctrl Pts',(-3.53533283886516,0.805433683828222,
6.32966586510928));
#162338=CARTESIAN_POINT('Ctrl Pts',(-4.56897239578246,0.940837228,5.94830889693276));
#162339=CARTESIAN_POINT('Ctrl Pts',(-4.24452340803253,0.875180297,6.19752232790587));
#162340=CARTESIAN_POINT('Ctrl Pts',(-3.89489332643019,0.809946053,6.40996828921937));
#162341=CARTESIAN_POINT('Ctrl Pts',(-3.88280105782242,0.807689868414112,
6.41731592251532));
#162342=CARTESIAN_POINT('Ctrl Pts',(-3.87070878921457,0.805433683828225,
6.42466355581122));
#162343=CARTESIAN_POINT('',(-3.89419951934794,0.809946052265047,6.40977460218573));
#162344=CARTESIAN_POINT('Origin',(0.117388635218625,0.946416084216885,-0.151261912564934));
#162345=CARTESIAN_POINT('',(-3.72668161723396,0.809946053334091,6.36300593903434));
#162346=CARTESIAN_POINT('Origin',(-7.9580439460436E-14,0.901573517999945,
1.06251812903579E-13));
#162347=CARTESIAN_POINT('Origin',(0.101098668520509,0.803568548821323,-0.164434834408524));
#162348=CARTESIAN_POINT('Origin',(0.13633379929227,0.94634946544834,-0.128939078902941));
#162349=CARTESIAN_POINT('Ctrl Pts',(-3.559163733,0.809946053,6.316237292));
#162350=CARTESIAN_POINT('Ctrl Pts',(-3.214652856,0.875601501,6.51036720800001));
#162351=CARTESIAN_POINT('Ctrl Pts',(-2.85107144,0.940829639,6.66587516));
#162352=CARTESIAN_POINT('Ctrl Pts',(-3.465626441,0.809946053,6.651273064));
#162353=CARTESIAN_POINT('Ctrl Pts',(-3.102841477,0.875601501,6.840301112));
#162354=CARTESIAN_POINT('Ctrl Pts',(-2.721649282,0.940829639,6.988749902));
#162355=CARTESIAN_POINT('',(-3.46562642958225,0.809946052007886,6.65127306832622));
#162356=CARTESIAN_POINT('',(-2.95436459608682,0.90066950062014,6.89360064336847));
#162357=CARTESIAN_POINT('Origin',(0.0899083630963088,0.803573330762241,
-0.170319809647436));
#162358=CARTESIAN_POINT('Ctrl Pts',(-2.85539439212087,0.940053944205486,
6.66402454021118));
#162359=CARTESIAN_POINT('Ctrl Pts',(-2.87190456469636,0.933168237788074,
6.70221560956731));
#162360=CARTESIAN_POINT('Ctrl Pts',(-2.88841473462254,0.926448448815871,
6.74046360253844));
#162361=CARTESIAN_POINT('Ctrl Pts',(-2.92139824827267,0.913330774428465,
6.81697715038138));
#162362=CARTESIAN_POINT('Ctrl Pts',(-2.93789004469382,0.906925555292992,
6.85528551900787));
#162363=CARTESIAN_POINT('Ctrl Pts',(-2.95436459778852,0.900669500620776,
6.89360064263689));
#162364=CARTESIAN_POINT('',(-3.51239507107219,0.809946050061996,6.48375518662845));
#162365=CARTESIAN_POINT('Origin',(3.7398469737715E-12,0.714028548000245,
-8.67752050770498E-12));
#162366=CARTESIAN_POINT('',(-2.77562550215833,0.750000003027913,6.96748898868309));
#162367=CARTESIAN_POINT('',(-2.93667239101668,0.714243089168973,6.8622795164615));
#162368=CARTESIAN_POINT('Origin',(1.33273820257263,0.473612193361007,0.590704469769952));
#162369=CARTESIAN_POINT('',(-3.12690324859456,0.750000003690145,6.81707239937356));
#162370=CARTESIAN_POINT('Origin',(0.,0.750000005282026,0.));
#162371=CARTESIAN_POINT('Origin',(-1.23048643239192,0.692072905717779,-0.771849190163528));
#162372=CARTESIAN_POINT('Ctrl Pts',(-2.859730162,0.940837228,6.662165068));
#162373=CARTESIAN_POINT('Ctrl Pts',(-2.496344072,0.875180297,6.818148319));
#162374=CARTESIAN_POINT('Ctrl Pts',(-2.118148151,0.809946053,6.933682168));
#162375=CARTESIAN_POINT('Ctrl Pts',(-2.10506790742243,0.807689868430738,
6.93767800931519));
#162376=CARTESIAN_POINT('Ctrl Pts',(-2.09198766384487,0.805433683861471,
6.9416738506305));
#162377=CARTESIAN_POINT('Ctrl Pts',(-3.18344177797812,0.940837228,6.79143474773948));
#162378=CARTESIAN_POINT('Ctrl Pts',(-2.81300470636392,0.875180297,6.96507476535259));
#162379=CARTESIAN_POINT('Ctrl Pts',(-2.42587918037184,0.809946053,7.09739372559584));
#162380=CARTESIAN_POINT('Ctrl Pts',(-2.41249009843335,0.807689868430738,
7.10197009496898));
#162381=CARTESIAN_POINT('Ctrl Pts',(-2.39910101649486,0.805433683861474,
7.10654646434213));
#162382=CARTESIAN_POINT('',(-2.42524323109857,0.809946052265054,7.09705541884243));
#162383=CARTESIAN_POINT('Origin',(0.0821273247219212,0.946416076993006,
-0.172960606955359));
#162384=CARTESIAN_POINT('',(-2.2716956840529,0.809946053334091,7.0153687836305));
#162385=CARTESIAN_POINT('Origin',(2.4459601011273E-13,0.90157351800025,
-7.43762690325056E-13));
#162386=CARTESIAN_POINT('Origin',(0.0633873961025447,0.803569528795175,
-0.182327060850242));
#162387=CARTESIAN_POINT('Origin',(0.105428588023943,0.946349169809241,-0.155232932580697));
#162388=CARTESIAN_POINT('Ctrl Pts',(-2.118148151,0.809946053,6.933682168));
#162389=CARTESIAN_POINT('Ctrl Pts',(-1.739959553,0.875601501,7.04921378));
#162390=CARTESIAN_POINT('Ctrl Pts',(-1.351448856,0.940829639,7.122926785));
#162391=CARTESIAN_POINT('Ctrl Pts',(-1.954774922,0.809946053,7.24077723800001));
#162392=CARTESIAN_POINT('Ctrl Pts',(-1.559836226,0.875601501,7.347397871));
#162393=CARTESIAN_POINT('Ctrl Pts',(-1.155643991,0.940829639,7.410430957));
#162394=CARTESIAN_POINT('',(-1.95477490990743,0.80994605211794,7.24077723976916));
#162395=CARTESIAN_POINT('',(-1.40337282846125,0.900669500586772,7.36753314887519));
#162396=CARTESIAN_POINT('Origin',(0.0511926721787856,0.803573321280154,
-0.185665675624656));
#162397=CARTESIAN_POINT('Ctrl Pts',(-1.3560685684962,0.940053944109252,
7.12204873926195));
#162398=CARTESIAN_POINT('Ctrl Pts',(-1.36398279154419,0.933168237664389,
7.16289612185191));
#162399=CARTESIAN_POINT('Ctrl Pts',(-1.37188477495162,0.926448448773429,
7.20379909602903));
#162400=CARTESIAN_POINT('Ctrl Pts',(-1.38764900142186,0.913330774387375,
7.28561428017792));
#162401=CARTESIAN_POINT('Ctrl Pts',(-1.39552006200217,0.906925555236195,
7.32657226934425));
#162402=CARTESIAN_POINT('Ctrl Pts',(-1.4033728302277,0.900669500587413,
7.36753314853664));
#162403=CARTESIAN_POINT('',(-2.03646151908971,0.809946050061996,7.08722970800272));
#162404=CARTESIAN_POINT('Origin',(-1.49132008825381E-12,0.714028547998533,
8.0183255868338E-12));
#162405=CARTESIAN_POINT('',(-1.21292876289188,0.7499999994391,7.40127039826681));
#162406=CARTESIAN_POINT('',(-1.39282737462974,0.714243089195332,7.33314099135441));
#162407=CARTESIAN_POINT('Origin',(1.42856879364856,0.473617195858478,0.290378570482246));
#162408=CARTESIAN_POINT('',(-1.58832891769568,0.750000000357976,7.32988480500076));
#162409=CARTESIAN_POINT('Origin',(0.,0.750000000000029,0.));
#162410=CARTESIAN_POINT('Origin',(-1.36764246652044,0.692075156497888,-0.489307690687903));
#162411=CARTESIAN_POINT('Ctrl Pts',(-1.360702703,0.940837228,7.12116480300001));
#162412=CARTESIAN_POINT('Ctrl Pts',(-0.97228059,0.875180297,7.19538398400001));
#162413=CARTESIAN_POINT('Ctrl Pts',(-0.578090317,0.809946053,7.226915773));
#162414=CARTESIAN_POINT('Ctrl Pts',(-0.564456894327321,0.807689868405652,
7.22800632808598));
#162415=CARTESIAN_POINT('Ctrl Pts',(-0.550823471654651,0.8054336838113,
7.22909688317197));
#162416=CARTESIAN_POINT('Ctrl Pts',(-1.64905696119033,0.940837228,7.3170006579265));
#162417=CARTESIAN_POINT('Ctrl Pts',(-1.24995303106258,0.875180297,7.40694804796768));
#162418=CARTESIAN_POINT('Ctrl Pts',(-0.843433619567465,0.809946053,7.45295291915378));
#162419=CARTESIAN_POINT('Ctrl Pts',(-0.829373782627856,0.807689868405651,
7.45454403871418));
#162420=CARTESIAN_POINT('Ctrl Pts',(-0.815313945688232,0.805433683811302,
7.45613515827444));
#162421=CARTESIAN_POINT('',(-0.842885264404958,0.809946052265035,7.45248581153022));
#162422=CARTESIAN_POINT('Origin',(0.0430257963966185,0.946416066071054,
-0.186571768009569));
#162423=CARTESIAN_POINT('',(-0.710487785962877,0.809946053334091,7.3397007811972));
#162424=CARTESIAN_POINT('Origin',(2.90349341791618E-13,0.901573517999945,
-8.2572837456496E-13));
#162425=CARTESIAN_POINT('Origin',(0.0227102601950326,0.803569500238102,
-0.19168863190188));
#162426=CARTESIAN_POINT('Origin',(0.0695932217806294,0.946349460745737,
-0.174267442991308));
#162427=CARTESIAN_POINT('Origin',(6.5199683488542E-13,0.714028547998044,
9.41868111281607E-12));
#162428=CARTESIAN_POINT('',(0.406483194510219,0.749999999382397,7.48897663951845));
#162429=CARTESIAN_POINT('',(0.216144698514716,0.714243089127833,7.46111294407942));
#162430=CARTESIAN_POINT('Origin',(1.45759410732055,0.473613193749064,-0.0235166762380834));
#162431=CARTESIAN_POINT('',(0.0245138937354052,0.750000000265122,7.49995993809237));
#162432=CARTESIAN_POINT('Origin',(0.,0.750000000000029,0.));
#162433=CARTESIAN_POINT('Origin',(-1.4408544571891,0.692072055132696,-0.1838623608636));
#162434=CARTESIAN_POINT('Origin',(-1.29562159612018E-13,0.901573518000111,
-1.69222275081538E-12));
#162435=CARTESIAN_POINT('Origin',(-0.0190280583507755,0.803569332138143,
-0.192089151140023));
#162436=CARTESIAN_POINT('',(-0.352520287816385,0.809946052007895,7.49171071413411));
#162437=CARTESIAN_POINT('Origin',(0.0100831895880892,0.803573329523321,
-0.192329770834291));
#162438=CARTESIAN_POINT('Origin',(0.0305037823483433,0.946349178008734,
-0.185153758430255));
#162439=CARTESIAN_POINT('Ctrl Pts',(-0.578090316999999,0.809946053,7.226915773));
#162440=CARTESIAN_POINT('Ctrl Pts',(-0.183907677,0.875601501,7.258446951));
#162441=CARTESIAN_POINT('Ctrl Pts',(0.211365974,0.940829639,7.246918271));
#162442=CARTESIAN_POINT('Ctrl Pts',(-0.3525203,0.809946053,7.491710715));
#162443=CARTESIAN_POINT('Ctrl Pts',(0.056105233,0.875601501,7.510938472));
#162444=CARTESIAN_POINT('Ctrl Pts',(0.464397928,0.940829639,7.485608497));
#162445=CARTESIAN_POINT('',(-0.465305290421314,0.809946050061996,7.35931324514306));
#162446=CARTESIAN_POINT('Origin',(-6.831,5.5,-6.831));
#162447=CARTESIAN_POINT('Ctrl Pts',(-0.0319404048748598,0.679837254,7.50015957748802));
#162448=CARTESIAN_POINT('Ctrl Pts',(0.374474514429064,0.744719353,7.50189034821298));
#162449=CARTESIAN_POINT('Ctrl Pts',(0.778696744357235,0.809946053,7.4596947157045));
#162450=CARTESIAN_POINT('Ctrl Pts',(0.784807551964174,0.810932114094676,
7.45905682552177));
#162451=CARTESIAN_POINT('Ctrl Pts',(0.790918359571115,0.811918175189354,
7.45841893533904));
#162452=CARTESIAN_POINT('Ctrl Pts',(0.207112381,0.679837254,7.247041083));
#162453=CARTESIAN_POINT('Ctrl Pts',(0.599811441,0.744719353,7.23581818000001));
#162454=CARTESIAN_POINT('Ctrl Pts',(0.988998379,0.809946053,7.182226828));
#162455=CARTESIAN_POINT('Ctrl Pts',(0.994881891397807,0.810932114094676,
7.18141666364678));
#162456=CARTESIAN_POINT('Ctrl Pts',(1.00076540379561,0.811918175189354,
7.18060649929357));
#162457=CARTESIAN_POINT('',(0.211783654916351,0.680609079917163,7.24690609400179));
#162458=CARTESIAN_POINT('Origin',(0.680510006550487,-0.209901599065594,
14.713132500196));
#162459=CARTESIAN_POINT('Origin',(-0.0261189597533898,0.803568149720519,
-0.197293460469613));
#162460=CARTESIAN_POINT('Ctrl Pts',(1.266217779,0.809946053,7.392340126));
#162461=CARTESIAN_POINT('Ctrl Pts',(1.672049896,0.744288122,7.32282603));
#162462=CARTESIAN_POINT('Ctrl Pts',(2.067833513,0.679844992,7.209304028));
#162463=CARTESIAN_POINT('Ctrl Pts',(0.988998379000001,0.809946053,7.182226828));
#162464=CARTESIAN_POINT('Ctrl Pts',(1.383295485,0.744288122,7.127931801));
#162465=CARTESIAN_POINT('Ctrl Pts',(1.769279415,0.679844992,7.030800122));
#162466=CARTESIAN_POINT('',(1.76470286410966,0.680609079808175,7.03195023234919));
#162467=CARTESIAN_POINT('Origin',(-0.00355486455109438,0.946280588255798,
-0.191345552750808));
#162468=CARTESIAN_POINT('Origin',(5.41950269662529,-0.919059860839161,19.7580986531931));
#162469=CARTESIAN_POINT('Ctrl Pts',(1.5811189502161,0.679837254,7.33167625657691));
#162470=CARTESIAN_POINT('Ctrl Pts',(1.97840417914827,0.744719353,7.24599936953168));
#162471=CARTESIAN_POINT('Ctrl Pts',(2.36410510414471,0.809946053,7.11789441685984));
#162472=CARTESIAN_POINT('Ctrl Pts',(2.36993592080826,0.810932114750492,
7.1159577959074));
#162473=CARTESIAN_POINT('Ctrl Pts',(2.3757667374718,0.811918176500982,7.11402117495497));
#162474=CARTESIAN_POINT('Ctrl Pts',(1.76016982,0.679837254,7.03308625));
#162475=CARTESIAN_POINT('Ctrl Pts',(2.141275202,0.744719353,6.93770704300001));
#162476=CARTESIAN_POINT('Ctrl Pts',(2.509842609,0.809946053,6.801704939));
#162477=CARTESIAN_POINT('Ctrl Pts',(2.51541441046351,0.810932114750492,
6.79964893321188));
#162478=CARTESIAN_POINT('Ctrl Pts',(2.52098621192704,0.811918176500982,
6.79759292742373));
#162479=CARTESIAN_POINT('Origin',(-0.0679205186180731,0.803568141971726,
-0.187065872158867));
#162480=CARTESIAN_POINT('Ctrl Pts',(2.825748922,0.809946053,6.947311928));
#162481=CARTESIAN_POINT('Ctrl Pts',(3.207149434,0.744288122,6.792181124));
#162482=CARTESIAN_POINT('Ctrl Pts',(3.569275975,0.679844992,6.596231425));
#162483=CARTESIAN_POINT('Ctrl Pts',(2.509842609,0.809946053,6.801704939));
#162484=CARTESIAN_POINT('Ctrl Pts',(2.883249442,0.744288122,6.663917077));
#162485=CARTESIAN_POINT('Ctrl Pts',(3.239328843,0.679844992,6.486081147));
#162486=CARTESIAN_POINT('',(3.23510652851057,0.68060907995182,6.48818819109484));
#162487=CARTESIAN_POINT('Origin',(-0.0446053175177707,0.946280595435742,
-0.186107667924471));
#162488=CARTESIAN_POINT('Origin',(9.53942525657404,-0.918876384710192,18.1296796878941));
#162489=CARTESIAN_POINT('Ctrl Pts',(3.12024693994115,0.679837254,6.82037190337756));
#162490=CARTESIAN_POINT('Ctrl Pts',(3.4898258629797,0.744719353,6.65129351328347));
#162491=CARTESIAN_POINT('Ctrl Pts',(3.8389705365879,0.809946053,6.44326928575995));
#162492=CARTESIAN_POINT('Ctrl Pts',(3.84424871724141,0.810932115031176,
6.44012448781177));
#162493=CARTESIAN_POINT('Ctrl Pts',(3.84952689789492,0.811918177062351,
6.43697968986362));
#162494=CARTESIAN_POINT('Ctrl Pts',(3.230923675,0.679837254,6.490272121));
#162495=CARTESIAN_POINT('Ctrl Pts',(3.582615315,0.744719353,6.315196435));
#162496=CARTESIAN_POINT('Ctrl Pts',(3.913329389,0.809946053,6.10314288700001));
#162497=CARTESIAN_POINT('Ctrl Pts',(3.91832894580031,0.810932115031176,
6.09993717596052));
#162498=CARTESIAN_POINT('Ctrl Pts',(3.92332850260062,0.811918177062351,
6.09673146492104));
#162499=CARTESIAN_POINT('Origin',(-0.106546367331508,0.803568122919176,
-0.168091762861144));
#162500=CARTESIAN_POINT('Ctrl Pts',(4.253151186,0.809946053,6.177435146));
#162501=CARTESIAN_POINT('Ctrl Pts',(4.592286229,0.744288122,5.943941379));
#162502=CARTESIAN_POINT('Ctrl Pts',(4.903823059,0.679844992,5.674726372));
#162503=CARTESIAN_POINT('Ctrl Pts',(3.913329389,0.809946053,6.103142887));
#162504=CARTESIAN_POINT('Ctrl Pts',(4.24838586,0.744288122,5.888304997));
#162505=CARTESIAN_POINT('Ctrl Pts',(4.557910854,0.679844992,5.638080227));
#162506=CARTESIAN_POINT('',(4.55424020729894,0.680609079944476,5.64104568189662));
#162507=CARTESIAN_POINT('Origin',(-0.083570205332133,0.946280566572918,
-0.172167845103236));
#162508=CARTESIAN_POINT('Origin',(13.2145781900805,-0.919019804357942,15.6560946877858));
#162509=CARTESIAN_POINT('Ctrl Pts',(4.51347565132549,0.679837254,5.99015454003778));
#162510=CARTESIAN_POINT('Ctrl Pts',(4.83806716842846,0.744719353,5.74558056475493));
#162511=CARTESIAN_POINT('Ctrl Pts',(5.13432997385664,0.809946053,5.46736404465009));
#162512=CARTESIAN_POINT('Ctrl Pts',(5.13880871367383,0.810932114743429,
5.46315811875066));
#162513=CARTESIAN_POINT('Ctrl Pts',(5.14328745349099,0.811918176486856,
5.4589521928512));
#162514=CARTESIAN_POINT('Ctrl Pts',(4.55060313,0.679837254,5.643980081));
#162515=CARTESIAN_POINT('Ctrl Pts',(4.856436318,0.744719353,5.39739426));
#162516=CARTESIAN_POINT('Ctrl Pts',(5.133833235,0.809946053,5.119204656));
#162517=CARTESIAN_POINT('Ctrl Pts',(5.13802677058587,0.810932114743429,
5.11499913700358));
#162518=CARTESIAN_POINT('Ctrl Pts',(5.14222030617174,0.811918176486856,
5.11079361800716));
#162519=CARTESIAN_POINT('Origin',(-0.140189871307624,0.803568097858735,
-0.141257253492768));
#162520=CARTESIAN_POINT('Ctrl Pts',(5.481680828,0.809946053,5.11870836300001));
#162521=CARTESIAN_POINT('Ctrl Pts',(5.762692823,0.744288122,4.81776954));
#162522=CARTESIAN_POINT('Ctrl Pts',(6.00907282800001,0.679844992,4.487877421));
#162523=CARTESIAN_POINT('Ctrl Pts',(5.133833235,0.809946053,5.119204656));
#162524=CARTESIAN_POINT('Ctrl Pts',(5.414872477,0.744288122,4.83736232));
#162525=CARTESIAN_POINT('Ctrl Pts',(5.663370019,0.679844992,4.526448942));
#162526=CARTESIAN_POINT('',(5.66042267655931,0.680609079843256,4.53013414747271));
#162527=CARTESIAN_POINT('Origin',(-0.118627125200667,0.946280598598074,
-0.150177324068743));
#162528=CARTESIAN_POINT('Origin',(16.2709444742823,-0.918980550492197,12.4491087468896));
#162529=CARTESIAN_POINT('Ctrl Pts',(5.69565925739822,0.679837254,4.87984420868066));
#162530=CARTESIAN_POINT('Ctrl Pts',(5.96008583006358,0.744719353,4.57121065596384));
#162531=CARTESIAN_POINT('Ctrl Pts',(6.1896138473021,0.809946053,4.23581093640374));
#162532=CARTESIAN_POINT('Ctrl Pts',(6.19308372685913,0.810932114726258,
4.2307405461118));
#162533=CARTESIAN_POINT('Ctrl Pts',(6.19655360641617,0.811918176452514,
4.22567015581985));
#162534=CARTESIAN_POINT('Ctrl Pts',(5.65750144,0.679837254,4.533781805));
#162535=CARTESIAN_POINT('Ctrl Pts',(5.903175755,0.744719353,4.227215929));
#162536=CARTESIAN_POINT('Ctrl Pts',(6.114284746,0.809946053,3.895898106));
#162537=CARTESIAN_POINT('Ctrl Pts',(6.11747617674989,0.810932114726258,
3.89088942359714));
#162538=CARTESIAN_POINT('Ctrl Pts',(6.12066760749978,0.811918176452514,
3.88588074119426));
#162539=CARTESIAN_POINT('Origin',(-0.167278719693816,0.803568145827063,
-0.107818265580796));
#162540=CARTESIAN_POINT('Ctrl Pts',(6.453893166,0.809946053,3.820636465));
#162541=CARTESIAN_POINT('Ctrl Pts',(6.663642306,0.744288122,3.466324153));
#162542=CARTESIAN_POINT('Ctrl Pts',(6.833345029,0.679844992,3.09118031));
#162543=CARTESIAN_POINT('Ctrl Pts',(6.114284746,0.809946053,3.895898106));
#162544=CARTESIAN_POINT('Ctrl Pts',(6.328165675,0.744288122,3.560229957));
#162545=CARTESIAN_POINT('Ctrl Pts',(6.504016297,0.679844992,3.203165935));
#162546=CARTESIAN_POINT('',(6.50193007002564,0.680609079906773,3.20739857317831));
#162547=CARTESIAN_POINT('Origin',(-0.148137647194987,0.946280588273123,
-0.121165073592281));
#162548=CARTESIAN_POINT('Origin',(18.5668200740015,-0.919005909663884,8.6603200934186));
#162549=CARTESIAN_POINT('Ctrl Pts',(6.61152016658401,0.679837254,3.54135778485581));
#162550=CARTESIAN_POINT('Ctrl Pts',(6.803417501554,0.744719353,3.18309601629077));
#162551=CARTESIAN_POINT('Ctrl Pts',(6.9554782573042,0.809946053,2.8061960172087));
#162552=CARTESIAN_POINT('Ctrl Pts',(6.9577770284796,0.810932114506048,2.80049824956562));
#162553=CARTESIAN_POINT('Ctrl Pts',(6.96007579965497,0.811918176012098,
2.79480048192255));
#162554=CARTESIAN_POINT('Ctrl Pts',(6.499861271,0.679837254,3.211588931));
#162555=CARTESIAN_POINT('Ctrl Pts',(6.673889256,0.744719353,2.859377679));
#162556=CARTESIAN_POINT('Ctrl Pts',(6.808839097,0.809946053,2.49042369));
#162557=CARTESIAN_POINT('Ctrl Pts',(6.81087919474306,0.810932114506048,
2.48484604578289));
#162558=CARTESIAN_POINT('Ctrl Pts',(6.81291929248613,0.811918176012098,
2.47926840156579));
#162559=CARTESIAN_POINT('Origin',(-0.18654538333014,0.803568163185117,-0.0693374685299075));
#162560=CARTESIAN_POINT('Ctrl Pts',(7.124328633,0.809946053,2.343915853));
#162561=CARTESIAN_POINT('Ctrl Pts',(7.253007281,0.744288122,1.9527973));
#162562=CARTESIAN_POINT('Ctrl Pts',(7.33809761200001,0.679844992,1.549943043));
#162563=CARTESIAN_POINT('Ctrl Pts',(6.808839097,0.809946053,2.49042369));
#162564=CARTESIAN_POINT('Ctrl Pts',(6.945560879,0.744288122,2.116625199));
#162565=CARTESIAN_POINT('Ctrl Pts',(7.040542002,0.679844992,1.730106449));
#162566=CARTESIAN_POINT('',(7.03941444172257,0.680609079894364,1.73468860760923));
#162567=CARTESIAN_POINT('Origin',(-0.170721307163793,0.946280565852508,
-0.0864871263428832));
#162568=CARTESIAN_POINT('Origin',(19.9937280304115,-0.918922005754596,4.46638008064186));
#162569=CARTESIAN_POINT('Ctrl Pts',(7.21823374108708,0.679837254,2.03728140705634));
#162570=CARTESIAN_POINT('Ctrl Pts',(7.32862893308932,0.744719353,1.64614334500659));
#162571=CARTESIAN_POINT('Ctrl Pts',(7.39611223383465,0.809946053,1.2453664911386));
#162572=CARTESIAN_POINT('Ctrl Pts',(7.39713240963888,0.810932114742612,
1.23930776483597));
#162573=CARTESIAN_POINT('Ctrl Pts',(7.39815258544312,0.811918176485222,
1.23324903853334));
#162574=CARTESIAN_POINT('Ctrl Pts',(7.038294813,0.679837254,1.739225727));
#162575=CARTESIAN_POINT('Ctrl Pts',(7.13253911200001,0.744719353,1.357838106));
#162576=CARTESIAN_POINT('Ctrl Pts',(7.18501969900001,0.809946053,0.96849983));
#162577=CARTESIAN_POINT('Ctrl Pts',(7.18581307194498,0.810932114742612,
0.962614025890673));
#162578=CARTESIAN_POINT('Ctrl Pts',(7.18660644488997,0.811918176485222,
0.956728221781344));
#162579=CARTESIAN_POINT('Origin',(-0.197089526502294,0.803568141080806,
-0.0276146383221554));
#162580=CARTESIAN_POINT('Ctrl Pts',(7.461638412,0.809946053,0.75759634));
#162581=CARTESIAN_POINT('Ctrl Pts',(7.503229697,0.744288122,0.347959816));
#162582=CARTESIAN_POINT('Ctrl Pts',(7.499728906,0.679844992,-0.063767838));
#162583=CARTESIAN_POINT('Ctrl Pts',(7.185019699,0.809946053,0.96849983));
#162584=CARTESIAN_POINT('Ctrl Pts',(7.238189376,0.744288122,0.574049398));
#162585=CARTESIAN_POINT('Ctrl Pts',(7.247859787,0.679844992,0.176149108));
#162586=CARTESIAN_POINT('',(7.24774361921728,0.680609079812669,0.180866530829771));
#162587=CARTESIAN_POINT('Origin',(-0.185321732206588,0.946280559786437,
-0.0477650476507504));
#162588=CARTESIAN_POINT('Origin',(20.4864779452742,-0.918914818035844,0.063898929278453));
#162589=CARTESIAN_POINT('Ctrl Pts',(7.48743072874736,0.679837254,0.437944015219146));
#162590=CARTESIAN_POINT('Ctrl Pts',(7.51116182146427,0.744719353,0.0322188409795213));
#162591=CARTESIAN_POINT('Ctrl Pts',(7.49091222296789,0.809946053,-0.373694987688807));
#162592=CARTESIAN_POINT('Ctrl Pts',(7.49060610072142,0.810932114226693,
-0.37983136876938));
#162593=CARTESIAN_POINT('Ctrl Pts',(7.49029997847496,0.811918175453385,
-0.385967749849952));
#162594=CARTESIAN_POINT('Ctrl Pts',(7.24762551100001,0.679837254,0.185538262));
#162595=CARTESIAN_POINT('Ctrl Pts',(7.257679367,0.744719353,-0.207192467));
#162596=CARTESIAN_POINT('Ctrl Pts',(7.225236766,0.809946053,-0.598710006));
#162597=CARTESIAN_POINT('Ctrl Pts',(7.22474631667573,0.810932114226693,
-0.604628751924261));
#162598=CARTESIAN_POINT('Ctrl Pts',(7.22425586735147,0.811918175453385,
-0.610547497848522));
#162599=CARTESIAN_POINT('Origin',(-0.198417951097591,0.803568118635443,
0.0153993916838719));
#162600=CARTESIAN_POINT('Ctrl Pts',(7.450050271,0.809946053,-0.864147535));
#162601=CARTESIAN_POINT('Ctrl Pts',(7.402609431,0.744288122,-1.273147882));
#162602=CARTESIAN_POINT('Ctrl Pts',(7.310681212,0.679844992,-1.674497005));
#162603=CARTESIAN_POINT('Ctrl Pts',(7.225236766,0.809946053,-0.598710006));
#162604=CARTESIAN_POINT('Ctrl Pts',(7.192368183,0.744288122,-0.995368314));
#162605=CARTESIAN_POINT('Ctrl Pts',(7.116275704,0.679844992,-1.386044769));
#162606=CARTESIAN_POINT('',(7.11717635838003,0.680609079831188,-1.38141266477938));
#162607=CARTESIAN_POINT('Origin',(-0.191257343635393,0.946280592086966,
-0.00680959738268955));
#162608=CARTESIAN_POINT('Origin',(20.0210910547472,-0.918903429656103,-4.34154776765039));
#162609=CARTESIAN_POINT('Ctrl Pts',(7.40652377624533,0.679837254,-1.18187115244431));
#162610=CARTESIAN_POINT('Ctrl Pts',(7.34248112992593,0.744719353,-1.58321218171481));
#162611=CARTESIAN_POINT('Ctrl Pts',(7.23544548158936,0.809946053,-1.97528290532036));
#162612=CARTESIAN_POINT('Ctrl Pts',(7.23382737490774,0.810932114753538,
-1.98121001715079));
#162613=CARTESIAN_POINT('Ctrl Pts',(7.23220926822613,0.811918176507078,
-1.98713712898122));
#162614=CARTESIAN_POINT('Ctrl Pts',(7.118065296,0.679837254,-1.376824766));
#162615=CARTESIAN_POINT('Ctrl Pts',(7.0434586,0.744719353,-1.762534951));
#162616=CARTESIAN_POINT('Ctrl Pts',(6.927609792,0.809946053,-2.137924827));
#162617=CARTESIAN_POINT('Ctrl Pts',(6.9258584527668,0.810932114753538,-2.14359976685422));
#162618=CARTESIAN_POINT('Ctrl Pts',(6.92410711353362,0.811918176507078,
-2.14927470670844));
#162619=CARTESIAN_POINT('Origin',(-0.190468597948358,0.803568146623334,
0.0576933426523757));
#162620=CARTESIAN_POINT('Ctrl Pts',(7.090106059,0.809946053,-2.445484832));
#162621=CARTESIAN_POINT('Ctrl Pts',(6.955851376,0.744288122,-2.8347246));
#162622=CARTESIAN_POINT('Ctrl Pts',(6.779794189,0.679844992,-3.206928554));
#162623=CARTESIAN_POINT('Ctrl Pts',(6.927609792,0.809946053,-2.137924827));
#162624=CARTESIAN_POINT('Ctrl Pts',(6.81023984700001,0.744288122,-2.518243711));
#162625=CARTESIAN_POINT('Ctrl Pts',(6.65194247900001,0.679844992,-2.883428734));
#162626=CARTESIAN_POINT('',(6.6538178404657,0.680609079934148,-2.8790985384958));
#162627=CARTESIAN_POINT('Origin',(-0.188249734722257,0.946280573583837,
0.0344642921835409));
#162628=CARTESIAN_POINT('Origin',(18.6195617475465,-0.918877917958552,-8.54391955967953));
#162629=CARTESIAN_POINT('Ctrl Pts',(6.97929600465152,0.679837254,-2.74642333766407));
#162630=CARTESIAN_POINT('Ctrl Pts',(6.83047418193199,0.744719353,-3.12461396142994));
#162631=CARTESIAN_POINT('Ctrl Pts',(6.64165735171076,0.809946053,-3.48450878846813));
#162632=CARTESIAN_POINT('Ctrl Pts',(6.63880292162864,0.810932114753182,
-3.48994948260275));
#162633=CARTESIAN_POINT('Ctrl Pts',(6.63594849154651,0.811918176506363,
-3.49539017673736));
#162634=CARTESIAN_POINT('Ctrl Pts',(6.655672259,0.679837254,-2.874808998));
#162635=CARTESIAN_POINT('Ctrl Pts',(6.49989353800001,0.744719353,-3.235463259));
#162636=CARTESIAN_POINT('Ctrl Pts',(6.306055484,0.809946053,-3.577172659));
#162637=CARTESIAN_POINT('Ctrl Pts',(6.30312514578941,0.810932114753182,
-3.58233843574545));
#162638=CARTESIAN_POINT('Ctrl Pts',(6.30019480757882,0.811918176506363,
-3.58750421249091));
#162639=CARTESIAN_POINT('Origin',(-0.173613336813595,0.803568116995496,
0.0972897037180659));
#162640=CARTESIAN_POINT('Ctrl Pts',(6.398636369,0.809946053,-3.912473977));
#162641=CARTESIAN_POINT('Ctrl Pts',(6.183845441,0.744288122,-4.263752746));
#162642=CARTESIAN_POINT('Ctrl Pts',(5.93189152599999,0.679844992,-4.589407688));
#162643=CARTESIAN_POINT('Ctrl Pts',(6.306055484,0.809946053,-3.577172659));
#162644=CARTESIAN_POINT('Ctrl Pts',(6.109672265,0.744288122,-3.92336883));
#162645=CARTESIAN_POINT('Ctrl Pts',(5.876571816,0.679844992,-4.245986775));
#162646=CARTESIAN_POINT('',(5.87933419646206,0.680609079917205,-4.24216096441692));
#162647=CARTESIAN_POINT('Origin',(-0.176439515626958,0.946280541725487,
0.0741265169878685));
#162648=CARTESIAN_POINT('Origin',(16.348679514349,-0.919047985408652,-12.3476875756904));
#162649=CARTESIAN_POINT('Ctrl Pts',(6.22572410826749,0.679837254,-4.1825558210505));
#162650=CARTESIAN_POINT('Ctrl Pts',(5.9990818528282,0.744719353,-4.51991226497366));
#162651=CARTESIAN_POINT('Ctrl Pts',(5.73731270545755,0.809946053,-4.83080291392708));
#162652=CARTESIAN_POINT('Ctrl Pts',(5.73335542199936,0.810932114740028,
-4.83550278950358));
#162653=CARTESIAN_POINT('Ctrl Pts',(5.72939813854119,0.811918176480054,
-4.84020266508007));
#162654=CARTESIAN_POINT('Ctrl Pts',(5.88206738500001,0.679837254,-4.238370357));
#162655=CARTESIAN_POINT('Ctrl Pts',(5.65240067800001,0.744719353,-4.557104901));
#162656=CARTESIAN_POINT('Ctrl Pts',(5.38963703,0.809946053,-4.849155874));
#162657=CARTESIAN_POINT('Ctrl Pts',(5.38566471222273,0.810932114740028,
-4.85357094161209));
#162658=CARTESIAN_POINT('Ctrl Pts',(5.38169239444545,0.811918176480054,
-4.85798600922415));
#162659=CARTESIAN_POINT('Origin',(-0.148639930843035,0.803568108054348,
0.13233683330104));
#162660=CARTESIAN_POINT('Ctrl Pts',(5.407973553,0.809946053,-5.196520186));
#162661=CARTESIAN_POINT('Ctrl Pts',(5.122689766,0.744288122,-5.493412553));
#162662=CARTESIAN_POINT('Ctrl Pts',(4.806620207,0.679844992,-5.75729121900001));
#162663=CARTESIAN_POINT('Ctrl Pts',(5.38963702999999,0.809946053,-4.849155874));
#162664=CARTESIAN_POINT('Ctrl Pts',(5.123423198,0.744288122,-5.145041583));
#162665=CARTESIAN_POINT('Ctrl Pts',(4.826419186,0.679844992,-5.410007194));
#162666=CARTESIAN_POINT('',(4.8299394211557,0.680609079820267,-5.4068646602954));
#162667=CARTESIAN_POINT('Origin',(-0.156379663221219,0.946280575238907,
0.110322979496779));
#162668=CARTESIAN_POINT('Origin',(13.3109697368389,-0.918851572015798,-15.5721798564474));
#162669=CARTESIAN_POINT('Ctrl Pts',(5.18104427232235,0.679837254,-5.42311664268225));
#162670=CARTESIAN_POINT('Ctrl Pts',(4.88717912351137,0.744719353,-5.70386449497362));
#162671=CARTESIAN_POINT('Ctrl Pts',(4.56469769334661,0.809946053,-5.95121406393451));
#162672=CARTESIAN_POINT('Ctrl Pts',(4.55982259305757,0.810932115062118,
-5.95495336127798));
#162673=CARTESIAN_POINT('Ctrl Pts',(4.55494749276852,0.811918177124235,
-5.95869265862146));
#162674=CARTESIAN_POINT('Ctrl Pts',(4.833423576,0.679837254,-5.403750228));
#162675=CARTESIAN_POINT('Ctrl Pts',(4.540607845,0.744719353,-5.665661383));
#162676=CARTESIAN_POINT('Ctrl Pts',(4.221205138,0.809946053,-5.894397949));
#162677=CARTESIAN_POINT('Ctrl Pts',(4.21637658018686,0.810932115062118,
-5.89785586500604));
#162678=CARTESIAN_POINT('Ctrl Pts',(4.21154802237372,0.811918177124235,
-5.9013137810121));
#162679=CARTESIAN_POINT('Origin',(-0.116716233245275,0.803568103427335,
0.161195976465628));
#162680=CARTESIAN_POINT('Ctrl Pts',(4.164439905,0.809946053,-6.237582888));
#162681=CARTESIAN_POINT('Ctrl Pts',(3.822002811,0.744288122,-6.46620649400001));
#162682=CARTESIAN_POINT('Ctrl Pts',(3.45659667,0.679844992,-6.655970212));
#162683=CARTESIAN_POINT('Ctrl Pts',(4.221205138,0.809946053,-5.894397949));
#162684=CARTESIAN_POINT('Ctrl Pts',(3.897608556,0.744288122,-6.12613791));
#162685=CARTESIAN_POINT('Ctrl Pts',(3.55058856,0.679844992,-6.321061689));
#162686=CARTESIAN_POINT('',(3.55470204592073,0.680609079806426,-6.31874937276602));
#162687=CARTESIAN_POINT('Origin',(-0.129007325136785,0.946280573576781,
0.141360544234609));
#162688=CARTESIAN_POINT('Origin',(9.65240306669682,-0.91890051911108,-18.0699482044124));
#162689=CARTESIAN_POINT('Ctrl Pts',(3.89410456449864,0.679837254,-6.4100985573269));
#162690=CARTESIAN_POINT('Ctrl Pts',(3.54675733026341,0.744719353,-6.62111036018678));
#162691=CARTESIAN_POINT('Ctrl Pts',(3.17864249022696,0.809946053,-6.79335305972249));
#162692=CARTESIAN_POINT('Ctrl Pts',(3.17307753073869,0.810932114694818,
-6.79595693096271));
#162693=CARTESIAN_POINT('Ctrl Pts',(3.16751257125042,0.811918176389634,
-6.79856080220291));
#162694=CARTESIAN_POINT('Ctrl Pts',(3.558774254,0.679837254,-6.316456745));
#162695=CARTESIAN_POINT('Ctrl Pts',(3.216501235,0.744719353,-6.509297835));
#162696=CARTESIAN_POINT('Ctrl Pts',(2.855394386,0.809946053,-6.664024527));
#162697=CARTESIAN_POINT('Ctrl Pts',(2.84993536950008,0.810932114694818,
-6.66636360078645));
#162698=CARTESIAN_POINT('Ctrl Pts',(2.84447635300018,0.811918176389633,
-6.66870267457291));
#162699=CARTESIAN_POINT('Origin',(-0.0793350860434211,0.803568151356397,
0.18251784667311));
#162700=CARTESIAN_POINT('Ctrl Pts',(2.726181675,0.809946053,-6.986983146));
#162701=CARTESIAN_POINT('Ctrl Pts',(2.342603253,0.744288122,-7.136647807));
#162702=CARTESIAN_POINT('Ctrl Pts',(1.944946514,0.679844992,-7.243423435));
#162703=CARTESIAN_POINT('Ctrl Pts',(2.855394386,0.809946053,-6.664024527));
#162704=CARTESIAN_POINT('Ctrl Pts',(2.489546071,0.744288122,-6.82078283800001));
#162705=CARTESIAN_POINT('Ctrl Pts',(2.108736358,0.679844992,-6.936550365));
#162706=CARTESIAN_POINT('',(2.11325075223419,0.680609079948131,-6.9351763867474));
#162707=CARTESIAN_POINT('Origin',(-0.0956029385533522,0.946280548888431,
0.165788545440595));
#162708=CARTESIAN_POINT('Origin',(5.54219511633975,-0.918869543282762,-19.7223186336196));
#162709=CARTESIAN_POINT('Ctrl Pts',(2.42508085481774,0.679837254,-7.09735138772923));
#162710=CARTESIAN_POINT('Ctrl Pts',(2.04049310563864,0.744719353,-7.22876046326209));
#162711=CARTESIAN_POINT('Ctrl Pts',(1.64395749819145,0.809946053,-7.31784241489472));
#162712=CARTESIAN_POINT('Ctrl Pts',(1.6379628885056,0.810932114781724,-7.31918910739864));
#162713=CARTESIAN_POINT('Ctrl Pts',(1.63196827881974,0.811918176563451,
-7.32053579990259));
#162714=CARTESIAN_POINT('Ctrl Pts',(2.117720602,0.679837254,-6.933812764));
#162715=CARTESIAN_POINT('Ctrl Pts',(1.741994603,0.744719353,-7.048566756));
#162716=CARTESIAN_POINT('Ctrl Pts',(1.356068566,0.809946053,-7.122048725));
#162717=CARTESIAN_POINT('Ctrl Pts',(1.35023434603091,0.810932114781724,
-7.12315958544943));
#162718=CARTESIAN_POINT('Ctrl Pts',(1.34440012606181,0.811918176563451,
-7.12427044589887));
#162719=CARTESIAN_POINT('Origin',(-0.0382443479738842,0.803568118805305,
0.195305453929068));
#162720=CARTESIAN_POINT('Ctrl Pts',(1.16045022,0.809946053,-7.409679837));
#162721=CARTESIAN_POINT('Ctrl Pts',(0.75366617,0.744288122,-7.473387399));
#162722=CARTESIAN_POINT('Ctrl Pts',(0.342352821,0.679844992,-7.49218222900001));
#162723=CARTESIAN_POINT('Ctrl Pts',(1.356068566,0.809946053,-7.122048725));
#162724=CARTESIAN_POINT('Ctrl Pts',(0.965075178000001,0.744288122,-7.19649554));
#162725=CARTESIAN_POINT('Ctrl Pts',(0.568281989,0.679844992,-7.227693656));
#162726=CARTESIAN_POINT('',(0.572986203812444,0.680609079901549,-7.22732226094589));
#162727=CARTESIAN_POINT('Origin',(-0.0577281455887602,0.946280608526164,
0.182464146390054));
#162728=CARTESIAN_POINT('Origin',(1.17292302164358,-0.918918442993689,-20.4529436923275));
#162729=CARTESIAN_POINT('Ctrl Pts',(0.842663060359861,0.679837254,-7.45273995492195));
#162730=CARTESIAN_POINT('Ctrl Pts',(0.43881769232648,0.744719353,-7.49840176169412));
#162731=CARTESIAN_POINT('Ctrl Pts',(0.0324028797431824,0.809946053,-7.50015759317151));
#162732=CARTESIAN_POINT('Ctrl Pts',(0.0262589216279636,0.810932114778227,
-7.50018413687691));
#162733=CARTESIAN_POINT('Ctrl Pts',(0.020114963512745,0.811918176556457,
-7.50021068058231));
#162734=CARTESIAN_POINT('Ctrl Pts',(0.577644689,0.679837254,-7.226951405));
#162735=CARTESIAN_POINT('Ctrl Pts',(0.186034238,0.744719353,-7.25825252900001));
#162736=CARTESIAN_POINT('Ctrl Pts',(-0.206665513,0.809946053,-7.24705384));
#162737=CARTESIAN_POINT('Ctrl Pts',(-0.212602134272893,0.810932114778227,
-7.2468845443099));
#162738=CARTESIAN_POINT('Ctrl Pts',(-0.218538755545785,0.811918176556456,
-7.24671524861982));
#162739=CARTESIAN_POINT('Origin',(0.00463467896617421,0.803568114703985,
0.198960813235042));
#162740=CARTESIAN_POINT('Ctrl Pts',(-0.459542598,0.809946053,-7.485908135));
#162741=CARTESIAN_POINT('Ctrl Pts',(-0.870511505,0.744288122,-7.460679703));
#162742=CARTESIAN_POINT('Ctrl Pts',(-1.276248909,0.679844992,-7.390614908));
#162743=CARTESIAN_POINT('Ctrl Pts',(-0.206665513,0.809946053,-7.24705384000001));
#162744=CARTESIAN_POINT('Ctrl Pts',(-0.604521557,0.744288122,-7.235708109));
#162745=CARTESIAN_POINT('Ctrl Pts',(-0.998744615,0.679844992,-7.180878024));
#162746=CARTESIAN_POINT('',(-0.994070543634724,0.680609079119151,-7.18152658032342));
#162747=CARTESIAN_POINT('Origin',(-0.0171541070111382,0.946280593383585,
0.190607868645933));
#162748=CARTESIAN_POINT('Origin',(-3.25137816860814,-0.918993617172282,
-20.2274616516324));
#162749=CARTESIAN_POINT('Ctrl Pts',(-0.779156723184081,0.679837254,-7.45964668465108));
#162750=CARTESIAN_POINT('Ctrl Pts',(-1.18337634970542,0.744719353,-7.41742612728615));
#162751=CARTESIAN_POINT('Ctrl Pts',(-1.58066686107051,0.809946053,-7.33177373711505));
#162752=CARTESIAN_POINT('Ctrl Pts',(-1.58667286991739,0.810932112636579,
-7.33047889367327));
#162753=CARTESIAN_POINT('Ctrl Pts',(-1.59267887876426,0.811918172273156,
-7.32918405023149));
#162754=CARTESIAN_POINT('Ctrl Pts',(-0.989441248,0.679837254,-7.182165831));
#162755=CARTESIAN_POINT('Ctrl Pts',(-1.37862488,0.744719353,-7.12855048));
#162756=CARTESIAN_POINT('Ctrl Pts',(-1.759736143,0.809946053,-7.033194773));
#162757=CARTESIAN_POINT('Ctrl Pts',(-1.76549756330012,0.810932112636579,
-7.03175324040997));
#162758=CARTESIAN_POINT('Ctrl Pts',(-1.77125898360023,0.811918172273156,
-7.03031170781994));
#162759=CARTESIAN_POINT('Origin',(0.0472970133577211,0.803568096753134,
0.193313010487212));
#162760=CARTESIAN_POINT('Ctrl Pts',(-2.058047714,0.809946053,-7.212103688));
#162761=CARTESIAN_POINT('Ctrl Pts',(-2.45398503,0.744288122,-7.099118916));
#162762=CARTESIAN_POINT('Ctrl Pts',(-2.835174659,0.679844992,-6.943470649));
#162763=CARTESIAN_POINT('Ctrl Pts',(-1.759736143,0.809946053,-7.03319477300001));
#162764=CARTESIAN_POINT('Ctrl Pts',(-2.145851537,0.744288122,-6.936587009));
#162765=CARTESIAN_POINT('Ctrl Pts',(-2.519071031,0.679844992,-6.798292516));
#162766=CARTESIAN_POINT('',(-2.51464565671269,0.680609079944213,-6.799930695879));
#162767=CARTESIAN_POINT('Origin',(0.0242221099862061,0.94628052984048,0.189839453464968));
#162768=CARTESIAN_POINT('Origin',(-7.52367615252197,-0.918977858636926,
-19.0556263464347));
#162769=CARTESIAN_POINT('Ctrl Pts',(-2.3645440035047,0.679837254,-7.1177486281266));
#162770=CARTESIAN_POINT('Ctrl Pts',(-2.75023702794865,0.744719353,-6.9896198925137));
#162771=CARTESIAN_POINT('Ctrl Pts',(-3.11982637566339,0.809946053,-6.82056429141002));
#162772=CARTESIAN_POINT('Ctrl Pts',(-3.12541363059661,0.810932115513994,
-6.81800859886343));
#162773=CARTESIAN_POINT('Ctrl Pts',(-3.13100088552983,0.811918178027987,
-6.81545290631684));
#162774=CARTESIAN_POINT('Ctrl Pts',(-2.510262011,0.679837254,-6.801550164));
#162775=CARTESIAN_POINT('Ctrl Pts',(-2.878821031,0.744719353,-6.665525334));
#162776=CARTESIAN_POINT('Ctrl Pts',(-3.230523466,0.809946053,-6.490471334));
#162777=CARTESIAN_POINT('Ctrl Pts',(-3.23584031611251,0.810932115513994,
-6.48782496085335));
#162778=CARTESIAN_POINT('Ctrl Pts',(-3.24115716622503,0.811918178027986,
-6.48517858770671));
#162779=CARTESIAN_POINT('Origin',(0.0877477662178078,0.803568115035289,
0.178625850947978));
#162780=CARTESIAN_POINT('Ctrl Pts',(-3.560320807,0.809946053,-6.601069288));
#162781=CARTESIAN_POINT('Ctrl Pts',(-3.922712942,0.744288122,-6.405611219));
#162782=CARTESIAN_POINT('Ctrl Pts',(-4.261530793,0.679844992,-6.171657419));
#162783=CARTESIAN_POINT('Ctrl Pts',(-3.230523466,0.809946053,-6.49047133400001));
#162784=CARTESIAN_POINT('Ctrl Pts',(-3.586843883,0.744288122,-6.31311881));
#162785=CARTESIAN_POINT('Ctrl Pts',(-3.921608485,0.679844992,-6.09782640700001));
#162786=CARTESIAN_POINT('',(-3.91763873447842,0.680609079056139,-6.10037761276869));
#162787=CARTESIAN_POINT('Origin',(0.0644657035781965,0.94628054675428,0.180194127610646));
#162788=CARTESIAN_POINT('Origin',(-11.444372356347,-0.919014173525902,-16.9930411751167));
#162789=CARTESIAN_POINT('Ctrl Pts',(-3.83936783438881,0.679837254,-6.44303255478497));
#162790=CARTESIAN_POINT('Ctrl Pts',(-4.18849968021581,0.744719353,-6.23498679924312));
#162791=CARTESIAN_POINT('Ctrl Pts',(-4.51310627720805,0.809946053,-5.99043283899561));
#162792=CARTESIAN_POINT('Ctrl Pts',(-4.51801350316094,0.810932114768393,
-5.98673580525775));
#162793=CARTESIAN_POINT('Ctrl Pts',(-4.52292072911385,0.811918176536784,
-5.9830387715199));
#162794=CARTESIAN_POINT('Ctrl Pts',(-3.913705713,0.679837254,-6.10290157100001));
#162795=CARTESIAN_POINT('Ctrl Pts',(-4.24440671,0.744719353,-5.890827631));
#162796=CARTESIAN_POINT('Ctrl Pts',(-4.550255102,0.809946053,-5.644260669));
#162797=CARTESIAN_POINT('Ctrl Pts',(-4.55487875161397,0.810932114768393,
-5.64053320379669));
#162798=CARTESIAN_POINT('Ctrl Pts',(-4.55950240122794,0.811918176536784,
-5.63680573859337));
#162799=CARTESIAN_POINT('Origin',(0.124095595416366,0.80356814062132,0.155586552527208));
#162800=CARTESIAN_POINT('Ctrl Pts',(-4.896117256,0.809946053,-5.681376225));
#162801=CARTESIAN_POINT('Ctrl Pts',(-5.208019157,0.744288122,-5.41258426));
#162802=CARTESIAN_POINT('Ctrl Pts',(-5.488622484,0.679844992,-5.11126434800001));
#162803=CARTESIAN_POINT('Ctrl Pts',(-4.550255102,0.809946053,-5.644260669));
#162804=CARTESIAN_POINT('Ctrl Pts',(-4.86011939600001,0.744288122,-5.394456192));
#162805=CARTESIAN_POINT('Ctrl Pts',(-5.14077588500001,0.679844992,-5.112232712));
#162806=CARTESIAN_POINT('',(-5.13744737780991,0.68060907991806,-5.1155776495944));
#162807=CARTESIAN_POINT('Origin',(0.101694863213478,0.946280537045227,0.162122989659684));
#162808=CARTESIAN_POINT('Origin',(-14.8290719530443,-0.918907507355324,
-14.1348558842815));
#162809=CARTESIAN_POINT('Ctrl Pts',(-5.13466709208186,0.679837254,-5.46704744072571));
#162810=CARTESIAN_POINT('Ctrl Pts',(-5.4309127425148,0.744719353,-5.1888126525784));
#162811=CARTESIAN_POINT('Ctrl Pts',(-5.69535834529991,0.809946053,-4.88019540489622));
#162812=CARTESIAN_POINT('Ctrl Pts',(-5.69935609130509,0.810932115073296,
-4.87552989578561));
#162813=CARTESIAN_POINT('Ctrl Pts',(-5.7033538373103,0.811918177146594,
-4.87086438667502));
#162814=CARTESIAN_POINT('Ctrl Pts',(-5.134148886,0.679837254,-5.118888084));
#162815=CARTESIAN_POINT('Ctrl Pts',(-5.411528649,0.744719353,-4.840681376));
#162816=CARTESIAN_POINT('Ctrl Pts',(-5.657221867,0.809946053,-4.534130649));
#162817=CARTESIAN_POINT('Ctrl Pts',(-5.66093612456532,0.810932115073296,
-4.52949638043458));
#162818=CARTESIAN_POINT('Ctrl Pts',(-5.66465038213065,0.811918177146594,
-4.52486211186916));
#162819=CARTESIAN_POINT('Origin',(0.154640799378106,0.803568169766499,0.125272107590645));
#162820=CARTESIAN_POINT('Ctrl Pts',(-6.002976704,0.809946053,-4.496028325));
#162821=CARTESIAN_POINT('Ctrl Pts',(-6.24980418500001,0.744288122,-4.166470877));
#162822=CARTESIAN_POINT('Ctrl Pts',(-6.459072287,0.679844992,-3.811874236));
#162823=CARTESIAN_POINT('Ctrl Pts',(-5.657221867,0.809946053,-4.534130649));
#162824=CARTESIAN_POINT('Ctrl Pts',(-5.906141128,0.744288122,-4.223554798));
#162825=CARTESIAN_POINT('Ctrl Pts',(-6.119566318,0.679844992,-3.887596697));
#162826=CARTESIAN_POINT('',(-6.11703469298358,0.680609079912898,-3.89157896256683));
#162827=CARTESIAN_POINT('Origin',(0.134168955827877,0.946280612859217,0.136471289280882));
#162828=CARTESIAN_POINT('Origin',(-17.5208345759338,-0.918884980963102,
-10.6165118135106));
#162829=CARTESIAN_POINT('Ctrl Pts',(-6.18987502407395,0.679837254,-4.2354292642493));
#162830=CARTESIAN_POINT('Ctrl Pts',(-6.41938236008868,0.744719353,-3.90001539367355));
#162831=CARTESIAN_POINT('Ctrl Pts',(-6.61130178639777,0.809946053,-3.5417654580932));
#162832=CARTESIAN_POINT('Ctrl Pts',(-6.61420311981289,0.810932114744282,
-3.53634963058135));
#162833=CARTESIAN_POINT('Ctrl Pts',(-6.61710445322799,0.811918176488562,
-3.53093380306951));
#162834=CARTESIAN_POINT('Ctrl Pts',(-6.114524963,0.679837254,-3.895521079));
#162835=CARTESIAN_POINT('Ctrl Pts',(-6.32561352300001,0.744719353,-3.564190239));
#162836=CARTESIAN_POINT('Ctrl Pts',(-6.499663225,0.809946053,-3.211989719));
#162837=CARTESIAN_POINT('Ctrl Pts',(-6.50229441365044,0.810932114744282,
-3.20666534325988));
#162838=CARTESIAN_POINT('Ctrl Pts',(-6.50492560230089,0.811918176488562,
-3.20134096751977));
#162839=CARTESIAN_POINT('Origin',(0.177955159893456,0.803568129644429,0.0891001020318583));
#162840=CARTESIAN_POINT('Ctrl Pts',(-6.829143632,0.809946053,-3.100451136));
#162841=CARTESIAN_POINT('Ctrl Pts',(-6.999355314,0.744288122,-2.725537947));
#162842=CARTESIAN_POINT('Ctrl Pts',(-7.127503049,0.679844992,-2.334245122));
#162843=CARTESIAN_POINT('Ctrl Pts',(-6.499663225,0.809946053,-3.211989719));
#162844=CARTESIAN_POINT('Ctrl Pts',(-6.675998265,0.744288122,-2.855164676));
#162845=CARTESIAN_POINT('Ctrl Pts',(-6.812212632,0.679844992,-2.481180981));
#162846=CARTESIAN_POINT('',(-6.81059626498796,0.680609079812778,-2.4856143691262));
#162847=CARTESIAN_POINT('Origin',(0.160369492607678,0.946280612470604,0.104438320064307));
#162848=CARTESIAN_POINT('Origin',(-19.3937873098339,-0.9189196105624,-6.60195672059528));
#162849=CARTESIAN_POINT('Ctrl Pts',(-6.95565127974782,0.679837254,-2.80576712312369));
#162850=CARTESIAN_POINT('Ctrl Pts',(-7.1076887940586,0.744719353,-2.42885774909654));
#162851=CARTESIAN_POINT('Ctrl Pts',(-7.21810810459673,0.809946053,-2.03772649393948));
#162852=CARTESIAN_POINT('Ctrl Pts',(-7.21977736329806,0.81093211455031,
-2.03181358570044));
#162853=CARTESIAN_POINT('Ctrl Pts',(-7.22144662199938,0.811918176100622,
-2.0259006774614));
#162854=CARTESIAN_POINT('Ctrl Pts',(-6.80899264800001,0.679837254,-2.490003838));
#162855=CARTESIAN_POINT('Ctrl Pts',(-6.943919739,0.744719353,-2.121041529));
#162856=CARTESIAN_POINT('Ctrl Pts',(-7.038187555,0.809946053,-1.73965972));
#162857=CARTESIAN_POINT('Ctrl Pts',(-7.03961264424704,0.81093211455031,
-1.73389419855183));
#162858=CARTESIAN_POINT('Ctrl Pts',(-7.04103773349406,0.811918176100623,
-1.72812867710368));
#162859=CARTESIAN_POINT('Origin',(0.192948619704593,0.803568097880944,0.0487619255622365));
#162860=CARTESIAN_POINT('Ctrl Pts',(-7.335987395,0.809946053,-1.559900299));
#162861=CARTESIAN_POINT('Ctrl Pts',(-7.421624369,0.744288122,-1.157161891));
#162862=CARTESIAN_POINT('Ctrl Pts',(-7.46265969,0.679844992,-0.7474693));
#162863=CARTESIAN_POINT('Ctrl Pts',(-7.038187555,0.809946053,-1.73965972));
#162864=CARTESIAN_POINT('Ctrl Pts',(-7.133693143,0.744288122,-1.353270226));
#162865=CARTESIAN_POINT('Ctrl Pts',(-7.186327454,0.679844992,-0.958748));
#162866=CARTESIAN_POINT('',(-7.18570192399795,0.680609079819347,-0.963425209256815));
#162867=CARTESIAN_POINT('Origin',(0.179071211428947,0.946280567038781,0.0675218811833105));
#162868=CARTESIAN_POINT('Origin',(-20.3590065423551,-0.918863189645757,
-2.27845220396367));
#162869=CARTESIAN_POINT('Ctrl Pts',(-7.39618901112522,0.679837254,-1.24491042948448));
#162870=CARTESIAN_POINT('Ctrl Pts',(-7.46364759923879,0.744719353,-0.844129415789026));
#162871=CARTESIAN_POINT('Ctrl Pts',(-7.48740370966554,0.809946053,-0.438405704310963));
#162872=CARTESIAN_POINT('Ctrl Pts',(-7.48776284161505,0.810932114754673,
-0.432272194032922));
#162873=CARTESIAN_POINT('Ctrl Pts',(-7.48812197356457,0.811918176509348,
-0.42613868375488));
#162874=CARTESIAN_POINT('Ctrl Pts',(-7.185079405,0.679837254,-0.968056785));
#162875=CARTESIAN_POINT('Ctrl Pts',(-7.23753598500001,0.744719353,-0.578715273));
#162876=CARTESIAN_POINT('Ctrl Pts',(-7.247614057,0.809946053,-0.185985165));
#162877=CARTESIAN_POINT('Ctrl Pts',(-7.24776641180808,0.810932114754673,
-0.180048084948309));
#162878=CARTESIAN_POINT('Ctrl Pts',(-7.24791876661615,0.811918176509348,
-0.174111004896619));
#162879=CARTESIAN_POINT('Origin',(0.198919786025193,0.803568105559062,0.00614363756408852));
#162880=CARTESIAN_POINT('Ctrl Pts',(-7.49980854000001,0.809946053,0.053589743));
#162881=CARTESIAN_POINT('Ctrl Pts',(-7.496866517,0.744288122,0.465321769));
#162882=CARTESIAN_POINT('Ctrl Pts',(-7.448870658,0.679844992,0.874257356));
#162883=CARTESIAN_POINT('Ctrl Pts',(-7.24761405700001,0.809946053,-0.185985165));
#162884=CARTESIAN_POINT('Ctrl Pts',(-7.257824457,0.744288122,0.211901635));
#162885=CARTESIAN_POINT('Ctrl Pts',(-7.224417591,0.679844992,0.608514971));
#162886=CARTESIAN_POINT('',(-7.22481214561418,0.680609079902423,0.603812642589529));
#162887=CARTESIAN_POINT('Origin',(0.189399765800756,0.946280567050045,0.02744823793889));
#162888=CARTESIAN_POINT('Origin',(-20.3741608616577,-0.919019427051703,
2.15155633872438));
#162889=CARTESIAN_POINT('Ctrl Pts',(-7.49088916474174,0.679837254,0.374156892912213));
#162890=CARTESIAN_POINT('Ctrl Pts',(-7.47061453742044,0.744719353,0.780069471217557));
#162891=CARTESIAN_POINT('Ctrl Pts',(-7.40659663794375,0.809946053,1.18141444887646));
#162892=CARTESIAN_POINT('Ctrl Pts',(-7.40562885218112,0.810932112713297,
1.18748175127876));
#162893=CARTESIAN_POINT('Ctrl Pts',(-7.40466106641846,0.811918172426596,
1.19354905368104));
#162894=CARTESIAN_POINT('Ctrl Pts',(-7.225199835,0.679837254,0.599155527));
#162895=CARTESIAN_POINT('Ctrl Pts',(-7.192733093,0.744719353,0.990671065));
#162896=CARTESIAN_POINT('Ctrl Pts',(-7.118150181,0.809946053,1.376385849));
#162897=CARTESIAN_POINT('Ctrl Pts',(-7.11702267945809,0.810932112713297,
1.38221686312957));
#162898=CARTESIAN_POINT('Ctrl Pts',(-7.11589517791618,0.811918172426596,
1.38804787725915));
#162899=CARTESIAN_POINT('Origin',(0.195589888903499,0.803568151949699,-0.0367618791827232));
#162900=CARTESIAN_POINT('Ctrl Pts',(-7.312946974,0.809946053,1.664573988));
#162901=CARTESIAN_POINT('Ctrl Pts',(-7.221563518,0.744288122,2.0660475));
#162902=CARTESIAN_POINT('Ctrl Pts',(-7.086780713,0.679844992,2.455104709));
#162903=CARTESIAN_POINT('Ctrl Pts',(-7.118150181,0.809946053,1.376385849));
#162904=CARTESIAN_POINT('Ctrl Pts',(-7.042587967,0.744288122,1.767165211));
#162905=CARTESIAN_POINT('Ctrl Pts',(-6.924701991,0.679844992,2.147324459));
#162906=CARTESIAN_POINT('',(-6.92609818329531,0.680609079950017,2.1428168859889));
#162907=CARTESIAN_POINT('Origin',(0.190872315132972,0.946280526448961,-0.0139088557421879));
#162908=CARTESIAN_POINT('Origin',(-19.4345323938522,-0.918914486389337,
6.48082719568603));
#162909=CARTESIAN_POINT('Ctrl Pts',(-7.23532366753185,0.679837254,1.97572905333991));
#162910=CARTESIAN_POINT('Ctrl Pts',(-7.12826384427363,0.744719353,2.36779317643012));
#162911=CARTESIAN_POINT('Ctrl Pts',(-6.97946534152131,0.809946053,2.74599297580928));
#162912=CARTESIAN_POINT('Ctrl Pts',(-6.97721588704522,0.810932114617301,
2.75171039376601));
#162913=CARTESIAN_POINT('Ctrl Pts',(-6.97496643256913,0.811918176234604,
2.75742781172276));
#162914=CARTESIAN_POINT('Ctrl Pts',(-6.92747795,0.679837254,2.138351993));
#162915=CARTESIAN_POINT('Ctrl Pts',(-6.811605995,0.744719353,2.513734725));
#162916=CARTESIAN_POINT('Ctrl Pts',(-6.655849513,0.809946053,2.874398591));
#162917=CARTESIAN_POINT('Ctrl Pts',(-6.65349487159478,0.810932114617301,
2.87985091029578));
#162918=CARTESIAN_POINT('Ctrl Pts',(-6.65114023018955,0.811918176234604,
2.88530322959156));
#162919=CARTESIAN_POINT('Origin',(0.183114638037944,0.803568143872066,-0.0779485444577915));
#162920=CARTESIAN_POINT('Ctrl Pts',(-6.784140134,0.809946053,3.197724603));
#162921=CARTESIAN_POINT('Ctrl Pts',(-6.608588236,0.744288122,3.570167146));
#162922=CARTESIAN_POINT('Ctrl Pts',(-6.393320778,0.679844992,3.921154095));
#162923=CARTESIAN_POINT('Ctrl Pts',(-6.655849513,0.809946053,2.874398591));
#162924=CARTESIAN_POINT('Ctrl Pts',(-6.49804789100001,0.744288122,3.239798106));
#162925=CARTESIAN_POINT('Ctrl Pts',(-6.301195022,0.679844992,3.585727442));
#162926=CARTESIAN_POINT('',(-6.30352756759927,0.680609079949565,3.58162539327411));
#162927=CARTESIAN_POINT('Origin',(0.183420109496064,0.946280576848784,-0.0546157096338185));
#162928=CARTESIAN_POINT('Origin',(-17.5862892028171,-0.918828340772164,
10.5067409239504));
#162929=CARTESIAN_POINT('Ctrl Pts',(-6.64144247684645,0.679837254,3.48491831999589));
#162930=CARTESIAN_POINT('Ctrl Pts',(-6.45260345462069,0.744719353,3.84480150431211));
#162931=CARTESIAN_POINT('Ctrl Pts',(-6.22598200120882,0.809946053,4.18217192206895));
#162932=CARTESIAN_POINT('Ctrl Pts',(-6.22255606118742,0.810932114816432,
4.18727210476934));
#162933=CARTESIAN_POINT('Ctrl Pts',(-6.21913012116601,0.811918176632866,
4.19237228746973));
#162934=CARTESIAN_POINT('Ctrl Pts',(-6.305834896,0.679837254,3.577561496));
#162935=CARTESIAN_POINT('Ctrl Pts',(-6.111975772,0.744719353,3.919258944));
#162936=CARTESIAN_POINT('Ctrl Pts',(-5.88232872,0.809946053,4.238007649));
#162937=CARTESIAN_POINT('Ctrl Pts',(-5.87885704062279,0.810932114816432,
4.24282631876312));
#162938=CARTESIAN_POINT('Ctrl Pts',(-5.87538536124559,0.811918176632866,
4.24764498852623));
#162939=CARTESIAN_POINT('Origin',(0.16207692372856,0.803568121700288,-0.115490408361313));
#162940=CARTESIAN_POINT('Ctrl Pts',(-5.938114442,0.809946053,4.58135317));
#162941=CARTESIAN_POINT('Ctrl Pts',(-5.686602712,0.744288122,4.907349744));
#162942=CARTESIAN_POINT('Ctrl Pts',(-5.400916269,0.679844992,5.203854673));
#162943=CARTESIAN_POINT('Ctrl Pts',(-5.88232872,0.809946053,4.238007649));
#162944=CARTESIAN_POINT('Ctrl Pts',(-5.649666317,0.744288122,4.560941642));
#162945=CARTESIAN_POINT('Ctrl Pts',(-5.383051178,0.679844992,4.856465795));
#162946=CARTESIAN_POINT('',(-5.38621100825962,0.680609079924947,4.85296107797159));
#162947=CARTESIAN_POINT('Origin',(0.167390889420725,0.946280564445741,-0.0927685709128245));
#162948=CARTESIAN_POINT('Origin',(-14.9171667056585,-0.918935963699563,
14.0422811013448));
#162949=CARTESIAN_POINT('Ctrl Pts',(-5.73701481756621,0.679837254,4.83115667912201));
#162950=CARTESIAN_POINT('Ctrl Pts',(-5.47522650015516,0.744719353,5.1420311871362));
#162951=CARTESIAN_POINT('Ctrl Pts',(-5.18137866338577,0.809946053,5.42279715848552));
#162952=CARTESIAN_POINT('Ctrl Pts',(-5.17693643039999,0.810932115043126,
5.42704162689108));
#162953=CARTESIAN_POINT('Ctrl Pts',(-5.17249419741424,0.811918177086253,
5.43128609529664));
#162954=CARTESIAN_POINT('Ctrl Pts',(-5.389338011,0.679837254,4.8494882));
#162955=CARTESIAN_POINT('Ctrl Pts',(-5.12655635500001,0.744719353,5.14152297));
#162956=CARTESIAN_POINT('Ctrl Pts',(-4.833756773,0.809946053,5.403452179));
#162957=CARTESIAN_POINT('Ctrl Pts',(-4.82933038696402,0.810932115043127,
5.4074118833999));
#162958=CARTESIAN_POINT('Ctrl Pts',(-4.82490400092802,0.811918177086251,
5.4113715877998));
#162959=CARTESIAN_POINT('Origin',(0.133460466573784,0.803568152816683,-0.147631903631662));
#162960=CARTESIAN_POINT('Ctrl Pts',(-4.814429119,0.809946053,5.75076275500001));
#162961=CARTESIAN_POINT('Ctrl Pts',(-4.498717966,0.744288122,6.015070122));
#162962=CARTESIAN_POINT('Ctrl Pts',(-4.155970918,0.679844992,6.24322879000001));
#162963=CARTESIAN_POINT('Ctrl Pts',(-4.833756773,0.809946053,5.403452179));
#162964=CARTESIAN_POINT('Ctrl Pts',(-4.537112626,0.744288122,5.66882061600001));
#162965=CARTESIAN_POINT('Ctrl Pts',(-4.213201843,0.679844992,5.900121205));
#162966=CARTESIAN_POINT('',(-4.21704120849093,0.680609079904585,5.89737769623315));
#162967=CARTESIAN_POINT('Origin',(0.143534843142958,0.946280593422227,-0.126583721164557));
#162968=CARTESIAN_POINT('Origin',(-11.5499800133793,-0.918992406372022,
16.9210941645051));
#162969=CARTESIAN_POINT('Ctrl Pts',(-4.56433072088425,0.679837254,5.95149552184957));
#162970=CARTESIAN_POINT('Ctrl Pts',(-4.24183403969426,0.744719353,6.19882520562349));
#162971=CARTESIAN_POINT('Ctrl Pts',(-3.89449981646425,0.809946053,6.40985842675195));
#162972=CARTESIAN_POINT('Ctrl Pts',(-3.88924901058972,0.810932114023159,
6.41304870977939));
#162973=CARTESIAN_POINT('Ctrl Pts',(-3.88399820471517,0.811918175046322,
6.41623899280684));
#162974=CARTESIAN_POINT('Ctrl Pts',(-4.22084167,0.679837254,5.894658226));
#162975=CARTESIAN_POINT('Ctrl Pts',(-3.90142486,0.744719353,6.123375096));
#162976=CARTESIAN_POINT('Ctrl Pts',(-3.559163733,0.809946053,6.316237292));
#162977=CARTESIAN_POINT('Ctrl Pts',(-3.55398961937663,0.810932114023161,
6.31915287556189));
#162978=CARTESIAN_POINT('Ctrl Pts',(-3.54881550575326,0.811918175046319,
6.3220684591238));
#162979=CARTESIAN_POINT('Origin',(0.0986037502081683,0.803568105149723,
-0.172870385270595));
#162980=CARTESIAN_POINT('Ctrl Pts',(-3.465626441,0.809946053,6.651273064));
#162981=CARTESIAN_POINT('Ctrl Pts',(-3.100478168,0.744288122,6.841532507));
#162982=CARTESIAN_POINT('Ctrl Pts',(-2.716696986,0.679844992,6.99067646800001));
#162983=CARTESIAN_POINT('Ctrl Pts',(-3.559163733,0.809946053,6.316237292));
#162984=CARTESIAN_POINT('Ctrl Pts',(-3.212408591,0.744288122,6.511631839));
#162985=CARTESIAN_POINT('Ctrl Pts',(-2.846347872,0.679844992,6.667893505));
#162986=CARTESIAN_POINT('',(-2.85068724914484,0.680609079940132,6.66603948790399));
#162987=CARTESIAN_POINT('Origin',(0.112967313262388,0.946280564787144,-0.154480030424337));
#162988=CARTESIAN_POINT('Origin',(-7.64227220663124,-0.918948768628997,
19.0080412821093));
#162989=CARTESIAN_POINT('Ctrl Pts',(-3.17822359332481,0.679837254,6.7935490476677));
#162990=CARTESIAN_POINT('Ctrl Pts',(-2.81009813331689,0.744719353,6.9657690488301));
#162991=CARTESIAN_POINT('Ctrl Pts',(-2.42551848805247,0.809946053,7.0972018388643));
#162992=CARTESIAN_POINT('Ctrl Pts',(-2.4197046177963,0.810932115511907,
7.09918876978505));
#162993=CARTESIAN_POINT('Ctrl Pts',(-2.41389074754013,0.811918178023817,
7.1011757007058));
#162994=CARTESIAN_POINT('Ctrl Pts',(-2.854983464,0.679837254,6.664200584));
#162995=CARTESIAN_POINT('Ctrl Pts',(-2.493867074,0.744719353,6.818905009));
#162996=CARTESIAN_POINT('Ctrl Pts',(-2.118148151,0.809946053,6.933682168));
#162997=CARTESIAN_POINT('Ctrl Pts',(-2.11246823242395,0.810932115511907,
6.93541730796129));
#162998=CARTESIAN_POINT('Ctrl Pts',(-2.10678831384789,0.811918178023817,
6.93715244792259));
#162999=CARTESIAN_POINT('Origin',(0.0591363929493419,0.803568159525722,
-0.190025607610674));
#163000=CARTESIAN_POINT('Ctrl Pts',(-1.954774922,0.809946053,7.240777238));
#163001=CARTESIAN_POINT('Ctrl Pts',(-1.557263457,0.744288122,7.348092436));
#163002=CARTESIAN_POINT('Ctrl Pts',(-1.150393323,0.679844992,7.411247884));
#163003=CARTESIAN_POINT('Ctrl Pts',(-2.118148151,0.809946053,6.933682168));
#163004=CARTESIAN_POINT('Ctrl Pts',(-1.7374959,0.744288122,7.049966394));
#163005=CARTESIAN_POINT('Ctrl Pts',(-1.346401839,0.679844992,7.123882515));
#163006=CARTESIAN_POINT('',(-1.35103832225975,0.680609079911867,7.12300468231609));
#163007=CARTESIAN_POINT('Origin',(0.0771176410036584,0.946280540915505,
-0.175153319735645));
#163008=CARTESIAN_POINT('Origin',(-3.37736490900802,-0.918896036187134,
20.2060467750998));
#163009=CARTESIAN_POINT('Ctrl Pts',(-1.64350626238501,0.679837254,7.31794377079529));
#163010=CARTESIAN_POINT('Ctrl Pts',(-1.24696516207443,0.744719353,7.40700127184289));
#163011=CARTESIAN_POINT('Ctrl Pts',(-0.843122609833158,0.809946053,7.45268798029123));
#163012=CARTESIAN_POINT('Ctrl Pts',(-0.837017537601804,0.810932114802311,
7.45337864712052));
#163013=CARTESIAN_POINT('Ctrl Pts',(-0.830912465370449,0.811918176604621,
7.45406931394981));
#163014=CARTESIAN_POINT('Ctrl Pts',(-1.355629403,0.679837254,7.12213233));
#163015=CARTESIAN_POINT('Ctrl Pts',(-0.969698837,0.744719353,7.195590502));
#163016=CARTESIAN_POINT('Ctrl Pts',(-0.578090316999999,0.809946053,7.226915773));
#163017=CARTESIAN_POINT('Ctrl Pts',(-0.572170192219328,0.810932114802312,
7.22738933142286));
#163018=CARTESIAN_POINT('Ctrl Pts',(-0.566250067438653,0.811918176604621,
7.22786288984572));
#163019=CARTESIAN_POINT('Origin',(0.0169039340594927,0.803568164770754,
-0.198295592186956));
#163020=CARTESIAN_POINT('Ctrl Pts',(-0.3525203,0.809946053,7.49171071500001));
#163021=CARTESIAN_POINT('Ctrl Pts',(0.058767163,0.744288122,7.51106372900001));
#163022=CARTESIAN_POINT('Ctrl Pts',(0.469701454,0.679844992,7.485277586));
#163023=CARTESIAN_POINT('Ctrl Pts',(-0.578090317,0.809946053,7.226915773));
#163024=CARTESIAN_POINT('Ctrl Pts',(-0.181339832,0.744288122,7.258652356));
#163025=CARTESIAN_POINT('Ctrl Pts',(0.216500448,0.679844992,7.246766697));
#163026=CARTESIAN_POINT('Origin',(0.0376618935714465,0.946280616501933,
-0.18763604326458));
#163027=CARTESIAN_POINT('Ctrl Pts',(0.211783654,0.680609079,7.246906077));
#163028=CARTESIAN_POINT('Ctrl Pts',(0.604481562,0.745496505000001,7.23542986900001));
#163029=CARTESIAN_POINT('Ctrl Pts',(0.993639891,0.810723991,7.18158616));
#163030=CARTESIAN_POINT('Ctrl Pts',(0.464829365,0.680609079,7.485581718));
#163031=CARTESIAN_POINT('Ctrl Pts',(0.870460713,0.745496505,7.46039338));
#163032=CARTESIAN_POINT('Ctrl Pts',(1.270995025,0.810723991,7.391520253));
#163033=CARTESIAN_POINT('Ctrl Pts',(0.4838423694909,0.680609079,7.50351500371454));
#163034=CARTESIAN_POINT('Ctrl Pts',(0.890445492716139,0.745496505,7.4772963823391));
#163035=CARTESIAN_POINT('Ctrl Pts',(1.29183455785545,0.810723991,7.40729399536943));
#163036=CARTESIAN_POINT('',(0.395386353409136,0.680609080400561,7.42008227489806));
#163037=CARTESIAN_POINT('',(0.304135795241984,0.680609082082805,7.33401370379862));
#163038=CARTESIAN_POINT('',(1.02663072523825,0.76798017562717,7.44739982155537));
#163039=CARTESIAN_POINT('Ctrl Pts',(0.395386359566659,0.680609079136169,
7.42008227135047));
#163040=CARTESIAN_POINT('Ctrl Pts',(0.500009482076225,0.695136944977305,
7.42905580208087));
#163041=CARTESIAN_POINT('Ctrl Pts',(0.604810648040692,0.709660812710993,
7.43582945914476));
#163042=CARTESIAN_POINT('Ctrl Pts',(0.815284577790083,0.738780776738529,
7.44500505794044));
#163043=CARTESIAN_POINT('Ctrl Pts',(0.920936382652429,0.753373671667379,
7.44737846514938));
#163044=CARTESIAN_POINT('Ctrl Pts',(1.02660466604954,0.767949007798904,
7.44752577326926));
#163045=CARTESIAN_POINT('Ctrl Pts',(0.988998379602801,0.809946052545264,
7.18222682905853));
#163046=CARTESIAN_POINT('Ctrl Pts',(0.994923072744043,0.802922931274876,
7.22424856499997));
#163047=CARTESIAN_POINT('Ctrl Pts',(1.00087662461022,0.796078752403875,
7.26632383852537));
#163048=CARTESIAN_POINT('Ctrl Pts',(1.01341493206971,0.782074139994843,
7.35464723293283));
#163049=CARTESIAN_POINT('Ctrl Pts',(1.0200128069643,0.774939590237252,7.40095924419224));
#163050=CARTESIAN_POINT('Ctrl Pts',(1.02663085166062,0.767997185229757,
7.44726315247994));
#163051=CARTESIAN_POINT('Origin',(-5.43456338958359E-14,0.560925699999933,
-6.93889390390723E-14));
#163052=CARTESIAN_POINT('',(1.63504458648,0.680609080181315,7.24848815475887));
#163053=CARTESIAN_POINT('',(1.00401106526424,0.562053379613689,7.24279548290209));
#163054=CARTESIAN_POINT('Ctrl Pts',(1.63504458645295,0.680609079948412,
7.24848815266485));
#163055=CARTESIAN_POINT('Ctrl Pts',(1.58723214217251,0.671661524751094,
7.25010086045261));
#163056=CARTESIAN_POINT('Ctrl Pts',(1.53425686505398,0.661738573429343,
7.25142167916517));
#163057=CARTESIAN_POINT('Ctrl Pts',(1.42431339294704,0.641119488187471,
7.25276715487363));
#163058=CARTESIAN_POINT('Ctrl Pts',(1.37187915142337,0.631275792584381,
7.25284991854614));
#163059=CARTESIAN_POINT('Ctrl Pts',(1.21423924388054,0.601654471621312,
7.25142233155372));
#163060=CARTESIAN_POINT('Ctrl Pts',(1.1090790626735,0.581858135018139,7.24822487778146));
#163061=CARTESIAN_POINT('Ctrl Pts',(1.0040110651189,0.562053380213309,7.24279548352759));
#163062=CARTESIAN_POINT('Ctrl Pts',(1.02663059881587,0.767963166024584,
7.4475364906308));
#163063=CARTESIAN_POINT('Ctrl Pts',(1.12966842526234,0.753333602537456,
7.41856499043498));
#163064=CARTESIAN_POINT('Ctrl Pts',(1.23208600136148,0.738713518212131,
7.38742430932713));
#163065=CARTESIAN_POINT('Ctrl Pts',(1.43495011980214,0.709588701416252,
7.3210310126199));
#163066=CARTESIAN_POINT('Ctrl Pts',(1.53538301094752,0.695086898841886,
7.28581043640534));
#163067=CARTESIAN_POINT('Ctrl Pts',(1.63504458150421,0.680609078982399,
7.24848815279085));
#163068=CARTESIAN_POINT('Ctrl Pts',(1.00401106512942,0.562053379355767,
7.24279548266039));
#163069=CARTESIAN_POINT('Ctrl Pts',(0.904086842224673,0.582224590119512,
7.27701127625761));
#163070=CARTESIAN_POINT('Ctrl Pts',(0.803350409959279,0.602198953310061,
7.30891500817337));
#163071=CARTESIAN_POINT('Ctrl Pts',(0.651321854294389,0.631811121642218,
7.3532027391429));
#163072=CARTESIAN_POINT('Ctrl Pts',(0.600593664771072,0.641604433043982,
7.3673457081378));
#163073=CARTESIAN_POINT('Ctrl Pts',(0.494453675786446,0.66191430093601,
7.39561665600437));
#163074=CARTESIAN_POINT('Ctrl Pts',(0.443161379792506,0.671620850615904,
7.40853555255282));
#163075=CARTESIAN_POINT('Ctrl Pts',(0.395386352780817,0.680609080018574,
7.42008227259572));
#163076=CARTESIAN_POINT('Ctrl Pts',(0.984280001000001,0.810731746,7.182874973));
#163077=CARTESIAN_POINT('Ctrl Pts',(1.378634468,0.745065281,7.128835996));
#163078=CARTESIAN_POINT('Ctrl Pts',(1.764702859,0.680609079,7.03195021400001));
#163079=CARTESIAN_POINT('Ctrl Pts',(0.773984637,0.810731746,7.45995628600001));
#163080=CARTESIAN_POINT('Ctrl Pts',(1.183551433,0.745065281,7.417462952));
#163081=CARTESIAN_POINT('Ctrl Pts',(1.586004669,0.680609079,7.330388065));
#163082=CARTESIAN_POINT('Ctrl Pts',(0.758157006316509,0.810731746,7.48081048177514));
#163083=CARTESIAN_POINT('Ctrl Pts',(1.16886874018232,0.745065281,7.43918611687617));
#163084=CARTESIAN_POINT('Ctrl Pts',(1.5725551620716,0.680609079,7.35284963523035));
#163085=CARTESIAN_POINT('',(1.69948476214558,0.680609081791274,7.14086879303845));
#163086=CARTESIAN_POINT('Ctrl Pts',(1.764702859,0.680609079,7.03195021400001));
#163087=CARTESIAN_POINT('Ctrl Pts',(2.145752663,0.745496505000001,6.936323872));
#163088=CARTESIAN_POINT('Ctrl Pts',(2.51423788,0.810723991,6.800081461));
#163089=CARTESIAN_POINT('Ctrl Pts',(2.06314071,0.680609079,7.210648404));
#163090=CARTESIAN_POINT('Ctrl Pts',(2.453873874,0.745496505000001,7.098850206));
#163091=CARTESIAN_POINT('Ctrl Pts',(2.83023823,0.810723991,6.94548425700001));
#163092=CARTESIAN_POINT('Ctrl Pts',(2.085564327413,0.680609079,7.22407518559466));
#163093=CARTESIAN_POINT('Ctrl Pts',(2.47702506654861,0.745496505000001,
7.11106188867009));
#163094=CARTESIAN_POINT('Ctrl Pts',(2.85398143458022,0.810723991,6.95640933455756));
#163095=CARTESIAN_POINT('',(1.98124079348741,0.680609080419527,7.1616084961454));
#163096=CARTESIAN_POINT('',(1.87253223753562,0.680609082082805,7.09651615128199));
#163097=CARTESIAN_POINT('',(2.60359948730395,0.767980175627753,7.05258849344245));
#163098=CARTESIAN_POINT('Ctrl Pts',(1.9812407986416,0.680609079126786,7.16160849143538));
#163099=CARTESIAN_POINT('Ctrl Pts',(2.08534693316848,0.695136944794904,
7.14788134749876));
#163100=CARTESIAN_POINT('Ctrl Pts',(2.18915404078839,0.709660812349475,
7.13196748774765));
#163101=CARTESIAN_POINT('Ctrl Pts',(2.39667969198913,0.738780776740227,
7.09568289240512));
#163102=CARTESIAN_POINT('Ctrl Pts',(2.50037162874458,0.753373671672762,
7.07528879568255));
#163103=CARTESIAN_POINT('Ctrl Pts',(2.60360111327753,0.767949007806505,
7.05271710243074));
#163104=CARTESIAN_POINT('Ctrl Pts',(2.50984261070199,0.809946052649527,
6.80170493940386));
#163105=CARTESIAN_POINT('Ctrl Pts',(2.52466221878819,0.802922931334229,
6.84147059690226));
#163106=CARTESIAN_POINT('Ctrl Pts',(2.53952151974974,0.796078752498655,
6.88128233605344));
#163107=CARTESIAN_POINT('Ctrl Pts',(2.57075360736643,0.782074140027835,
6.96484541348759));
#163108=CARTESIAN_POINT('Ctrl Pts',(2.58715294097028,0.774939590254329,
7.0086563276866));
#163109=CARTESIAN_POINT('Ctrl Pts',(2.603570230945,0.767997185232552,7.05245499244542));
#163110=CARTESIAN_POINT('Origin',(8.00141203294302E-14,0.560925700000022,
-2.07733136248223E-13));
#163111=CARTESIAN_POINT('',(3.15502884266931,0.680609080190964,6.72753627498307));
#163112=CARTESIAN_POINT('',(2.53752478129952,0.562053379772718,6.85763024758604));
#163113=CARTESIAN_POINT('Ctrl Pts',(3.15502884219952,0.68060907997646,6.7275362729842));
#163114=CARTESIAN_POINT('Ctrl Pts',(3.1086809112377,0.671661524850685,6.73938953863211));
#163115=CARTESIAN_POINT('Ctrl Pts',(3.05722810394215,0.661738573577959,
6.75206759590499));
#163116=CARTESIAN_POINT('Ctrl Pts',(2.95014428708656,0.641119488421689,
6.77701621164918));
#163117=CARTESIAN_POINT('Ctrl Pts',(2.89895372092233,0.631275792858778,
6.78836885231258));
#163118=CARTESIAN_POINT('Ctrl Pts',(2.74469245849335,0.601654472053282,
6.8208625617643));
#163119=CARTESIAN_POINT('Ctrl Pts',(2.64130350622483,0.581858135561308,
6.84034619314135));
#163120=CARTESIAN_POINT('Ctrl Pts',(2.53752478128929,0.562053380894578,
6.85763024881006));
#163121=CARTESIAN_POINT('Ctrl Pts',(2.6036287436629,0.767963166022953,7.05272199443948));
#163122=CARTESIAN_POINT('Ctrl Pts',(2.69802958696195,0.753333602540172,
7.00227774486911));
#163123=CARTESIAN_POINT('Ctrl Pts',(2.79135837124678,0.738713518219378,
6.94984836411526));
#163124=CARTESIAN_POINT('Ctrl Pts',(2.97520704219334,0.709588701614233,
6.84139751752858));
#163125=CARTESIAN_POINT('Ctrl Pts',(3.06572048612681,0.695086898944589,
6.78541027559763));
#163126=CARTESIAN_POINT('Ctrl Pts',(3.15502883751132,0.680609078987249,
6.72753627409024));
#163127=CARTESIAN_POINT('Ctrl Pts',(2.53752478053378,0.562053378680438,
6.85763024672876));
#163128=CARTESIAN_POINT('Ctrl Pts',(2.44729211420189,0.58222458955668,6.9125268486052));
#163129=CARTESIAN_POINT('Ctrl Pts',(2.35576920258763,0.602198952866584,
6.96534004450702));
#163130=CARTESIAN_POINT('Ctrl Pts',(2.2168143959035,0.631811365719166,7.04127462546337));
#163131=CARTESIAN_POINT('Ctrl Pts',(2.17031136200528,0.641604918880096,
7.06599260123164));
#163132=CARTESIAN_POINT('Ctrl Pts',(2.07273008286579,0.66191481702943,7.11641958370329));
#163133=CARTESIAN_POINT('Ctrl Pts',(2.02541538654176,0.671621107824337,
7.14006213116803));
#163134=CARTESIAN_POINT('Ctrl Pts',(1.98124079243869,0.680609080077605,
7.16160849413794));
#163135=CARTESIAN_POINT('Ctrl Pts',(2.505373877,0.810731746,6.803352243));
#163136=CARTESIAN_POINT('Ctrl Pts',(2.878891773,0.745065281,6.665802114));
#163137=CARTESIAN_POINT('Ctrl Pts',(3.23510652,0.680609079,6.488188176));
#163138=CARTESIAN_POINT('Ctrl Pts',(2.359559393,0.810731746,7.119162835));
#163139=CARTESIAN_POINT('Ctrl Pts',(2.750415934,0.745065281,6.98961821800001));
#163140=CARTESIAN_POINT('Ctrl Pts',(3.124741511,0.680609079,6.818063544));
#163141=CARTESIAN_POINT('Ctrl Pts',(2.34858483909455,0.810731746,7.14293194401264));
#163142=CARTESIAN_POINT('Ctrl Pts',(2.74074635261154,0.745065281,7.01398985236249));
#163143=CARTESIAN_POINT('Ctrl Pts',(3.11643501971519,0.680609079,6.84289122166883));
#163144=CARTESIAN_POINT('',(3.1948274609048,0.680609081791274,6.60858026205276));
#163145=CARTESIAN_POINT('Ctrl Pts',(3.23510652,0.680609079,6.488188176));
#163146=CARTESIAN_POINT('Ctrl Pts',(3.586690754,0.745496505000001,6.31288308));
#163147=CARTESIAN_POINT('Ctrl Pts',(3.917272901,0.810723991,6.100612512));
#163148=CARTESIAN_POINT('Ctrl Pts',(3.564981888,0.680609079,6.59855318500001));
#163149=CARTESIAN_POINT('Ctrl Pts',(3.922546621,0.745496505000001,6.405372686));
#163150=CARTESIAN_POINT('Ctrl Pts',(4.257142641,0.810723991,6.174685136));
#163151=CARTESIAN_POINT('Ctrl Pts',(3.58976761490954,0.680609079,6.60684564099643));
#163152=CARTESIAN_POINT('Ctrl Pts',(3.94778170251245,0.745496505000001,
6.41232204426881));
#163153=CARTESIAN_POINT('Ctrl Pts',(4.28267931144474,0.810723991,6.18025070411462));
#163154=CARTESIAN_POINT('',(3.47445461509448,0.680609080408186,6.56826586412171));
#163155=CARTESIAN_POINT('',(3.35549859635723,0.680609082082805,6.52846725931103));
#163156=CARTESIAN_POINT('',(4.05882683126017,0.767980175582968,6.32800596564452));
#163157=CARTESIAN_POINT('Ctrl Pts',(3.47445461920584,0.680609079123292,
6.56826585833953));
#163158=CARTESIAN_POINT('Ctrl Pts',(3.57317587970167,0.695136944718301,
6.5324799059097));
#163159=CARTESIAN_POINT('Ctrl Pts',(3.67113502507767,0.70966081219651,6.49462264385934));
#163160=CARTESIAN_POINT('Ctrl Pts',(3.86600872735986,0.738780776674586,
6.41457448117895));
#163161=CARTESIAN_POINT('Ctrl Pts',(3.96289227645095,0.753373671607418,
6.37236648572888));
#163162=CARTESIAN_POINT('Ctrl Pts',(4.05885606630356,0.767949007742122,
6.32813121830147));
#163163=CARTESIAN_POINT('Ctrl Pts',(3.91332939002799,0.809946052501965,
6.10314288788829));
#163164=CARTESIAN_POINT('Ctrl Pts',(3.93635096497877,0.802922931194473,
6.13879306854643));
#163165=CARTESIAN_POINT('Ctrl Pts',(3.95942121084569,0.796078752396678,
6.17447972056928));
#163166=CARTESIAN_POINT('Ctrl Pts',(4.00788670128113,0.782074139948338,
6.24937516371998));
#163167=CARTESIAN_POINT('Ctrl Pts',(4.0333206790917,0.774939590190608,6.28863643094237));
#163168=CARTESIAN_POINT('Ctrl Pts',(4.05876956016351,0.767997185182016,
6.32788187504603));
#163169=CARTESIAN_POINT('Origin',(-5.14345510627123E-13,0.560925699999955,
-8.15320033709099E-13));
#163170=CARTESIAN_POINT('',(4.52748745641034,0.680609080270237,5.89201227580179));
#163171=CARTESIAN_POINT('',(3.95238665241763,0.562053379603276,6.15180984556242));
#163172=CARTESIAN_POINT('Ctrl Pts',(4.52748745566869,0.680609080100659,
5.89201227426056));
#163173=CARTESIAN_POINT('Ctrl Pts',(4.48477121484114,0.671661524881241,
5.91355185251235));
#163174=CARTESIAN_POINT('Ctrl Pts',(4.43724675273578,0.661738573524651,
5.9369943366818));
#163175=CARTESIAN_POINT('Ctrl Pts',(4.33802971034782,0.641119488246075,
5.98437952315467));
#163176=CARTESIAN_POINT('Ctrl Pts',(4.2904764331093,0.631275792632267,6.00647120401911));
#163177=CARTESIAN_POINT('Ctrl Pts',(4.14680689960514,0.601654471665006,
6.07136684033878));
#163178=CARTESIAN_POINT('Ctrl Pts',(4.05002352800819,0.581858135071578,
6.11262052392551));
#163179=CARTESIAN_POINT('Ctrl Pts',(3.95238665256539,0.562053380281048,
6.15180984627309));
#163180=CARTESIAN_POINT('Ctrl Pts',(4.05888410235683,0.767963165983919,
6.328130056243));
#163181=CARTESIAN_POINT('Ctrl Pts',(4.14023388382345,0.753333602501295,
6.25857177437937));
#163182=CARTESIAN_POINT('Ctrl Pts',(4.22010992589841,0.738713518183888,
6.18730523359868));
#163183=CARTESIAN_POINT('Ctrl Pts',(4.37634659231398,0.709588701304981,
6.04186787645319));
#163184=CARTESIAN_POINT('Ctrl Pts',(4.45270827935236,0.695086898787018,
5.96773187095885));
#163185=CARTESIAN_POINT('Ctrl Pts',(4.52748745077445,0.680609078979747,
5.89201227660773));
#163186=CARTESIAN_POINT('Ctrl Pts',(3.95238665216459,0.562053379311736,
6.15180984537846));
#163187=CARTESIAN_POINT('Ctrl Pts',(3.87606472234309,0.582224590119441,
6.2248203509263));
#163188=CARTESIAN_POINT('Ctrl Pts',(3.79803484175112,0.602198953352741,
6.29607352398231));
#163189=CARTESIAN_POINT('Ctrl Pts',(3.67865339709232,0.631811121720754,
6.40010311370272));
#163190=CARTESIAN_POINT('Ctrl Pts',(3.63855221784974,0.641604433110253,
6.43423913857157));
#163191=CARTESIAN_POINT('Ctrl Pts',(3.55409282914178,0.661914302620708,
6.50446418606829));
#163192=CARTESIAN_POINT('Ctrl Pts',(3.51296570938833,0.67162085133905,6.53772613200226));
#163193=CARTESIAN_POINT('Ctrl Pts',(3.47445461360268,0.680609080045858,
6.56826586234716));
#163194=CARTESIAN_POINT('Ctrl Pts',(3.909319254,0.810731746,6.105712323));
#163195=CARTESIAN_POINT('Ctrl Pts',(4.244535298,0.745065281,5.891082733));
#163196=CARTESIAN_POINT('Ctrl Pts',(4.554240196,0.680609079,5.64104566900001));
#163197=CARTESIAN_POINT('Ctrl Pts',(3.834803774,0.810731746,6.44548524300001));
#163198=CARTESIAN_POINT('Ctrl Pts',(4.188674043,0.745065281,6.234946704));
#163199=CARTESIAN_POINT('Ctrl Pts',(4.517368912,0.680609079,5.98693394900001));
#163200=CARTESIAN_POINT('Ctrl Pts',(3.82919545491968,0.810731746,6.47105784818504));
#163201=CARTESIAN_POINT('Ctrl Pts',(4.18446971200371,0.745065281,6.26082721727852));
#163202=CARTESIAN_POINT('Ctrl Pts',(4.51459383861158,0.680609079,6.0129668194906));
#163203=CARTESIAN_POINT('',(4.5407835784437,0.680609081791273,5.7672818619153));
#163204=CARTESIAN_POINT('Ctrl Pts',(4.554240196,0.680609079,5.641045669));
#163205=CARTESIAN_POINT('Ctrl Pts',(4.859919172,0.745496505000001,5.394258892));
#163206=CARTESIAN_POINT('Ctrl Pts',(5.13714059500001,0.810723991,5.11588570100001));
#163207=CARTESIAN_POINT('Ctrl Pts',(4.900128476,0.680609079,5.677916952));
#163208=CARTESIAN_POINT('Ctrl Pts',(5.207805447,0.745496505,5.412387059));
#163209=CARTESIAN_POINT('Ctrl Pts',(5.484987794,0.810723991,5.115164602));
#163210=CARTESIAN_POINT('Ctrl Pts',(4.92611735858291,0.680609079,5.68068733625404));
#163211=CARTESIAN_POINT('Ctrl Pts',(5.23394445221053,0.745496505,5.41374914852672));
#163212=CARTESIAN_POINT('Ctrl Pts',(5.51112386317125,0.810723991,5.11511042104527));
#163213=CARTESIAN_POINT('',(4.80520680196463,0.680609080418716,5.66779841952658));
#163214=CARTESIAN_POINT('',(4.68047638465213,0.680609082082805,5.65450231179023));
#163215=CARTESIAN_POINT('',(5.32426794337827,0.767980175627075,5.30753291231732));
#163216=CARTESIAN_POINT('Ctrl Pts',(4.80520680463989,0.680609079133469,
5.66779841310038));
#163217=CARTESIAN_POINT('Ctrl Pts',(4.89392709595556,0.695136944934551,
5.61162696295109));
#163218=CARTESIAN_POINT('Ctrl Pts',(4.98145781965976,0.709660812623477,
5.55359646132803));
#163219=CARTESIAN_POINT('Ctrl Pts',(5.15456749200145,0.738780776780364,
5.4335276963075));
#163220=CARTESIAN_POINT('Ctrl Pts',(5.24011248597806,0.753373671704646,
5.37147940132803));
#163221=CARTESIAN_POINT('Ctrl Pts',(5.32432342063299,0.767949007828576,
5.30764895191927));
#163222=CARTESIAN_POINT('Ctrl Pts',(5.13383323629986,0.809946052590815,
5.11920465603347));
#163223=CARTESIAN_POINT('Ctrl Pts',(5.16398031444869,0.802922931346625,
5.14907239727279));
#163224=CARTESIAN_POINT('Ctrl Pts',(5.19418276650767,0.796078752460896,
5.17896529494774));
#163225=CARTESIAN_POINT('Ctrl Pts',(5.2576154669957,0.782074140043799,5.24169107672195));
#163226=CARTESIAN_POINT('Ctrl Pts',(5.29089482450484,0.774939590271432,
5.27456688412485));
#163227=CARTESIAN_POINT('Ctrl Pts',(5.32418533538452,0.767997185238257,
5.30742403456664));
#163228=CARTESIAN_POINT('Origin',(4.23272528138341E-13,0.560925700000045,
4.69242700251726E-13));
#163229=CARTESIAN_POINT('',(5.68824578855907,0.680609080239763,4.78098433135749));
#163230=CARTESIAN_POINT('',(5.18243931891629,0.562053379594032,5.15833765197501));
#163231=CARTESIAN_POINT('Ctrl Pts',(5.68824578738182,0.680609080006679,
4.78098432984365));
#163232=CARTESIAN_POINT('Ctrl Pts',(5.65115860086945,0.671661524746398,
4.8112030540888));
#163233=CARTESIAN_POINT('Ctrl Pts',(5.60978467527665,0.661738573380851,
4.84431382069644));
#163234=CARTESIAN_POINT('Ctrl Pts',(5.52307368641531,0.641119488099716,
4.91191989931352));
#163235=CARTESIAN_POINT('Ctrl Pts',(5.48138123678228,0.631275792512947,
4.94371763787759));
#163236=CARTESIAN_POINT('Ctrl Pts',(5.35502126062242,0.601654471582552,
5.03798075320548));
#163237=CARTESIAN_POINT('Ctrl Pts',(5.26936895293617,0.581858134996619,
5.0990755126484));
#163238=CARTESIAN_POINT('Ctrl Pts',(5.18243931919477,0.562053380229362,
5.15833765259582));
#163239=CARTESIAN_POINT('Ctrl Pts',(5.32435055137201,0.767963166015893,
5.307641790068));
#163240=CARTESIAN_POINT('Ctrl Pts',(5.38884544570401,0.753333602523817,
5.22222194381651));
#163241=CARTESIAN_POINT('Ctrl Pts',(5.45153383068676,0.738713518204724,
5.1354505872009));
#163242=CARTESIAN_POINT('Ctrl Pts',(5.57285303448452,0.709588702185143,
4.95982721477735));
#163243=CARTESIAN_POINT('Ctrl Pts',(5.63149237997482,0.695086899228591,
4.87100895977395));
#163244=CARTESIAN_POINT('Ctrl Pts',(5.68824578310611,0.680609079003327,
4.78098433337133));
#163245=CARTESIAN_POINT('Ctrl Pts',(5.18243931864758,0.562053379320748,
5.15833765185759));
#163246=CARTESIAN_POINT('Ctrl Pts',(5.12359685382635,0.582224590076786,
5.24604817094438));
#163247=CARTESIAN_POINT('Ctrl Pts',(5.06270859463274,0.602198953250477,
5.33240960193516));
#163248=CARTESIAN_POINT('Ctrl Pts',(4.96848150840265,0.631811121639871,
5.45967051949857));
#163249=CARTESIAN_POINT('Ctrl Pts',(4.93665610844004,0.641604433114055,
5.50162903160987));
#163250=CARTESIAN_POINT('Ctrl Pts',(4.8692674654864,0.661914356005798,5.5883687565125));
#163251=CARTESIAN_POINT('Ctrl Pts',(4.8362522563773,0.671620886396292,5.629694100555));
#163252=CARTESIAN_POINT('Ctrl Pts',(4.80520680015511,0.680609080072647,
5.6677984181339));
#163253=CARTESIAN_POINT('Ctrl Pts',(5.130469208,0.810731746,5.12257608100001));
#163254=CARTESIAN_POINT('Ctrl Pts',(5.41170907,0.745065281,4.840902871));
#163255=CARTESIAN_POINT('Ctrl Pts',(5.660422662,0.680609079,4.530134136));
#163256=CARTESIAN_POINT('Ctrl Pts',(5.130736993,0.810731746,5.47042392400001));
#163257=CARTESIAN_POINT('Ctrl Pts',(5.431074409,0.745065281,5.188736012));
#163258=CARTESIAN_POINT('Ctrl Pts',(5.698769164,0.680609079,4.875861977));
#163259=CARTESIAN_POINT('Ctrl Pts',(5.13075714752001,0.810731746,5.49660427881381));
#163260=CARTESIAN_POINT('Ctrl Pts',(5.43253191824237,0.745065281,5.21491526028523));
#163261=CARTESIAN_POINT('Ctrl Pts',(5.70165526793432,0.680609079,4.9018827723809));
#163262=CARTESIAN_POINT('',(5.674417702854,0.680609081791274,4.65631177227276));
#163263=CARTESIAN_POINT('Ctrl Pts',(5.660422662,0.680609079,4.530134136));
#163264=CARTESIAN_POINT('Ctrl Pts',(5.905903171,0.745496505000001,4.223405152));
#163265=CARTESIAN_POINT('Ctrl Pts',(6.116801304,0.810723991,3.891945762));
#163266=CARTESIAN_POINT('Ctrl Pts',(6.006150502,0.680609079,4.491787634));
#163267=CARTESIAN_POINT('Ctrl Pts',(6.249553078,0.745496505000001,4.166324228));
#163268=CARTESIAN_POINT('Ctrl Pts',(6.456361013,0.810723991,3.816464655));
#163269=CARTESIAN_POINT('Ctrl Pts',(6.03212733019216,0.680609079,4.48890640669061));
#163270=CARTESIAN_POINT('Ctrl Pts',(6.27537377728876,0.745496505000001,
4.16203535917243));
#163271=CARTESIAN_POINT('Ctrl Pts',(6.48187438855481,0.810723991,3.81079325824962));
#163272=CARTESIAN_POINT('',(5.91127285818404,0.680609080424646,4.502311021008));
#163273=CARTESIAN_POINT('',(5.7866002991413,0.680609082082805,4.51613912119474));
#163274=CARTESIAN_POINT('',(6.34075220412026,0.767980175591255,4.0388855187467));
#163275=CARTESIAN_POINT('Ctrl Pts',(5.91127285940175,0.68060907913183,4.50231101419889));
#163276=CARTESIAN_POINT('Ctrl Pts',(5.98584371810131,0.695136944892643,
4.42838058139215));
#163277=CARTESIAN_POINT('Ctrl Pts',(6.05885317952404,0.709660812546431,
4.35289028258863));
#163278=CARTESIAN_POINT('Ctrl Pts',(6.20210440905884,0.738780776759475,
4.19841519563974));
#163279=CARTESIAN_POINT('Ctrl Pts',(6.27231085937759,0.753373671676262,
4.11942791022291));
#163280=CARTESIAN_POINT('Ctrl Pts',(6.34083132940497,0.767949007777661,
4.03898691946156));
#163281=CARTESIAN_POINT('Ctrl Pts',(6.11428474712324,0.809946052491448,
3.89589810638952));
#163282=CARTESIAN_POINT('Ctrl Pts',(6.15014768492995,0.802922931193169,
3.9185868255266));
#163283=CARTESIAN_POINT('Ctrl Pts',(6.18607010946796,0.796078752357421,
3.94128820902625));
#163284=CARTESIAN_POINT('Ctrl Pts',(6.26150397751342,0.782074139939529,
3.98891134102536));
#163285=CARTESIAN_POINT('Ctrl Pts',(6.30107260881191,0.774939590191973,
4.01386445207685));
#163286=CARTESIAN_POINT('Ctrl Pts',(6.34064812196814,0.767997185198326,
4.03879694473977));
#163287=CARTESIAN_POINT('Origin',(1.99493199737333E-14,0.560925700000045,
3.53449908230274E-14));
#163288=CARTESIAN_POINT('',(6.5830280693915,0.680609080232035,3.4464028733435));
#163289=CARTESIAN_POINT('',(6.17016688332989,0.562053379630163,3.92366732259758));
#163290=CARTESIAN_POINT('Ctrl Pts',(6.58302806789696,0.680609079983393,
3.44640287209903));
#163291=CARTESIAN_POINT('Ctrl Pts',(6.55330409170877,0.671661524738439,
3.48388774809406));
#163292=CARTESIAN_POINT('Ctrl Pts',(6.52001530162182,0.661738573384056,
3.52511857431923));
#163293=CARTESIAN_POINT('Ctrl Pts',(6.44986487602543,0.641119488114012,
3.6097843597748));
#163294=CARTESIAN_POINT('Ctrl Pts',(6.41598274652342,0.631275792517561,
3.64980132916812));
#163295=CARTESIAN_POINT('Ctrl Pts',(6.31284077969711,0.601654471558908,
3.76902428504385));
#163296=CARTESIAN_POINT('Ctrl Pts',(6.24232454263553,0.581858134953565,
3.84710339731782));
#163297=CARTESIAN_POINT('Ctrl Pts',(6.17016688366903,0.562053380161616,
3.92366732305467));
#163298=CARTESIAN_POINT('Ctrl Pts',(6.34085628627237,0.767963165984184,
4.03897409275364));
#163299=CARTESIAN_POINT('Ctrl Pts',(6.38548058389055,0.753333602495987,
3.94168681918178));
#163300=CARTESIAN_POINT('Ctrl Pts',(6.42805007255938,0.738713518174777,
3.84346797891347));
#163301=CARTESIAN_POINT('Ctrl Pts',(6.50877906791305,0.709588701869491,
3.6458705387371));
#163302=CARTESIAN_POINT('Ctrl Pts',(6.54695415822974,0.695086899074947,
3.54652308034844));
#163303=CARTESIAN_POINT('Ctrl Pts',(6.58302806441533,0.680609078994068,
3.44640287661631));
#163304=CARTESIAN_POINT('Ctrl Pts',(6.17016688308926,0.562053379401562,
3.92366732254997));
#163305=CARTESIAN_POINT('Ctrl Pts',(6.13155529124598,0.582224590154151,
4.02197660907586));
#163306=CARTESIAN_POINT('Ctrl Pts',(6.09065572053444,0.602198953333873,
4.11940813371797));
#163307=CARTESIAN_POINT('Ctrl Pts',(6.02598894669228,0.631811121710703,
4.26394979991525));
#163308=CARTESIAN_POINT('Ctrl Pts',(6.00392744676189,0.641604433160521,
4.31176886545943));
#163309=CARTESIAN_POINT('Ctrl Pts',(5.95676085305035,0.661914328754221,
4.41096709673942));
#163310=CARTESIAN_POINT('Ctrl Pts',(5.93340123289289,0.671620868693789,
4.45842361264364));
#163311=CARTESIAN_POINT('Ctrl Pts',(5.91127285614981,0.680609080090536,
4.50231102005075));
#163312=CARTESIAN_POINT('Ctrl Pts',(6.111724124,0.810731746,3.899913875));
#163313=CARTESIAN_POINT('Ctrl Pts',(6.32583734,0.745065281,3.564367771));
#163314=CARTESIAN_POINT('Ctrl Pts',(6.501930055,0.680609079,3.207398566));
#163315=CARTESIAN_POINT('Ctrl Pts',(6.186762652,0.810731746,4.239571663));
#163316=CARTESIAN_POINT('Ctrl Pts',(6.419523772,0.745065281,3.899905791));
#163317=CARTESIAN_POINT('Ctrl Pts',(6.61370130300001,0.680609079,3.536800117));
#163318=CARTESIAN_POINT('Ctrl Pts',(6.19241033773507,0.810731746,4.26513560322141));
#163319=CARTESIAN_POINT('Ctrl Pts',(6.42657497009355,0.745065281,3.92515966177328));
#163320=CARTESIAN_POINT('Ctrl Pts',(6.62211363330213,0.680609079,3.56159213371832));
#163321=CARTESIAN_POINT('',(6.5427223617568,0.680609081791281,3.32761771924868));
#163322=CARTESIAN_POINT('Ctrl Pts',(6.501930055,0.680609079,3.207398566));
#163323=CARTESIAN_POINT('Ctrl Pts',(6.675733702,0.745496505000001,2.855069682));
#163324=CARTESIAN_POINT('Ctrl Pts',(6.81044718200001,0.810723991,2.486022764));
#163325=CARTESIAN_POINT('Ctrl Pts',(6.831331606,0.680609079,3.095627318));
#163326=CARTESIAN_POINT('Ctrl Pts',(6.999078553,0.745496505000001,2.725448706));
#163327=CARTESIAN_POINT('Ctrl Pts',(7.12584196800001,0.810723991,2.339311063));
#163328=CARTESIAN_POINT('Ctrl Pts',(6.85608173160809,0.680609079,3.08722920202582));
#163329=CARTESIAN_POINT('Ctrl Pts',(7.02337359852327,0.745496505000001,
2.71570942144684));
#163330=CARTESIAN_POINT('Ctrl Pts',(7.14953967235489,0.810723991,2.32828763880268));
#163331=CARTESIAN_POINT('',(6.74093436582087,0.680609080455689,3.12630056270069));
#163332=CARTESIAN_POINT('',(6.62214921468494,0.680609082082812,3.16660628438882));
#163333=CARTESIAN_POINT('',(7.06074993928123,0.767980175616009,2.58138432684563));
#163334=CARTESIAN_POINT('Ctrl Pts',(6.74093436550991,0.680609079128079,
3.12630055604194));
#163335=CARTESIAN_POINT('Ctrl Pts',(6.79786894095172,0.695136944786355,
3.03806804583507));
#163336=CARTESIAN_POINT('Ctrl Pts',(6.85294329871174,0.709660812346982,
2.94864779267141));
#163337=CARTESIAN_POINT('Ctrl Pts',(6.95963781737309,0.738780776736229,
2.76698946628084));
#163338=CARTESIAN_POINT('Ctrl Pts',(7.01122294842257,0.753373671662706,
2.6747565480841));
#163339=CARTESIAN_POINT('Ctrl Pts',(7.0608490127954,0.767949007789042,2.58146634729615));
#163340=CARTESIAN_POINT('Ctrl Pts',(6.80883909838719,0.809946052553749,
2.49042368966192));
#163341=CARTESIAN_POINT('Ctrl Pts',(6.84874098462263,0.80292293123736,2.50487248776642));
#163342=CARTESIAN_POINT('Ctrl Pts',(6.88870368917698,0.796078752408176,
2.51932086611966));
#163343=CARTESIAN_POINT('Ctrl Pts',(6.97261152107854,0.782074139968656,
2.54961454392142));
#163344=CARTESIAN_POINT('Ctrl Pts',(7.01661924109567,0.774939590214728,
2.56547817894248));
#163345=CARTESIAN_POINT('Ctrl Pts',(7.06062924972398,0.767997185218944,
2.58132019820442));
#163346=CARTESIAN_POINT('Origin',(1.26504709485609E-12,0.560925699999955,
4.67941657644744E-13));
#163347=CARTESIAN_POINT('',(7.16999527408755,0.680609080192563,1.95067144819131));
#163348=CARTESIAN_POINT('',(6.86938430225266,0.562053379538648,2.5055306689776));
#163349=CARTESIAN_POINT('Ctrl Pts',(7.1699952722679,0.68060907998119,1.95067144725986));
#163350=CARTESIAN_POINT('Ctrl Pts',(7.14902436655433,0.671661524774049,
1.99366972355771));
#163351=CARTESIAN_POINT('Ctrl Pts',(7.125377258842,0.661738573439555,2.04109270155846));
#163352=CARTESIAN_POINT('Ctrl Pts',(7.07506755250471,0.641119488180572,
2.13885931550801));
#163353=CARTESIAN_POINT('Ctrl Pts',(7.05058003388874,0.631275792568541,
2.1852243666409));
#163354=CARTESIAN_POINT('Ctrl Pts',(6.97547888030251,0.60165447159557,2.32383242984726));
#163355=CARTESIAN_POINT('Ctrl Pts',(6.92339597490006,0.581858135006135,
2.4152450022131));
#163356=CARTESIAN_POINT('Ctrl Pts',(6.86938430282194,0.562053380243108,
2.50553066947269));
#163357=CARTESIAN_POINT('Ctrl Pts',(7.06087062883848,0.767963166013075,
2.58144845548684));
#163358=CARTESIAN_POINT('Ctrl Pts',(7.08353774714955,0.75333360255102,2.47684279946778));
#163359=CARTESIAN_POINT('Ctrl Pts',(7.10399783748468,0.738713518238969,
2.37176907944768));
#163360=CARTESIAN_POINT('Ctrl Pts',(7.14036182541816,0.709588701622422,
2.16143700787481));
#163361=CARTESIAN_POINT('Ctrl Pts',(7.1562876362193,0.695086898948571,2.05620572292349));
#163362=CARTESIAN_POINT('Ctrl Pts',(7.16999527007506,0.680609078987201,
1.95067145153359));
#163363=CARTESIAN_POINT('Ctrl Pts',(6.86938430192758,0.562053379235629,
2.50553066898454));
#163364=CARTESIAN_POINT('Ctrl Pts',(6.85280901821899,0.582224589991481,
2.60984189004187));
#163365=CARTESIAN_POINT('Ctrl Pts',(6.83381055446812,0.602198953194961,
2.71378771864018));
#163366=CARTESIAN_POINT('Ctrl Pts',(6.8017278394544,0.631811121640532,2.86885152610303));
#163367=CARTESIAN_POINT('Ctrl Pts',(6.79046181068709,0.641604433126681,
2.920295178957));
#163368=CARTESIAN_POINT('Ctrl Pts',(6.76572262811083,0.661914332930743,
3.02731365616675));
#163369=CARTESIAN_POINT('Ctrl Pts',(6.75311089226061,0.671620871200531,
3.07868228515498));
#163370=CARTESIAN_POINT('Ctrl Pts',(6.74093436379984,0.680609080182541,
3.12630056223545));
#163371=CARTESIAN_POINT('Ctrl Pts',(6.807201613,0.810731746,2.49489603));
#163372=CARTESIAN_POINT('Ctrl Pts',(6.94417648700001,0.745065281,2.121166795));
#163373=CARTESIAN_POINT('Ctrl Pts',(7.039414425,0.680609079,1.734688604));
#163374=CARTESIAN_POINT('Ctrl Pts',(6.953502166,0.810731746,2.810481743));
#163375=CARTESIAN_POINT('Ctrl Pts',(7.107803339,0.745065281,2.428720309));
#163376=CARTESIAN_POINT('Ctrl Pts',(7.21938412,0.680609079,2.032361415));
#163377=CARTESIAN_POINT('Ctrl Pts',(6.96451330330129,0.810731746,2.83423392674035));
#163378=CARTESIAN_POINT('Ctrl Pts',(7.12011851961009,0.745065281,2.4518679588257));
#163379=CARTESIAN_POINT('Ctrl Pts',(7.23292932527149,0.680609079,2.0547654054537));
#163380=CARTESIAN_POINT('',(7.10509659429687,0.680609081791282,1.84332795993776));
#163381=CARTESIAN_POINT('Ctrl Pts',(7.039414425,0.680609079,1.734688604));
#163382=CARTESIAN_POINT('Ctrl Pts',(7.133414344,0.745496505000001,1.353234327));
#163383=CARTESIAN_POINT('Ctrl Pts',(7.185644119,0.810723991,0.963856104));
#163384=CARTESIAN_POINT('Ctrl Pts',(7.337087236,0.680609079,1.554718909));
#163385=CARTESIAN_POINT('Ctrl Pts',(7.421334894,0.745496505000001,1.157134232));
#163386=CARTESIAN_POINT('Ctrl Pts',(7.462126472,0.810723991,0.752773886));
#163387=CARTESIAN_POINT('Ctrl Pts',(7.35945337054856,0.680609079,1.54119659099081));
#163388=CARTESIAN_POINT('Ctrl Pts',(7.44296827643409,0.745496505000001,
1.14239992994863));
#163389=CARTESIAN_POINT('Ctrl Pts',(7.48290042675498,0.810723991,0.736913877580905));
#163390=CARTESIAN_POINT('',(7.2553972746655,0.680609080401357,1.60410776492566));
#163391=CARTESIAN_POINT('',(7.14805379311743,0.680609082082812,1.66900645776976));
#163392=CARTESIAN_POINT('',(7.45059485449452,0.767980175618517,1.00318047335778));
#163393=CARTESIAN_POINT('Ctrl Pts',(7.25539727289291,0.68060907913724,1.60410775805583));
#163394=CARTESIAN_POINT('Ctrl Pts',(7.29203336852415,0.695136944988277,
1.50569882284163));
#163395=CARTESIAN_POINT('Ctrl Pts',(7.3265974075645,0.709660812732467,1.40652980529827));
#163396=CARTESIAN_POINT('Ctrl Pts',(7.39174629634048,0.738780776713929,
1.20618238492266));
#163397=CARTESIAN_POINT('Ctrl Pts',(7.42229804465085,0.753373671641964,
1.10501654288154));
#163398=CARTESIAN_POINT('Ctrl Pts',(7.45070924368572,0.767949007780856,
1.00323927836238));
#163399=CARTESIAN_POINT('Ctrl Pts',(7.18501969994167,0.809946052636564,
0.968499828836897));
#163400=CARTESIAN_POINT('Ctrl Pts',(7.22709476677672,0.802922931348075,
0.974033096202646));
#163401=CARTESIAN_POINT('Ctrl Pts',(7.26922914024265,0.796078752458098,
0.979552879520431));
#163402=CARTESIAN_POINT('Ctrl Pts',(7.35768749908181,0.782074140010044,
0.991100604673837));
#163403=CARTESIAN_POINT('Ctrl Pts',(7.40407655575484,0.774939590240218,
0.997132997879333));
#163404=CARTESIAN_POINT('Ctrl Pts',(7.45046320082775,0.767997185218328,
1.00314378867028));
#163405=CARTESIAN_POINT('Origin',(-1.05861500121485E-12,0.560925700000134,
-1.37422625362538E-14));
#163406=CARTESIAN_POINT('',(7.42170146886965,0.680609080233179,0.363728792693982));
#163407=CARTESIAN_POINT('',(7.24739694553545,0.562053379620976,0.970238187390015));
#163408=CARTESIAN_POINT('Ctrl Pts',(7.42170146700829,0.680609079992507,
0.363728792197865));
#163409=CARTESIAN_POINT('Ctrl Pts',(7.41046420776432,0.671661524759858,
0.410229917826462));
#163410=CARTESIAN_POINT('Ctrl Pts',(7.39756449471215,0.661738573404569,
0.461627602379835));
#163411=CARTESIAN_POINT('Ctrl Pts',(7.36944793333281,0.641119488121199,
0.567923587341595));
#163412=CARTESIAN_POINT('Ctrl Pts',(7.35550003476589,0.631275792530468,
0.618468741997286));
#163413=CARTESIAN_POINT('Ctrl Pts',(7.31195134080634,0.601654471595934,
0.769980753821589));
#163414=CARTESIAN_POINT('Ctrl Pts',(7.28073710570731,0.581858135014435,
0.870452436201094));
#163415=CARTESIAN_POINT('Ctrl Pts',(7.24739694613023,0.562053380253525,
0.970238187714283));
#163416=CARTESIAN_POINT('Ctrl Pts',(7.45072650816129,0.767963166018706,
1.00321715804528));
#163417=CARTESIAN_POINT('Ctrl Pts',(7.45037655791925,0.753333602551921,
0.896184363727295));
#163418=CARTESIAN_POINT('Ctrl Pts',(7.4477705588714,0.73871351824202,0.78916889425916));
#163419=CARTESIAN_POINT('Ctrl Pts',(7.43806919902117,0.709588701781099,
0.575937088238746));
#163420=CARTESIAN_POINT('Ctrl Pts',(7.43100105757009,0.695086899033531,
0.469742473131814));
#163421=CARTESIAN_POINT('Ctrl Pts',(7.42170146573539,0.680609078990994,
0.363728797710933));
#163422=CARTESIAN_POINT('Ctrl Pts',(7.24739694525172,0.562053379348888,
0.970238187458852));
#163423=CARTESIAN_POINT('Ctrl Pts',(7.25363301157249,0.58222459010264,1.07567386611614));
#163424=CARTESIAN_POINT('Ctrl Pts',(7.25742400185949,0.602198953284748,
1.18127360706405));
#163425=CARTESIAN_POINT('Ctrl Pts',(7.25942549781448,0.631811121645755,
1.33960894389367));
#163426=CARTESIAN_POINT('Ctrl Pts',(7.25948172723322,0.641604433069193,
1.39227173559095));
#163427=CARTESIAN_POINT('Ctrl Pts',(7.25832674329939,0.661914312715681,
1.50210626427859));
#163428=CARTESIAN_POINT('Ctrl Pts',(7.25705260194503,0.671620857839493,
1.5549851053256));
#163429=CARTESIAN_POINT('Ctrl Pts',(7.25539727228099,0.680609080020491,
1.60410776491499));
#163430=CARTESIAN_POINT('Ctrl Pts',(7.18438192,0.810731746,0.97321962));
#163431=CARTESIAN_POINT('Ctrl Pts',(7.23781366,0.745065281,0.578782418));
#163432=CARTESIAN_POINT('Ctrl Pts',(7.2477436,0.680609079,0.180866531));
#163433=CARTESIAN_POINT('Ctrl Pts',(7.39510364700001,0.810731746,1.24997682));
#163434=CARTESIAN_POINT('Ctrl Pts',(7.463729921,0.745065281,0.843970566000001));
#163435=CARTESIAN_POINT('Ctrl Pts',(7.48749656,0.680609079,0.432891753));
#163436=CARTESIAN_POINT('Ctrl Pts',(7.41096336723259,0.810731746,1.27080662159114));
#163437=CARTESIAN_POINT('Ctrl Pts',(7.48073323976765,0.745065281,0.863929636648076));
#163438=CARTESIAN_POINT('Ctrl Pts',(7.50554128146593,0.680609079,0.451860131673525));
#163439=CARTESIAN_POINT('',(7.33524440713602,0.680609081791281,0.272846233901281));
#163440=CARTESIAN_POINT('Ctrl Pts',(7.2477436,0.680609079,0.180866531));
#163441=CARTESIAN_POINT('Ctrl Pts',(7.25754446000001,0.745496505000001,
-0.211876761));
#163442=CARTESIAN_POINT('Ctrl Pts',(7.22484832400001,0.810723991,-0.603379396));
#163443=CARTESIAN_POINT('Ctrl Pts',(7.499768822,0.680609079,-0.058886428));
#163444=CARTESIAN_POINT('Ctrl Pts',(7.496577864,0.745496505000001,-0.465286552));
#163445=CARTESIAN_POINT('Ctrl Pts',(7.449490235,0.810723991,-0.868962162));
#163446=CARTESIAN_POINT('Ctrl Pts',(7.51870515021548,0.680609079,-0.076900659616291));
#163447=CARTESIAN_POINT('Ctrl Pts',(7.51453803067176,0.745496505000001,
-0.4843269120771));
#163448=CARTESIAN_POINT('Ctrl Pts',(7.46636907325234,0.810723991,-0.888917158509634));
#163449=CARTESIAN_POINT('',(7.43060587058891,0.680609080425494,0.00690867068859535));
#163450=CARTESIAN_POINT('',(7.33880352304754,0.680609082082812,0.0942407518356454));
#163451=CARTESIAN_POINT('',(7.49205823513684,0.767980175622892,-0.621930984430037));
#163452=CARTESIAN_POINT('Ctrl Pts',(7.43060586743964,0.680609079131675,
0.00690866453753127));
#163453=CARTESIAN_POINT('Ctrl Pts',(7.44523041930225,0.695136944893849,
-0.0970752012570951));
#163454=CARTESIAN_POINT('Ctrl Pts',(7.45766796293523,0.709660812543815,
-0.201355948185125));
#163455=CARTESIAN_POINT('Ctrl Pts',(7.47822493391373,0.738780776767852,
-0.411024444247337));
#163456=CARTESIAN_POINT('Ctrl Pts',(7.48631473371831,0.753373671689276,
-0.516392807950393));
#163457=CARTESIAN_POINT('Ctrl Pts',(7.49218259132217,0.767949007805525,
-0.621898144596978));
#163458=CARTESIAN_POINT('Ctrl Pts',(7.22523676700086,0.80994605257742,-0.598710006733521));
#163459=CARTESIAN_POINT('Ctrl Pts',(7.26751763093187,0.802922931299024,
-0.602350999705705));
#163460=CARTESIAN_POINT('Ctrl Pts',(7.3098535164192,0.79607875240577,-0.606017910679099));
#163461=CARTESIAN_POINT('Ctrl Pts',(7.39872618738651,0.782074139992209,
-0.613756097291337));
#163462=CARTESIAN_POINT('Ctrl Pts',(7.44532747993427,0.774939590232648,
-0.617837014054864));
#163463=CARTESIAN_POINT('Ctrl Pts',(7.49192177335025,0.767997185228654,
-0.621938509756826));
#163464=CARTESIAN_POINT('Origin',(9.68409380464053E-13,0.560925700000022,
-7.01377161644451E-14));
#163465=CARTESIAN_POINT('',(7.32637715136353,0.680609080273142,-1.24022141673702));
#163466=CARTESIAN_POINT('',(7.28652936266848,0.562053379784689,-0.610421555804528));
#163467=CARTESIAN_POINT('Ctrl Pts',(7.32637714962487,0.680609080098861,
-1.24022141680518));
#163468=CARTESIAN_POINT('Ctrl Pts',(7.32539897868996,0.671661524913783,
-1.19239178347266));
#163469=CARTESIAN_POINT('Ctrl Pts',(7.32384983662865,0.661738573559669,
-1.13942269132726));
#163470=CARTESIAN_POINT('Ctrl Pts',(7.31924111951911,0.641119488285343,
-1.02956761794737));
#163471=CARTESIAN_POINT('Ctrl Pts',(7.31648502923072,0.631275792705557,
-0.977205795057172));
#163472=CARTESIAN_POINT('Ctrl Pts',(7.30652508348097,0.601654471841923,
-0.819874368190679));
#163473=CARTESIAN_POINT('Ctrl Pts',(7.29763906171505,0.581858135332135,
-0.715041520235852));
#163474=CARTESIAN_POINT('Ctrl Pts',(7.2865293635274,0.562053380619792,-0.610421555555234));
#163475=CARTESIAN_POINT('Ctrl Pts',(7.49219469692343,0.76796316601713,-0.621923459103248));
#163476=CARTESIAN_POINT('Ctrl Pts',(7.46884404140746,0.753333602554716,
-0.726378657295504));
#163477=CARTESIAN_POINT('Ctrl Pts',(7.44329380657706,0.73871351824609,-0.830331951877381));
#163478=CARTESIAN_POINT('Ctrl Pts',(7.38798072444135,0.709588702079347,
-1.03649300931035));
#163479=CARTESIAN_POINT('Ctrl Pts',(7.35824912877455,0.695086899177824,
-1.13868541307905));
#163480=CARTESIAN_POINT('Ctrl Pts',(7.32637714941249,0.680609078999391,
-1.24022141147247));
#163481=CARTESIAN_POINT('Ctrl Pts',(7.28652936194102,0.562053379030082,
-0.610421555448924));
#163482=CARTESIAN_POINT('Ctrl Pts',(7.31528607861313,0.582225215395378,
-0.508788322522507));
#163483=CARTESIAN_POINT('Ctrl Pts',(7.34168762411948,0.60219834043125,-0.406478737699217));
#163484=CARTESIAN_POINT('Ctrl Pts',(7.37768078505445,0.63181136590102,-0.252270992317658));
#163485=CARTESIAN_POINT('Ctrl Pts',(7.38905691094103,0.641604918991269,
-0.200850235723201));
#163486=CARTESIAN_POINT('Ctrl Pts',(7.41154005366641,0.661914800536601,
-0.0933352359651138));
#163487=CARTESIAN_POINT('Ctrl Pts',(7.42166281552644,0.671621097024362,
-0.0414200839496619));
#163488=CARTESIAN_POINT('Ctrl Pts',(7.4306058683949,0.68060908009308,0.00690867115641031));
#163489=CARTESIAN_POINT('Ctrl Pts',(7.22562851299999,0.810731746,-0.593963458000001));
#163490=CARTESIAN_POINT('Ctrl Pts',(7.193018709,0.745065281,-0.990665182));
#163491=CARTESIAN_POINT('Ctrl Pts',(7.11717634,0.680609079,-1.381412661));
#163492=CARTESIAN_POINT('Ctrl Pts',(7.4909183,0.810731746,-0.36897563));
#163493=CARTESIAN_POINT('Ctrl Pts',(7.470660787,0.745065281,-0.780242304));
#163494=CARTESIAN_POINT('Ctrl Pts',(7.405501982,0.680609079,-1.186819448));
#163495=CARTESIAN_POINT('Ctrl Pts',(7.51088502066177,0.810731746,-0.352042188404765));
#163496=CARTESIAN_POINT('Ctrl Pts',(7.49155718816973,0.745065281,-0.764405076063766));
#163497=CARTESIAN_POINT('Ctrl Pts',(7.4272024689224,0.680609079,-1.1721736209948));
#163498=CARTESIAN_POINT('',(7.22240434444543,0.680609081791281,-1.31039347883568));
#163499=CARTESIAN_POINT('Ctrl Pts',(7.11717634000001,0.680609079,-1.381412661));
#163500=CARTESIAN_POINT('Ctrl Pts',(7.04231986300001,0.745496505000001,
-1.767080728));
#163501=CARTESIAN_POINT('Ctrl Pts',(6.926226651,0.810723991,-2.142401545));
#163502=CARTESIAN_POINT('Ctrl Pts',(7.311769554,0.680609079,-1.669738302));
#163503=CARTESIAN_POINT('Ctrl Pts',(7.221289184,0.745496505000001,-2.065951054));
#163504=CARTESIAN_POINT('Ctrl Pts',(7.088524115,0.810723991,-2.450066505));
#163505=CARTESIAN_POINT('Ctrl Pts',(7.32639063412096,0.680609079,-1.69140212167456));
#163506=CARTESIAN_POINT('Ctrl Pts',(7.23473633730893,0.745496505000001,
-2.08840716586741));
#163507=CARTESIAN_POINT('Ctrl Pts',(7.10071860100388,0.810723991,-2.47318341610961));
#163508=CARTESIAN_POINT('',(7.25836759458169,0.680609080422382,-1.59061346520233));
#163509=CARTESIAN_POINT('',(7.18819554290371,0.680609082082812,-1.48664064912483));
#163510=CARTESIAN_POINT('',(7.18320129951193,0.76798017563633,-2.21796164054473));
#163511=CARTESIAN_POINT('Ctrl Pts',(7.25836759016924,0.68060907912728,-1.5906134705797));
#163512=CARTESIAN_POINT('Ctrl Pts',(7.25029677077617,0.695136944811777,
-1.69531009716092));
#163513=CARTESIAN_POINT('Ctrl Pts',(7.2400262535728,0.709660812377614,-1.79982652179942));
#163514=CARTESIAN_POINT('Ctrl Pts',(7.21503008497306,0.73878077675353,-2.00901222711682));
#163515=CARTESIAN_POINT('Ctrl Pts',(7.20027966622202,0.753373671680877,
-2.11365620488811));
#163516=CARTESIAN_POINT('Ctrl Pts',(7.18332980791151,0.767949007807122,
-2.21795630136356));
#163517=CARTESIAN_POINT('Ctrl Pts',(6.92760979322194,0.809946052627665,
-2.13792482796008));
#163518=CARTESIAN_POINT('Ctrl Pts',(6.96811944822111,0.802922931326775,
-2.1505698326309));
#163519=CARTESIAN_POINT('Ctrl Pts',(7.00867726647099,0.796078752464882,
-2.16325197719105));
#163520=CARTESIAN_POINT('Ctrl Pts',(7.09380866237873,0.782074140016891,
-2.1899142465429));
#163521=CARTESIAN_POINT('Ctrl Pts',(7.1384431660475,0.774939590251537,-2.20391765404315));
#163522=CARTESIAN_POINT('Ctrl Pts',(7.18306641038926,0.767997185238686,
-2.21793965470795));
#163523=CARTESIAN_POINT('Origin',(7.68482499857726E-13,0.560925699999978,
-3.48679418671338E-13));
#163524=CARTESIAN_POINT('',(6.88847958174721,0.680609080136121,-2.78618024951889));
#163525=CARTESIAN_POINT('',(6.98495176503208,0.562053379593368,-2.16253866235914));
#163526=CARTESIAN_POINT('Ctrl Pts',(6.88847957946011,0.680609079829239,
-2.7861802491228));
#163527=CARTESIAN_POINT('Ctrl Pts',(6.89780623497149,0.671661524659695,
-2.73925856817232));
#163528=CARTESIAN_POINT('Ctrl Pts',(6.90768010001637,0.661738573367639,
-2.6871948444348));
#163529=CARTESIAN_POINT('Ctrl Pts',(6.92679472560154,0.641119488158189,
-2.57891738392072));
#163530=CARTESIAN_POINT('Ctrl Pts',(6.93535931529209,0.631275792572596,
-2.5271872733699));
#163531=CARTESIAN_POINT('Ctrl Pts',(6.95945383363896,0.601654471656685,
-2.3713930736837));
#163532=CARTESIAN_POINT('Ctrl Pts',(6.97331152558087,0.581858135084815,
-2.26710092725075));
#163533=CARTESIAN_POINT('Ctrl Pts',(6.98495176580074,0.562053380312653,
-2.16253866230847));
#163534=CARTESIAN_POINT('Ctrl Pts',(7.18333618863459,0.767963166033974,
-2.21798362638151));
#163535=CARTESIAN_POINT('Ctrl Pts',(7.13807667852258,0.753333602535863,
-2.31497701929691));
#163536=CARTESIAN_POINT('Ctrl Pts',(7.09077690848965,0.738713518201341,
-2.41100739830454));
#163537=CARTESIAN_POINT('Ctrl Pts',(6.9924384802054,0.709588701397635,-2.60045785090637));
#163538=CARTESIAN_POINT('Ctrl Pts',(6.94143364784321,0.695086898839987,
-2.69386963643605));
#163539=CARTESIAN_POINT('Ctrl Pts',(6.88847958060598,0.680609078980756,
-2.78618024402691));
#163540=CARTESIAN_POINT('Ctrl Pts',(6.98495176477214,0.562053379283973,
-2.16253866215263));
#163541=CARTESIAN_POINT('Ctrl Pts',(7.0348827576773,0.582224590025707,-2.06946628806565));
#163542=CARTESIAN_POINT('Ctrl Pts',(7.08266354766498,0.602198953223101,
-1.97521835430801));
#163543=CARTESIAN_POINT('Ctrl Pts',(7.15096333852608,0.631811121595153,
-1.83235750092));
#163544=CARTESIAN_POINT('Ctrl Pts',(7.17312690322427,0.641604433008838,
-1.78458565585862));
#163545=CARTESIAN_POINT('Ctrl Pts',(7.21819699626072,0.661914315589568,
-1.68441755785409));
#163546=CARTESIAN_POINT('Ctrl Pts',(7.23924386442132,0.67162086007449,-1.63589102589247));
#163547=CARTESIAN_POINT('Ctrl Pts',(7.25836759253305,0.680609080085683,
-1.59061346427022));
#163548=CARTESIAN_POINT('Ctrl Pts',(6.929012748,0.810731746,-2.133373465));
#163549=CARTESIAN_POINT('Ctrl Pts',(6.811886199,0.745065281,-2.513790379));
#163550=CARTESIAN_POINT('Ctrl Pts',(6.653817825,0.680609079,-2.879098531));
#163551=CARTESIAN_POINT('Ctrl Pts',(7.23646594,0.810731746,-1.97067519));
#163552=CARTESIAN_POINT('Ctrl Pts',(7.128271858,0.745065281,-2.36797191));
#163553=CARTESIAN_POINT('Ctrl Pts',(6.977234361,0.680609079,-2.751036289));
#163554=CARTESIAN_POINT('Ctrl Pts',(7.2596060389333,0.810731746,-1.95842989778076));
#163555=CARTESIAN_POINT('Ctrl Pts',(7.15208424844132,0.745065281,-2.35699705630923));
#163556=CARTESIAN_POINT('Ctrl Pts',(7.00157592203899,0.680609079,-2.74139783662219));
#163557=CARTESIAN_POINT('',(6.77185268139767,0.680609081791281,-2.83236064878544));
#163558=CARTESIAN_POINT('Ctrl Pts',(6.653817825,0.680609079,-2.879098531));
#163559=CARTESIAN_POINT('Ctrl Pts',(6.497804216,0.745496505000001,-3.239657963));
#163560=CARTESIAN_POINT('Ctrl Pts',(6.303742317,0.810723991,-3.58124738));
#163561=CARTESIAN_POINT('Ctrl Pts',(6.781880067,0.680609079,-3.202515068));
#163562=CARTESIAN_POINT('Ctrl Pts',(6.60834104800001,0.745496505000001,
-3.570013982));
#163563=CARTESIAN_POINT('Ctrl Pts',(6.39610648500001,0.810723991,-3.916608461));
#163564=CARTESIAN_POINT('Ctrl Pts',(6.79150223349964,0.680609079,-3.22681549972093));
#163565=CARTESIAN_POINT('Ctrl Pts',(6.6166464140879,0.745496505000001,-3.59483582307768));
#163566=CARTESIAN_POINT('Ctrl Pts',(6.40304641818575,0.810723991,-3.94180636561641));
#163567=CARTESIAN_POINT('',(6.74673611715292,0.680609080387324,-3.11376028311889));
#163568=CARTESIAN_POINT('',(6.70055573137004,0.680609082082812,-2.9971333764053));
#163569=CARTESIAN_POINT('',(6.53846585449635,0.767980175610573,-3.71028287566516));
#163570=CARTESIAN_POINT('Ctrl Pts',(6.74673611150703,0.680609079138449,
-3.11376028760432));
#163571=CARTESIAN_POINT('Ctrl Pts',(6.71634730295497,0.695136945031465,
-3.21427417927895));
#163572=CARTESIAN_POINT('Ctrl Pts',(6.68384896227507,0.709660812809216,
-3.31413921196611));
#163573=CARTESIAN_POINT('Ctrl Pts',(6.61446844803407,0.738780776729096,
-3.51306083143574));
#163574=CARTESIAN_POINT('Ctrl Pts',(6.57756752389879,0.753373671653006,
-3.61208738714968));
#163575=CARTESIAN_POINT('Ctrl Pts',(6.53859250620473,0.767949007785863,
-3.71030528682909));
#163576=CARTESIAN_POINT('Ctrl Pts',(6.30605548416853,0.809946052542317,
-3.57717266017008));
#163577=CARTESIAN_POINT('Ctrl Pts',(6.3428997437586,0.802922931278537,-3.59823041009158));
#163578=CARTESIAN_POINT('Ctrl Pts',(6.37978305667582,0.796078752422255,
-3.61933478530699));
#163579=CARTESIAN_POINT('Ctrl Pts',(6.4571925281524,0.78207413999555,-3.66367443941286));
#163580=CARTESIAN_POINT('Ctrl Pts',(6.49777318326057,0.774939590234295,
-3.68694555399608));
#163581=CARTESIAN_POINT('Ctrl Pts',(6.53833884531886,0.767997185214201,
-3.71023240666292));
#163582=CARTESIAN_POINT('Origin',(1.00700697780454E-12,0.560925699999933,
-5.77012396196785E-13));
#163583=CARTESIAN_POINT('',(6.12848436165721,0.680609080255617,-4.2018603922199));
#163584=CARTESIAN_POINT('',(6.3567655862665,0.562053379588068,-3.61353786574919));
#163585=CARTESIAN_POINT('Ctrl Pts',(6.12848435999572,0.680609080058053,
-4.20186039153242));
#163586=CARTESIAN_POINT('Ctrl Pts',(6.14767973809234,0.671661524805192,
-4.15804066821971));
#163587=CARTESIAN_POINT('Ctrl Pts',(6.16851491939803,0.661738573445309,
-4.10931675421297));
#163588=CARTESIAN_POINT('Ctrl Pts',(6.21045910905953,0.641119488185435,
-4.00767983985874));
#163589=CARTESIAN_POINT('Ctrl Pts',(6.22994390802001,0.631275792590329,
-3.95900028417221));
#163590=CARTESIAN_POINT('Ctrl Pts',(6.2869662575588,0.601654471628634,-3.81202807549649));
#163591=CARTESIAN_POINT('Ctrl Pts',(6.32291969295443,0.581858135013998,
-3.71315321560427));
#163592=CARTESIAN_POINT('Ctrl Pts',(6.35676558692114,0.562053380206358,
-3.6135378658487));
#163593=CARTESIAN_POINT('Ctrl Pts',(6.53859286367383,0.767963166006944,
-3.71033334466741));
#163594=CARTESIAN_POINT('Ctrl Pts',(6.47354078340064,0.753333602518642,
-3.79532962912656));
#163595=CARTESIAN_POINT('Ctrl Pts',(6.40670316287955,0.738713518200544,
-3.87894681883908));
#163596=CARTESIAN_POINT('Ctrl Pts',(6.26993758578123,0.709588701540351,
-4.04282816925933));
#163597=CARTESIAN_POINT('Ctrl Pts',(6.20004444501731,0.695086898908745,
-4.12309150837784));
#163598=CARTESIAN_POINT('Ctrl Pts',(6.12848436216369,0.680609078985776,
-4.20186038647418));
#163599=CARTESIAN_POINT('Ctrl Pts',(6.35676558608643,0.562053379322113,
-3.6135378655278));
#163600=CARTESIAN_POINT('Ctrl Pts',(6.42553702937026,0.582224590083683,
-3.53337515935516));
#163601=CARTESIAN_POINT('Ctrl Pts',(6.49246125085151,0.602198953290983,
-3.45160214738175));
#163602=CARTESIAN_POINT('Ctrl Pts',(6.58987509110844,0.631811121652785,
-3.32676373741278));
#163603=CARTESIAN_POINT('Ctrl Pts',(6.62179001855158,0.641604433060423,
-3.28487328276653));
#163604=CARTESIAN_POINT('Ctrl Pts',(6.68733942155397,0.661914267144304,
-3.19673600722322));
#163605=CARTESIAN_POINT('Ctrl Pts',(6.7183260480719,0.671620828781777,-3.15386839323973));
#163606=CARTESIAN_POINT('Ctrl Pts',(6.74673611518767,0.680609079979072,
-3.11376028163534));
#163607=CARTESIAN_POINT('Ctrl Pts',(6.308404047,0.810731746,-3.573029299));
#163608=CARTESIAN_POINT('Ctrl Pts',(6.112237461,0.745065281,-3.919373532));
#163609=CARTESIAN_POINT('Ctrl Pts',(5.879334183,0.680609079,-4.242160954));
#163610=CARTESIAN_POINT('Ctrl Pts',(6.643644474,0.810731746,-3.480228168));
#163611=CARTESIAN_POINT('Ctrl Pts',(6.452572859,0.745065281,-3.844977782));
#163612=CARTESIAN_POINT('Ctrl Pts',(6.222719017,0.680609079,-4.186617732));
#163613=CARTESIAN_POINT('Ctrl Pts',(6.66887594644061,0.810731746,-3.47324360113186));
#163614=CARTESIAN_POINT('Ctrl Pts',(6.47818779837961,0.745065281,-3.83937847426548));
#163615=CARTESIAN_POINT('Ctrl Pts',(6.24856346855714,0.680609079,-4.18243733738681));
#163616=CARTESIAN_POINT('',(6.00465671315862,0.680609081791282,-4.22188978249707));
#163617=CARTESIAN_POINT('Ctrl Pts',(5.879334183,0.680609079,-4.242160954));
#163618=CARTESIAN_POINT('Ctrl Pts',(5.649458466,0.745496505000001,-4.560752393));
#163619=CARTESIAN_POINT('Ctrl Pts',(5.386501999,0.810723991,-4.852638067));
#163620=CARTESIAN_POINT('Ctrl Pts',(5.934877406,0.680609079,-4.585545789));
#163621=CARTESIAN_POINT('Ctrl Pts',(5.68639423,0.745496505000001,-4.907147023));
#163622=CARTESIAN_POINT('Ctrl Pts',(5.404614025,0.810723991,-5.200014158));
#163623=CARTESIAN_POINT('Ctrl Pts',(5.93905073708842,0.680609079,-4.61134657134199));
#163624=CARTESIAN_POINT('Ctrl Pts',(5.68916945916119,0.745496505000001,
-4.93317395122199));
#163625=CARTESIAN_POINT('Ctrl Pts',(5.40597490175684,0.810723991,-5.22611482990271));
#163626=CARTESIAN_POINT('',(5.91963475714295,0.680609080402124,-4.49131113113577));
#163627=CARTESIAN_POINT('',(5.89960538046839,0.680609082082812,-4.36748347900849));
#163628=CARTESIAN_POINT('',(5.58799901358701,0.767980175609575,-5.02911540651578));
#163629=CARTESIAN_POINT('Ctrl Pts',(5.91963475075909,0.680609079135094,
-4.49131113423801));
#163630=CARTESIAN_POINT('Ctrl Pts',(5.86834890042719,0.695136944971322,
-4.58294237093696));
#163631=CARTESIAN_POINT('Ctrl Pts',(5.81514232318593,0.709660812691301,
-4.6734864315971));
#163632=CARTESIAN_POINT('Ctrl Pts',(5.70462161828251,0.738780776758252,
-4.85284261521551));
#163633=CARTESIAN_POINT('Ctrl Pts',(5.64729563502227,0.753373671679497,
-4.94162137712873));
#163634=CARTESIAN_POINT('Ctrl Pts',(5.5881178864952,0.767949007801361,-5.02916452012994));
#163635=CARTESIAN_POINT('Ctrl Pts',(5.38963703028742,0.809946052468512,
-4.84915587539728));
#163636=CARTESIAN_POINT('Ctrl Pts',(5.42109309803381,0.802922931155035,
-4.87764173345527));
#163637=CARTESIAN_POINT('Ctrl Pts',(5.45257728230892,0.796078752405789,
-4.9061815214961));
#163638=CARTESIAN_POINT('Ctrl Pts',(5.51864524857705,0.782074139963076,
-4.96612528710073));
#163639=CARTESIAN_POINT('Ctrl Pts',(5.55327454877581,0.774939590215754,
-4.99757597712486));
#163640=CARTESIAN_POINT('Ctrl Pts',(5.58788582318887,0.76799718521808,-5.029038814209));
#163641=CARTESIAN_POINT('Origin',(-3.43475248243408E-13,0.560925700000089,
3.95950633391706E-13));
#163642=CARTESIAN_POINT('',(5.08192802476734,0.680609080255333,-5.42106621224534));
#163643=CARTESIAN_POINT('',(5.43134411396266,0.562053379559575,-4.89557205454599));
#163644=CARTESIAN_POINT('Ctrl Pts',(5.08192802331054,0.680609080058393,
-5.42106621122977));
#163645=CARTESIAN_POINT('Ctrl Pts',(5.1100945693517,0.671661524800105,-5.38239740756182));
#163646=CARTESIAN_POINT('Ctrl Pts',(5.14091683688863,0.661738573453892,
-5.33929157974953));
#163647=CARTESIAN_POINT('Ctrl Pts',(5.20372932683127,0.641119488223043,
-5.24904764102523));
#163648=CARTESIAN_POINT('Ctrl Pts',(5.23322324759152,0.631275792608505,
-5.20569484202607));
#163649=CARTESIAN_POINT('Ctrl Pts',(5.32050712680759,0.601654471599338,
-5.07441688130195));
#163650=CARTESIAN_POINT('Ctrl Pts',(5.37687516309367,0.58185813495123,-4.98558258638997));
#163651=CARTESIAN_POINT('Ctrl Pts',(5.43134411450069,0.562053380097903,
-4.89557205475313));
#163652=CARTESIAN_POINT('Ctrl Pts',(5.58811220398515,0.767963166001071,
-5.02919199882256));
#163653=CARTESIAN_POINT('Ctrl Pts',(5.50630931642712,0.753333602510161,
-5.09821684315267));
#163654=CARTESIAN_POINT('Ctrl Pts',(5.42305909815561,0.738713518179266,
-5.16551099681846));
#163655=CARTESIAN_POINT('Ctrl Pts',(5.25426137545546,0.709588701049038,
-5.29616033816167));
#163656=CARTESIAN_POINT('Ctrl Pts',(5.16874805351855,0.695086898663409,
-5.35952220462778));
#163657=CARTESIAN_POINT('Ctrl Pts',(5.08192802658712,0.680609078972075,
-5.42106620666916));
#163658=CARTESIAN_POINT('Ctrl Pts',(5.43134411385099,0.562053379328016,
-4.89557205432403));
#163659=CARTESIAN_POINT('Ctrl Pts',(5.51574033120653,0.582224590136018,
-4.83206733521017));
#163660=CARTESIAN_POINT('Ctrl Pts',(5.59867868192533,0.602198953374283,
-4.7665928602493));
#163661=CARTESIAN_POINT('Ctrl Pts',(5.72065160839433,0.631811121718146,
-4.66561419936138));
#163662=CARTESIAN_POINT('Ctrl Pts',(5.76082559180801,0.641604433083129,
-4.63156388649604));
#163663=CARTESIAN_POINT('Ctrl Pts',(5.84378956186459,0.661914308017457,
-4.55957825087984));
#163664=CARTESIAN_POINT('Ctrl Pts',(5.88326695168444,0.67162085454678,-4.52437410847237));
#163665=CARTESIAN_POINT('Ctrl Pts',(5.9196347555966,0.680609080023521,-4.49131112933193));
#163666=CARTESIAN_POINT('Ctrl Pts',(5.392821385,0.810731746,-4.845614255));
#163667=CARTESIAN_POINT('Ctrl Pts',(5.126787292,0.745065281,-5.141691134));
#163668=CARTESIAN_POINT('Ctrl Pts',(4.829939409,0.680609079,-5.406864646));
#163669=CARTESIAN_POINT('Ctrl Pts',(5.74017357700001,0.810731746,-4.827049544));
#163670=CARTESIAN_POINT('Ctrl Pts',(5.475158725,0.745065281,-5.142196766));
#163671=CARTESIAN_POINT('Ctrl Pts',(5.177236248,0.680609079,-5.426437582));
#163672=CARTESIAN_POINT('Ctrl Pts',(5.76631662721193,0.810731746,-4.82565229307423));
#163673=CARTESIAN_POINT('Ctrl Pts',(5.50137848717533,0.745065281,-5.14223482179199));
#163674=CARTESIAN_POINT('Ctrl Pts',(5.20337513213411,0.680609079,-5.42791071578303));
#163675=CARTESIAN_POINT('',(4.95668967087975,0.680609081791281,-5.41400804255423));
#163676=CARTESIAN_POINT('Ctrl Pts',(4.829939409,0.680609079,-5.40686464600001));
#163677=CARTESIAN_POINT('Ctrl Pts',(4.536950317,0.745496505000001,-5.66859111));
#163678=CARTESIAN_POINT('Ctrl Pts',(4.217394834,0.810723991,-5.89712479200001));
#163679=CARTESIAN_POINT('Ctrl Pts',(4.810366473,0.680609079,-5.754161485));
#163680=CARTESIAN_POINT('Ctrl Pts',(4.498557937,0.745496505000001,-6.014827323));
#163681=CARTESIAN_POINT('Ctrl Pts',(4.16040782,0.810723991,-6.240272973));
#163682=CARTESIAN_POINT('Ctrl Pts',(4.80889582836633,0.680609079,-5.78025620234674));
#163683=CARTESIAN_POINT('Ctrl Pts',(4.49567326258934,0.745496505000001,
-6.04084234847347));
#163684=CARTESIAN_POINT('Ctrl Pts',(4.15612600728023,0.810723991,-6.26605597412672));
#163685=CARTESIAN_POINT('',(4.81573785460079,0.680609080426409,-5.65885326274786));
#163686=CARTESIAN_POINT('',(4.82279603853048,0.680609082082812,-5.53361490783603));
#163687=CARTESIAN_POINT('',(4.37624354905032,0.76798017563068,-6.11279209097898));
#163688=CARTESIAN_POINT('Ctrl Pts',(4.81573784785622,0.680609079124368,
-5.65885326435406));
#163689=CARTESIAN_POINT('Ctrl Pts',(4.7459530260031,0.69513694474491,-5.73731727061858));
#163690=CARTESIAN_POINT('Ctrl Pts',(4.67452609357664,0.709660812247418,
-5.81430661899299));
#163691=CARTESIAN_POINT('Ctrl Pts',(4.52803302162047,0.738780776727708,
-5.96571087218322));
#163692=CARTESIAN_POINT('Ctrl Pts',(4.45296247846833,0.753373671660118,
-6.04009064412939));
#163693=CARTESIAN_POINT('Ctrl Pts',(4.37634908483691,0.767949007797225,
-6.11286561045525));
#163694=CARTESIAN_POINT('Ctrl Pts',(4.22120513800344,0.80994605254875,-5.89439795062712));
#163695=CARTESIAN_POINT('Ctrl Pts',(4.24580216291263,0.802922931255788,
-5.92897994973941));
#163696=CARTESIAN_POINT('Ctrl Pts',(4.27041505395194,0.796078752431283,
-5.96362066270131));
#163697=CARTESIAN_POINT('Ctrl Pts',(4.3220522501715,0.782074139997033,-6.03636563608711));
#163698=CARTESIAN_POINT('Ctrl Pts',(4.34911096790233,0.774939590239716,
-6.07452530240738));
#163699=CARTESIAN_POINT('Ctrl Pts',(4.37614947000743,0.767997185231775,
-6.11269295679182));
#163700=CARTESIAN_POINT('Origin',(5.86119694445664E-13,0.5609257,-8.27463098040937E-13));
#163701=CARTESIAN_POINT('',(3.7977463825975,0.68060908017408,-6.38678900099291));
#163702=CARTESIAN_POINT('',(4.25195902659592,0.562053379571023,-5.94869473597743));
#163703=CARTESIAN_POINT('Ctrl Pts',(3.79774638114675,0.680609079925947,
-6.3867889994241));
#163704=CARTESIAN_POINT('Ctrl Pts',(3.8335670582867,0.671661524756492,-6.35507922606506));
#163705=CARTESIAN_POINT('Ctrl Pts',(3.87293519691386,0.66173857344991,-6.3196070651455));
#163706=CARTESIAN_POINT('Ctrl Pts',(3.95367894493431,0.641119488224729,
-6.24497580820599));
#163707=CARTESIAN_POINT('Ctrl Pts',(3.99180288446093,0.631275792626585,
-6.2089768947307));
#163708=CARTESIAN_POINT('Ctrl Pts',(4.10526699590558,0.601654471696003,
-6.0995315939306));
#163709=CARTESIAN_POINT('Ctrl Pts',(4.17941392619882,0.581858135115378,
-6.02489165720565));
#163710=CARTESIAN_POINT('Ctrl Pts',(4.25195902726286,0.562053380317572,
-5.94869473641836));
#163711=CARTESIAN_POINT('Ctrl Pts',(4.3763376280932,0.767963166029586,-6.11289122516614));
#163712=CARTESIAN_POINT('Ctrl Pts',(4.28160894554066,0.753333602562223,
-6.16271710418354));
#163713=CARTESIAN_POINT('Ctrl Pts',(4.18583881739736,0.738713518245378,
-6.21054162179682));
#163714=CARTESIAN_POINT('Ctrl Pts',(3.99290174802687,0.709588701510303,
-6.30184993204269));
#163715=CARTESIAN_POINT('Ctrl Pts',(3.89576675037785,0.695086898897569,
-6.34534759749871));
#163716=CARTESIAN_POINT('Ctrl Pts',(3.79774638490242,0.680609078983362,
-6.38678899609424));
#163717=CARTESIAN_POINT('Ctrl Pts',(4.2519590265095,0.562053379244821,-5.94869473563823));
#163718=CARTESIAN_POINT('Ctrl Pts',(4.34803374463893,0.582224590082613,
-5.90481741360385));
#163719=CARTESIAN_POINT('Ctrl Pts',(4.44310811953507,0.602198953317149,
-5.85870298923816));
#163720=CARTESIAN_POINT('Ctrl Pts',(4.58393681431553,0.631811121707079,
-5.78630572681304));
#163721=CARTESIAN_POINT('Ctrl Pts',(4.63049136343402,0.641604433135485,
-5.76168771002945));
#163722=CARTESIAN_POINT('Ctrl Pts',(4.72699058372725,0.661914332869367,
-5.70921979554073));
#163723=CARTESIAN_POINT('Ctrl Pts',(4.77311282974381,0.671620871273028,
-5.68332519320183));
#163724=CARTESIAN_POINT('Ctrl Pts',(4.8157378535464,0.680609080098608,-5.65885326079093));
#163725=CARTESIAN_POINT('Ctrl Pts',(4.225076389,0.810731746,-5.891623674));
#163726=CARTESIAN_POINT('Ctrl Pts',(3.901614248,0.745065281,-6.123588974));
#163727=CARTESIAN_POINT('Ctrl Pts',(3.554702037,0.680609079,-6.318749356));
#163728=CARTESIAN_POINT('Ctrl Pts',(4.568298544,0.810731746,-5.948163449));
#163729=CARTESIAN_POINT('Ctrl Pts',(4.241732254,0.745065281,-6.198972345));
#163730=CARTESIAN_POINT('Ctrl Pts',(3.889671666,0.680609079,-6.412523242));
#163731=CARTESIAN_POINT('Ctrl Pts',(4.59413075144553,0.810731746,-5.95241884794627));
#163732=CARTESIAN_POINT('Ctrl Pts',(4.26733083136151,0.745065281,-6.20464598479641));
#163733=CARTESIAN_POINT('Ctrl Pts',(3.91488275688742,0.680609079,-6.41958102204373));
#163734=CARTESIAN_POINT('',(3.67695332919104,0.680609081791273,-6.35297330357109));
#163735=CARTESIAN_POINT('Ctrl Pts',(3.554702037,0.680609079,-6.318749356));
#163736=CARTESIAN_POINT('Ctrl Pts',(3.212299413,0.745496505000001,-6.511372807));
#163737=CARTESIAN_POINT('Ctrl Pts',(2.851086974,0.810723991,-6.665868515));
#163738=CARTESIAN_POINT('Ctrl Pts',(3.460928151,0.680609079,-6.653718985));
#163739=CARTESIAN_POINT('Ctrl Pts',(3.100374075,0.745496505000001,-6.841260983));
#163740=CARTESIAN_POINT('Ctrl Pts',(2.721665569,0.810723991,-6.988743559));
#163741=CARTESIAN_POINT('Ctrl Pts',(3.45388229633626,0.680609079,-6.67888747724637));
#163742=CARTESIAN_POINT('Ctrl Pts',(3.09196438123154,0.745496505000001,
-6.86604767194434));
#163743=CARTESIAN_POINT('Ctrl Pts',(2.71194127955328,0.810723991,-7.01300330477373));
#163744=CARTESIAN_POINT('',(3.48666240302753,0.680609080421826,-6.5617937045755));
#163745=CARTESIAN_POINT('',(3.52082035429993,0.680609082082812,-6.43977814068483));
#163746=CARTESIAN_POINT('',(2.95985979999369,0.767980175639301,-6.91064141109326));
#163747=CARTESIAN_POINT('Ctrl Pts',(3.48666239612088,0.680609079139956,
-6.56179370465681));
#163748=CARTESIAN_POINT('Ctrl Pts',(3.40164166089227,0.695136945044024,
-6.62342159344771));
#163749=CARTESIAN_POINT('Ctrl Pts',(3.3153342144121,0.709660812849234,-6.68325629570886));
#163750=CARTESIAN_POINT('Ctrl Pts',(3.13971863331975,0.73878077678132,-6.79962911927942));
#163751=CARTESIAN_POINT('Ctrl Pts',(3.05041374545117,0.753373671704107,
-6.85613198576015));
#163752=CARTESIAN_POINT('Ctrl Pts',(2.959947063858,0.767949007827794,-6.91073589883575));
#163753=CARTESIAN_POINT('Ctrl Pts',(2.85539438562627,0.809946052527927,
-6.66402452831394));
#163754=CARTESIAN_POINT('Ctrl Pts',(2.87198223802458,0.802922931249818,
-6.70308565289529));
#163755=CARTESIAN_POINT('Ctrl Pts',(2.88857296395146,0.796078752434789,
-6.74220752935955));
#163756=CARTESIAN_POINT('Ctrl Pts',(2.92336489219696,0.782074140012189,
-6.82435223668418));
#163757=CARTESIAN_POINT('Ctrl Pts',(2.94158779189988,0.774939590256684,
-6.86743657576036));
#163758=CARTESIAN_POINT('Ctrl Pts',(2.95978923143777,0.767997185246865,
-6.91052437038489));
#163759=CARTESIAN_POINT('Origin',(-1.68051336735253E-13,0.560925699999978,
5.18682319317065E-13));
#163760=CARTESIAN_POINT('',(2.3359863380162,0.680609080244164,-7.05387263538529));
#163761=CARTESIAN_POINT('',(2.87375705924332,0.562053379750906,-6.72366306359679));
#163762=CARTESIAN_POINT('Ctrl Pts',(2.33598633705615,0.680609080018014,
-7.05387263374758));
#163763=CARTESIAN_POINT('Ctrl Pts',(2.37778621086744,0.671661524820673,
-7.03060460389659));
#163764=CARTESIAN_POINT('Ctrl Pts',(2.42385941050709,0.661738573500913,
-7.0044247484152));
#163765=CARTESIAN_POINT('Ctrl Pts',(2.51875892880942,0.641119488297372,
-6.94889584785191));
#163766=CARTESIAN_POINT('Ctrl Pts',(2.56373025394769,0.631275792746461,
-6.92193408914264));
#163767=CARTESIAN_POINT('Ctrl Pts',(2.69806914162172,0.601654471945102,
-6.83943898895643));
#163768=CARTESIAN_POINT('Ctrl Pts',(2.78652793768544,0.581858135446601,
-6.78248349093925));
#163769=CARTESIAN_POINT('Ctrl Pts',(2.87375705997847,0.562053380737001,
-6.72366306435497));
#163770=CARTESIAN_POINT('Ctrl Pts',(2.9599303685496,0.767963166031737,-6.91075845180163));
#163771=CARTESIAN_POINT('Ctrl Pts',(2.85670529872925,0.753333602552418,
-6.93905556288548));
#163772=CARTESIAN_POINT('Ctrl Pts',(2.75289336527756,0.738713518238556,
-6.96517422327883));
#163773=CARTESIAN_POINT('Ctrl Pts',(2.54483847479892,0.709588702262668,
-7.01287202811285));
#163774=CARTESIAN_POINT('Ctrl Pts',(2.44062372419453,0.695086899270088,
-7.03447158992617));
#163775=CARTESIAN_POINT('Ctrl Pts',(2.33598634187701,0.680609079004666,
-7.05387263108362));
#163776=CARTESIAN_POINT('Ctrl Pts',(2.87375705921098,0.562053378832269,
-6.72366306261159));
#163777=CARTESIAN_POINT('Ctrl Pts',(2.9770211335591,0.582225215204339,-6.70146410395925));
#163778=CARTESIAN_POINT('Ctrl Pts',(3.0797795908864,0.602198340253702,-6.67686751428585));
#163779=CARTESIAN_POINT('Ctrl Pts',(3.23288349207581,0.631811365792358,
-6.63643569582469));
#163780=CARTESIAN_POINT('Ctrl Pts',(3.28364302353049,0.641604918933792,
-6.62240072356809));
#163781=CARTESIAN_POINT('Ctrl Pts',(3.38916501123893,0.66191478057786,-6.59190394743353));
#163782=CARTESIAN_POINT('Ctrl Pts',(3.43977429202624,0.671621084023588,
-6.57653002766987));
#163783=CARTESIAN_POINT('Ctrl Pts',(3.4866624024038,0.680609080079151,-6.56179370238188));
#163784=CARTESIAN_POINT('Ctrl Pts',(2.859771516,0.810731746,-6.662147317));
#163785=CARTESIAN_POINT('Ctrl Pts',(2.494006057,0.745065281,-6.819154599));
#163786=CARTESIAN_POINT('Ctrl Pts',(2.113250748,0.680609079,-6.93517637));
#163787=CARTESIAN_POINT('Ctrl Pts',(3.182814947,0.810731746,-6.79114784200001));
#163788=CARTESIAN_POINT('Ctrl Pts',(2.809967097,0.745065281,-6.965890866));
#163789=CARTESIAN_POINT('Ctrl Pts',(2.420230359,0.680609079,-7.098766443));
#163790=CARTESIAN_POINT('Ctrl Pts',(3.20712842706674,0.810731746,-6.80085691326475));
#163791=CARTESIAN_POINT('Ctrl Pts',(2.83374752932183,0.745065281,-6.97693479681675));
#163792=CARTESIAN_POINT('Ctrl Pts',(2.44333481473786,0.680609079,-7.11107885550346));
#163793=CARTESIAN_POINT('',(2.22528673569468,0.680609081791282,-6.99488059468723));
#163794=CARTESIAN_POINT('Ctrl Pts',(2.113250748,0.680609079,-6.93517637));
#163795=CARTESIAN_POINT('Ctrl Pts',(1.73744496,0.745496505000001,-7.04968994800001));
#163796=CARTESIAN_POINT('Ctrl Pts',(1.351465456,0.810723991,-7.122923636));
#163797=CARTESIAN_POINT('Ctrl Pts',(1.949660675,0.680609079,-7.24215598100001));
#163798=CARTESIAN_POINT('Ctrl Pts',(1.557220167,0.745496505000001,-7.34780488300001));
#163799=CARTESIAN_POINT('Ctrl Pts',(1.155661261,0.810723991,-7.410428264));
#163800=CARTESIAN_POINT('Ctrl Pts',(1.93736906680233,0.680609079,-7.26522139709702));
#163801=CARTESIAN_POINT('Ctrl Pts',(1.54367868185706,0.745496505000001,
-7.37020423713987));
#163802=CARTESIAN_POINT('Ctrl Pts',(1.14094919195899,0.810723991,-7.43203039533711));
#163803=CARTESIAN_POINT('',(1.99455449275703,0.68060908041698,-7.15791196576213));
#163804=CARTESIAN_POINT('',(2.05354654700497,0.680609082082812,-7.04721236860769));
#163805=CARTESIAN_POINT('',(1.40507629648974,0.767980175645073,-7.38535681937711));
#163806=CARTESIAN_POINT('Ctrl Pts',(1.99455448593649,0.680609079136802,
-7.15791196436369));
#163807=CARTESIAN_POINT('Ctrl Pts',(1.89827331417205,0.695136945000173,
-7.19982208236072));
#163808=CARTESIAN_POINT('Ctrl Pts',(1.80112099588355,0.709660812754888,
-7.23970433265933));
#163809=CARTESIAN_POINT('Ctrl Pts',(1.60459449158103,0.738780776796205,
-7.31560426581368));
#163810=CARTESIAN_POINT('Ctrl Pts',(1.50523105622012,0.753373671720888,
-7.3515882156345));
#163811=CARTESIAN_POINT('Ctrl Pts',(1.40514120807807,0.76794900784462,-7.38546785721208));
#163812=CARTESIAN_POINT('Ctrl Pts',(1.35606856510727,0.809946052688147,
-7.12204872604119));
#163813=CARTESIAN_POINT('Ctrl Pts',(1.36387161560445,0.802922931425193,
-7.16376252090609));
#163814=CARTESIAN_POINT('Ctrl Pts',(1.37166441273046,0.79607875249018,-7.20553626587412));
#163815=CARTESIAN_POINT('Ctrl Pts',(1.38798424115962,0.782074140061212,
-7.29323971148109));
#163816=CARTESIAN_POINT('Ctrl Pts',(1.39651924027891,0.774939590284013,
-7.3392341474405));
#163817=CARTESIAN_POINT('Ctrl Pts',(1.40503253810627,0.767997185255711,
-7.38522734486377));
#163818=CARTESIAN_POINT('Origin',(6.91720986045752E-14,0.560925700000067,
-4.49727061146987E-13));
#163819=CARTESIAN_POINT('',(0.764998169984091,0.680609080258875,-7.39112502442283));
#163820=CARTESIAN_POINT('',(1.36118141054067,0.562053379621627,-7.18424037696642));
#163821=CARTESIAN_POINT('Ctrl Pts',(0.764998169435021,0.68060908006245,
-7.39112502271931));
#163822=CARTESIAN_POINT('Ctrl Pts',(0.810822724249504,0.671661524822522,
-7.3773867236855));
#163823=CARTESIAN_POINT('Ctrl Pts',(0.861446653293738,0.66173857347019,
-7.36172331463118));
#163824=CARTESIAN_POINT('Ctrl Pts',(0.966064546025971,0.641119488217196,
-7.32789324004562));
#163825=CARTESIAN_POINT('Ctrl Pts',(1.01578044798146,0.631275792611451,
-7.31122933773633));
#163826=CARTESIAN_POINT('Ctrl Pts',(1.16471257591828,0.601654471644855,
-7.25954181665948));
#163827=CARTESIAN_POINT('Ctrl Pts',(1.26334700347819,0.581858135037895,
-7.22293393264052));
#163828=CARTESIAN_POINT('Ctrl Pts',(1.36118141087409,0.562053380214067,
-7.18424037750623));
#163829=CARTESIAN_POINT('Ctrl Pts',(1.40512005487322,0.767963166034435,
-7.38548629389044));
#163830=CARTESIAN_POINT('Ctrl Pts',(1.29822528732601,0.753333602530371,
-7.39093149553088));
#163831=CARTESIAN_POINT('Ctrl Pts',(1.19122567919874,0.738713518197604,
-7.39412301911702));
#163832=CARTESIAN_POINT('Ctrl Pts',(0.977781373906088,0.709588701609241,
-7.39598002441255));
#163833=CARTESIAN_POINT('Ctrl Pts',(0.871359841310341,0.695086898941891,
-7.39467150955204));
#163834=CARTESIAN_POINT('Ctrl Pts',(0.764998174704899,0.680609078987347,
-7.39112502109302));
#163835=CARTESIAN_POINT('Ctrl Pts',(1.36118141059066,0.562053379366792,
-7.18424037669758));
#163836=CARTESIAN_POINT('Ctrl Pts',(1.46680007254095,0.582224590158785,
-7.18475912476055));
#163837=CARTESIAN_POINT('Ctrl Pts',(1.57245018243156,0.602198953355514,
-7.18282750052659));
#163838=CARTESIAN_POINT('Ctrl Pts',(1.73066166566679,0.631811121704626,
-7.17625395876863));
#163839=CARTESIAN_POINT('Ctrl Pts',(1.78325026707083,0.641604433121933,
-7.17345899964121));
#163840=CARTESIAN_POINT('Ctrl Pts',(1.89286125451794,0.661914325723975,
-7.1663593834956));
#163841=CARTESIAN_POINT('Ctrl Pts',(1.94559354184426,0.671620866139669,
-7.16222430769084));
#163842=CARTESIAN_POINT('Ctrl Pts',(1.99455449261922,0.680609080066209,
-7.15791196346636));
#163843=CARTESIAN_POINT('Ctrl Pts',(1.360746905,0.810731746,-7.121156357));
#163844=CARTESIAN_POINT('Ctrl Pts',(0.969780916,0.745065281,-7.195864134));
#163845=CARTESIAN_POINT('Ctrl Pts',(0.572986203,0.680609079,-7.227322244));
#163846=CARTESIAN_POINT('Ctrl Pts',(1.648506461,0.810731746,-7.31658571));
#163847=CARTESIAN_POINT('Ctrl Pts',(1.246811002,0.745065281,-7.407092072));
#163848=CARTESIAN_POINT('Ctrl Pts',(0.837621771,0.680609079,-7.453079214));
#163849=CARTESIAN_POINT('Ctrl Pts',(1.67016434216083,0.810731746,-7.3312944681085));
#163850=CARTESIAN_POINT('Ctrl Pts',(1.26766134234651,0.745065281,-7.42298989184181));
#163851=CARTESIAN_POINT('Ctrl Pts',(0.857539252672341,0.680609079,-7.47007054417667));
#163852=CARTESIAN_POINT('',(0.669568207960791,0.680609081791281,-7.30971504256078));
#163853=CARTESIAN_POINT('Ctrl Pts',(0.572986203,0.680609079,-7.227322244));
#163854=CARTESIAN_POINT('Ctrl Pts',(0.181349511,0.745496505000001,-7.25837142200001));
#163855=CARTESIAN_POINT('Ctrl Pts',(-0.211349085,0.810723991,-7.24691876300001));
#163856=CARTESIAN_POINT('Ctrl Pts',(0.347229232,0.680609079,-7.491957812));
#163857=CARTESIAN_POINT('Ctrl Pts',(-0.0587476260000001,0.745496505000001,
-7.510773593));
#163858=CARTESIAN_POINT('Ctrl Pts',(-0.464380483,0.810723991,-7.485609579));
#163859=CARTESIAN_POINT('Ctrl Pts',(0.330266612023814,0.680609079,-7.51184163907424));
#163860=CARTESIAN_POINT('Ctrl Pts',(-0.0767877178485978,0.745496505000001,
-7.52973824374311));
#163861=CARTESIAN_POINT('Ctrl Pts',(-0.483392411744903,0.810723991,-7.50354400461565));
#163862=CARTESIAN_POINT('',(0.409183430363367,0.68060908042706,-7.41933421904734));
#163863=CARTESIAN_POINT('',(0.490593424731522,0.680609082082812,-7.32390426471177));
#163864=CARTESIAN_POINT('',(-0.215407013297438,0.767980175633115,-7.51474115102437));
#163865=CARTESIAN_POINT('Ctrl Pts',(0.409183424044645,0.68060907912779,
-7.41933421624228));
#163866=CARTESIAN_POINT('Ctrl Pts',(0.306143817310809,0.695136944806357,
-7.43956689283184));
#163867=CARTESIAN_POINT('Ctrl Pts',(0.202689362634763,0.70966081237921,
-7.4576318414953));
#163868=CARTESIAN_POINT('Ctrl Pts',(-0.0055587055481005,0.738780776750879,
-7.48950988760412));
#163869=CARTESIAN_POINT('Ctrl Pts',(-0.11033456455517,0.753373671687691,
-7.50329235124383));
#163870=CARTESIAN_POINT('Ctrl Pts',(-0.215367489144336,0.767949007826713,
-7.51486354692501));
#163871=CARTESIAN_POINT('Ctrl Pts',(-0.206665514471121,0.809946052642357,
-7.24705384082526));
#163872=CARTESIAN_POINT('Ctrl Pts',(-0.208012127760169,0.802922931364602,
-7.28946981573807));
#163873=CARTESIAN_POINT('Ctrl Pts',(-0.209381642207943,0.796078752490285,
-7.33194213449867));
#163874=CARTESIAN_POINT('Ctrl Pts',(-0.212297010597966,0.782074140047893,
-7.42110340320246));
#163875=CARTESIAN_POINT('Ctrl Pts',(-0.213848999176155,0.774939590272211,
-7.46785728735778));
#163876=CARTESIAN_POINT('Ctrl Pts',(-0.215421915454735,0.76799718524202,
-7.51460529679075));
#163877=CARTESIAN_POINT('Origin',(-5.12014475956279E-14,0.560925700000022,
9.36750677027476E-14));
#163878=CARTESIAN_POINT('',(-0.84176046229091,0.680609080286941,-7.38277662196963));
#163879=CARTESIAN_POINT('',(-0.215041571561947,0.562053379558999,-7.3088905962547));
#163880=CARTESIAN_POINT('Ctrl Pts',(-0.841760462439525,0.680609080144953,
-7.38277662033779));
#163881=CARTESIAN_POINT('Ctrl Pts',(-0.794053931958486,0.671661524879478,
-7.37921043980768));
#163882=CARTESIAN_POINT('Ctrl Pts',(-0.741246392298931,0.661738573515153,
-7.37479588085074));
#163883=CARTESIAN_POINT('Ctrl Pts',(-0.631801941938972,0.641119488276378,
-7.36424648905931));
#163884=CARTESIAN_POINT('Ctrl Pts',(-0.579666123820091,0.63127579267547,
-7.35865962885286));
#163885=CARTESIAN_POINT('Ctrl Pts',(-0.423104657345012,0.60165447171773,
-7.34019653839765));
#163886=CARTESIAN_POINT('Ctrl Pts',(-0.318906635060471,0.581858135111766,
-7.32564801267825));
#163887=CARTESIAN_POINT('Ctrl Pts',(-0.215041571295957,0.562053380310879,
-7.30889059701473));
#163888=CARTESIAN_POINT('Ctrl Pts',(-0.215392111140141,0.767963166024209,
-7.514877005258));
#163889=CARTESIAN_POINT('Ctrl Pts',(-0.320958295798627,0.75333360254386,
-7.49721568589562));
#163890=CARTESIAN_POINT('Ctrl Pts',(-0.426142395756981,0.738713518225547,
-7.47733084058546));
#163891=CARTESIAN_POINT('Ctrl Pts',(-0.634995693504388,0.709588701579514,
-7.433260213766));
#163892=CARTESIAN_POINT('Ctrl Pts',(-0.73864785765739,0.695086898924898,
-7.40910480755326));
#163893=CARTESIAN_POINT('Ctrl Pts',(-0.841760457205502,0.680609078986858,
-7.38277661976896));
#163894=CARTESIAN_POINT('Ctrl Pts',(-0.215041571424503,0.562053379230467,
-7.30889059593007));
#163895=CARTESIAN_POINT('Ctrl Pts',(-0.112003730550206,0.582224590007247,
-7.33210210620165));
#163896=CARTESIAN_POINT('Ctrl Pts',(-0.00840841935307247,0.602198953227445,
-7.35292729293288));
#163897=CARTESIAN_POINT('Ctrl Pts',(0.147517284441341,0.631811121614305,
-7.3805182291761));
#163898=CARTESIAN_POINT('Ctrl Pts',(0.199477227084608,0.641604433037009,
-7.38909360944579));
#163899=CARTESIAN_POINT('Ctrl Pts',(0.308051845719433,0.661914338321119,
-7.40572311100768));
#163900=CARTESIAN_POINT('Ctrl Pts',(0.360440179027586,0.671620874009537,
-7.41302058903849));
#163901=CARTESIAN_POINT('Ctrl Pts',(0.409183430708766,0.680609080099152,
-7.41933421684758));
#163902=CARTESIAN_POINT('Ctrl Pts',(-0.201904718,0.810731746,-7.24718804));
#163903=CARTESIAN_POINT('Ctrl Pts',(-0.599790104,0.745065281,-7.23610306));
#163904=CARTESIAN_POINT('Ctrl Pts',(-0.994070541000001,0.680609079,-7.18152656200001));
#163905=CARTESIAN_POINT('Ctrl Pts',(0.037115645,0.810731746,-7.499908161));
#163906=CARTESIAN_POINT('Ctrl Pts',(-0.37464459,0.745065281,-7.501945886));
#163907=CARTESIAN_POINT('Ctrl Pts',(-0.78415308,0.680609079,-7.458894285));
#163908=CARTESIAN_POINT('Ctrl Pts',(0.0551052287059663,0.810731746,-7.51892884071888));
#163909=CARTESIAN_POINT('Ctrl Pts',(-0.357699280323076,0.745065281,-7.52195423052317));
#163910=CARTESIAN_POINT('Ctrl Pts',(-0.768353891643804,0.680609079,-7.47977003720628));
#163911=CARTESIAN_POINT('',(-0.917458585476369,0.680609081791282,-7.28275533886137));
#163912=CARTESIAN_POINT('Ctrl Pts',(-0.994070541,0.680609079,-7.181526562));
#163913=CARTESIAN_POINT('Ctrl Pts',(-1.38322564,0.745496505000001,-7.127659516));
#163914=CARTESIAN_POINT('Ctrl Pts',(-1.764281177,0.810723991,-7.03205602400001));
#163915=CARTESIAN_POINT('Ctrl Pts',(-1.271438263,0.680609079,-7.391444023));
#163916=CARTESIAN_POINT('Ctrl Pts',(-1.671968444,0.745496505000001,-7.32254687700001));
#163917=CARTESIAN_POINT('Ctrl Pts',(-2.062708312,0.810723991,-7.21077211));
#163918=CARTESIAN_POINT('Ctrl Pts',(-1.29227874146047,0.680609079,-7.40721651553411));
#163919=CARTESIAN_POINT('Ctrl Pts',(-1.69366360789286,0.745496505000001,
-7.33719005833291));
#163920=CARTESIAN_POINT('Ctrl Pts',(-2.08513112397734,0.810723991,-7.22420023607741));
#163921=CARTESIAN_POINT('',(-1.19532059374951,0.680609080406583,-7.33383665026911));
#163922=CARTESIAN_POINT('',(-1.09428701315318,0.680609082082812,-7.25737241764844));
#163923=CARTESIAN_POINT('',(-1.82581813019941,0.76798017564556,-7.29274453850138));
#163924=CARTESIAN_POINT('Ctrl Pts',(-1.19532059940679,0.680609079142472,
-7.33383664609925));
#163925=CARTESIAN_POINT('Ctrl Pts',(-1.30030062681116,0.695136945115343,
-7.33144582430566));
#163926=CARTESIAN_POINT('Ctrl Pts',(-1.40521980584584,0.709660812978692,
-7.32684877463772));
#163927=CARTESIAN_POINT('Ctrl Pts',(-1.61545198357233,0.738780776798224,
-7.31321435110408));
#163928=CARTESIAN_POINT('Ctrl Pts',(-1.7207410634257,0.753373671714424,
-7.30415087586492));
#163929=CARTESIAN_POINT('Ctrl Pts',(-1.82580584156822,0.767949007826193,
-7.29287256937691));
#163930=CARTESIAN_POINT('Ctrl Pts',(-1.75973614394106,0.809946052460278,
-7.03319477416626));
#163931=CARTESIAN_POINT('Ctrl Pts',(-1.77016945517068,0.802922931140822,
-7.07432960524266));
#163932=CARTESIAN_POINT('Ctrl Pts',(-1.78063724403593,0.796078752428626,
-7.11551453861799));
#163933=CARTESIAN_POINT('Ctrl Pts',(-1.80265149000155,0.78207413998448,
-7.20196454829124));
#163934=CARTESIAN_POINT('Ctrl Pts',(-1.81421789693137,0.774939590244176,
-7.24729172070654));
#163935=CARTESIAN_POINT('Ctrl Pts',(-1.82580347933559,0.76799718525082,
-7.29260865692637));
#163936=CARTESIAN_POINT('Origin',(-1.14166488762724E-13,0.560925699999978,
-5.13911829758129E-13));
#163937=CARTESIAN_POINT('',(-2.40915931034892,0.680609080213132,-7.02921779044765));
#163938=CARTESIAN_POINT('',(-1.78120945046844,0.562053379756257,-7.09178521403228));
#163939=CARTESIAN_POINT('Ctrl Pts',(-2.40915931011412,0.680609079936094,
-7.02921778843984));
#163940=CARTESIAN_POINT('Ctrl Pts',(-2.36180150889329,0.671661524763371,
-7.03599047701499));
#163941=CARTESIAN_POINT('Ctrl Pts',(-2.30927958083451,0.661738573470731,
-7.04303118800338));
#163942=CARTESIAN_POINT('Ctrl Pts',(-2.20012607373983,0.641119488286034,
-7.05625575679003));
#163943=CARTESIAN_POINT('Ctrl Pts',(-2.1480081524798,0.631275792729284,
-7.06200717403117));
#163944=CARTESIAN_POINT('Ctrl Pts',(-1.99113798809114,0.601654471923386,
-7.07763182771462));
#163945=CARTESIAN_POINT('Ctrl Pts',(-1.88624855517428,0.581858135430499,
-7.08582293316892));
#163946=CARTESIAN_POINT('Ctrl Pts',(-1.78120945034197,0.562053380742793,
-7.09178521508122));
#163947=CARTESIAN_POINT('Ctrl Pts',(-1.82583278106323,0.7679631660403,-7.29288042007639));
#163948=CARTESIAN_POINT('Ctrl Pts',(-1.9251342252849,0.753333602553888,
-7.25293840338144));
#163949=CARTESIAN_POINT('Ctrl Pts',(-2.02358452538462,0.738713518227169,
-7.21090698245767));
#163950=CARTESIAN_POINT('Ctrl Pts',(-2.2180810666693,0.70958870158529,-7.12296941717666));
#163951=CARTESIAN_POINT('Ctrl Pts',(-2.3141172022883,0.695086898937427,
-7.07709659967735));
#163952=CARTESIAN_POINT('Ctrl Pts',(-2.40915930432956,0.68060907898539,
-7.02921778941742));
#163953=CARTESIAN_POINT('Ctrl Pts',(-1.78120944989328,0.562053378830073,
-7.09178521322179));
#163954=CARTESIAN_POINT('Ctrl Pts',(-1.68556739894358,0.582225215193757,
-7.13660553132821));
#163955=CARTESIAN_POINT('Ctrl Pts',(-1.58887688169021,0.602198340238744,
-7.17921112563103));
#163956=CARTESIAN_POINT('Ctrl Pts',(-1.44252363383872,0.631811365737381,
-7.23967816847744));
#163957=CARTESIAN_POINT('Ctrl Pts',(-1.39362071976889,0.641604918834856,
-7.25922338390512));
#163958=CARTESIAN_POINT('Ctrl Pts',(-1.29115944627396,0.661914798004255,
-7.29880433212849));
#163959=CARTESIAN_POINT('Ctrl Pts',(-1.24156587658882,0.671621094886457,
-7.31719267986154));
#163960=CARTESIAN_POINT('Ctrl Pts',(-1.19532059288389,0.680609080033675,
-7.33383664806536));
#163961=CARTESIAN_POINT('Ctrl Pts',(-1.755115501,0.810731746,-7.034349265));
#163962=CARTESIAN_POINT('Ctrl Pts',(-2.141315605,0.745065281,-6.937989849));
#163963=CARTESIAN_POINT('Ctrl Pts',(-2.51464565,0.680609079,-6.79993068000001));
#163964=CARTESIAN_POINT('Ctrl Pts',(-1.576010657,0.810731746,-7.332543243));
#163965=CARTESIAN_POINT('Ctrl Pts',(-1.978582217,0.745065281,-7.246017048));
#163966=CARTESIAN_POINT('Ctrl Pts',(-2.369261804,0.680609079,-7.115939748));
#163967=CARTESIAN_POINT('Ctrl Pts',(-1.5625305438092,0.810731746,-7.35498645830609));
#163968=CARTESIAN_POINT('Ctrl Pts',(-1.96633428198512,0.745065281,-7.26920034899641));
#163969=CARTESIAN_POINT('Ctrl Pts',(-2.35831966164122,0.680609079,-7.13972379487905));
#163970=CARTESIAN_POINT('',(-2.46158603461972,0.680609081791281,-6.91526209026196));
#163971=CARTESIAN_POINT('Ctrl Pts',(-2.51464565,0.680609079,-6.79993068));
#163972=CARTESIAN_POINT('Ctrl Pts',(-2.883122697,0.745496505000001,-6.663666173));
#163973=CARTESIAN_POINT('Ctrl Pts',(-3.234717443,0.810723991,-6.488382161));
#163974=CARTESIAN_POINT('Ctrl Pts',(-2.830654719,0.680609079,-6.945314526));
#163975=CARTESIAN_POINT('Ctrl Pts',(-3.207009877,0.745496505000001,-6.791926008));
#163976=CARTESIAN_POINT('Ctrl Pts',(-3.564586193,0.810723991,-6.598766951));
#163977=CARTESIAN_POINT('Ctrl Pts',(-2.85439857823173,0.680609079,-6.95623817950437));
#163978=CARTESIAN_POINT('Ctrl Pts',(-3.23134567101129,0.745496505000001,
-6.80156302087739));
#163979=CARTESIAN_POINT('Ctrl Pts',(-3.58937142207502,0.810723991,-6.60706089308014));
#163980=CARTESIAN_POINT('',(-2.74393275571236,0.680609080390424,-6.90541703064292));
#163981=CARTESIAN_POINT('',(-2.62997704800503,0.680609082082812,-6.85299031890594));
#163982=CARTESIAN_POINT('',(-3.35085602073211,0.767980175593935,-6.72974729659381));
#163983=CARTESIAN_POINT('Ctrl Pts',(-2.74393276050547,0.680609079132267,
-6.90541702525689));
#163984=CARTESIAN_POINT('Ctrl Pts',(-2.84594445597044,0.695136944937039,
-6.88051449714559));
#163985=CARTESIAN_POINT('Ctrl Pts',(-2.94742245181023,0.70966081261579,
-6.85347040226978));
#163986=CARTESIAN_POINT('Ctrl Pts',(-3.14980852231464,0.738780776766089,
-6.79496103952786));
#163987=CARTESIAN_POINT('Ctrl Pts',(-3.25068762275745,0.753373671682622,
-6.76347542344459));
#163988=CARTESIAN_POINT('Ctrl Pts',(-3.35087154228855,0.767949007788142,
-6.72987497586571));
#163989=CARTESIAN_POINT('Ctrl Pts',(-3.23052346694552,0.809946052592434,
-6.49047133466123));
#163990=CARTESIAN_POINT('Ctrl Pts',(-3.24955562579035,0.802922931297973,
-6.52840160248477));
#163991=CARTESIAN_POINT('Ctrl Pts',(-3.26863222728892,0.796078752413679,
-6.56637339069007));
#163992=CARTESIAN_POINT('Ctrl Pts',(-3.30871598903657,0.782074139977129,
-6.64606983483956));
#163993=CARTESIAN_POINT('Ctrl Pts',(-3.32975598209915,0.774939590214679,
-6.68785084763502));
#163994=CARTESIAN_POINT('Ctrl Pts',(-3.35081250185054,0.767997185203043,
-6.72961774137811));
#163995=CARTESIAN_POINT('Origin',(5.85469173142172E-13,0.560925700000111,
1.36782946080771E-12));
#163996=CARTESIAN_POINT('',(-3.86390854712789,0.680609080271912,-6.34698054711008));
#163997=CARTESIAN_POINT('',(-3.26408995016512,0.562053379612811,-6.54307583813135));
#163998=CARTESIAN_POINT('Ctrl Pts',(-3.86390854656277,0.680609080104214,
-6.34698054551348));
#163999=CARTESIAN_POINT('Ctrl Pts',(-3.81911387217345,0.671661524886997,
-6.36377541977018));
#164000=CARTESIAN_POINT('Ctrl Pts',(-3.76933342214294,0.66173857352756,
-6.38194218488432));
#164001=CARTESIAN_POINT('Ctrl Pts',(-3.66557475447777,0.641119488245391,
-6.41832234811752));
#164002=CARTESIAN_POINT('Ctrl Pts',(-3.61591170567734,0.631275792618738,
-6.4351431129641));
#164003=CARTESIAN_POINT('Ctrl Pts',(-3.46606791648177,0.601654471617293,
-6.48412491938828));
#164004=CARTESIAN_POINT('Ctrl Pts',(-3.36539158528181,0.581858135000715,
-6.51467264899996));
#164005=CARTESIAN_POINT('Ctrl Pts',(-3.26408995022167,0.56205338015989,
-6.54307583871452));
#164006=CARTESIAN_POINT('Ctrl Pts',(-3.35089953961369,0.767963165984828,
-6.7298768518095));
#164007=CARTESIAN_POINT('Ctrl Pts',(-3.43929301839793,0.753333602505536,
-6.66952178206919));
#164008=CARTESIAN_POINT('Ctrl Pts',(-3.52640609218595,0.738713518184776,
-6.60730912803424));
#164009=CARTESIAN_POINT('Ctrl Pts',(-3.69745143796608,0.709588701116743,
-6.47961648509564));
#164010=CARTESIAN_POINT('Ctrl Pts',(-3.78138100101789,0.695086898699007,
-6.41417121913299));
#164011=CARTESIAN_POINT('Ctrl Pts',(-3.86390854139516,0.680609078973892,
-6.34698054733611));
#164012=CARTESIAN_POINT('Ctrl Pts',(-3.26408994997813,0.562053379377489,
-6.54307583796165));
#164013=CARTESIAN_POINT('Ctrl Pts',(-3.18032159845886,0.582224590134105,
-6.60740650056184));
#164014=CARTESIAN_POINT('Ctrl Pts',(-3.09504530934754,0.602198953333155,
-6.66980547027568));
#164015=CARTESIAN_POINT('Ctrl Pts',(-2.96511610677917,0.631811121670721,
-6.76031782940335));
#164016=CARTESIAN_POINT('Ctrl Pts',(-2.92155924884402,0.641604433060527,
-6.78991804730418));
#164017=CARTESIAN_POINT('Ctrl Pts',(-2.83000234288128,0.661914293374162,
-6.85059973890839));
#164018=CARTESIAN_POINT('Ctrl Pts',(-2.78552004907774,0.671620845873208,
-6.87922008882333));
#164019=CARTESIAN_POINT('Ctrl Pts',(-2.74393275435454,0.680609079990549,
-6.90541702862458));
#164020=CARTESIAN_POINT('Ctrl Pts',(-3.226259034,0.810731746,-6.492592136));
#164021=CARTESIAN_POINT('Ctrl Pts',(-3.582715568,0.745065281,-6.315463943));
#164022=CARTESIAN_POINT('Ctrl Pts',(-3.917638724,0.680609079,-6.100377597));
#164023=CARTESIAN_POINT('Ctrl Pts',(-3.115444452,0.810731746,-6.822316752));
#164024=CARTESIAN_POINT('Ctrl Pts',(-3.490003539,0.745065281,-6.651272505));
#164025=CARTESIAN_POINT('Ctrl Pts',(-3.84358648,0.680609079,-6.440251778));
#164026=CARTESIAN_POINT('Ctrl Pts',(-3.10710412403857,0.810731746,-6.84713308379284));
#164027=CARTESIAN_POINT('Ctrl Pts',(-3.48302567819979,0.745065281,-6.67654673776603));
#164028=CARTESIAN_POINT('Ctrl Pts',(-3.83801302576597,0.680609079,-6.46583200475358));
#164029=CARTESIAN_POINT('',(-3.89061245650934,0.680609081791279,-6.22441887193084));
#164030=CARTESIAN_POINT('Ctrl Pts',(-3.917638724,0.680609079,-6.100377597));
#164031=CARTESIAN_POINT('Ctrl Pts',(-4.248208141,0.745496505000001,-5.888087205));
#164032=CARTESIAN_POINT('Ctrl Pts',(-4.553901916,0.810723991,-5.64131875900001));
#164033=CARTESIAN_POINT('Ctrl Pts',(-4.257512905,0.680609079,-6.174429841));
#164034=CARTESIAN_POINT('Ctrl Pts',(-4.592095092,0.745496505000001,-5.94372222700001));
#164035=CARTESIAN_POINT('Ctrl Pts',(-4.899787985,0.810723991,-5.67821078400001));
#164036=CARTESIAN_POINT('Ctrl Pts',(-4.28304990857418,0.680609079,-6.17999387770952));
#164037=CARTESIAN_POINT('Ctrl Pts',(-4.61793360162425,0.745496505000001,
-5.94790245555247));
#164038=CARTESIAN_POINT('Ctrl Pts',(-4.92577670163132,0.810723991,-5.68098272675691));
#164039=CARTESIAN_POINT('',(-4.16424167156072,0.68060908040942,-6.15410778545866));
#164040=CARTESIAN_POINT('',(-4.04043957907103,0.680609082082812,-6.12713362678962));
#164041=CARTESIAN_POINT('',(-4.71921160804611,0.767980175629172,-5.85207455067974));
#164042=CARTESIAN_POINT('Ctrl Pts',(-4.16424167499564,0.680609079127669,
-6.15410777928402));
#164043=CARTESIAN_POINT('Ctrl Pts',(-4.25851508568839,0.695136944827101,
-6.10785795963635));
#164044=CARTESIAN_POINT('Ctrl Pts',(-4.35180690085521,0.709660812410746,
-6.05963137155408));
#164045=CARTESIAN_POINT('Ctrl Pts',(-4.53688351532785,0.738780776763756,
-5.95898290182754));
#164046=CARTESIAN_POINT('Ctrl Pts',(-4.62863564177466,0.753373671697259,
-5.90654737729357));
#164047=CARTESIAN_POINT('Ctrl Pts',(-4.7192542139961,0.767949007827546,
-5.85219590820191));
#164048=CARTESIAN_POINT('Ctrl Pts',(-4.55025510319298,0.809946052614754,
-5.64426066970121));
#164049=CARTESIAN_POINT('Ctrl Pts',(-4.57699618717919,0.802922931345544,
-5.67721279729065));
#164050=CARTESIAN_POINT('Ctrl Pts',(-4.6037896005029,0.796078752452168,
-5.71019592084041));
#164051=CARTESIAN_POINT('Ctrl Pts',(-4.66006860596506,0.782074140026348,
-5.77941228251503));
#164052=CARTESIAN_POINT('Ctrl Pts',(-4.68959837845096,0.774939590259562,
-5.81569350193402));
#164053=CARTESIAN_POINT('Ctrl Pts',(-4.71914125606377,0.767997185239498,
-5.85195737967383));
#164054=CARTESIAN_POINT('Origin',(-2.12503625807159E-14,0.560925699999978,
6.54858112181245E-14));
#164055=CARTESIAN_POINT('',(-4.594345237046,0.562053379770818,-5.68841950555253));
#164056=CARTESIAN_POINT('Ctrl Pts',(-4.5943452360446,0.562053378678052,
-5.68841950498304));
#164057=CARTESIAN_POINT('Ctrl Pts',(-4.52636453261428,0.582224589590113,
-5.76925387232301));
#164058=CARTESIAN_POINT('Ctrl Pts',(-4.45649588941519,0.602198952910481,
-5.84852587065802));
#164059=CARTESIAN_POINT('Ctrl Pts',(-4.34906095411072,0.631811365757422,
-5.96485399947606));
#164060=CARTESIAN_POINT('Ctrl Pts',(-4.31288469410678,0.641604918902546,
-6.0031265574176));
#164061=CARTESIAN_POINT('Ctrl Pts',(-4.23651301061102,0.661914787148201,
-6.0820715827627));
#164062=CARTESIAN_POINT('Ctrl Pts',(-4.19922415999308,0.67162108824664,
-6.11958420968522));
#164063=CARTESIAN_POINT('Ctrl Pts',(-4.16424166988398,0.680609080047746,
-6.1541077838538));
#164064=CARTESIAN_POINT('',(-5.13798571439363,0.680609080190355,-5.36796554832296));
#164065=CARTESIAN_POINT('Ctrl Pts',(-5.13798571330918,0.680609079974861,
-5.36796554657682));
#164066=CARTESIAN_POINT('Ctrl Pts',(-5.09784871543656,0.671661524847478,
-5.39399729660559));
#164067=CARTESIAN_POINT('Ctrl Pts',(-5.053137422544,0.661738573571544,-5.42244065785812));
#164068=CARTESIAN_POINT('Ctrl Pts',(-4.95962523510226,0.641119488400852,
-5.48027531923473));
#164069=CARTESIAN_POINT('Ctrl Pts',(-4.91473924827774,0.631275792831726,
-5.50737891125491));
#164070=CARTESIAN_POINT('Ctrl Pts',(-4.77892836490913,0.601654472016654,
-5.58742753516421));
#164071=CARTESIAN_POINT('Ctrl Pts',(-4.6871726497635,0.581858135529807,
-5.63890351086657));
#164072=CARTESIAN_POINT('Ctrl Pts',(-4.59434523742545,0.562053380890475,
-5.68841950671169));
#164073=CARTESIAN_POINT('Ctrl Pts',(-4.71928196002846,0.767963166018845,
-5.85219172168565));
#164074=CARTESIAN_POINT('Ctrl Pts',(-4.79263429243288,0.753333602530235,
-5.7742457349207));
#164075=CARTESIAN_POINT('Ctrl Pts',(-4.8643368292945,0.738713518208989,
-5.69476084238225));
#164076=CARTESIAN_POINT('Ctrl Pts',(-5.00393308407793,0.709588701590787,
-5.53328389173144));
#164077=CARTESIAN_POINT('Ctrl Pts',(-5.07183162414147,0.695086898935622,
-5.45132632333071));
#164078=CARTESIAN_POINT('Ctrl Pts',(-5.13798570921413,0.680609078986734,
-5.36796554912861));
#164079=CARTESIAN_POINT('Ctrl Pts',(-4.54654628,0.810731746,-5.647248615));
#164080=CARTESIAN_POINT('Ctrl Pts',(-4.85659173300001,0.745065281,-5.397633963));
#164081=CARTESIAN_POINT('Ctrl Pts',(-5.137447365,0.680609079,-5.11557763800001));
#164082=CARTESIAN_POINT('Ctrl Pts',(-4.509203528,0.810731746,-5.993086312));
#164083=CARTESIAN_POINT('Ctrl Pts',(-4.838236174,0.745065281,-5.745521853));
#164084=CARTESIAN_POINT('Ctrl Pts',(-5.138189324,0.680609079,-5.46342479300001));
#164085=CARTESIAN_POINT('Ctrl Pts',(-4.50639297011688,0.810731746,-6.01911537556728));
#164086=CARTESIAN_POINT('Ctrl Pts',(-4.8368546646499,0.745065281,-5.77170522190873));
#164087=CARTESIAN_POINT('Ctrl Pts',(-5.13824516666302,0.680609079,-5.48960509603734));
#164088=CARTESIAN_POINT('',(-5.13771816422049,0.680609081791273,-5.24252874552383));
#164089=CARTESIAN_POINT('Ctrl Pts',(-5.137447365,0.680609079,-5.115577638));
#164090=CARTESIAN_POINT('Ctrl Pts',(-5.41465209400001,0.745496505000001,
-4.837187824));
#164091=CARTESIAN_POINT('Ctrl Pts',(-5.66015099700001,0.810723991,-4.530473562));
#164092=CARTESIAN_POINT('Ctrl Pts',(-5.48529452,0.680609079,-5.114835679));
#164093=CARTESIAN_POINT('Ctrl Pts',(-5.762459044,0.745496505000001,-4.81759660100001));
#164094=CARTESIAN_POINT('Ctrl Pts',(-6.005881136,0.810723991,-4.492147791));
#164095=CARTESIAN_POINT('Ctrl Pts',(-5.51143058654251,0.680609079,-5.11477993069355));
#164096=CARTESIAN_POINT('Ctrl Pts',(-5.78859208967389,0.745496505000001,
-4.81612458232567));
#164097=CARTESIAN_POINT('Ctrl Pts',(-6.03185813707295,0.810723991,-4.48926812133259));
#164098=CARTESIAN_POINT('',(-5.38983527524761,0.680609080402338,-5.11503929999281));
#164099=CARTESIAN_POINT('',(-5.26439847106798,0.680609082082805,-5.11530686482352));
#164100=CARTESIAN_POINT('',(-5.86690210549644,0.767980175626098,-4.70076530286576));
#164101=CARTESIAN_POINT('Ctrl Pts',(-5.38983527725203,0.680609079140822,
-5.11503929321169));
#164102=CARTESIAN_POINT('Ctrl Pts',(-5.47196228524896,0.695136945077434,
-5.04960477097213));
#164103=CARTESIAN_POINT('Ctrl Pts',(-5.55270570005654,0.709660812908944,
-4.98245070991648));
#164104=CARTESIAN_POINT('Ctrl Pts',(-5.71181887766143,0.73878077677887,
-4.84436934646061));
#164105=CARTESIAN_POINT('Ctrl Pts',(-5.79015380252541,0.753373671697209,
-4.77343574038703));
#164106=CARTESIAN_POINT('Ctrl Pts',(-5.86696980358536,0.767949007805755,
-4.7008746641221));
#164107=CARTESIAN_POINT('Ctrl Pts',(-5.65722186833464,0.809946052775441,
-4.53413064874382));
#164108=CARTESIAN_POINT('Ctrl Pts',(-5.69042149382425,0.802922931489543,
-4.5605638312732));
#164109=CARTESIAN_POINT('Ctrl Pts',(-5.72367888890452,0.796078752502292,
-4.58701603616805));
#164110=CARTESIAN_POINT('Ctrl Pts',(-5.79352159409118,0.782074140054355,
-4.64251583519036));
#164111=CARTESIAN_POINT('Ctrl Pts',(-5.83016036667187,0.77493959026445,
-4.67160079174287));
#164112=CARTESIAN_POINT('Ctrl Pts',(-5.86680821002045,0.76799718523115,
-4.7006659948091));
#164113=CARTESIAN_POINT('Origin',(1.16920362280837E-12,0.560925700000067,
9.99200722162641E-13));
#164114=CARTESIAN_POINT('',(-6.171816381008,0.680609080257676,-4.13795044509658));
#164115=CARTESIAN_POINT('',(-5.7097740415247,0.56205337966577,-4.56777900317126));
#164116=CARTESIAN_POINT('Ctrl Pts',(-6.17181637974723,0.680609080059578,
-4.13795044380038));
#164117=CARTESIAN_POINT('Ctrl Pts',(-6.13821381882902,0.671661524822212,
-4.17200185466163));
#164118=CARTESIAN_POINT('Ctrl Pts',(-6.10066233257506,0.66173857345913,
-4.20939183272496));
#164119=CARTESIAN_POINT('Ctrl Pts',(-6.02176915015887,0.641119488189323,
-4.28597670856538));
#164120=CARTESIAN_POINT('Ctrl Pts',(-5.98375904373633,0.631275792604873,
-4.32209579415727));
#164121=CARTESIAN_POINT('Ctrl Pts',(-5.86833143070661,0.601654471690628,
-4.42946825164726));
#164122=CARTESIAN_POINT('Ctrl Pts',(-5.78978672597655,0.581858135122761,
-4.49946551441468));
#164123=CARTESIAN_POINT('Ctrl Pts',(-5.70977404189956,0.562053380358149,
-4.56777900381104));
#164124=CARTESIAN_POINT('Ctrl Pts',(-5.86699600097242,0.767963166021046,
-4.70086461092242));
#164125=CARTESIAN_POINT('Ctrl Pts',(-5.92187731353065,0.753333602539643,
-4.60897237482362));
#164126=CARTESIAN_POINT('Ctrl Pts',(-5.97481658259202,0.738713518220881,
-4.51593186898607));
#164127=CARTESIAN_POINT('Ctrl Pts',(-6.07643638237694,0.709588701895203,
-4.32822109318138));
#164128=CARTESIAN_POINT('Ctrl Pts',(-6.12512903837064,0.69508689908163,
-4.23358346708829));
#164129=CARTESIAN_POINT('Ctrl Pts',(-6.17181637588744,0.680609078995239,
-4.13795044764606));
#164130=CARTESIAN_POINT('Ctrl Pts',(-5.70977404121975,0.562053379367947,
-4.56777900307571));
#164131=CARTESIAN_POINT('Ctrl Pts',(-5.66075968858094,0.582224590114487,
-4.66133734899429));
#164132=CARTESIAN_POINT('Ctrl Pts',(-5.6095656720655,0.602198953299526,
-4.75377570448088));
#164133=CARTESIAN_POINT('Ctrl Pts',(-5.52965027461911,0.631811121650233,
-4.89047835301904));
#164134=CARTESIAN_POINT('Ctrl Pts',(-5.50254794981892,0.641604433065763,
-4.93563183327623));
#164135=CARTESIAN_POINT('Ctrl Pts',(-5.44493274063811,0.661914290831286,
-5.02914878027505));
#164136=CARTESIAN_POINT('Ctrl Pts',(-5.4165790761668,0.671620843889875,
-5.07380153903629));
#164137=CARTESIAN_POINT('Ctrl Pts',(-5.38983527320803,0.680609080021972,
-5.11503929875299));
#164138=CARTESIAN_POINT('Ctrl Pts',(-5.654242076,0.810731746,-4.537846025));
#164139=CARTESIAN_POINT('Ctrl Pts',(-5.903379066,0.745065281,-4.227416618));
#164140=CARTESIAN_POINT('Ctrl Pts',(-6.117034678,0.680609079,-3.891578954));
#164141=CARTESIAN_POINT('Ctrl Pts',(-5.69211725800001,0.810731746,-4.883625817));
#164142=CARTESIAN_POINT('Ctrl Pts',(-5.960238263,0.745065281,-4.571116985));
#164143=CARTESIAN_POINT('Ctrl Pts',(-6.19253614600001,0.680609079,-4.231134137));
#164144=CARTESIAN_POINT('Ctrl Pts',(-5.69496788857757,0.810731746,-4.90965052225889));
#164145=CARTESIAN_POINT('Ctrl Pts',(-5.96451770291355,0.745065281,-4.59698518480662));
#164146=CARTESIAN_POINT('Ctrl Pts',(-6.19821867429337,0.680609079,-4.25669035445733));
#164147=CARTESIAN_POINT('',(-6.14458988136026,0.680609081791273,-4.01550380117678));
#164148=CARTESIAN_POINT('Ctrl Pts',(-6.117034678,0.680609079,-3.891578954));
#164149=CARTESIAN_POINT('Ctrl Pts',(-6.327912933,0.745496505000001,-3.560106917));
#164150=CARTESIAN_POINT('Ctrl Pts',(-6.501737708,0.810723991,-3.207788456));
#164151=CARTESIAN_POINT('Ctrl Pts',(-6.45658986,0.680609079,-3.816077485));
#164152=CARTESIAN_POINT('Ctrl Pts',(-6.66337681600001,0.745496505000001,
-3.466205512));
#164153=CARTESIAN_POINT('Ctrl Pts',(-6.831145961,0.810723991,-3.096036961));
#164154=CARTESIAN_POINT('Ctrl Pts',(-6.48210289523078,0.680609079,-3.81040455835748));
#164155=CARTESIAN_POINT('Ctrl Pts',(-6.68858244477358,0.745496505000001,
-3.4591500760032));
#164156=CARTESIAN_POINT('Ctrl Pts',(-6.85589659008656,0.810723991,-3.08764032922948));
#164157=CARTESIAN_POINT('',(-6.36340617191394,0.680609080415348,-3.83679726143964));
#164158=CARTESIAN_POINT('',(-6.24095952935366,0.680609082082805,-3.86402377588782));
#164159=CARTESIAN_POINT('',(-6.74026278091922,0.767980175615045,-3.32965349430743));
#164160=CARTESIAN_POINT('Ctrl Pts',(-6.36340617240637,0.680609079133212,
-3.83679725446595));
#164161=CARTESIAN_POINT('Ctrl Pts',(-6.42954660781029,0.695136944914254,
-3.75523767683706));
#164162=CARTESIAN_POINT('Ctrl Pts',(-6.49396614771468,0.709660812589365,
-3.67229619395753));
#164163=CARTESIAN_POINT('Ctrl Pts',(-6.61967593729421,0.738780776744085,
-3.50323846473616));
#164164=CARTESIAN_POINT('Ctrl Pts',(-6.68093080659687,0.753373671673061,
-3.4171235537493));
#164165=CARTESIAN_POINT('Ctrl Pts',(-6.74035240571884,0.767949007805381,
-3.3297457456512));
#164166=CARTESIAN_POINT('Ctrl Pts',(-6.4996632263326,0.809946052740608,
-3.2119897183158));
#164167=CARTESIAN_POINT('Ctrl Pts',(-6.53776901585845,0.802922931466638,
-3.23066796985503));
#164168=CARTESIAN_POINT('Ctrl Pts',(-6.57593531355083,0.796078752499066,
-3.24935238013516));
#164169=CARTESIAN_POINT('Ctrl Pts',(-6.65607595132773,0.782074140053557,
-3.28854050775976));
#164170=CARTESIAN_POINT('Ctrl Pts',(-6.69811053569426,0.774939590261598,
-3.30906922110622));
#164171=CARTESIAN_POINT('Ctrl Pts',(-6.74014973236584,0.767997185222975,
-3.32957669279489));
#164172=CARTESIAN_POINT('Origin',(-9.28077059647592E-14,0.560925699999911,
-3.27429056090622E-14));
#164173=CARTESIAN_POINT('',(-6.91705977240974,0.68060908019651,-2.71444937956975));
#164174=CARTESIAN_POINT('',(-6.5582201603214,0.562053379605623,-3.23355422947506));
#164175=CARTESIAN_POINT('Ctrl Pts',(-6.91705977069972,0.68060907998662,
-2.71444937844625));
#164176=CARTESIAN_POINT('Ctrl Pts',(-6.89156286604869,0.671661524826028,
-2.75492824303347));
#164177=CARTESIAN_POINT('Ctrl Pts',(-6.86292705281543,0.661738573476922,
-2.79951652352871));
#164178=CARTESIAN_POINT('Ctrl Pts',(-6.80234183353219,0.641119488147585,
-2.89127058978293));
#164179=CARTESIAN_POINT('Ctrl Pts',(-6.77298491792337,0.631275792530207,
-2.93471628064139));
#164180=CARTESIAN_POINT('Ctrl Pts',(-6.68333784270071,0.601654471575429,
-3.06439195463014));
#164181=CARTESIAN_POINT('Ctrl Pts',(-6.62167681188939,0.581858135004092,
-3.1496375100711));
#164182=CARTESIAN_POINT('Ctrl Pts',(-6.55822016075729,0.562053380204891,
-3.23355422994611));
#164183=CARTESIAN_POINT('Ctrl Pts',(-6.7403758294726,0.767963166007114,
-3.32973029581996));
#164184=CARTESIAN_POINT('Ctrl Pts',(-6.77421993302505,0.75333360253631,
-3.2281885891875));
#164185=CARTESIAN_POINT('Ctrl Pts',(-6.80592055292293,0.738713518224552,
-3.12594294066681));
#164186=CARTESIAN_POINT('Ctrl Pts',(-6.86481227006701,0.709588701971743,
-2.92077548577845));
#164187=CARTESIAN_POINT('Ctrl Pts',(-6.89202222679128,0.695086899117976,
-2.81788295276974));
#164188=CARTESIAN_POINT('Ctrl Pts',(-6.91705976808422,0.680609078997742,
-2.71444938240418));
#164189=CARTESIAN_POINT('Ctrl Pts',(-6.55822016004584,0.562053379347851,
-3.23355422945103));
#164190=CARTESIAN_POINT('Ctrl Pts',(-6.53046401461873,0.582224590123798,
-3.33546187009727));
#164191=CARTESIAN_POINT('Ctrl Pts',(-6.50033839978795,0.602198953325635,
-3.43674426839289));
#164192=CARTESIAN_POINT('Ctrl Pts',(-6.45167840855641,0.631811121666125,
-3.58743033294494));
#164193=CARTESIAN_POINT('Ctrl Pts',(-6.43491638461924,0.641604433068652,
-3.63735434851988));
#164194=CARTESIAN_POINT('Ctrl Pts',(-6.39875152628777,0.661914313305449,
-3.74107060286569));
#164195=CARTESIAN_POINT('Ctrl Pts',(-6.38065978734003,0.671620858343132,
-3.79077456868463));
#164196=CARTESIAN_POINT('Ctrl Pts',(-6.36340616973765,0.680609080062905,
-3.83679726069259));
#164197=CARTESIAN_POINT('Ctrl Pts',(-6.49755179600001,0.810731746,-3.216258799));
#164198=CARTESIAN_POINT('Ctrl Pts',(-6.674130955,0.745065281,-2.85952997));
#164199=CARTESIAN_POINT('Ctrl Pts',(-6.810596247,0.680609079,-2.485614363));
#164200=CARTESIAN_POINT('Ctrl Pts',(-6.608873911,0.810731746,-3.545812407));
#164201=CARTESIAN_POINT('Ctrl Pts',(-6.803546235,0.745065281,-3.182971767));
#164202=CARTESIAN_POINT('Ctrl Pts',(-6.95732686000001,0.680609079,-2.80100035));
#164203=CARTESIAN_POINT('Ctrl Pts',(-6.61725243779714,0.810731746,-3.57061586798096));
#164204=CARTESIAN_POINT('Ctrl Pts',(-6.81328652237631,0.745065281,-3.20731522978346));
#164205=CARTESIAN_POINT('Ctrl Pts',(-6.96837036535365,0.680609079,-2.8247375018096));
#164206=CARTESIAN_POINT('',(-6.86414740406235,0.680609081791274,-2.60071836199947));
#164207=CARTESIAN_POINT('Ctrl Pts',(-6.810596247,0.680609079,-2.485614363));
#164208=CARTESIAN_POINT('Ctrl Pts',(-6.945287596,0.745496505000001,-2.116559367));
#164209=CARTESIAN_POINT('Ctrl Pts',(-7.03931039,0.810723991,-1.735110727));
#164210=CARTESIAN_POINT('Ctrl Pts',(-7.125982234,0.680609079,-2.33888375));
#164211=CARTESIAN_POINT('Ctrl Pts',(-7.25272249400001,0.745496505000001,
-1.952738506));
#164212=CARTESIAN_POINT('Ctrl Pts',(-7.33699399300001,0.810723991,-1.555158883));
#164213=CARTESIAN_POINT('Ctrl Pts',(-7.14967927697468,0.680609079,-2.32785890493623));
#164214=CARTESIAN_POINT('Ctrl Pts',(-7.27582211887275,0.745496505000001,
-1.94042955714596));
#164215=CARTESIAN_POINT('Ctrl Pts',(-7.35936093834291,0.810723991,-1.54163790630347));
#164216=CARTESIAN_POINT('',(-7.03943126796915,0.680609080398537,-2.37915084812029));
#164217=CARTESIAN_POINT('',(-6.92454921546236,0.680609082082805,-2.43259874169282));
#164218=CARTESIAN_POINT('',(-7.29845626022657,0.767980175663714,-1.80285078869209));
#164219=CARTESIAN_POINT('Ctrl Pts',(-7.03943126697314,0.680609079127621,
-2.37915084103021));
#164220=CARTESIAN_POINT('Ctrl Pts',(-7.08649247720474,0.695136944835417,
-2.28527984298937));
#164221=CARTESIAN_POINT('Ctrl Pts',(-7.13157595674395,0.709660812421988,
-2.19042918962929));
#164222=CARTESIAN_POINT('Ctrl Pts',(-7.21800430741299,0.73878077676706,
-1.99830004607331));
#164223=CARTESIAN_POINT('Ctrl Pts',(-7.25931491163413,0.7533736717087,-1.9010304675125));
#164224=CARTESIAN_POINT('Ctrl Pts',(-7.29856362095871,0.767949007853029,
-1.80292161657032));
#164225=CARTESIAN_POINT('Ctrl Pts',(-7.03818755585394,0.80994605260326,
-1.73965971901071));
#164226=CARTESIAN_POINT('Ctrl Pts',(-7.0794177252991,0.802922931357737,
-1.74970966491208));
#164227=CARTESIAN_POINT('Ctrl Pts',(-7.1207083119314,0.796078752449335,
-1.7597526181006));
#164228=CARTESIAN_POINT('Ctrl Pts',(-7.20739959525797,0.782074140048543,
-1.78079668077467));
#164229=CARTESIAN_POINT('Ctrl Pts',(-7.2528645008597,0.774939590288263,
-1.791809251067));
#164230=CARTESIAN_POINT('Ctrl Pts',(-7.29832934463069,0.767997185271285,
-1.80280008485094));
#164231=CARTESIAN_POINT('Origin',(-1.32272665043232E-13,0.560925699999955,
-3.29597460435593E-14));
#164232=CARTESIAN_POINT('',(-7.33886913689214,0.680609080243553,-1.16402367627227));
#164233=CARTESIAN_POINT('',(-7.10001119469846,0.562053379812254,-1.74813204992909));
#164234=CARTESIAN_POINT('Ctrl Pts',(-7.33886913513934,0.680609080018306,
-1.16402367559671));
#164235=CARTESIAN_POINT('Ctrl Pts',(-7.32267009318878,0.671661524821512,
-1.20903724808586));
#164236=CARTESIAN_POINT('Ctrl Pts',(-7.30428893170297,0.661738573525927,
-1.25873893268598));
#164237=CARTESIAN_POINT('Ctrl Pts',(-7.26484457355725,0.641119488408449,
-1.36137187037028));
#164238=CARTESIAN_POINT('Ctrl Pts',(-7.24551354579363,0.631275792887089,
-1.41011269380347));
#164239=CARTESIAN_POINT('Ctrl Pts',(-7.1858388065163,0.601654472133851,
-1.55602809298206));
#164240=CARTESIAN_POINT('Ctrl Pts',(-7.14394465112516,0.581858135634878,
-1.65253595324458));
#164241=CARTESIAN_POINT('Ctrl Pts',(-7.10001119570797,0.562053380932133,
-1.74813205062504));
#164242=CARTESIAN_POINT('Ctrl Pts',(-7.29858317582244,0.767963166056144,
-1.80290149253324));
#164243=CARTESIAN_POINT('Ctrl Pts',(-7.30980755765121,0.753333602557733,
-1.6964582926769));
#164244=CARTESIAN_POINT('Ctrl Pts',(-7.3187872425921,0.738713518228104,
-1.58978839432786));
#164245=CARTESIAN_POINT('Ctrl Pts',(-7.33219716607111,0.709588701809224,
-1.37675766104373));
#164246=CARTESIAN_POINT('Ctrl Pts',(-7.33665211594474,0.695086899044866,
-1.270421362579));
#164247=CARTESIAN_POINT('Ctrl Pts',(-7.33886913326281,0.680609078992077,
-1.16402368087677));
#164248=CARTESIAN_POINT('Ctrl Pts',(-7.10001119357155,0.562053378727583,
-1.74813205008095));
#164249=CARTESIAN_POINT('Ctrl Pts',(-7.09481110174453,0.582224589605302,
-1.85362389826389));
#164250=CARTESIAN_POINT('Ctrl Pts',(-7.08716252876118,0.602198952927782,
-1.95901448777532));
#164251=CARTESIAN_POINT('Ctrl Pts',(-7.07203310580689,0.631811365744268,
-2.11663935704751));
#164252=CARTESIAN_POINT('Ctrl Pts',(-7.06639500129622,0.64160491886239,
-2.16900081468051));
#164253=CARTESIAN_POINT('Ctrl Pts',(-7.05337152457618,0.661914791451309,
-2.27806659903441));
#164254=CARTESIAN_POINT('Ctrl Pts',(-7.04638780387179,0.671621091156144,
-2.33049638581521));
#164255=CARTESIAN_POINT('Ctrl Pts',(-7.03943126560501,0.680609080016027,
-2.37915084785294));
#164256=CARTESIAN_POINT('Ctrl Pts',(-7.037043215,0.810731746,-1.744282886));
#164257=CARTESIAN_POINT('Ctrl Pts',(-7.13280789900001,0.745065281,-1.357934879));
#164258=CARTESIAN_POINT('Ctrl Pts',(-7.18570190500001,0.680609079,-0.963425207));
#164259=CARTESIAN_POINT('Ctrl Pts',(-7.21660696600001,0.810731746,-2.042200749));
#164260=CARTESIAN_POINT('Ctrl Pts',(-7.328727947,0.745065281,-1.645994327));
#164261=CARTESIAN_POINT('Ctrl Pts',(-7.396800703,0.680609079,-1.239894901));
#164262=CARTESIAN_POINT('Ctrl Pts',(-7.2301216182923,0.810731746,-2.06462318285809));
#164263=CARTESIAN_POINT('Ctrl Pts',(-7.34347363654515,0.745065281,-1.66767477897067));
#164264=CARTESIAN_POINT('Ctrl Pts',(-7.41268880312268,0.680609079,-1.26070306391127));
#164265=CARTESIAN_POINT('',(-7.26274502348097,0.680609081791273,-1.06432622257033));
#164266=CARTESIAN_POINT('Ctrl Pts',(-7.185701905,0.680609079,-0.963425207));
#164267=CARTESIAN_POINT('Ctrl Pts',(-7.237908331,0.745496505000001,-0.574043853));
#164268=CARTESIAN_POINT('Ctrl Pts',(-7.247732742,0.810723991,-0.181301149));
#164269=CARTESIAN_POINT('Ctrl Pts',(-7.462171599,0.680609079,-0.75232641));
#164270=CARTESIAN_POINT('Ctrl Pts',(-7.502938928,0.745496505,-0.347963618));
#164271=CARTESIAN_POINT('Ctrl Pts',(-7.49977234,0.810723991,0.058436696));
#164272=CARTESIAN_POINT('Ctrl Pts',(-7.48294460305386,0.680609079,-0.736465155544213));
#164273=CARTESIAN_POINT('Ctrl Pts',(-7.522852436733,0.745496505,-0.330976708620506));
#164274=CARTESIAN_POINT('Ctrl Pts',(-7.51870974870921,0.810723991,0.0764497923144575));
#164275=CARTESIAN_POINT('',(-7.28559392484547,0.680609082082805,-0.887152541785874));
#164276=CARTESIAN_POINT('Ctrl Pts',(-7.24761405796479,0.809946052533277,
-0.185985164613406));
#164277=CARTESIAN_POINT('Ctrl Pts',(-7.29004073015667,0.802922931301267,
-0.186936880615135));
#164278=CARTESIAN_POINT('Ctrl Pts',(-7.33252490372907,0.796078752413943,
-0.187868779482898));
#164279=CARTESIAN_POINT('Ctrl Pts',(-7.42171324432903,0.782074140020066,
-0.189784780224056));
#164280=CARTESIAN_POINT('Ctrl Pts',(-7.46848258277582,0.774939590255079,
-0.190766271942571));
#164281=CARTESIAN_POINT('Ctrl Pts',(-7.51524718812475,0.767997185234041,
-0.191726548669481));
#164282=CARTESIAN_POINT('Ctrl Pts',(-7.247490315,0.810731746,-0.190746244));
#164283=CARTESIAN_POINT('Ctrl Pts',(-7.257962673,0.745065281,0.207155738));
#164284=CARTESIAN_POINT('Ctrl Pts',(-7.224812129,0.680609079,0.603812641));
#164285=CARTESIAN_POINT('Ctrl Pts',(-7.48689949900001,0.810731746,-0.443098054));
#164286=CARTESIAN_POINT('Ctrl Pts',(-7.511226485,0.745065281,-0.032052021));
#164287=CARTESIAN_POINT('Ctrl Pts',(-7.49040836500001,0.680609079,0.379186656));
#164288=CARTESIAN_POINT('Ctrl Pts',(-7.50491834708005,0.810731746,-0.462091013464394));
#164289=CARTESIAN_POINT('Ctrl Pts',(-7.53028808521247,0.745065281,-0.0500557090664949));
#164290=CARTESIAN_POINT('Ctrl Pts',(-7.51039815046754,0.680609079,0.362280447846572));
#164291=CARTESIAN_POINT('',(-7.32174475728359,0.680609081791271,0.521832628067191));
#164292=CARTESIAN_POINT('Ctrl Pts',(-7.224812129,0.680609079,0.603812641));
#164293=CARTESIAN_POINT('Ctrl Pts',(-7.192092516,0.745496505000001,0.995313314));
#164294=CARTESIAN_POINT('Ctrl Pts',(-7.117259166,0.810723991,1.380985869));
#164295=CARTESIAN_POINT('Ctrl Pts',(-7.449438113,0.680609079,0.869408877));
#164296=CARTESIAN_POINT('Ctrl Pts',(-7.402326278,0.745496505000001,1.273081663));
#164297=CARTESIAN_POINT('Ctrl Pts',(-7.311869668,0.810723991,1.66929984));
#164298=CARTESIAN_POINT('Ctrl Pts',(-7.46631575460598,0.680609079,0.889364885665074));
#164299=CARTESIAN_POINT('Ctrl Pts',(-7.41812253640843,0.745496505000001,
1.2939522433328));
#164300=CARTESIAN_POINT('Ctrl Pts',(-7.32649204715234,0.810723991,1.69096278293244));
#164301=CARTESIAN_POINT('',(-7.38779429941529,0.680609080381726,0.79652164116979));
#164302=CARTESIAN_POINT('',(-7.30679216084005,0.680609082082804,0.700745251313463));
#164303=CARTESIAN_POINT('',(-7.3808969011864,0.767980175586769,1.42831918057935));
#164304=CARTESIAN_POINT('Ctrl Pts',(-7.38779429547985,0.680609079134893,
0.796521647287301));
#164305=CARTESIAN_POINT('Ctrl Pts',(-7.39109048409698,0.695136944972495,
0.901477148014278));
#164306=CARTESIAN_POINT('Ctrl Pts',(-7.39218038627761,0.709660812691676,
1.00649133226492));
#164307=CARTESIAN_POINT('Ctrl Pts',(-7.38994769944287,0.738780776730923,
1.21715334075509));
#164308=CARTESIAN_POINT('Ctrl Pts',(-7.38659775244984,0.753373671654153,
1.32277869175213));
#164309=CARTESIAN_POINT('Ctrl Pts',(-7.38102407900311,0.767949007775986,
1.42829997853959));
#164310=CARTESIAN_POINT('Ctrl Pts',(-7.11815018181283,0.809946052543578,
1.37638584987182));
#164311=CARTESIAN_POINT('Ctrl Pts',(-7.15978953283649,0.80292293127717,
1.38457686486786));
#164312=CARTESIAN_POINT('Ctrl Pts',(-7.20148078055054,0.79607875240361,
1.39279959469045));
#164313=CARTESIAN_POINT('Ctrl Pts',(-7.2889958308382,0.78207413997985,1.41010124571203));
#164314=CARTESIAN_POINT('Ctrl Pts',(-7.33488271979528,0.774939590214053,
1.4191967259174));
#164315=CARTESIAN_POINT('Ctrl Pts',(-7.38076042572,0.767997185194551,1.42831190766354));
#164316=CARTESIAN_POINT('Origin',(-3.9118014383277E-13,0.560925700000022,
4.52112305926455E-14));
#164317=CARTESIAN_POINT('',(-7.1493380926488,0.680609080220652,2.02507189136407));
#164318=CARTESIAN_POINT('',(-7.17781723606865,0.562053379630161,1.39465563927328));
#164319=CARTESIAN_POINT('Ctrl Pts',(-7.14933809065069,0.680609079955072,
2.02507189123788));
#164320=CARTESIAN_POINT('Ctrl Pts',(-7.15353694685268,0.671661524738824,
1.97741687808363));
#164321=CARTESIAN_POINT('Ctrl Pts',(-7.15772385219997,0.661738573386025,
1.92459080120668));
#164322=CARTESIAN_POINT('Ctrl Pts',(-7.1650195743026,0.641119488092974,
1.81488141282109));
#164323=CARTESIAN_POINT('Ctrl Pts',(-7.1679409492184,0.631275792509169,
1.76252855139152));
#164324=CARTESIAN_POINT('Ctrl Pts',(-7.17504990849782,0.601654471589547,
1.60504254835791));
#164325=CARTESIAN_POINT('Ctrl Pts',(-7.17755040153564,0.581858135011411,
1.49986348694586));
#164326=CARTESIAN_POINT('Ctrl Pts',(-7.1778172367069,0.562053380235276,
1.39465563916099));
#164327=CARTESIAN_POINT('Ctrl Pts',(-7.3810333766528,0.767963165978988,
1.42832645349517));
#164328=CARTESIAN_POINT('Ctrl Pts',(-7.34652601019056,0.753333602506669,
1.52964468079876));
#164329=CARTESIAN_POINT('Ctrl Pts',(-7.30988622378075,0.738713518198376,
1.630226130322));
#164330=CARTESIAN_POINT('Ctrl Pts',(-7.23260745793012,0.7095887019381,1.82919826716056));
#164331=CARTESIAN_POINT('Ctrl Pts',(-7.19200120797997,0.695086899113309,
1.92757706315618));
#164332=CARTESIAN_POINT('Ctrl Pts',(-7.14933809126938,0.680609078995803,
2.02507188553382));
#164333=CARTESIAN_POINT('Ctrl Pts',(-7.17781723583245,0.562053379369874,
1.39465563912421));
#164334=CARTESIAN_POINT('Ctrl Pts',(-7.21739263744442,0.582224590179618,
1.29673036939688));
#164335=CARTESIAN_POINT('Ctrl Pts',(-7.25470334031654,0.602198953386825,
1.1978689089469));
#164336=CARTESIAN_POINT('Ctrl Pts',(-7.30715677953051,0.631811121695678,
1.04846100592241));
#164337=CARTESIAN_POINT('Ctrl Pts',(-7.32402537537675,0.641604433053326,
0.998572898853101));
#164338=CARTESIAN_POINT('Ctrl Pts',(-7.35800117062359,0.661914304541736,
0.894119113304538));
#164339=CARTESIAN_POINT('Ctrl Pts',(-7.37367802588683,0.671620852112805,
0.843601466303717));
#164340=CARTESIAN_POINT('Ctrl Pts',(-7.38779429705825,0.680609079964133,
0.796521640383342));
#164341=CARTESIAN_POINT('Ctrl Pts',(-7.119052823,0.810731746,1.371709481));
#164342=CARTESIAN_POINT('Ctrl Pts',(-7.043743179,0.745065281,1.762559983));
#164343=CARTESIAN_POINT('Ctrl Pts',(-6.926098167,0.680609079,2.14281688));
#164344=CARTESIAN_POINT('Ctrl Pts',(-7.407112933,0.810731746,1.176723413));
#164345=CARTESIAN_POINT('Ctrl Pts',(-7.342508421,0.745065281,1.583389001));
#164346=CARTESIAN_POINT('Ctrl Pts',(-7.233772858,0.680609079,1.980537866));
#164347=CARTESIAN_POINT('Ctrl Pts',(-7.42879343523788,0.810731746,1.16204801804986));
#164348=CARTESIAN_POINT('Ctrl Pts',(-7.36499463229034,0.745065281,1.56990390972439));
#164349=CARTESIAN_POINT('Ctrl Pts',(-7.25692962839339,0.680609079,1.96832412864432));
#164350=CARTESIAN_POINT('',(-7.03838784414309,0.680609081791273,2.08359116440669));
#164351=CARTESIAN_POINT('Ctrl Pts',(-6.926098167,0.680609079,2.14281688));
#164352=CARTESIAN_POINT('Ctrl Pts',(-6.809982448,0.745496505000001,2.518130736));
#164353=CARTESIAN_POINT('Ctrl Pts',(-6.653990461,0.810723991,2.878699522));
#164354=CARTESIAN_POINT('Ctrl Pts',(-7.08837718100001,0.680609079,2.450491571));
#164355=CARTESIAN_POINT('Ctrl Pts',(-6.955589078,0.745496505000001,2.834599059));
#164356=CARTESIAN_POINT('Ctrl Pts',(-6.78207209700001,0.810723991,3.202108379));
#164357=CARTESIAN_POINT('Ctrl Pts',(-7.10057028074634,0.680609079,2.47360921328975));
#164358=CARTESIAN_POINT('Ctrl Pts',(-6.9665294708429,0.745496505000001,
2.85837742524577));
#164359=CARTESIAN_POINT('Ctrl Pts',(-6.79169572068939,0.810723991,3.22640823364571));
#164360=CARTESIAN_POINT('',(-7.04384316618178,0.680609080443654,2.36605680054315));
#164361=CARTESIAN_POINT('',(-6.98532390492157,0.680609082082805,2.25510654365759));
#164362=CARTESIAN_POINT('',(-6.90128923026718,0.76798017566292,2.98160052805709));
#164363=CARTESIAN_POINT('Ctrl Pts',(-7.04384316132244,0.680609079132359,
2.36605680523004));
#164364=CARTESIAN_POINT('Ctrl Pts',(-7.02449995680018,0.695136944893178,
2.4692670872381));
#164365=CARTESIAN_POINT('Ctrl Pts',(-7.00298943239152,0.709660812558863,
2.57206039456985));
#164366=CARTESIAN_POINT('Ctrl Pts',(-6.95552283949714,0.73878077680655,
2.77731728216213));
#164367=CARTESIAN_POINT('Ctrl Pts',(-6.9295448841773,0.753373671737292,
2.87975303164855));
#164368=CARTESIAN_POINT('Ctrl Pts',(-6.90141756260734,0.767949007858333,
2.98160911443684));
#164369=CARTESIAN_POINT('Ctrl Pts',(-6.65584951416331,0.809946052493932,
2.87439859193774));
#164370=CARTESIAN_POINT('Ctrl Pts',(-6.69475453452101,0.802922931174187,
2.89134933527514));
#164371=CARTESIAN_POINT('Ctrl Pts',(-6.73370341957374,0.796078752424214,
2.90834220783244));
#164372=CARTESIAN_POINT('Ctrl Pts',(-6.81545307337181,0.782074139996443,
2.9440525048495));
#164373=CARTESIAN_POINT('Ctrl Pts',(-6.85831189299476,0.774939590258443,
2.96279966249814));
#164374=CARTESIAN_POINT('Ctrl Pts',(-6.90115750899145,0.767997185272505,
2.98156408697476));
#164375=CARTESIAN_POINT('Origin',(1.39471767468535E-12,0.5609257,-6.60929644347164E-13));
#164376=CARTESIAN_POINT('',(-6.54685994543919,0.680609080168776,3.51462319239164));
#164377=CARTESIAN_POINT('',(-6.71019412140591,0.562053379647482,2.90506789591289));
#164378=CARTESIAN_POINT('Ctrl Pts',(-6.54685994337891,0.680609079914941,
3.51462319179381));
#164379=CARTESIAN_POINT('Ctrl Pts',(-6.56120505181549,0.671661524687892,
3.46898495629405));
#164380=CARTESIAN_POINT('Ctrl Pts',(-6.5766501145436,0.661738573380289,
3.41829398489273));
#164381=CARTESIAN_POINT('Ctrl Pts',(-6.60735954205801,0.641119488174177,
3.31271790618056));
#164382=CARTESIAN_POINT('Ctrl Pts',(-6.62146693454012,0.631275792558321,
3.26221703469908));
#164383=CARTESIAN_POINT('Ctrl Pts',(-6.66226452575419,0.601654471559685,
3.10994118271523));
#164384=CARTESIAN_POINT('Ctrl Pts',(-6.68731694782609,0.581858134941924,
3.0077586812105));
#164385=CARTESIAN_POINT('Ctrl Pts',(-6.71019412196659,0.562053380171493,
2.90506789593674));
#164386=CARTESIAN_POINT('Ctrl Pts',(-6.90142095154291,0.767963166053335,
2.98163696913943));
#164387=CARTESIAN_POINT('Ctrl Pts',(-6.84593992415734,0.753333602551252,
3.07316836886803));
#164388=CARTESIAN_POINT('Ctrl Pts',(-6.78853471705588,0.738713518208592,
3.16352180901211));
#164389=CARTESIAN_POINT('Ctrl Pts',(-6.67028955484223,0.709588701147707,
3.34122944213753));
#164390=CARTESIAN_POINT('Ctrl Pts',(-6.60948412490161,0.695086898711526,
3.42857905058261));
#164391=CARTESIAN_POINT('Ctrl Pts',(-6.54685994492008,0.680609078974318,
3.51462318693433));
#164392=CARTESIAN_POINT('Ctrl Pts',(-6.7101941212339,0.562053379422081,
2.90506789574284));
#164393=CARTESIAN_POINT('Ctrl Pts',(-6.76989531021481,0.582224590210383,
2.81793960600833));
#164394=CARTESIAN_POINT('Ctrl Pts',(-6.82758600118962,0.602198953412185,
2.72941016993194));
#164395=CARTESIAN_POINT('Ctrl Pts',(-6.91093139096509,0.631811121780453,
2.59477127936949));
#164396=CARTESIAN_POINT('Ctrl Pts',(-6.93813007693746,0.641604433206543,
2.54967577767941));
#164397=CARTESIAN_POINT('Ctrl Pts',(-6.99376615698564,0.661914357167096,
2.45496761047726));
#164398=CARTESIAN_POINT('Ctrl Pts',(-7.01993624758915,0.671620886225413,
2.4090011686433));
#164399=CARTESIAN_POINT('Ctrl Pts',(-7.04384316433259,0.680609080145789,
2.36605679945138));
#164400=CARTESIAN_POINT('Ctrl Pts',(-6.657736333,0.810731746,2.870025595));
#164401=CARTESIAN_POINT('Ctrl Pts',(-6.500166082,0.745065281,3.235548881));
#164402=CARTESIAN_POINT('Ctrl Pts',(-6.303527553,0.680609079,3.581625384));
#164403=CARTESIAN_POINT('Ctrl Pts',(-6.980977999,0.810731746,2.741522602));
#164404=CARTESIAN_POINT('Ctrl Pts',(-6.830462824,0.745065281,3.124792514));
#164405=CARTESIAN_POINT('Ctrl Pts',(-6.638894171,0.680609079,3.489281327));
#164406=CARTESIAN_POINT('Ctrl Pts',(-7.00530639894729,0.810731746,2.73185097690657));
#164407=CARTESIAN_POINT('Ctrl Pts',(-6.85532221586027,0.745065281,3.11645656762765));
#164408=CARTESIAN_POINT('Ctrl Pts',(-6.66413514105389,0.680609079,3.4823311612641));
#164409=CARTESIAN_POINT('',(-6.42592373772969,0.680609081791273,3.54792329397902));
#164410=CARTESIAN_POINT('Ctrl Pts',(-6.303527553,0.680609079,3.581625384));
#164411=CARTESIAN_POINT('Ctrl Pts',(-6.10944517000001,0.745496505000001,
3.923203163));
#164412=CARTESIAN_POINT('Ctrl Pts',(-5.87958855800001,0.810723991,4.241808386));
#164413=CARTESIAN_POINT('Ctrl Pts',(-6.39587161000001,0.680609079,3.916992003));
#164414=CARTESIAN_POINT('Ctrl Pts',(-6.18361626300001,0.745496505000001,
4.263573754));
#164415=CARTESIAN_POINT('Ctrl Pts',(-5.935152372,0.810723991,4.585189889));
#164416=CARTESIAN_POINT('Ctrl Pts',(-6.40281003213691,0.680609079,3.94219032381072));
#164417=CARTESIAN_POINT('Ctrl Pts',(-6.18918922968903,0.745496505000001,
4.28914805645182));
#164418=CARTESIAN_POINT('Ctrl Pts',(-5.93932725027147,0.810723991,4.61099042126185));
#164419=CARTESIAN_POINT('',(-6.37052975546877,0.680609080438259,3.8249577733505));
#164420=CARTESIAN_POINT('',(-6.33722966772581,0.68060908208268,3.70402156086006));
#164421=CARTESIAN_POINT('',(-6.09898494522745,0.767980175587502,4.39546554820092));
#164422=CARTESIAN_POINT('Ctrl Pts',(-6.37052974967258,0.680609079127803,
3.82495777693731));
#164423=CARTESIAN_POINT('Ctrl Pts',(-6.3294516189924,0.695136944801263,
3.92159684217388));
#164424=CARTESIAN_POINT('Ctrl Pts',(-6.28634647644809,0.709660812370041,
4.01736277163909));
#164425=CARTESIAN_POINT('Ctrl Pts',(-6.19586546215903,0.73878077674373,
4.20761695386509));
#164426=CARTESIAN_POINT('Ctrl Pts',(-6.14847419881717,0.753373671664429,
4.30207331998296));
#164427=CARTESIAN_POINT('Ctrl Pts',(-6.09910843141784,0.76794900777477,
4.39550152147733));
#164428=CARTESIAN_POINT('Ctrl Pts',(-5.8823287202579,0.80994605250801,4.23800765046644));
#164429=CARTESIAN_POINT('Ctrl Pts',(-5.91668025409125,0.802922931192687,
4.26292552407541));
#164430=CARTESIAN_POINT('Ctrl Pts',(-5.95106557075331,0.796078752403965,
4.2878939716896));
#164431=CARTESIAN_POINT('Ctrl Pts',(-6.02322730488898,0.782074139955645,
4.34034314065554));
#164432=CARTESIAN_POINT('Ctrl Pts',(-6.06105402446624,0.774939590200093,
4.36786537940377));
#164433=CARTESIAN_POINT('Ctrl Pts',(-6.09886413726223,0.767997185194965,
4.39540164292246));
#164434=CARTESIAN_POINT('Origin',(-1.0542781925249E-12,0.560925699999866,
7.22295487309843E-13));
#164435=CARTESIAN_POINT('',(-5.63825790320071,0.680609080157228,4.83983461982158));
#164436=CARTESIAN_POINT('',(-5.92880978678887,0.562053379604336,4.27964240775555));
#164437=CARTESIAN_POINT('Ctrl Pts',(-5.6382579012457,0.680609079874176,
4.83983461876012));
#164438=CARTESIAN_POINT('Ctrl Pts',(-5.66207850044105,0.671661524698012,
4.7983471543782));
#164439=CARTESIAN_POINT('Ctrl Pts',(-5.68805952660668,0.661738573402297,
4.75216154169928));
#164440=CARTESIAN_POINT('Ctrl Pts',(-5.74074672097875,0.641119488182738,
4.65565539206355));
#164441=CARTESIAN_POINT('Ctrl Pts',(-5.76538048503894,0.631275792582272,
4.60936787529185));
#164442=CARTESIAN_POINT('Ctrl Pts',(-5.83795905812051,0.601654471648306,
4.46942242443583));
#164443=CARTESIAN_POINT('Ctrl Pts',(-5.8843919857667,0.581858135073001,
4.37501442338295));
#164444=CARTESIAN_POINT('Ctrl Pts',(-5.9288097875027,0.562053380293896,
4.27964240794481));
#164445=CARTESIAN_POINT('Ctrl Pts',(-6.09910575319267,0.767963165980039,
4.39552945347938));
#164446=CARTESIAN_POINT('Ctrl Pts',(-6.02524529610966,0.753333602494622,
4.47299411909348));
#164447=CARTESIAN_POINT('Ctrl Pts',(-5.94975887205415,0.738713518171871,
4.54889472340646));
#164448=CARTESIAN_POINT('Ctrl Pts',(-5.79607632924243,0.709588701400169,
4.69702843502404));
#164449=CARTESIAN_POINT('Ctrl Pts',(-5.71791491197682,0.695086898841296,
4.7692644888865));
#164450=CARTESIAN_POINT('Ctrl Pts',(-5.63825790391852,0.68060907898151,
4.83983461427586));
#164451=CARTESIAN_POINT('Ctrl Pts',(-5.92880978661593,0.562053379307726,
4.27964240748837));
#164452=CARTESIAN_POINT('Ctrl Pts',(-6.00584520189072,0.582224590082771,
4.20738511946269));
#164453=CARTESIAN_POINT('Ctrl Pts',(-6.08121832855712,0.602198953299093,
4.13332724547259));
#164454=CARTESIAN_POINT('Ctrl Pts',(-6.19155853115221,0.631811121691396,
4.01975293231709));
#164455=CARTESIAN_POINT('Ctrl Pts',(-6.22781552682973,0.641604433120965,
3.98155865187309));
#164456=CARTESIAN_POINT('Ctrl Pts',(-6.30251013258213,0.661914305404527,
3.90102502652879));
#164457=CARTESIAN_POINT('Ctrl Pts',(-6.33794987209892,0.671620853463615,
3.86175899060336));
#164458=CARTESIAN_POINT('Ctrl Pts',(-6.37052975388443,0.680609080131929,
3.82495777187308));
#164459=CARTESIAN_POINT('Ctrl Pts',(-5.885111492,0.810731746,4.234142502));
#164460=CARTESIAN_POINT('Ctrl Pts',(-5.652648444,0.745065281,4.557247111));
#164461=CARTESIAN_POINT('Ctrl Pts',(-5.38621099600001,0.680609079,4.852961066));
#164462=CARTESIAN_POINT('Ctrl Pts',(-6.22842029200001,0.810731746,4.17813124));
#164463=CARTESIAN_POINT('Ctrl Pts',(-5.999032377,0.745065281,4.520084201));
#164464=CARTESIAN_POINT('Ctrl Pts',(-5.733588172,0.680609079,4.83486987100001));
#164465=CARTESIAN_POINT('Ctrl Pts',(-6.25425902122499,0.810731746,4.17391561886717));
#164466=CARTESIAN_POINT('Ctrl Pts',(-6.02510255245916,0.745065281,4.51728717870199));
#164467=CARTESIAN_POINT('Ctrl Pts',(-5.75973310271428,0.680609079,4.83350825868783));
#164468=CARTESIAN_POINT('',(-5.512990579203,0.680609081791274,4.84635847385095));
#164469=CARTESIAN_POINT('Ctrl Pts',(-5.386210996,0.680609079,4.852961066));
#164470=CARTESIAN_POINT('Ctrl Pts',(-5.123237026,0.745496505000001,5.144830971));
#164471=CARTESIAN_POINT('Ctrl Pts',(-4.830263629,0.810723991,5.406575004));
#164472=CARTESIAN_POINT('Ctrl Pts',(-5.40430219,0.680609079,5.200338242));
#164473=CARTESIAN_POINT('Ctrl Pts',(-5.122504424,0.745496505000001,5.493188479));
#164474=CARTESIAN_POINT('Ctrl Pts',(-4.810711519,0.810723991,5.75387301500001));
#164475=CARTESIAN_POINT('Ctrl Pts',(-5.40566150155319,0.680609079,5.22643899624792));
#164476=CARTESIAN_POINT('Ctrl Pts',(-5.12244937874635,0.745496505000001,
5.51936289210171));
#164477=CARTESIAN_POINT('Ctrl Pts',(-4.80924243912545,0.810723991,5.77996782105572));
#164478=CARTESIAN_POINT('',(-5.3993374531762,0.680609080406291,5.10500797269187));
#164479=CARTESIAN_POINT('',(-5.39281361407524,0.680609082082614,4.97974064684016));
#164480=CARTESIAN_POINT('',(-5.01149890225682,0.767980175651308,5.60380348523056));
#164481=CARTESIAN_POINT('Ctrl Pts',(-5.39933744653031,0.680609079136191,
5.10500797506104));
#164482=CARTESIAN_POINT('Ctrl Pts',(-5.33844515663971,0.695136944985681,
5.19055708977868));
#164483=CARTESIAN_POINT('Ctrl Pts',(-5.27576094361556,0.709660812727179,
5.27481773443682));
#164484=CARTESIAN_POINT('Ctrl Pts',(-5.14649630147005,0.738780776769514,
5.44117313407239));
#164485=CARTESIAN_POINT('Ctrl Pts',(-5.07990769298335,0.753373671694956,
5.5232334420372));
#164486=CARTESIAN_POINT('Ctrl Pts',(-5.01161176825204,0.767949007809954,
5.60386516329118));
#164487=CARTESIAN_POINT('Ctrl Pts',(-4.833756773168,0.80994605261842,5.40345218029789));
#164488=CARTESIAN_POINT('Ctrl Pts',(-4.86194858070813,0.802922931354232,
5.43517205213695));
#164489=CARTESIAN_POINT('Ctrl Pts',(-4.89016251007618,0.796078752434557,
5.46694857875674));
#164490=CARTESIAN_POINT('Ctrl Pts',(-4.94936212170107,0.782074140029164,
5.53368415521112));
#164491=CARTESIAN_POINT('Ctrl Pts',(-4.98038800577312,0.774939590264265,
5.56869456611257));
#164492=CARTESIAN_POINT('Ctrl Pts',(-5.01139465640152,0.767997185250274,
5.60371510391402));
#164493=CARTESIAN_POINT('Origin',(-1.02652261690928E-12,0.5609257,1.19218870886506E-12));
#164494=CARTESIAN_POINT('',(-4.46601718720579,0.680609080243162,5.93874075972541));
#164495=CARTESIAN_POINT('',(-4.87020089678171,0.562053379627107,5.45410559592523));
#164496=CARTESIAN_POINT('Ctrl Pts',(-4.46601718577088,0.68060908001573,
5.9387407584783));
#164497=CARTESIAN_POINT('Ctrl Pts',(-4.498199451366,0.671661524767342,5.9033439723503));
#164498=CARTESIAN_POINT('Ctrl Pts',(-4.53350159734835,0.661738573394949,
5.863823305951));
#164499=CARTESIAN_POINT('Ctrl Pts',(-4.60570296414624,0.641119488096921,
5.78089960549891));
#164500=CARTESIAN_POINT('Ctrl Pts',(-4.63971125229766,0.63127579251093,
5.74098979630539));
#164501=CARTESIAN_POINT('Ctrl Pts',(-4.74067711382384,0.601654471587487,
5.61991844014854));
#164502=CARTESIAN_POINT('Ctrl Pts',(-4.80631939498106,0.581858135014818,
5.53769935257863));
#164503=CARTESIAN_POINT('Ctrl Pts',(-4.8702008973831,0.562053380258828,
5.45410559623515));
#164504=CARTESIAN_POINT('Ctrl Pts',(-5.01160314811211,0.767963166052343,
5.60389186654709));
#164505=CARTESIAN_POINT('Ctrl Pts',(-4.92281689431306,0.753333602579392,
5.66366763626224));
#164506=CARTESIAN_POINT('Ctrl Pts',(-4.83277891469519,0.738713518264693,
5.72156637672409));
#164507=CARTESIAN_POINT('Ctrl Pts',(-4.65084501993623,0.709588702238808,
5.83319959762432));
#164508=CARTESIAN_POINT('Ctrl Pts',(-4.55898235436246,0.695086899255936,
5.88694442006499));
#164509=CARTESIAN_POINT('Ctrl Pts',(-4.4660171894992,0.680609079003592,
5.93874075440816));
#164510=CARTESIAN_POINT('Ctrl Pts',(-4.87020089667959,0.562053379355376,
5.45410559565212));
#164511=CARTESIAN_POINT('Ctrl Pts',(-4.96096844761636,0.582224590156947,
5.40009798016166));
#164512=CARTESIAN_POINT('Ctrl Pts',(-5.05049964606646,0.602198953364876,
5.34397453247609));
#164513=CARTESIAN_POINT('Ctrl Pts',(-5.18267527581382,0.631811121689457,
5.25677540579544));
#164514=CARTESIAN_POINT('Ctrl Pts',(-5.22629524420352,0.641604433078536,
5.22726826882805));
#164515=CARTESIAN_POINT('Ctrl Pts',(-5.31655605975392,0.661914345679666,
5.16467448282507));
#164516=CARTESIAN_POINT('Ctrl Pts',(-5.3596082152923,0.671620878862863,
5.13394499620549));
#164517=CARTESIAN_POINT('Ctrl Pts',(-5.39933745184495,0.680609080035479,
5.10500797074894));
#164518=CARTESIAN_POINT('Ctrl Pts',(-4.837305378,0.810731746,5.400275611));
#164519=CARTESIAN_POINT('Ctrl Pts',(-4.540819247,0.745065281,5.66585353));
#164520=CARTESIAN_POINT('Ctrl Pts',(-4.217041199,0.680609079,5.897377682));
#164521=CARTESIAN_POINT('Ctrl Pts',(-5.184628575,0.810731746,5.419375106));
#164522=CARTESIAN_POINT('Ctrl Pts',(-4.88709384300001,0.745065281,5.704021776));
#164523=CARTESIAN_POINT('Ctrl Pts',(-4.56018596200001,0.680609079,5.954385274));
#164524=CARTESIAN_POINT('Ctrl Pts',(-5.21076944247076,0.810731746,5.42081260678274));
#164525=CARTESIAN_POINT('Ctrl Pts',(-4.91315578876324,0.745065281,5.70689446365488));
#164526=CARTESIAN_POINT('Ctrl Pts',(-4.58601234460372,0.680609079,5.95867588263245));
#164527=CARTESIAN_POINT('',(-4.34227610870454,0.680609081791272,5.91818331762197));
#164528=CARTESIAN_POINT('Ctrl Pts',(-4.217041199,0.680609079,5.897377682));
#164529=CARTESIAN_POINT('Ctrl Pts',(-3.897472013,0.745496505000001,6.125892201));
#164530=CARTESIAN_POINT('Ctrl Pts',(-3.555080941,0.810723991,6.318536183));
#164531=CARTESIAN_POINT('Ctrl Pts',(-4.160033607,0.680609079,6.240522445));
#164532=CARTESIAN_POINT('Ctrl Pts',(-3.821869971,0.745496505000001,6.465947816));
#164533=CARTESIAN_POINT('Ctrl Pts',(-3.461327142,0.810723991,6.653511435));
#164534=CARTESIAN_POINT('Ctrl Pts',(-4.15575024804733,0.680609079,6.2663051897379));
#164535=CARTESIAN_POINT('Ctrl Pts',(-3.81618948754017,0.745496505000001,
6.4914984525348));
#164536=CARTESIAN_POINT('Ctrl Pts',(-3.45428279649785,0.810723991,6.67868035012586));
#164537=CARTESIAN_POINT('',(-4.17567813270082,0.680609080429674,6.14635367235228));
#164538=CARTESIAN_POINT('',(-4.19623558931298,0.680609082082512,6.02261259398236));
#164539=CARTESIAN_POINT('',(-3.68968074061468,0.767980175621886,6.55011379903614));
#164540=CARTESIAN_POINT('Ctrl Pts',(-4.17567812587055,0.680609079129443,
6.14635367319251));
#164541=CARTESIAN_POINT('Ctrl Pts',(-4.09781893374167,0.695136944833282,
6.21681265412599));
#164542=CARTESIAN_POINT('Ctrl Pts',(-4.01848669565778,0.709660812426448,
6.28562807827921));
#164543=CARTESIAN_POINT('Ctrl Pts',(-3.85648269393038,0.73878077672691,
6.42030610538059));
#164544=CARTESIAN_POINT('Ctrl Pts',(-3.77381034952353,0.753373671653238,
6.48613330649975));
#164545=CARTESIAN_POINT('Ctrl Pts',(-3.68977770889971,0.767949007783995,
6.55019829795612));
#164546=CARTESIAN_POINT('Ctrl Pts',(-3.55916373241255,0.809946052468782,
6.31623729349231));
#164547=CARTESIAN_POINT('Ctrl Pts',(-3.57987759654876,0.80292293116247,
6.35327597790358));
#164548=CARTESIAN_POINT('Ctrl Pts',(-3.60060088545173,0.796078752430467,
6.39037474676793));
#164549=CARTESIAN_POINT('Ctrl Pts',(-3.64407026689995,0.782074139979874,
6.46827624924014));
#164550=CARTESIAN_POINT('Ctrl Pts',(-3.66684457949304,0.774939590228884,
6.50913778396703));
#164551=CARTESIAN_POINT('Ctrl Pts',(-3.6895979313482,0.767997185221761,
6.55000507424667));
#164552=CARTESIAN_POINT('Origin',(-3.39355279987963E-13,0.560925700000022,
7.31619625993218E-13));
#164553=CARTESIAN_POINT('',(-3.08495047167216,0.680609080268415,6.75995798165497));
#164554=CARTESIAN_POINT('',(-3.58386682551787,0.562053379558525,6.37354086850205));
#164555=CARTESIAN_POINT('Ctrl Pts',(-3.08495047063983,0.680609080090048,
6.75995798025519));
#164556=CARTESIAN_POINT('Ctrl Pts',(-3.12398959543952,0.671661524832574,
6.73230698711131));
#164557=CARTESIAN_POINT('Ctrl Pts',(-3.16696217186839,0.661738573458893,
6.70129920981335));
#164558=CARTESIAN_POINT('Ctrl Pts',(-3.25530165505472,0.641119488173938,
6.63583537910247));
#164559=CARTESIAN_POINT('Ctrl Pts',(-3.29709427764183,0.63127579255954,
6.60416941568338));
#164560=CARTESIAN_POINT('Ctrl Pts',(-3.42172637630531,0.601654471555052,
6.50763331609108));
#164561=CARTESIAN_POINT('Ctrl Pts',(-3.50350865092829,0.581858134924881,
6.44144761507033));
#164562=CARTESIAN_POINT('Ctrl Pts',(-3.58386682596175,0.562053380097039,
6.37354086887026));
#164563=CARTESIAN_POINT('Ctrl Pts',(-3.68976354988115,0.767963166022011,
6.5502225238256));
#164564=CARTESIAN_POINT('Ctrl Pts',(-3.5902030457854,0.753333602537464,
6.58951434920594));
#164565=CARTESIAN_POINT('Ctrl Pts',(-3.48982358633362,0.738713518218971,
6.62670394518843));
#164566=CARTESIAN_POINT('Ctrl Pts',(-3.28814535830902,0.70958870162373,
6.69661683535173));
#164567=CARTESIAN_POINT('Ctrl Pts',(-3.18687684475388,0.695086898950739,
6.72935737524069));
#164568=CARTESIAN_POINT('Ctrl Pts',(-3.08495047502156,0.680609078987373,
6.75995797704349));
#164569=CARTESIAN_POINT('Ctrl Pts',(-3.5838668254829,0.562053379326887,
6.37354086825596));
#164570=CARTESIAN_POINT('Ctrl Pts',(-3.68412232234193,0.582224590112365,
6.34030826119271));
#164571=CARTESIAN_POINT('Ctrl Pts',(-3.78362521335049,0.602198953309315,
6.30474350967115));
#164572=CARTESIAN_POINT('Ctrl Pts',(-3.93145588525735,0.63181112170061,
6.247996903327));
#164573=CARTESIAN_POINT('Ctrl Pts',(-3.98039920558153,0.641604433162138,
6.22855663050104));
#164574=CARTESIAN_POINT('Ctrl Pts',(-4.08200559680042,0.661914347710843,
6.18682965572533));
#164575=CARTESIAN_POINT('Ctrl Pts',(-4.13065714833452,0.671620880942573,
6.16607354790408));
#164576=CARTESIAN_POINT('Ctrl Pts',(-4.17567813186649,0.680609080106447,
6.14635367030016));
#164577=CARTESIAN_POINT('Ctrl Pts',(-3.563312241,0.810731746,6.313897835));
#164578=CARTESIAN_POINT('Ctrl Pts',(-3.216666389,0.745065281,6.509530936));
#164579=CARTESIAN_POINT('Ctrl Pts',(-2.850687243,0.680609079,6.666039472));
#164580=CARTESIAN_POINT('Ctrl Pts',(-3.898409388,0.810731746,6.407215015));
#164581=CARTESIAN_POINT('Ctrl Pts',(-3.546640232,0.745065281,6.621245631));
#164582=CARTESIAN_POINT('Ctrl Pts',(-3.173554525,0.680609079,6.79548023900001));
#164583=CARTESIAN_POINT('Ctrl Pts',(-3.92363007654055,0.810731746,6.41423842165485));
#164584=CARTESIAN_POINT('Ctrl Pts',(-3.57147532115351,0.745065281,6.62965370475778));
#164585=CARTESIAN_POINT('Ctrl Pts',(-3.19785474728526,0.680609079,6.80522244450126));
#164586=CARTESIAN_POINT('',(-2.96852163335115,0.680609081791273,6.71328048691971));
#164587=CARTESIAN_POINT('Ctrl Pts',(-2.850687243,0.680609079,6.666039472));
#164588=CARTESIAN_POINT('Ctrl Pts',(-2.48946554,0.745496505000001,6.82051352));
#164589=CARTESIAN_POINT('Ctrl Pts',(-2.11366662,0.810723991,6.93504963400001));
#164590=CARTESIAN_POINT('Ctrl Pts',(-2.721246476,0.680609079,6.988906754));
#164591=CARTESIAN_POINT('Ctrl Pts',(-2.342529127,0.745496505000001,7.13636662));
#164592=CARTESIAN_POINT('Ctrl Pts',(-1.950094955,0.810723991,7.242039054));
#164593=CARTESIAN_POINT('Ctrl Pts',(-2.71152073168206,0.680609079,7.01316591675172));
#164594=CARTESIAN_POINT('Ctrl Pts',(-2.33148881862611,0.745496505000001,
7.16009876068353));
#164595=CARTESIAN_POINT('Ctrl Pts',(-1.93780472968444,0.810723991,7.26510520754985));
#164596=CARTESIAN_POINT('',(-2.75676874420522,0.68060908040802,6.90030270532544));
#164597=CARTESIAN_POINT('',(-2.80344625281094,0.680609082082373,6.7838738706396));
#164598=CARTESIAN_POINT('',(-2.19533720895636,0.767980175607453,7.19014807126775));
#164599=CARTESIAN_POINT('Ctrl Pts',(-2.75676873714112,0.680609079124013,
6.90030270471387));
#164600=CARTESIAN_POINT('Ctrl Pts',(-2.66558325206307,0.69513694475478,
6.95237696872478));
#164601=CARTESIAN_POINT('Ctrl Pts',(-2.57331247625661,0.709660812263954,
7.00252944006454));
#164602=CARTESIAN_POINT('Ctrl Pts',(-2.38614424234407,0.738780776730211,
7.09923269868999));
#164603=CARTESIAN_POINT('Ctrl Pts',(-2.29125382900687,0.753373671657563,
7.14574878616535));
#164604=CARTESIAN_POINT('Ctrl Pts',(-2.19541374540066,0.767949007772609,
7.19025143996891));
#164605=CARTESIAN_POINT('Ctrl Pts',(-2.11814815146974,0.80994605258979,
6.93368216929435));
#164606=CARTESIAN_POINT('Ctrl Pts',(-2.13041551445766,0.8029229313052,6.9743077780005));
#164607=CARTESIAN_POINT('Ctrl Pts',(-2.14267916591134,0.796078752395621,
7.01499409375212));
#164608=CARTESIAN_POINT('Ctrl Pts',(-2.16838573688887,0.782074139977238,
7.10041893415635));
#164609=CARTESIAN_POINT('Ctrl Pts',(-2.18184357659784,0.774939590214724,
7.14522095300597));
#164610=CARTESIAN_POINT('Ctrl Pts',(-2.19527970834756,0.767997185208149,
7.19002408685864));
#164611=CARTESIAN_POINT('Origin',(-2.64545330086463E-14,0.5609257,1.60895602396849E-13));
#164612=CARTESIAN_POINT('',(-1.55963490112623,0.680609080260179,7.2650870814962));
#164613=CARTESIAN_POINT('',(-2.12995512369142,0.562053379543022,6.9949564542138));
#164614=CARTESIAN_POINT('Ctrl Pts',(-1.55963490040577,0.68060908007041,
7.2650870798815));
#164615=CARTESIAN_POINT('Ctrl Pts',(-1.60370545790053,0.671661524877215,
7.24647480959136));
#164616=CARTESIAN_POINT('Ctrl Pts',(-1.65233911476708,0.66173857351751,
7.22542981061857));
#164617=CARTESIAN_POINT('Ctrl Pts',(-1.75268605847454,0.64111948821144,
7.18048686545229));
#164618=CARTESIAN_POINT('Ctrl Pts',(-1.8003088388687,0.631275792597886,
7.1585454131383));
#164619=CARTESIAN_POINT('Ctrl Pts',(-1.94277951599448,0.60165447163943,
7.09105849111672));
#164620=CARTESIAN_POINT('Ctrl Pts',(-2.03687773564085,0.581858135058827,
7.0440009466781));
#164621=CARTESIAN_POINT('Ctrl Pts',(-2.12995512416222,0.56205338025852,
6.99495645481837));
#164622=CARTESIAN_POINT('Ctrl Pts',(-2.19539470956517,0.767963166006757,
7.19027205567687));
#164623=CARTESIAN_POINT('Ctrl Pts',(-2.08971529368618,0.753333602535716,
7.20724269465628));
#164624=CARTESIAN_POINT('Ctrl Pts',(-1.98368798634468,0.738713518218528,
7.2219842019864));
#164625=CARTESIAN_POINT('Ctrl Pts',(-1.77169567685954,0.709588701411639,
7.2469077103715));
#164626=CARTESIAN_POINT('Ctrl Pts',(-1.66575651738361,0.695086898844228,
7.25711305757202));
#164627=CARTESIAN_POINT('Ctrl Pts',(-1.5596349054588,0.680609078981565,
7.26508707768309));
#164628=CARTESIAN_POINT('Ctrl Pts',(-2.12995512371633,0.562053379235256,
6.99495645388449));
#164629=CARTESIAN_POINT('Ctrl Pts',(-2.23501073117867,0.582224590034869,
6.984052774955));
#164630=CARTESIAN_POINT('Ctrl Pts',(-2.33983267040083,0.602198953270739,
6.97070968781844));
#164631=CARTESIAN_POINT('Ctrl Pts',(-2.49640598601594,0.631811121639731,
6.94706901029063));
#164632=CARTESIAN_POINT('Ctrl Pts',(-2.54838412220583,0.641604433021573,
6.93860460746325));
#164633=CARTESIAN_POINT('Ctrl Pts',(-2.65658491108027,0.661914316173451,
6.91969558617028));
#164634=CARTESIAN_POINT('Ctrl Pts',(-2.70856101523815,0.671620860105384,
6.90988338572812));
#164635=CARTESIAN_POINT('Ctrl Pts',(-2.75676874381832,0.680609080045511,
6.90030270303855));
#164636=CARTESIAN_POINT('Ctrl Pts',(-2.122702584,0.810731746,6.932289213));
#164637=CARTESIAN_POINT('Ctrl Pts',(-1.742105785,0.745065281,7.04882990900001));
#164638=CARTESIAN_POINT('Ctrl Pts',(-1.35103832,0.680609079,7.123004665));
#164639=CARTESIAN_POINT('Ctrl Pts',(-2.429904911,0.810731746,7.09546067));
#164640=CARTESIAN_POINT('Ctrl Pts',(-2.040349667,0.745065281,7.2288674));
#164641=CARTESIAN_POINT('Ctrl Pts',(-1.638531205,0.680609079,7.3188261));
#164642=CARTESIAN_POINT('Ctrl Pts',(-2.45302612909604,0.810731746,7.10774157581601));
#164643=CARTESIAN_POINT('Ctrl Pts',(-2.06279663837835,0.745065281,7.24241770782328));
#164644=CARTESIAN_POINT('Ctrl Pts',(-1.66016901536446,0.680609079,7.33356436761252));
#164645=CARTESIAN_POINT('',(-1.45596238572947,0.680609081791274,7.19447212189389));
#164646=CARTESIAN_POINT('Ctrl Pts',(-1.35103832,0.680609079,7.123004665));
#164647=CARTESIAN_POINT('Ctrl Pts',(-0.965054425,0.745496505000001,7.196215207));
#164648=CARTESIAN_POINT('Ctrl Pts',(-0.573419596,0.810723991,7.227287871));
#164649=CARTESIAN_POINT('Ctrl Pts',(-1.155216884,0.680609079,7.410497551));
#164650=CARTESIAN_POINT('Ctrl Pts',(-0.753654224,0.745496505000001,7.47309685200001));
#164651=CARTESIAN_POINT('Ctrl Pts',(-0.347678495,0.810723991,7.491936977));
#164652=CARTESIAN_POINT('Ctrl Pts',(-1.14050351955617,0.680609079,7.43209880004164));
#164653=CARTESIAN_POINT('Ctrl Pts',(-0.737770323522364,0.745496505000001,
7.49390080806278));
#164654=CARTESIAN_POINT('Ctrl Pts',(-0.330717067503553,0.810723991,7.51182182120221));
#164655=CARTESIAN_POINT('',(-1.27957088547559,0.680609082082176,7.22792874414072));
#164656=CARTESIAN_POINT('Ctrl Pts',(-0.578090315820934,0.809946052643239,
7.22691577379934));
#164657=CARTESIAN_POINT('Ctrl Pts',(-0.581337569923514,0.802922931341175,
7.26922869880324));
#164658=CARTESIAN_POINT('Ctrl Pts',(-0.584568148992888,0.796078752436324,
7.31160011357802));
#164659=CARTESIAN_POINT('Ctrl Pts',(-0.5913098993982,0.782074139999187,
7.40055392161798));
#164660=CARTESIAN_POINT('Ctrl Pts',(-0.59482199270295,0.774939590230869,
7.44720153191403));
#164661=CARTESIAN_POINT('Ctrl Pts',(-0.598312645844489,0.76799718521972,
7.49384556457247));
#164662=CARTESIAN_POINT('Ctrl Pts',(-0.582837713,0.810731746,7.226534453));
#164663=CARTESIAN_POINT('Ctrl Pts',(-0.186086252,0.745065281,7.258533431));
#164664=CARTESIAN_POINT('Ctrl Pts',(0.211783654,0.680609079,7.246906077));
#164665=CARTESIAN_POINT('Ctrl Pts',(-0.847780781,0.810731746,7.451930471));
#164666=CARTESIAN_POINT('Ctrl Pts',(-0.438654618,0.745065281,7.498475363));
#164667=CARTESIAN_POINT('Ctrl Pts',(-0.026891988,0.680609079,7.499951788));
#164668=CARTESIAN_POINT('Ctrl Pts',(-0.867721406319764,0.810731746,7.46889463457459));
#164669=CARTESIAN_POINT('Ctrl Pts',(-0.457663876072119,0.745065281,7.51653430751449));
#164670=CARTESIAN_POINT('Ctrl Pts',(-0.0448556267017154,0.680609079,7.51899697287656));
#164671=CARTESIAN_POINT('',(0.124676045108029,0.680609081791274,7.33925823720938));
#164672=CARTESIAN_POINT('Ctrl Pts',(0.38842861563543,0.681884070047851,
7.42155191714904));
#164673=CARTESIAN_POINT('Ctrl Pts',(0.392458295317715,0.681246574523926,
7.42133662307453));
#164674=CARTESIAN_POINT('Ctrl Pts',(0.396487975,0.680609079,7.421121329));
#164675=CARTESIAN_POINT('Ctrl Pts',(0.402929351,0.679590053,7.420777185));
#164676=CARTESIAN_POINT('Ctrl Pts',(0.40937012,0.678571429,7.420421861));
#164677=CARTESIAN_POINT('Ctrl Pts',(0.808182013,0.615498301,7.398420191));
#164678=CARTESIAN_POINT('Ctrl Pts',(1.202338414,0.551245526,7.333800299));
#164679=CARTESIAN_POINT('Ctrl Pts',(0.203913492723899,0.681884070047851,
7.2471360750122));
#164680=CARTESIAN_POINT('Ctrl Pts',(0.207848573361949,0.681246574523926,
7.2470210760061));
#164681=CARTESIAN_POINT('Ctrl Pts',(0.211783654,0.680609079,7.246906077));
#164682=CARTESIAN_POINT('Ctrl Pts',(0.218073815,0.679590053,7.246722253));
#164683=CARTESIAN_POINT('Ctrl Pts',(0.224363648,0.678571429,7.24652751));
#164684=CARTESIAN_POINT('Ctrl Pts',(0.613829558,0.615498301,7.234469046));
#164685=CARTESIAN_POINT('Ctrl Pts',(0.999759533999999,0.551245526,7.180736792));
#164686=CARTESIAN_POINT('',(0.995066308632371,0.55202682598065,7.18138865692373));
#164687=CARTESIAN_POINT('Origin',(-0.0491214261700275,0.411147083219614,
-0.184599448970936));
#164688=CARTESIAN_POINT('Origin',(1.09128087012227,0.300047239099359,9.32655164468723));
#164689=CARTESIAN_POINT('Ctrl Pts',(0.837099778000001,0.551266351,7.384409824));
#164690=CARTESIAN_POINT('Ctrl Pts',(1.239349841,0.615380951,7.338810589));
#164691=CARTESIAN_POINT('Ctrl Pts',(1.634266632,0.680609079,7.24978738));
#164692=CARTESIAN_POINT('Ctrl Pts',(1.63822684695898,0.681263184913293,
7.2488946576544));
#164693=CARTESIAN_POINT('Ctrl Pts',(1.64218706191796,0.681917290826586,
7.2480019353088));
#164694=CARTESIAN_POINT('Ctrl Pts',(0.990426433,0.551266351,7.182030039));
#164695=CARTESIAN_POINT('Ctrl Pts',(1.381652286,0.615380951,7.12807866));
#164696=CARTESIAN_POINT('Ctrl Pts',(1.764702859,0.680609079,7.03195021400001));
#164697=CARTESIAN_POINT('Ctrl Pts',(1.76854407984401,0.681263184913293,
7.03098624052886));
#164698=CARTESIAN_POINT('Ctrl Pts',(1.77238530068803,0.681917290826586,
7.03002226705771));
#164699=CARTESIAN_POINT('Origin',(-0.0663475152002066,0.803452713883071,
-0.180685821127333));
#164700=CARTESIAN_POINT('Ctrl Pts',(1.97476165197866,0.681884070047877,
7.16453948434253));
#164701=CARTESIAN_POINT('Ctrl Pts',(1.97865083848933,0.681246574523938,
7.16346296267127));
#164702=CARTESIAN_POINT('Ctrl Pts',(1.982540025,0.680609079,7.16238644100001));
#164703=CARTESIAN_POINT('Ctrl Pts',(1.988756825,0.679590053,7.160665639));
#164704=CARTESIAN_POINT('Ctrl Pts',(1.994970628,0.678571429,7.158934046));
#164705=CARTESIAN_POINT('Ctrl Pts',(2.379728812,0.615498301,7.051713995));
#164706=CARTESIAN_POINT('Ctrl Pts',(2.750778689,0.551245526,6.903872905));
#164707=CARTESIAN_POINT('Ctrl Pts',(1.75706614025095,0.681884070047877,
7.03386668559918));
#164708=CARTESIAN_POINT('Ctrl Pts',(1.76088449962548,0.681246574523938,
7.03290844979959));
#164709=CARTESIAN_POINT('Ctrl Pts',(1.764702859,0.680609079,7.031950214));
#164710=CARTESIAN_POINT('Ctrl Pts',(1.770806443,0.679590053,7.03041849));
#164711=CARTESIAN_POINT('Ctrl Pts',(1.776907359,0.678571429,7.028876172));
#164712=CARTESIAN_POINT('Ctrl Pts',(2.154675559,0.615498301,6.93337597));
#164713=CARTESIAN_POINT('Ctrl Pts',(2.52003186,0.551245526,6.79793640900001));
#164714=CARTESIAN_POINT('Ctrl Pts',(1.75488918513368,0.681884070047877,
7.03255995761175));
#164715=CARTESIAN_POINT('Ctrl Pts',(1.75870683623684,0.681246574523938,
7.03160290467088));
#164716=CARTESIAN_POINT('Ctrl Pts',(1.76252448734,0.680609079,7.03064585173001));
#164717=CARTESIAN_POINT('Ctrl Pts',(1.76862693918,0.679590053,7.02911601851));
#164718=CARTESIAN_POINT('Ctrl Pts',(1.77472672631,0.678571429,7.02757559326));
#164719=CARTESIAN_POINT('Ctrl Pts',(2.15242502647,0.615498301,6.93219258975));
#164720=CARTESIAN_POINT('Ctrl Pts',(2.51772439171,0.551245526,6.79687704404));
#164721=CARTESIAN_POINT('',(2.51558848957853,0.552026826152232,6.79958193857544));
#164722=CARTESIAN_POINT('Origin',(-0.0876565386706685,0.411145059523696,
-0.169723290623195));
#164723=CARTESIAN_POINT('Ctrl Pts',(2.53752478119287,0.562053380749443,
6.85763024745969));
#164724=CARTESIAN_POINT('Ctrl Pts',(2.53022429687456,0.558751695416953,
6.83826947494369));
#164725=CARTESIAN_POINT('Ctrl Pts',(2.52291237727739,0.555410033627866,
6.81891978007072));
#164726=CARTESIAN_POINT('Ctrl Pts',(2.51558848261983,0.552026824786843,
6.79958194233847));
#164727=CARTESIAN_POINT('Ctrl Pts',(2.404958681,0.551266351,7.031814718));
#164728=CARTESIAN_POINT('Ctrl Pts',(2.788001874,0.615380951000001,6.900809695));
#164729=CARTESIAN_POINT('Ctrl Pts',(3.154548371,0.680609079,6.728972363));
#164730=CARTESIAN_POINT('Ctrl Pts',(3.15822408941376,0.681263184913293,
6.72724918285622));
#164731=CARTESIAN_POINT('Ctrl Pts',(3.16189980782752,0.681917290826586,
6.72552600271243));
#164732=CARTESIAN_POINT('Ctrl Pts',(2.51119550620449,0.551266351,6.80120460239308));
#164733=CARTESIAN_POINT('Ctrl Pts',(2.88167670203736,0.615380951000001,
6.66441255329342));
#164734=CARTESIAN_POINT('Ctrl Pts',(3.23510692508309,0.680609079,6.48818696522738));
#164735=CARTESIAN_POINT('Ctrl Pts',(3.23865111385439,0.681263184913293,
6.48641977976979));
#164736=CARTESIAN_POINT('Ctrl Pts',(3.24219530262569,0.681917290826586,
6.48465259431219));
#164737=CARTESIAN_POINT('Origin',(-0.103639972525845,0.803453476587346,
-0.162201929279258));
#164738=CARTESIAN_POINT('Ctrl Pts',(3.46875702882675,0.681884070047877,
6.57252115311179));
#164739=CARTESIAN_POINT('Ctrl Pts',(3.47232386791338,0.681246574523938,
6.5706337390559));
#164740=CARTESIAN_POINT('Ctrl Pts',(3.475890707,0.680609079,6.568746325));
#164741=CARTESIAN_POINT('Ctrl Pts',(3.48159224,0.679590053,6.565729325));
#164742=CARTESIAN_POINT('Ctrl Pts',(3.487288527,0.678571429,6.562702432));
#164743=CARTESIAN_POINT('Ctrl Pts',(3.840002137,0.615498301,6.37527749));
#164744=CARTESIAN_POINT('Ctrl Pts',(4.17059561,0.551245526,6.151128087));
#164745=CARTESIAN_POINT('Ctrl Pts',(3.22806032850427,0.681884070047877,
6.49170151124601));
#164746=CARTESIAN_POINT('Ctrl Pts',(3.23158342425213,0.681246574523938,
6.48994484362301));
#164747=CARTESIAN_POINT('Ctrl Pts',(3.23510652,0.680609079,6.488188176));
#164748=CARTESIAN_POINT('Ctrl Pts',(3.24073813,0.679590053,6.485380172));
#164749=CARTESIAN_POINT('Ctrl Pts',(3.246364857,0.678571429,6.482562396));
#164750=CARTESIAN_POINT('Ctrl Pts',(3.594771326,0.615498301,6.308085939));
#164751=CARTESIAN_POINT('Ctrl Pts',(3.922470298,0.551245526,6.09727207499999));
#164752=CARTESIAN_POINT('',(3.91848455392433,0.552026825957499,6.09983432550923));
#164753=CARTESIAN_POINT('Origin',(-0.122092729018598,0.411147120165791,
-0.14691242890606));
#164754=CARTESIAN_POINT('Origin',(4.90675131577093,0.30001629144851,8.00672439438912));
#164755=CARTESIAN_POINT('Ctrl Pts',(3.860364389,0.551266351,6.350419771));
#164756=CARTESIAN_POINT('Ctrl Pts',(4.206290037,0.615380951,6.14013460900001));
#164757=CARTESIAN_POINT('Ctrl Pts',(4.527326934,0.680609079,5.893518076));
#164758=CARTESIAN_POINT('Ctrl Pts',(4.53054628336893,0.681263184913293,
5.89104501203975));
#164759=CARTESIAN_POINT('Ctrl Pts',(4.53376563273785,0.681917290826586,
5.88857194807951));
#164760=CARTESIAN_POINT('Ctrl Pts',(3.9145430984241,0.551266351,6.10236341471059));
#164761=CARTESIAN_POINT('Ctrl Pts',(4.24695640248066,0.615380951,5.88912698187087));
#164762=CARTESIAN_POINT('Ctrl Pts',(4.5542403313273,0.680609079,5.6410443994992));
#164763=CARTESIAN_POINT('Ctrl Pts',(4.55732176630146,0.681263184913293,
5.63855663403529));
#164764=CARTESIAN_POINT('Ctrl Pts',(4.56040320127563,0.681917290826586,
5.63606886857137));
#164765=CARTESIAN_POINT('Origin',(-0.136085561345225,0.803453460267691,
-0.136130227890238));
#164766=CARTESIAN_POINT('Ctrl Pts',(4.80055718210444,0.681884070047877,
5.67317903306963));
#164767=CARTESIAN_POINT('Ctrl Pts',(4.80363489255222,0.681246574523938,
5.67056898153481));
#164768=CARTESIAN_POINT('Ctrl Pts',(4.806712603,0.680609079,5.66795893));
#164769=CARTESIAN_POINT('Ctrl Pts',(4.811632272,0.679590053,5.663786806));
#164770=CARTESIAN_POINT('Ctrl Pts',(4.81654469,0.678571429,5.659606147));
#164771=CARTESIAN_POINT('Ctrl Pts',(5.120721229,0.615498301,5.40074009600001));
#164772=CARTESIAN_POINT('Ctrl Pts',(5.395400115,0.551245526,5.110763357));
#164773=CARTESIAN_POINT('Ctrl Pts',(4.5481140040602,0.681884070047877,5.64599158717324));
#164774=CARTESIAN_POINT('Ctrl Pts',(4.5511771000301,0.681246574523938,5.64351862808662));
#164775=CARTESIAN_POINT('Ctrl Pts',(4.554240196,0.680609079,5.641045669));
#164776=CARTESIAN_POINT('Ctrl Pts',(4.559136504,0.679590053,5.637092685));
#164777=CARTESIAN_POINT('Ctrl Pts',(4.564025943,0.678571429,5.633131207));
#164778=CARTESIAN_POINT('Ctrl Pts',(4.866779581,0.615498301,5.387836821));
#164779=CARTESIAN_POINT('Ctrl Pts',(5.141498385,0.551245526,5.111506076));
#164780=CARTESIAN_POINT('',(5.13815663269613,0.552026825934544,5.11486523958666));
#164781=CARTESIAN_POINT('Origin',(-0.150820139731521,0.41114713854277,-0.117231435818382));
#164782=CARTESIAN_POINT('Origin',(6.51225232756528,0.300122489565501,6.76356590004443));
#164783=CARTESIAN_POINT('Ctrl Pts',(5.135263749,0.551266351,5.372086254));
#164784=CARTESIAN_POINT('Ctrl Pts',(5.427896753,0.615380951,5.092353653));
#164785=CARTESIAN_POINT('Ctrl Pts',(5.688412722,0.680609079,4.782489435));
#164786=CARTESIAN_POINT('Ctrl Pts',(5.69102516913063,0.681263184913293,
4.7793821249556));
#164787=CARTESIAN_POINT('Ctrl Pts',(5.69363761626127,0.681917290826586,
4.77627481491121));
#164788=CARTESIAN_POINT('Ctrl Pts',(5.134851007,0.551266351,5.118183773));
#164789=CARTESIAN_POINT('Ctrl Pts',(5.413653213,0.615380951,4.838473655));
#164790=CARTESIAN_POINT('Ctrl Pts',(5.660422662,0.680609079,4.530134136));
#164791=CARTESIAN_POINT('Ctrl Pts',(5.66289725939779,0.681263184913293,
4.52704211559617));
#164792=CARTESIAN_POINT('Ctrl Pts',(5.66537185679557,0.681917290826586,
4.52395009519234));
#164793=CARTESIAN_POINT('Origin',(-0.162167589274738,0.803452522456232,
-0.103693095701407));
#164794=CARTESIAN_POINT('Ctrl Pts',(5.90788861795456,0.681884070047877,
4.50856537016347));
#164795=CARTESIAN_POINT('Ctrl Pts',(5.91033328897728,0.681246574523938,
4.50535472308173));
#164796=CARTESIAN_POINT('Ctrl Pts',(5.91277796,0.680609079,4.502144076));
#164797=CARTESIAN_POINT('Ctrl Pts',(5.916685726,0.679590053,4.49701191));
#164798=CARTESIAN_POINT('Ctrl Pts',(5.920584577,0.678571429,4.491872968));
#164799=CARTESIAN_POINT('Ctrl Pts',(6.162001088,0.615498301,4.173670097));
#164800=CARTESIAN_POINT('Ctrl Pts',(6.367921707,0.551245526,3.831425012));
#164801=CARTESIAN_POINT('Ctrl Pts',(5.65550292364228,0.681884070047877,
4.53628137163686));
#164802=CARTESIAN_POINT('Ctrl Pts',(5.65796279282114,0.681246574523938,
4.53320775381843));
#164803=CARTESIAN_POINT('Ctrl Pts',(5.660422662,0.680609079,4.530134136));
#164804=CARTESIAN_POINT('Ctrl Pts',(5.664354722,0.679590053,4.525221009));
#164805=CARTESIAN_POINT('Ctrl Pts',(5.668278248,0.678571429,4.520301063));
#164806=CARTESIAN_POINT('Ctrl Pts',(5.911222633,0.615498301,4.215658441));
#164807=CARTESIAN_POINT('Ctrl Pts',(6.120115721,0.551245526,3.886731733));
#164808=CARTESIAN_POINT('',(6.11757421807822,0.552026825940366,3.89073073953274));
#164809=CARTESIAN_POINT('Origin',(-0.172495070084803,0.411147101698712,
-0.0820685574945201));
#164810=CARTESIAN_POINT('Origin',(7.81397171485883,0.300138470944808,5.20550314261985));
#164811=CARTESIAN_POINT('Ctrl Pts',(6.170043883,0.551266351,4.142559954));
#164812=CARTESIAN_POINT('Ctrl Pts',(6.39570105,0.615380951,3.8064599));
#164813=CARTESIAN_POINT('Ctrl Pts',(6.583514653,0.680609079,3.447836903));
#164814=CARTESIAN_POINT('Ctrl Pts',(6.58539804275969,0.681263184913293,
3.44424064123114));
#164815=CARTESIAN_POINT('Ctrl Pts',(6.58728143251939,0.681917290826587,
3.44064437946229));
#164816=CARTESIAN_POINT('Ctrl Pts',(6.11505898654828,0.551266351,3.89468105272049));
#164817=CARTESIAN_POINT('Ctrl Pts',(6.32721347665985,0.615380951,3.56157618377961));
#164818=CARTESIAN_POINT('Ctrl Pts',(6.50192964480889,0.680609079,3.2073973571239));
#164819=CARTESIAN_POINT('Ctrl Pts',(6.50368169384414,0.681263184913293,
3.20384566137573));
#164820=CARTESIAN_POINT('Ctrl Pts',(6.5054337428794,0.681917290826587,3.20029396562756));
#164821=CARTESIAN_POINT('Origin',(-0.180667349183379,0.803453434661462,
-0.0664075156033789));
#164822=CARTESIAN_POINT('Ctrl Pts',(6.73897374700992,0.681884070047882,
3.13313619990097));
#164823=CARTESIAN_POINT('Ctrl Pts',(6.74067106900496,0.681246574523941,
3.12947508395048));
#164824=CARTESIAN_POINT('Ctrl Pts',(6.742368391,0.680609079,3.125813968));
#164825=CARTESIAN_POINT('Ctrl Pts',(6.745081532,0.679590053000001,3.119961735));
#164826=CARTESIAN_POINT('Ctrl Pts',(6.747784509,0.678571429,3.114104801));
#164827=CARTESIAN_POINT('Ctrl Pts',(6.915152625,0.615498301,2.751443923));
#164828=CARTESIAN_POINT('Ctrl Pts',(7.042686358,0.551245526,2.372933492));
#164829=CARTESIAN_POINT('Ctrl Pts',(6.49844681077687,0.681884070047882,
3.21445968164217));
#164830=CARTESIAN_POINT('Ctrl Pts',(6.50018843288844,0.681246574523941,
3.21092912382109));
#164831=CARTESIAN_POINT('Ctrl Pts',(6.501930055,0.680609079,3.207398566));
#164832=CARTESIAN_POINT('Ctrl Pts',(6.504714009,0.679590053000001,3.201755028));
#164833=CARTESIAN_POINT('Ctrl Pts',(6.507488162,0.678571429,3.196106666));
#164834=CARTESIAN_POINT('Ctrl Pts',(6.679263483,0.615498301,2.846360558));
#164835=CARTESIAN_POINT('Ctrl Pts',(6.81256324800001,0.551245526,2.480218134));
#164836=CARTESIAN_POINT('',(6.81094083240474,0.552026825957956,2.48466999354874));
#164837=CARTESIAN_POINT('Origin',(-0.186104521948789,0.411147115358488,
-0.0430684921105004));
#164838=CARTESIAN_POINT('Origin',(8.7514997255839,0.300018450747821,3.4045703757469));
#164839=CARTESIAN_POINT('Ctrl Pts',(6.916319623,0.551266351,2.719332154));
#164840=CARTESIAN_POINT('Ctrl Pts',(7.064449474,0.615380951,2.342580312));
#164841=CARTESIAN_POINT('Ctrl Pts',(7.170778755,0.680609079,1.951967349));
#164842=CARTESIAN_POINT('Ctrl Pts',(7.17184502217018,0.681263184913293,
1.94805029271246));
#164843=CARTESIAN_POINT('Ctrl Pts',(7.17291128934035,0.681917290826587,
1.94413323642491));
#164844=CARTESIAN_POINT('Ctrl Pts',(6.80933360604283,0.551266351,2.48906865116737));
#164845=CARTESIAN_POINT('Ctrl Pts',(6.94492034197236,0.615380951,2.11814464547145));
#164846=CARTESIAN_POINT('Ctrl Pts',(7.03941376445819,0.680609079,1.73468751145306));
#164847=CARTESIAN_POINT('Ctrl Pts',(7.0403613419575,0.681263184913293,1.73084221362609));
#164848=CARTESIAN_POINT('Ctrl Pts',(7.04130891945682,0.681917290826587,
1.72699691579912));
#164849=CARTESIAN_POINT('Origin',(-0.190719082213691,0.803453445641696,
-0.0260168029193106));
#164850=CARTESIAN_POINT('Ctrl Pts',(7.25495195577507,0.681884070047882,
1.61120506410122));
#164851=CARTESIAN_POINT('Ctrl Pts',(7.25582256288753,0.681246574523941,
1.60726466905061));
#164852=CARTESIAN_POINT('Ctrl Pts',(7.25669317,0.680609079,1.603324274));
#164853=CARTESIAN_POINT('Ctrl Pts',(7.258084821,0.679590053000001,1.597025618));
#164854=CARTESIAN_POINT('Ctrl Pts',(7.259465537,0.678571429,1.590724555));
#164855=CARTESIAN_POINT('Ctrl Pts',(7.344959311,0.615498301,1.200563289));
#164856=CARTESIAN_POINT('Ctrl Pts',(7.388142822,0.551245526,0.803486239));
#164857=CARTESIAN_POINT('Ctrl Pts',(7.03753054804688,0.681884070047882,
1.74233342918306));
#164858=CARTESIAN_POINT('Ctrl Pts',(7.03847248652344,0.681246574523941,
1.73851101659153));
#164859=CARTESIAN_POINT('Ctrl Pts',(7.039414425,0.680609079,1.734688604));
#164860=CARTESIAN_POINT('Ctrl Pts',(7.040920098,0.679590053000001,1.728578541));
#164861=CARTESIAN_POINT('Ctrl Pts',(7.042415162,0.678571429,1.722465874));
#164862=CARTESIAN_POINT('Ctrl Pts',(7.134989397,0.615498301,1.343970018));
#164863=CARTESIAN_POINT('Ctrl Pts',(7.186462889,0.551245526,0.957732292));
#164864=CARTESIAN_POINT('',(7.18583542279277,0.552026825978395,0.962428841414932));
#164865=CARTESIAN_POINT('Origin',(-0.191012030134711,0.411147106807098,
-0.00205461113786623));
#164866=CARTESIAN_POINT('Origin',(9.27850705784563,0.300053135916551,1.44360164381105));
#164867=CARTESIAN_POINT('Ctrl Pts',(7.339195944,0.551266351,1.168951406));
#164868=CARTESIAN_POINT('Ctrl Pts',(7.402872092,0.615380951,0.769164273));
#164869=CARTESIAN_POINT('Ctrl Pts',(7.422745213,0.680609079,0.364825971));
#164870=CARTESIAN_POINT('Ctrl Pts',(7.42294450012291,0.681263184913293,
0.360771277382102));
#164871=CARTESIAN_POINT('Ctrl Pts',(7.42314378724581,0.681917290826587,
0.356716583764203));
#164872=CARTESIAN_POINT('Ctrl Pts',(7.18521135359354,0.551266351,0.967070166715704));
#164873=CARTESIAN_POINT('Ctrl Pts',(7.23789045028809,0.615380951,0.575671017899855));
#164874=CARTESIAN_POINT('Ctrl Pts',(7.24774271989205,0.680609079,0.18086560584187));
#164875=CARTESIAN_POINT('Ctrl Pts',(7.24784151818667,0.681263184913293,
0.176906507787927));
#164876=CARTESIAN_POINT('Ctrl Pts',(7.24794031648128,0.681917290826587,
0.172947409733983));
#164877=CARTESIAN_POINT('Origin',(-0.191852911351374,0.803453428315243,
0.0155904250026355));
#164878=CARTESIAN_POINT('Ctrl Pts',(7.43169667121216,0.681884070047882,
0.0139357695080207));
#164879=CARTESIAN_POINT('Ctrl Pts',(7.43169985610608,0.681246574523941,
0.00990034375401035));
#164880=CARTESIAN_POINT('Ctrl Pts',(7.431703041,0.680609079,0.005864918));
#164881=CARTESIAN_POINT('Ctrl Pts',(7.431708132,0.679590053000001,-0.000585643));
#164882=CARTESIAN_POINT('Ctrl Pts',(7.431702024,0.678571429,-0.007036203));
#164883=CARTESIAN_POINT('Ctrl Pts',(7.431323862,0.615498301,-0.40645435));
#164884=CARTESIAN_POINT('Ctrl Pts',(7.38813793800001,0.551245526,-0.803531138000001));
#164885=CARTESIAN_POINT('Ctrl Pts',(7.24754717756366,0.681884070047882,
0.1887376018885));
#164886=CARTESIAN_POINT('Ctrl Pts',(7.24764538878184,0.681246574523941,
0.18480206644425));
#164887=CARTESIAN_POINT('Ctrl Pts',(7.2477436,0.680609079,0.180866531));
#164888=CARTESIAN_POINT('Ctrl Pts',(7.247900589,0.679590053000001,0.174575643));
#164889=CARTESIAN_POINT('Ctrl Pts',(7.248046656,0.678571429,0.168284491));
#164890=CARTESIAN_POINT('Ctrl Pts',(7.257091136,0.615498301,-0.221263065));
#164891=CARTESIAN_POINT('Ctrl Pts',(7.224331513,0.551245526,-0.609536047));
#164892=CARTESIAN_POINT('Ctrl Pts',(7.24570568262718,0.681884070047882,
0.190485620212305));
#164893=CARTESIAN_POINT('Ctrl Pts',(7.24580484410859,0.681246574523941,
0.186551083671152));
#164894=CARTESIAN_POINT('Ctrl Pts',(7.24590400559,0.680609079,0.18261654713));
#164895=CARTESIAN_POINT('Ctrl Pts',(7.24606251356999,0.679590053000001,
0.17632725586));
#164896=CARTESIAN_POINT('Ctrl Pts',(7.24621010232,0.678571429,0.17003769794));
#164897=CARTESIAN_POINT('Ctrl Pts',(7.25534880874,0.615498301,-0.21941115215));
#164898=CARTESIAN_POINT('Ctrl Pts',(7.22269344875001,0.551245526,-0.60759609609));
#164899=CARTESIAN_POINT('',(7.22472833507074,0.552026826383927,-0.604814410547277));
#164900=CARTESIAN_POINT('Origin',(-0.186987466365719,0.41114500527251,0.0390556790372377));
#164901=CARTESIAN_POINT('Ctrl Pts',(7.28652936256475,0.562053380502287,
-0.610421555679701));
#164902=CARTESIAN_POINT('Ctrl Pts',(7.26592120359517,0.558751695429002,
-0.60856673103941));
#164903=CARTESIAN_POINT('Ctrl Pts',(7.24532065958405,0.555410033641427,
-0.60669792256753));
#164904=CARTESIAN_POINT('Ctrl Pts',(7.22472833612555,0.552026824884503,
-0.604814404498353));
#164905=CARTESIAN_POINT('Ctrl Pts',(7.418899619,0.551266351,-0.436088211));
#164906=CARTESIAN_POINT('Ctrl Pts',(7.395144639,0.615380951,-0.840217033));
#164907=CARTESIAN_POINT('Ctrl Pts',(7.327632355,0.680609079,-1.239374263));
#164908=CARTESIAN_POINT('Ctrl Pts',(7.32695534363177,0.681263184913293,
-1.24337700096723));
#164909=CARTESIAN_POINT('Ctrl Pts',(7.32627833226354,0.681917290826587,
-1.24737973893445));
#164910=CARTESIAN_POINT('Ctrl Pts',(7.225117579,0.551266351,-0.600146619));
#164911=CARTESIAN_POINT('Ctrl Pts',(7.19242586500001,0.615380951,-0.993719575));
#164912=CARTESIAN_POINT('Ctrl Pts',(7.11717634000001,0.680609079,-1.381412661));
#164913=CARTESIAN_POINT('Ctrl Pts',(7.11642173978711,0.681263184913293,
-1.38530043683952));
#164914=CARTESIAN_POINT('Ctrl Pts',(7.11566713957423,0.681917290826587,
-1.38918821267904));
#164915=CARTESIAN_POINT('Origin',(-0.184016267475409,0.803452540152115,
0.056468539661578));
#164916=CARTESIAN_POINT('Ctrl Pts',(7.26094351293389,0.681884070047882,
-1.58398514730385));
#164917=CARTESIAN_POINT('Ctrl Pts',(7.26007912546694,0.681246574523941,
-1.58792691115192));
#164918=CARTESIAN_POINT('Ctrl Pts',(7.259214738,0.680609079,-1.591868675));
#164919=CARTESIAN_POINT('Ctrl Pts',(7.257833029,0.679590053000001,-1.598169519));
#164920=CARTESIAN_POINT('Ctrl Pts',(7.256440385,0.678571429,-1.604467956));
#164921=CARTESIAN_POINT('Ctrl Pts',(7.17020797,0.615498301,-1.994466635));
#164922=CARTESIAN_POINT('Ctrl Pts',(7.04267193700001,0.551245526,-2.372976291));
#164923=CARTESIAN_POINT('Ctrl Pts',(7.11867655828793,0.681884070047882,
-1.373683387019));
#164924=CARTESIAN_POINT('Ctrl Pts',(7.11792644914396,0.681246574523941,
-1.3775480240095));
#164925=CARTESIAN_POINT('Ctrl Pts',(7.11717634,0.680609079,-1.381412661));
#164926=CARTESIAN_POINT('Ctrl Pts',(7.115977303,0.679590053000001,-1.387590219));
#164927=CARTESIAN_POINT('Ctrl Pts',(7.114767544,0.678571429,-1.393765687));
#164928=CARTESIAN_POINT('Ctrl Pts',(7.03985936,0.615498301,-1.776150134));
#164929=CARTESIAN_POINT('Ctrl Pts',(6.92439842400001,0.551245526,-2.148303159));
#164930=CARTESIAN_POINT('',(6.9258009809809,0.552026825996016,-2.14377722029232));
#164931=CARTESIAN_POINT('Origin',(-0.174220359436987,0.411147148048371,
0.0783391005764139));
#164932=CARTESIAN_POINT('Origin',(9.02742321671478,0.300018637696928,-2.58584182573121));
#164933=CARTESIAN_POINT('Ctrl Pts',(7.151703794,0.551266351,-2.020736828));
#164934=CARTESIAN_POINT('Ctrl Pts',(7.04162844100001,0.615380951,-2.410310724));
#164935=CARTESIAN_POINT('Ctrl Pts',(6.889887551,0.680609079,-2.785622735));
#164936=CARTESIAN_POINT('Ctrl Pts',(6.8883658974361,0.681263184913293,-2.78938635375241));
#164937=CARTESIAN_POINT('Ctrl Pts',(6.88684424387221,0.681917290826587,
-2.79314997250481));
#164938=CARTESIAN_POINT('Ctrl Pts',(6.92718343146799,0.551266351,-2.13930282854591));
#164939=CARTESIAN_POINT('Ctrl Pts',(6.81064944691794,0.615380951,-2.5166464539081));
#164940=CARTESIAN_POINT('Ctrl Pts',(6.65381663525581,0.680609079,-2.87909900209931));
#164941=CARTESIAN_POINT('Ctrl Pts',(6.65224392003843,0.681263184913293,
-2.88273366650452));
#164942=CARTESIAN_POINT('Ctrl Pts',(6.65067120482106,0.681917290826587,
-2.88636833090973));
#164943=CARTESIAN_POINT('Origin',(-0.167571881686693,0.803452753912076,
0.0947052645359447));
#164944=CARTESIAN_POINT('Ctrl Pts',(6.7506767050316,0.681884070047882,-3.10784067502777));
#164945=CARTESIAN_POINT('Ctrl Pts',(6.7489851635158,0.681246574523941,-3.11150446601388));
#164946=CARTESIAN_POINT('Ctrl Pts',(6.747293622,0.680609079,-3.115168257));
#164947=CARTESIAN_POINT('Ctrl Pts',(6.744589721,0.679590053000001,-3.121024766));
#164948=CARTESIAN_POINT('Ctrl Pts',(6.741875659,0.678571429,-3.126876571));
#164949=CARTESIAN_POINT('Ctrl Pts',(6.573821121,0.615498301,-3.489219877));
#164950=CARTESIAN_POINT('Ctrl Pts',(6.367898423,0.551245526,-3.831463711));
#164951=CARTESIAN_POINT('Ctrl Pts',(6.65694453501887,0.681884070047882,
-2.87187246525371));
#164952=CARTESIAN_POINT('Ctrl Pts',(6.65538118000943,0.681246574523941,
-2.87548549812686));
#164953=CARTESIAN_POINT('Ctrl Pts',(6.653817825,0.680609079,-2.879098531));
#164954=CARTESIAN_POINT('Ctrl Pts',(6.651318828,0.679590053000001,-2.884873904));
#164955=CARTESIAN_POINT('Ctrl Pts',(6.64880981,0.678571429,-2.890644931));
#164956=CARTESIAN_POINT('Ctrl Pts',(6.49345158400001,0.615498301,-3.247986396));
#164957=CARTESIAN_POINT('Ctrl Pts',(6.300688161,0.551245526,-3.586618002));
#164958=CARTESIAN_POINT('',(6.3030308701282,0.552026825948882,-3.58249938561785));
#164959=CARTESIAN_POINT('Origin',(-0.15330670644422,0.411147129612742,0.113959870939336));
#164960=CARTESIAN_POINT('Origin',(8.26029530834744,0.300041800905005,-4.46592127356874));
#164961=CARTESIAN_POINT('Ctrl Pts',(6.550102248,0.551266351,-3.510898037));
#164962=CARTESIAN_POINT('Ctrl Pts',(6.358853524,0.615380951,-3.867700964));
#164963=CARTESIAN_POINT('Ctrl Pts',(6.129979263,0.680609079,-4.201618583));
#164964=CARTESIAN_POINT('Ctrl Pts',(6.1276841180662,0.681263184913293,-4.20496709990272));
#164965=CARTESIAN_POINT('Ctrl Pts',(6.12538897313239,0.681917290826587,
-4.20831561680543));
#164966=CARTESIAN_POINT('Ctrl Pts',(6.30534286154812,0.551266351,-3.57842678930755));
#164967=CARTESIAN_POINT('Ctrl Pts',(6.11041565201059,0.615380951,-3.92189696811787));
#164968=CARTESIAN_POINT('Ctrl Pts',(5.87933291988112,0.680609079,-4.24216115831215));
#164969=CARTESIAN_POINT('Ctrl Pts',(5.87701562845822,0.681263184913293,
-4.24537275899801));
#164970=CARTESIAN_POINT('Ctrl Pts',(5.87469833703533,0.681917290826587,
-4.24858435968387));
#164971=CARTESIAN_POINT('Origin',(-0.143295177047,0.803452728353365,0.128514024721328));
#164972=CARTESIAN_POINT('Ctrl Pts',(5.92475575618306,0.681884070047882,
-4.48637703227967));
#164973=CARTESIAN_POINT('Ctrl Pts',(5.92231615559153,0.681246574523941,
-4.48959153363984));
#164974=CARTESIAN_POINT('Ctrl Pts',(5.91987655500001,0.680609079,-4.492806035));
#164975=CARTESIAN_POINT('Ctrl Pts',(5.915976894,0.679590053000001,-4.497944362));
#164976=CARTESIAN_POINT('Ctrl Pts',(5.912068319,0.678571429,-4.503075913));
#164977=CARTESIAN_POINT('Ctrl Pts',(5.670049703,0.615498301,-4.820821076));
#164978=CARTESIAN_POINT('Ctrl Pts',(5.395369056,0.551245526,-5.11079614500001));
#164979=CARTESIAN_POINT('Ctrl Pts',(5.88394118241646,0.681884070047882,
-4.23577597926324));
#164980=CARTESIAN_POINT('Ctrl Pts',(5.88163768270823,0.681246574523941,
-4.23896846663162));
#164981=CARTESIAN_POINT('Ctrl Pts',(5.879334183,0.680609079,-4.242160954));
#164982=CARTESIAN_POINT('Ctrl Pts',(5.875652077,0.679590053000001,-4.247264092));
#164983=CARTESIAN_POINT('Ctrl Pts',(5.871961118,0.678571429,-4.25236083));
#164984=CARTESIAN_POINT('Ctrl Pts',(5.643417229,0.615498301,-4.567950425));
#164985=CARTESIAN_POINT('Ctrl Pts',(5.382364723,0.551245526,-4.857226574));
#164986=CARTESIAN_POINT('',(5.38553804102176,0.552026825913963,-4.85370786181476));
#164987=CARTESIAN_POINT('Origin',(-0.125224422707866,0.411147099587523,
0.144251912085741));
#164988=CARTESIAN_POINT('Origin',(7.1061891438417,0.300134040132493,-6.13650682902755));
#164989=CARTESIAN_POINT('Ctrl Pts',(5.642225201,0.551266351,-4.836893556));
#164990=CARTESIAN_POINT('Ctrl Pts',(5.378745684,0.615380951,-5.144241806));
#164991=CARTESIAN_POINT('Ctrl Pts',(5.083439958,0.680609079,-5.42115141600001));
#164992=CARTESIAN_POINT('Ctrl Pts',(5.08047864012183,0.681263184913293,
-5.42392825812168));
#164993=CARTESIAN_POINT('Ctrl Pts',(5.07751732224366,0.681917290826586,
-5.42670510024335));
#164994=CARTESIAN_POINT('Ctrl Pts',(5.388672745,0.551266351,-4.850227423));
#164995=CARTESIAN_POINT('Ctrl Pts',(5.124466893,0.615380951,-5.143763941));
#164996=CARTESIAN_POINT('Ctrl Pts',(4.829939409,0.680609079,-5.406864646));
#164997=CARTESIAN_POINT('Ctrl Pts',(4.82698589531167,0.681263184913293,
-5.40950301279373));
#164998=CARTESIAN_POINT('Ctrl Pts',(4.82403238162335,0.681917290826586,
-5.41214137958745));
#164999=CARTESIAN_POINT('Origin',(-0.112320525602429,0.80345250370582,0.156315845870442));
#165000=CARTESIAN_POINT('Ctrl Pts',(4.82179981207758,0.681884070047881,
-5.65513538147594));
#165001=CARTESIAN_POINT('Ctrl Pts',(4.81872622553879,0.681246574523941,
-5.65775028823797));
#165002=CARTESIAN_POINT('Ctrl Pts',(4.815652639,0.680609079,-5.660365195));
#165003=CARTESIAN_POINT('Ctrl Pts',(4.810739562,0.679590053000001,-5.66454508000001));
#165004=CARTESIAN_POINT('Ctrl Pts',(4.805819236,0.678571429,-5.668716429));
#165005=CARTESIAN_POINT('Ctrl Pts',(4.501153063,0.615498301,-5.927006039));
#165006=CARTESIAN_POINT('Ctrl Pts',(4.170558228,0.551245526,-6.15115343300001));
#165007=CARTESIAN_POINT('Ctrl Pts',(4.8358112798721,0.681884070047881,-5.40161931776974));
#165008=CARTESIAN_POINT('Ctrl Pts',(4.83287534443605,0.681246574523941,
-5.40424198188487));
#165009=CARTESIAN_POINT('Ctrl Pts',(4.829939409,0.680609079,-5.406864646));
#165010=CARTESIAN_POINT('Ctrl Pts',(4.825246365,0.679590053000001,-5.411056931));
#165011=CARTESIAN_POINT('Ctrl Pts',(4.82054605,0.678571429,-5.415241063));
#165012=CARTESIAN_POINT('Ctrl Pts',(4.529502956,0.615498301,-5.674322168));
#165013=CARTESIAN_POINT('Ctrl Pts',(4.212367892,0.551245526,-5.90071663));
#165014=CARTESIAN_POINT('',(4.21622343872244,0.552026825912812,-5.8979623527564));
#165015=CARTESIAN_POINT('Origin',(-0.0912870167708651,0.411147072761699,
0.167799146015306));
#165016=CARTESIAN_POINT('Origin',(5.62149350149955,0.300042050105536,-7.521392327659));
#165017=CARTESIAN_POINT('Ctrl Pts',(4.470523974,0.551266351,-5.936721307));
#165018=CARTESIAN_POINT('Ctrl Pts',(4.147133673,0.615380951,-6.180243619));
#165019=CARTESIAN_POINT('Ctrl Pts',(3.799204651,0.680609079,-6.387197234));
#165020=CARTESIAN_POINT('Ctrl Pts',(3.79571562812483,0.681263184913293,
-6.38927255928527));
#165021=CARTESIAN_POINT('Ctrl Pts',(3.79222660524966,0.681917290826586,
-6.39134788457053));
#165022=CARTESIAN_POINT('Ctrl Pts',(4.22003178354831,0.551266351,-5.8952369439236));
#165023=CARTESIAN_POINT('Ctrl Pts',(3.8989012549373,0.615380951,-6.12511422415422));
#165024=CARTESIAN_POINT('Ctrl Pts',(3.55470080472887,0.680609079,-6.31874901102887));
#165025=CARTESIAN_POINT('Ctrl Pts',(3.55124917187135,0.681263184913293,
-6.3206907754639));
#165026=CARTESIAN_POINT('Ctrl Pts',(3.54779753901383,0.681917290826586,
-6.32263253989893));
#165027=CARTESIAN_POINT('Origin',(-0.0760896690513591,0.803452726218141,
0.176804437617541));
#165028=CARTESIAN_POINT('Ctrl Pts',(3.49338187026732,0.681884070047882,
-6.55946588747028));
#165029=CARTESIAN_POINT('Ctrl Pts',(3.48981801463366,0.681246574523941,
-6.56135892873514));
#165030=CARTESIAN_POINT('Ctrl Pts',(3.486254159,0.680609079,-6.56325197));
#165031=CARTESIAN_POINT('Ctrl Pts',(3.480557395,0.679590053000001,-6.566277965));
#165032=CARTESIAN_POINT('Ctrl Pts',(3.474855387,0.678571429,-6.569294066));
#165033=CARTESIAN_POINT('Ctrl Pts',(3.121787509,0.615498301,-6.756050787));
#165034=CARTESIAN_POINT('Ctrl Pts',(2.750736733,0.551245526,-6.903889622));
#165035=CARTESIAN_POINT('Ctrl Pts',(3.56156421782437,0.681884070047882,
-6.31488893800863));
#165036=CARTESIAN_POINT('Ctrl Pts',(3.55813312741219,0.681246574523941,
-6.31681914700431));
#165037=CARTESIAN_POINT('Ctrl Pts',(3.554702037,0.680609079,-6.318749356));
#165038=CARTESIAN_POINT('Ctrl Pts',(3.549217496,0.679590053000001,-6.321834763));
#165039=CARTESIAN_POINT('Ctrl Pts',(3.543727607,0.678571429,-6.324910643));
#165040=CARTESIAN_POINT('Ctrl Pts',(3.20379416,0.615498301,-6.515368914));
#165041=CARTESIAN_POINT('Ctrl Pts',(2.84540542,0.551245526,-6.668295734));
#165042=CARTESIAN_POINT('Ctrl Pts',(3.56224604129995,0.681884070047882,
-6.31244316851402));
#165043=CARTESIAN_POINT('Ctrl Pts',(3.55881627853997,0.681246574523941,
-6.31437374918701));
#165044=CARTESIAN_POINT('Ctrl Pts',(3.55538651578,0.680609079,-6.31630432986));
#165045=CARTESIAN_POINT('Ctrl Pts',(3.54990409701,0.679590053000001,-6.31939033098));
#165046=CARTESIAN_POINT('Ctrl Pts',(3.5444163292,0.678571429,-6.32246680877));
#165047=CARTESIAN_POINT('Ctrl Pts',(3.20461422650999,0.615498301,-6.51296209527));
#165048=CARTESIAN_POINT('Ctrl Pts',(2.84635210687,0.551245526,-6.66593979512));
#165049=CARTESIAN_POINT('',(2.84976291824466,0.552026826190771,-6.66643467634339));
#165050=CARTESIAN_POINT('Origin',(-0.0530804187079026,0.411144977216728,
0.183499851431562));
#165051=CARTESIAN_POINT('Ctrl Pts',(2.87375705931618,0.56205338059825,-6.72366306341953));
#165052=CARTESIAN_POINT('Ctrl Pts',(2.86574278438241,0.558751695403869,
-6.70458669100326));
#165053=CARTESIAN_POINT('Ctrl Pts',(2.85774443038173,0.555410033604048,
-6.68551049651921));
#165054=CARTESIAN_POINT('Ctrl Pts',(2.84976292439803,0.552026824750786,
-6.66643467502883));
#165055=CARTESIAN_POINT('Ctrl Pts',(3.089786015,0.551266351,-6.758954569));
#165056=CARTESIAN_POINT('Ctrl Pts',(2.721606301,0.615380951,-6.927264109));
#165057=CARTESIAN_POINT('Ctrl Pts',(2.337322756,0.680609079,-7.054584809));
#165058=CARTESIAN_POINT('Ctrl Pts',(2.33346917094593,0.681263184913293,
-7.05586157755535));
#165059=CARTESIAN_POINT('Ctrl Pts',(2.32961558589186,0.681917290826586,
-7.0571383461107));
#165060=CARTESIAN_POINT('Ctrl Pts',(2.854069293,0.551266351,-6.664592146));
#165061=CARTESIAN_POINT('Ctrl Pts',(2.491029771,0.615380951,-6.82006151700001));
#165062=CARTESIAN_POINT('Ctrl Pts',(2.113250748,0.680609079,-6.93517637));
#165063=CARTESIAN_POINT('Ctrl Pts',(2.10946239011761,0.681263184913293,
-6.93633073864991));
#165064=CARTESIAN_POINT('Ctrl Pts',(2.10567403223522,0.681917290826586,
-6.93748510729981));
#165065=CARTESIAN_POINT('Origin',(-0.0363040560098285,0.803453434253933,
0.189031072590716));
#165066=CARTESIAN_POINT('Ctrl Pts',(2.00161727379074,0.681884070047882,
-7.15708305927178));
#165067=CARTESIAN_POINT('Ctrl Pts',(1.99772979139537,0.681246574523941,
-7.15816571863589));
#165068=CARTESIAN_POINT('Ctrl Pts',(1.993842309,0.680609079,-7.159248378));
#165069=CARTESIAN_POINT('Ctrl Pts',(1.987628233,0.679590053000001,-7.160978991));
#165070=CARTESIAN_POINT('Ctrl Pts',(1.981411162,0.678571429,-7.162698814));
#165071=CARTESIAN_POINT('Ctrl Pts',(1.59645064,0.615498301,-7.269190109));
#165072=CARTESIAN_POINT('Ctrl Pts',(1.202293846,0.551245526,-7.33380760600001));
#165073=CARTESIAN_POINT('Ctrl Pts',(2.12078237088003,0.681884070047882,
-6.93288137335172));
#165074=CARTESIAN_POINT('Ctrl Pts',(2.11701655944001,0.681246574523941,
-6.93402887167586));
#165075=CARTESIAN_POINT('Ctrl Pts',(2.113250748,0.680609079,-6.93517637));
#165076=CARTESIAN_POINT('Ctrl Pts',(2.107231161,0.679590053000001,-6.937010627));
#165077=CARTESIAN_POINT('Ctrl Pts',(2.1012084,0.678571429,-6.938834431));
#165078=CARTESIAN_POINT('Ctrl Pts',(1.728279509,0.615498301,-7.05176425));
#165079=CARTESIAN_POINT('Ctrl Pts',(1.345394953,0.551245526,-7.124072741));
#165080=CARTESIAN_POINT('',(1.35005064349767,0.552026825956876,-7.1231919291517));
#165081=CARTESIAN_POINT('Origin',(-0.0123928583365629,0.411147082466218,
0.190621017475019));
#165082=CARTESIAN_POINT('Origin',(1.94357642212787,0.300127903713799,-9.18589156190818));
#165083=CARTESIAN_POINT('Ctrl Pts',(1.564573096,0.551266351,-7.265146627));
#165084=CARTESIAN_POINT('Ctrl Pts',(1.168819643,0.615380951,-7.350373428));
#165085=CARTESIAN_POINT('Ctrl Pts',(0.766150247,0.680609079,-7.392107838));
#165086=CARTESIAN_POINT('Ctrl Pts',(0.762112289126585,0.681263184913293,
-7.39252634954104));
#165087=CARTESIAN_POINT('Ctrl Pts',(0.758074331253171,0.681917290826587,
-7.39294486108209));
#165088=CARTESIAN_POINT('Ctrl Pts',(1.35465137544855,0.551266351,-7.1223174988109));
#165089=CARTESIAN_POINT('Ctrl Pts',(0.966678236570384,0.615380951,-7.19610925931197));
#165090=CARTESIAN_POINT('Ctrl Pts',(0.572985231706459,0.680609079,-7.22732141540281));
#165091=CARTESIAN_POINT('Ctrl Pts',(0.56903728884194,0.681263184913293,
-7.22763441006465));
#165092=CARTESIAN_POINT('Ctrl Pts',(0.56508934597742,0.681917290826587,
-7.22794740472649));
#165093=CARTESIAN_POINT('Origin',(0.0051808062341413,0.803453412729377,
0.192415877054507));
#165094=CARTESIAN_POINT('Ctrl Pts',(0.416259277961287,0.681884070047882,
-7.42004298029424));
#165095=CARTESIAN_POINT('Ctrl Pts',(0.412229942980644,0.681246574523941,
-7.42026463414712));
#165096=CARTESIAN_POINT('Ctrl Pts',(0.408200608,0.680609079,-7.420486288));
#165097=CARTESIAN_POINT('Ctrl Pts',(0.401759783,0.679590053000001,-7.420840598));
#165098=CARTESIAN_POINT('Ctrl Pts',(0.395318353,0.678571429,-7.421183725));
#165099=CARTESIAN_POINT('Ctrl Pts',(-0.003534487,0.615498301,-7.442430181));
#165100=CARTESIAN_POINT('Ctrl Pts',(-0.402366966,0.551245526,-7.420804897));
#165101=CARTESIAN_POINT('Ctrl Pts',(0.580835096616944,0.681884070047882,
-7.22669998041423));
#165102=CARTESIAN_POINT('Ctrl Pts',(0.576910649808472,0.681246574523941,
-7.22701111220711));
#165103=CARTESIAN_POINT('Ctrl Pts',(0.572986203,0.680609079,-7.227322244));
#165104=CARTESIAN_POINT('Ctrl Pts',(0.56671304,0.679590053000001,-7.227819583));
#165105=CARTESIAN_POINT('Ctrl Pts',(0.560439023,0.678571429,-7.228306033));
#165106=CARTESIAN_POINT('Ctrl Pts',(0.17195243,0.615498301,-7.258426928));
#165107=CARTESIAN_POINT('Ctrl Pts',(-0.217524687,0.551245526,-7.246736025));
#165108=CARTESIAN_POINT('',(-0.212788494622047,0.552026825910877,-7.24687664144778));
#165109=CARTESIAN_POINT('Origin',(0.0288747599038717,0.411147101591151,
0.188828232147965));
#165110=CARTESIAN_POINT('Origin',(-0.0764596409031881,0.29994988413586,
-9.39079447355658));
#165111=CARTESIAN_POINT('Ctrl Pts',(-0.033797522,0.551266351,-7.431628504));
#165112=CARTESIAN_POINT('Ctrl Pts',(-0.438619722,0.615380951,-7.429787455));
#165113=CARTESIAN_POINT('Ctrl Pts',(-0.840846596,0.680609079,-7.38398412));
#165114=CARTESIAN_POINT('Ctrl Pts',(-0.8448801162747,0.681263184913293,
-7.38352480538849));
#165115=CARTESIAN_POINT('Ctrl Pts',(-0.848913636549401,0.681917290826586,
-7.38306549077698));
#165116=CARTESIAN_POINT('Ctrl Pts',(-0.208106472,0.551266351,-7.247012605));
#165117=CARTESIAN_POINT('Ctrl Pts',(-0.602872113,0.615380951,-7.23567644600001));
#165118=CARTESIAN_POINT('Ctrl Pts',(-0.994070541,0.680609079,-7.181526562));
#165119=CARTESIAN_POINT('Ctrl Pts',(-0.997993468314819,0.681263184913293,
-7.1809835484196));
#165120=CARTESIAN_POINT('Ctrl Pts',(-1.00191639562964,0.681917290826586,
-7.18044053483919));
#165121=CARTESIAN_POINT('Origin',(0.0464232560277618,0.803452544100388,
0.186803320626479));
#165122=CARTESIAN_POINT('Ctrl Pts',(-1.18856253854604,0.681884070047882,
-7.33604993996607));
#165123=CARTESIAN_POINT('Ctrl Pts',(-1.19254531877302,0.681246574523941,
-7.33540022348304));
#165124=CARTESIAN_POINT('Ctrl Pts',(-1.196528099,0.680609079,-7.334750507));
#165125=CARTESIAN_POINT('Ctrl Pts',(-1.202894507,0.679590053000001,-7.333711946));
#165126=CARTESIAN_POINT('Ctrl Pts',(-1.209259103,0.678571429,-7.332662334));
#165127=CARTESIAN_POINT('Ctrl Pts',(-1.603354344,0.615498301,-7.267670489));
#165128=CARTESIAN_POINT('Ctrl Pts',(-1.988213545,0.551245526,-7.160813598));
#165129=CARTESIAN_POINT('Ctrl Pts',(-0.986271382025895,0.681884070047882,
-7.18260612530439));
#165130=CARTESIAN_POINT('Ctrl Pts',(-0.990170961512947,0.681246574523941,
-7.18206634365219));
#165131=CARTESIAN_POINT('Ctrl Pts',(-0.994070541000001,0.680609079,-7.18152656200001));
#165132=CARTESIAN_POINT('Ctrl Pts',(-1.000303954,0.679590053000001,-7.18066373));
#165133=CARTESIAN_POINT('Ctrl Pts',(-1.00653586,0.678571429,-7.179790078));
#165134=CARTESIAN_POINT('Ctrl Pts',(-1.392414954,0.615498301,-7.125693629));
#165135=CARTESIAN_POINT('Ctrl Pts',(-1.770273114,0.551245526,-7.030549986));
#165136=CARTESIAN_POINT('Ctrl Pts',(-0.984248470460693,0.681884070047882,
-7.18107168715778));
#165137=CARTESIAN_POINT('Ctrl Pts',(-0.988147217940346,0.681246574523941,
-7.18053300485388));
#165138=CARTESIAN_POINT('Ctrl Pts',(-0.99204596542,0.680609079,-7.17999432255));
#165139=CARTESIAN_POINT('Ctrl Pts',(-0.998278048469998,0.679590053000001,
-7.17913324784));
#165140=CARTESIAN_POINT('Ctrl Pts',(-1.00450862757,0.678571429,-7.17826135544));
#165141=CARTESIAN_POINT('Ctrl Pts',(-1.3903055601,0.615498301,-7.1242738604));
#165142=CARTESIAN_POINT('Ctrl Pts',(-1.76809370969,0.551245526,-7.02924734988));
#165143=CARTESIAN_POINT('',(-1.76567787734294,0.55202682618642,-7.03170545575127));
#165144=CARTESIAN_POINT('Origin',(0.0687923889553491,0.411145011062635,
0.178205687137017));
#165145=CARTESIAN_POINT('Ctrl Pts',(-1.78120945030309,0.562053380603981,
-7.09178521393521));
#165146=CARTESIAN_POINT('Ctrl Pts',(-1.77604503026779,0.558751695424193,
-7.07174861365702));
#165147=CARTESIAN_POINT('Ctrl Pts',(-1.77086804335904,0.555410033626249,
-7.0517217898627));
#165148=CARTESIAN_POINT('Ctrl Pts',(-1.7656778697302,0.552026824831871,
-7.03170545921814));
#165149=CARTESIAN_POINT('Ctrl Pts',(-1.630587806,0.551266351,-7.250615691));
#165150=CARTESIAN_POINT('Ctrl Pts',(-2.025549717,0.615380951,-7.16179287900001));
#165151=CARTESIAN_POINT('Ctrl Pts',(-2.408526387,0.680609079,-7.030593512));
#165152=CARTESIAN_POINT('Ctrl Pts',(-2.41236686674672,0.681263184913293,
-7.02927784827629));
#165153=CARTESIAN_POINT('Ctrl Pts',(-2.41620734649343,0.681917290826587,
-7.02796218455258));
#165154=CARTESIAN_POINT('Ctrl Pts',(-1.761134548,0.551266351,-7.032844738));
#165155=CARTESIAN_POINT('Ctrl Pts',(-2.144233849,0.615380951,-6.936910668));
#165156=CARTESIAN_POINT('Ctrl Pts',(-2.51464565,0.680609079,-6.79993068));
#165157=CARTESIAN_POINT('Ctrl Pts',(-2.51836012957832,0.681263184913293,
-6.79855704836437));
#165158=CARTESIAN_POINT('Ctrl Pts',(-2.52207460915663,0.681917290826587,
-6.79718341672875));
#165159=CARTESIAN_POINT('Origin',(0.0854953302183697,0.803453457522902,
0.172456584285718));
#165160=CARTESIAN_POINT('Ctrl Pts',(-2.73780849035282,0.681884070047882,
-6.90903135754418));
#165161=CARTESIAN_POINT('Ctrl Pts',(-2.74155848617641,0.681246574523941,
-6.90754065077208));
#165162=CARTESIAN_POINT('Ctrl Pts',(-2.745308482,0.680609079,-6.906049944));
#165163=CARTESIAN_POINT('Ctrl Pts',(-2.751302788,0.679590053000001,-6.903667074));
#165164=CARTESIAN_POINT('Ctrl Pts',(-2.757292947,0.678571429,-6.901273802));
#165165=CARTESIAN_POINT('Ctrl Pts',(-3.128203135,0.615498301,-6.753082602));
#165166=CARTESIAN_POINT('Ctrl Pts',(-3.481093468,0.551245526,-6.565990615));
#165167=CARTESIAN_POINT('Ctrl Pts',(-2.50726090509375,0.681884070047882,
-6.80266159234725));
#165168=CARTESIAN_POINT('Ctrl Pts',(-2.51095327754687,0.681246574523941,
-6.80129613617363));
#165169=CARTESIAN_POINT('Ctrl Pts',(-2.51464565,0.680609079,-6.79993068000001));
#165170=CARTESIAN_POINT('Ctrl Pts',(-2.520547846,0.679590053000001,-6.797748021));
#165171=CARTESIAN_POINT('Ctrl Pts',(-2.526446244,0.678571429,-6.795555119));
#165172=CARTESIAN_POINT('Ctrl Pts',(-2.891674563,0.615498301,-6.659770816));
#165173=CARTESIAN_POINT('Ctrl Pts',(-3.240245538,0.551245526,-6.485623243));
#165174=CARTESIAN_POINT('',(-3.23600612945469,0.552026825943996,-6.48773953932139));
#165175=CARTESIAN_POINT('Origin',(0.10549294900999,0.411147121408226,0.159251690106229));
#165176=CARTESIAN_POINT('Origin',(-4.01239744936829,0.29999615904035,-8.49054704910549));
#165177=CARTESIAN_POINT('Ctrl Pts',(-3.151133616,0.551266351,-6.730572147));
#165178=CARTESIAN_POINT('Ctrl Pts',(-3.517767258,0.615380951,-6.558920827));
#165179=CARTESIAN_POINT('Ctrl Pts',(-3.86358616,0.680609079,-6.348460165));
#165180=CARTESIAN_POINT('Ctrl Pts',(-3.86705402264856,0.681263184913293,
-6.34634967114174));
#165181=CARTESIAN_POINT('Ctrl Pts',(-3.87052188529712,0.681917290826587,
-6.34423917728348));
#165182=CARTESIAN_POINT('Ctrl Pts',(-3.231813931,0.551266351,-6.489828867));
#165183=CARTESIAN_POINT('Ctrl Pts',(-3.585333593,0.615380951,-6.313782657));
#165184=CARTESIAN_POINT('Ctrl Pts',(-3.917638724,0.680609079,-6.100377597));
#165185=CARTESIAN_POINT('Ctrl Pts',(-3.92097107091642,0.681263184913293,
-6.09823757679779));
#165186=CARTESIAN_POINT('Ctrl Pts',(-3.92430341783284,0.681917290826586,
-6.09609755659558));
#165187=CARTESIAN_POINT('Origin',(0.120569400091427,0.8034525034028,0.15004570042049));
#165188=CARTESIAN_POINT('Ctrl Pts',(-4.15903756282769,0.681884070047881,
-6.15895414672883));
#165189=CARTESIAN_POINT('Ctrl Pts',(-4.16237942741384,0.681246574523941,
-6.15669215386441));
#165190=CARTESIAN_POINT('Ctrl Pts',(-4.165721292,0.680609079,-6.154430161));
#165191=CARTESIAN_POINT('Ctrl Pts',(-4.171063207,0.679590053000001,-6.150814403));
#165192=CARTESIAN_POINT('Ctrl Pts',(-4.176398838,0.678571429,-6.147189377));
#165193=CARTESIAN_POINT('Ctrl Pts',(-4.506780624,0.615498301,-5.922728079));
#165194=CARTESIAN_POINT('Ctrl Pts',(-4.811201331,0.551245526,-5.664149207));
#165195=CARTESIAN_POINT('Ctrl Pts',(-3.91101369546929,0.681884070047881,
-6.10463216359984));
#165196=CARTESIAN_POINT('Ctrl Pts',(-3.91432620973464,0.681246574523941,
-6.10250488029992));
#165197=CARTESIAN_POINT('Ctrl Pts',(-3.917638724,0.680609079,-6.100377597));
#165198=CARTESIAN_POINT('Ctrl Pts',(-3.922933723,0.679590053000001,-6.09697717));
#165199=CARTESIAN_POINT('Ctrl Pts',(-3.928222811,0.678571429,-6.093567555));
#165200=CARTESIAN_POINT('Ctrl Pts',(-4.255722683,0.615498301,-5.882444522));
#165201=CARTESIAN_POINT('Ctrl Pts',(-4.558707681,0.551245526,-5.637435967));
#165202=CARTESIAN_POINT('Ctrl Pts',(-3.9085334567957,0.681884070047881,
-6.10408894376855));
#165203=CARTESIAN_POINT('Ctrl Pts',(-3.91184567755785,0.681246574523941,
-6.10196300756427));
#165204=CARTESIAN_POINT('Ctrl Pts',(-3.91515789832,0.680609079,-6.09983707136001));
#165205=CARTESIAN_POINT('Ctrl Pts',(-3.92045242816,0.679590053000001,-6.09643879767));
#165206=CARTESIAN_POINT('Ctrl Pts',(-3.92574105073,0.678571429,-6.09303133678));
#165207=CARTESIAN_POINT('Ctrl Pts',(-4.25321210359,0.615498301,-5.88204168643001));
#165208=CARTESIAN_POINT('Ctrl Pts',(-4.55618274449999,0.551245526,-5.6371688346));
#165209=CARTESIAN_POINT('',(-4.55502232513917,0.552026826178051,-5.64041413373297));
#165210=CARTESIAN_POINT('Origin',(0.137260940792053,0.411144919528123,0.132849950390427));
#165211=CARTESIAN_POINT('Ctrl Pts',(-4.59434523690511,0.562053380745924,
-5.68841950546675));
#165212=CARTESIAN_POINT('Ctrl Pts',(-4.58124498540839,0.558751695407189,
-5.67240326384358));
#165213=CARTESIAN_POINT('Ctrl Pts',(-4.56813743426761,0.555410033596466,
-5.65640117123746));
#165214=CARTESIAN_POINT('Ctrl Pts',(-4.55502232113666,0.552026824779272,
-5.64041413851911));
#165215=CARTESIAN_POINT('Ctrl Pts',(-4.52433592,0.551266351,-5.89581453));
#165216=CARTESIAN_POINT('Ctrl Pts',(-4.845497912,0.615380951,-5.649360927));
#165217=CARTESIAN_POINT('Ctrl Pts',(-5.13798893900001,0.680609079,-5.369479877));
#165218=CARTESIAN_POINT('Ctrl Pts',(-5.1409220311523,0.681263184913293,
-5.36667323735792));
#165219=CARTESIAN_POINT('Ctrl Pts',(-5.1438551233046,0.681917290826586,
-5.36386659771584));
#165220=CARTESIAN_POINT('Ctrl Pts',(-4.551377285,0.551266351,-5.643355811));
#165221=CARTESIAN_POINT('Ctrl Pts',(-4.858787124,0.615380951,-5.395429187));
#165222=CARTESIAN_POINT('Ctrl Pts',(-5.137447365,0.680609079,-5.115577638));
#165223=CARTESIAN_POINT('Ctrl Pts',(-5.14024176240226,0.681263184913293,
-5.11277129419315));
#165224=CARTESIAN_POINT('Ctrl Pts',(-5.14303615980453,0.681917290826586,
-5.10996495038631));
#165225=CARTESIAN_POINT('Origin',(0.150005998797879,0.803453479443192,0.120618687140587));
#165226=CARTESIAN_POINT('Ctrl Pts',(-5.3857946597887,0.681884070047877,
-5.12089108640163));
#165227=CARTESIAN_POINT('Ctrl Pts',(-5.38857213189434,0.681246574523938,
-5.11796357520081));
#165228=CARTESIAN_POINT('Ctrl Pts',(-5.39134960400001,0.680609079,-5.115036064));
#165229=CARTESIAN_POINT('Ctrl Pts',(-5.395789347,0.679590053,-5.11035648600001));
#165230=CARTESIAN_POINT('Ctrl Pts',(-5.40022096,0.678571429,-5.105669209));
#165231=CARTESIAN_POINT('Ctrl Pts',(-5.67462606,0.615498301,-4.815433373));
#165232=CARTESIAN_POINT('Ctrl Pts',(-5.916342766,0.551245526,-4.497458479));
#165233=CARTESIAN_POINT('Ctrl Pts',(-5.13189183273128,0.681884070047877,
-5.12115692153225));
#165234=CARTESIAN_POINT('Ctrl Pts',(-5.13466959886564,0.681246574523938,
-5.11836727976612));
#165235=CARTESIAN_POINT('Ctrl Pts',(-5.137447365,0.680609079,-5.115577638));
#165236=CARTESIAN_POINT('Ctrl Pts',(-5.141887578,0.679590053,-5.111118442));
#165237=CARTESIAN_POINT('Ctrl Pts',(-5.146320044,0.678571429,-5.106651545));
#165238=CARTESIAN_POINT('Ctrl Pts',(-5.42077794,0.615498301,-4.830061659));
#165239=CARTESIAN_POINT('Ctrl Pts',(-5.66400972,0.551245526,-4.525648449));
#165240=CARTESIAN_POINT('',(-5.6610507458468,0.552026825822157,-4.52934923041454));
#165241=CARTESIAN_POINT('Origin',(0.162610771491941,0.411147080989508,0.100237490144345));
#165242=CARTESIAN_POINT('Origin',(-7.20657778905468,0.300004052182154,-6.02097698757969));
#165243=CARTESIAN_POINT('Ctrl Pts',(-5.685985305,0.551266351,-4.785375178));
#165244=CARTESIAN_POINT('Ctrl Pts',(-5.946658468,0.615380951,-4.475643188));
#165245=CARTESIAN_POINT('Ctrl Pts',(-6.172145066,0.680609079,-4.139428677));
#165246=CARTESIAN_POINT('Ctrl Pts',(-6.17440623954035,0.681263184913293,
-4.13605712692608));
#165247=CARTESIAN_POINT('Ctrl Pts',(-6.1766674130807,0.681917290826586,
-4.13268557685216));
#165248=CARTESIAN_POINT('Ctrl Pts',(-5.65812315589465,0.551266351,-4.53300444094894));
#165249=CARTESIAN_POINT('Ctrl Pts',(-5.9050489587658,0.615380951,-4.22479018258088));
#165250=CARTESIAN_POINT('Ctrl Pts',(-6.11703440087497,0.680609079,-3.89157770767668));
#165251=CARTESIAN_POINT('Ctrl Pts',(-6.11916018518716,0.681263184913293,
-3.88823626193999));
#165252=CARTESIAN_POINT('Ctrl Pts',(-6.12128596949935,0.681917290826586,
-3.8848948162033));
#165253=CARTESIAN_POINT('Origin',(0.172428499853304,0.803453447950604,0.0855519229008006));
#165254=CARTESIAN_POINT('Ctrl Pts',(-6.36071798545744,0.681884070047877,
-3.84338084831586));
#165255=CARTESIAN_POINT('Ctrl Pts',(-6.36280119322872,0.681246574523938,
-3.83992470665794));
#165256=CARTESIAN_POINT('Ctrl Pts',(-6.364884401,0.680609079,-3.836468565));
#165257=CARTESIAN_POINT('Ctrl Pts',(-6.368214374,0.679590053,-3.83094398));
#165258=CARTESIAN_POINT('Ctrl Pts',(-6.371534752,0.678571429,-3.825413623));
#165259=CARTESIAN_POINT('Ctrl Pts',(-6.577132288,0.615498301,-3.482974354));
#165260=CARTESIAN_POINT('Ctrl Pts',(-6.744842588,0.551245526,-3.12047159));
#165261=CARTESIAN_POINT('Ctrl Pts',(-6.11280841197592,0.681884070047877,
-3.89822207217764));
#165262=CARTESIAN_POINT('Ctrl Pts',(-6.11492154498796,0.681246574523938,
-3.89490051308882));
#165263=CARTESIAN_POINT('Ctrl Pts',(-6.117034678,0.680609079,-3.891578954));
#165264=CARTESIAN_POINT('Ctrl Pts',(-6.120412486,0.679590053,-3.886269497));
#165265=CARTESIAN_POINT('Ctrl Pts',(-6.123781072,0.678571429,-3.880954185));
#165266=CARTESIAN_POINT('Ctrl Pts',(-6.332363645,0.615498301,-3.551830482));
#165267=CARTESIAN_POINT('Ctrl Pts',(-6.50446896,0.551245526,-3.202246641));
#165268=CARTESIAN_POINT('',(-6.5023747244165,0.552026825926503,-3.2064969894312));
#165269=CARTESIAN_POINT('Origin',(0.180357310691638,0.411147121182753,0.0629375996474091));
#165270=CARTESIAN_POINT('Origin',(-8.33121035929084,0.300112759031273,-4.33028420864262));
#165271=CARTESIAN_POINT('Ctrl Pts',(-6.581764337,0.551266351,-3.451177002));
#165272=CARTESIAN_POINT('Ctrl Pts',(-6.769759885,0.615380951,-3.092649349));
#165273=CARTESIAN_POINT('Ctrl Pts',(-6.917698549,0.680609079,-2.715822393));
#165274=CARTESIAN_POINT('Ctrl Pts',(-6.91918207394382,0.681263184913293,
-2.71204358241988));
#165275=CARTESIAN_POINT('Ctrl Pts',(-6.92066559888766,0.681917290826586,
-2.70826477183976));
#165276=CARTESIAN_POINT('Ctrl Pts',(-6.50030134042989,0.551266351,-3.21069608698621));
#165277=CARTESIAN_POINT('Ctrl Pts',(-6.675197199408,0.615380951,-2.85660595835115));
#165278=CARTESIAN_POINT('Ctrl Pts',(-6.81059570720614,0.680609079,-2.48561320275527));
#165279=CARTESIAN_POINT('Ctrl Pts',(-6.81195347980084,0.681263184913293,
-2.48189289737989));
#165280=CARTESIAN_POINT('Ctrl Pts',(-6.81331125239553,0.681917290826586,
-2.47817259200452));
#165281=CARTESIAN_POINT('Origin',(0.186785362021775,0.803452743019938,0.0464835788768353));
#165282=CARTESIAN_POINT('Ctrl Pts',(-7.03822120603974,0.681884070047877,
-2.38615839511332));
#165283=CARTESIAN_POINT('Ctrl Pts',(-7.03951274151987,0.681246574523938,
-2.38233522805666));
#165284=CARTESIAN_POINT('Ctrl Pts',(-7.040804277,0.680609079,-2.378512061));
#165285=CARTESIAN_POINT('Ctrl Pts',(-7.042868775,0.679590053,-2.372400792));
#165286=CARTESIAN_POINT('Ctrl Pts',(-7.044922661,0.678571429,-2.366285948));
#165287=CARTESIAN_POINT('Ctrl Pts',(-7.17209912,0.615498301,-1.987655326));
#165288=CARTESIAN_POINT('Ctrl Pts',(-7.257961068,0.551245526,-1.597574918));
#165289=CARTESIAN_POINT('Ctrl Pts',(-6.80789686203716,0.681884070047877,
-2.49301069013488));
#165290=CARTESIAN_POINT('Ctrl Pts',(-6.80924655451858,0.681246574523938,
-2.48931252656744));
#165291=CARTESIAN_POINT('Ctrl Pts',(-6.810596247,0.680609079,-2.485614363));
#165292=CARTESIAN_POINT('Ctrl Pts',(-6.81275370800001,0.679590053,-2.47970291));
#165293=CARTESIAN_POINT('Ctrl Pts',(-6.814900903,0.678571429,-2.47378772));
#165294=CARTESIAN_POINT('Ctrl Pts',(-6.947855064,0.615498301,-2.107519659));
#165295=CARTESIAN_POINT('Ctrl Pts',(-7.04078646,0.551245526,-1.729111338));
#165296=CARTESIAN_POINT('Ctrl Pts',(-6.80559361859714,0.681884070047877,
-2.49407921308509));
#165297=CARTESIAN_POINT('Ctrl Pts',(-6.80694389264857,0.681246574523938,
-2.49038229955254));
#165298=CARTESIAN_POINT('Ctrl Pts',(-6.80829416669999,0.680609079,-2.48668538602));
#165299=CARTESIAN_POINT('Ctrl Pts',(-6.81045255733,0.679590053,-2.48077593118));
#165300=CARTESIAN_POINT('Ctrl Pts',(-6.81260068542,0.678571429,-2.47486273772));
#165301=CARTESIAN_POINT('Ctrl Pts',(-6.94561262344,0.615498301,-2.10871830233));
#165302=CARTESIAN_POINT('Ctrl Pts',(-7.03861471392,0.551245526,-1.7304267022));
#165303=CARTESIAN_POINT('',(-7.03965488398797,0.552026826194493,-1.73371251862539));
#165304=CARTESIAN_POINT('Origin',(0.189669970752134,0.411144947754553,0.0226941808511896));
#165305=CARTESIAN_POINT('Ctrl Pts',(-7.10001119453425,0.562053380786607,
-1.74813204994719));
#165306=CARTESIAN_POINT('Ctrl Pts',(-7.07988955854266,0.55875169543278,
-1.74330956532491));
#165307=CARTESIAN_POINT('Ctrl Pts',(-7.05977067420358,0.555410033642667,
-1.73850276224255));
#165308=CARTESIAN_POINT('Ctrl Pts',(-7.0396548836752,0.552026824799611,
-1.7337125249341));
#165309=CARTESIAN_POINT('Ctrl Pts',(-7.169787384,0.551266351,-1.955605624));
#165310=CARTESIAN_POINT('Ctrl Pts',(-7.276314852,0.615380951,-1.565046663));
#165311=CARTESIAN_POINT('Ctrl Pts',(-7.339788137,0.680609079,-1.165227272));
#165312=CARTESIAN_POINT('Ctrl Pts',(-7.34042464539488,0.681263184913293,
-1.16121789390008));
#165313=CARTESIAN_POINT('Ctrl Pts',(-7.34106115378977,0.681917290826586,
-1.15720851580015));
#165314=CARTESIAN_POINT('Ctrl Pts',(-7.03853332,0.551266351,-1.738260252));
#165315=CARTESIAN_POINT('Ctrl Pts',(-7.13322136,0.615380951,-1.354851078));
#165316=CARTESIAN_POINT('Ctrl Pts',(-7.185701905,0.680609079,-0.963425207));
#165317=CARTESIAN_POINT('Ctrl Pts',(-7.18622817849381,0.681263184913293,
-0.959499998892894));
#165318=CARTESIAN_POINT('Ctrl Pts',(-7.18675445198762,0.681917290826586,
-0.955574790785788));
#165319=CARTESIAN_POINT('Origin',(0.192414180828946,0.803453416295806,0.00524397244476754));
#165320=CARTESIAN_POINT('Ctrl Pts',(-7.38662502560974,0.681884070047877,
-0.817361827008927));
#165321=CARTESIAN_POINT('Ctrl Pts',(-7.38706449780487,0.681246574523938,
-0.813350401504463));
#165322=CARTESIAN_POINT('Ctrl Pts',(-7.38750397,0.680609079,-0.809338976000001));
#165323=CARTESIAN_POINT('Ctrl Pts',(-7.388206459,0.679590053,-0.802926779));
#165324=CARTESIAN_POINT('Ctrl Pts',(-7.388897816,0.678571429,-0.796513372));
#165325=CARTESIAN_POINT('Ctrl Pts',(-7.431706569,0.615498301,-0.399395744));
#165326=CARTESIAN_POINT('Ctrl Pts',(-7.431705355,0.551245526,2.2582E-5));
#165327=CARTESIAN_POINT('Ctrl Pts',(-7.18465562199158,0.681884070047877,
-0.971228900272081));
#165328=CARTESIAN_POINT('Ctrl Pts',(-7.18517876349579,0.681246574523938,
-0.967327053636041));
#165329=CARTESIAN_POINT('Ctrl Pts',(-7.185701905,0.680609079,-0.963425207));
#165330=CARTESIAN_POINT('Ctrl Pts',(-7.186538138,0.679590053,-0.95718817));
#165331=CARTESIAN_POINT('Ctrl Pts',(-7.187363542,0.678571429,-0.95094969));
#165332=CARTESIAN_POINT('Ctrl Pts',(-7.238472502,0.615498301,-0.564663559));
#165333=CARTESIAN_POINT('Ctrl Pts',(-7.247884611,0.551245526,-0.175124711));
#165334=CARTESIAN_POINT('Ctrl Pts',(-7.1826359279554,0.681884070047877,
-0.972767571004713));
#165335=CARTESIAN_POINT('Ctrl Pts',(-7.1831599061527,0.681246574523938,
-0.968866820157356));
#165336=CARTESIAN_POINT('Ctrl Pts',(-7.18368388435,0.680609079,-0.96496606931));
#165337=CARTESIAN_POINT('Ctrl Pts',(-7.18452145479,0.679590053,-0.95873078391));
#165338=CARTESIAN_POINT('Ctrl Pts',(-7.18534819926,0.678571429,-0.95249405318));
#165339=CARTESIAN_POINT('Ctrl Pts',(-7.23654016133,0.615498301,-0.56631623715));
#165340=CARTESIAN_POINT('Ctrl Pts',(-7.24604640356,0.551245526,-0.17687618393));
#165341=CARTESIAN_POINT('',(-7.24776860903089,0.552026825761896,-0.179861574595068));
#165342=CARTESIAN_POINT('Origin',(0.19011403374817,0.411144969445827,-0.0186098427601895));
#165343=CARTESIAN_POINT('Ctrl Pts',(-7.30981359466473,0.56205338065316,
-0.180969162687403));
#165344=CARTESIAN_POINT('Ctrl Pts',(-7.28912569973217,0.558751695414249,
-0.180584981340033));
#165345=CARTESIAN_POINT('Ctrl Pts',(-7.26844386309386,0.555410033612152,
-0.180215524115213));
#165346=CARTESIAN_POINT('Ctrl Pts',(-7.24776860924737,0.552026824727703,
-0.1798615806622));
#165347=CARTESIAN_POINT('Ctrl Pts',(-7.422559141,0.551266351,-0.368592301));
#165348=CARTESIAN_POINT('Ctrl Pts',(-7.442637425,0.615380951,0.035735865));
#165349=CARTESIAN_POINT('Ctrl Pts',(-7.418677388,0.680609079,0.439852581));
#165350=CARTESIAN_POINT('Ctrl Pts',(-7.41843711739337,0.681263184913293,
0.44390505255945));
#165351=CARTESIAN_POINT('Ctrl Pts',(-7.41819684678672,0.681917290826586,
0.4479575241189));
#165352=CARTESIAN_POINT('Ctrl Pts',(-7.247650894,0.551266351,-0.184544087));
#165353=CARTESIAN_POINT('Ctrl Pts',(-7.257703542,0.615380951,0.210256324));
#165354=CARTESIAN_POINT('Ctrl Pts',(-7.224812129,0.680609079,0.603812641));
#165355=CARTESIAN_POINT('Ctrl Pts',(-7.22448229479504,0.681263184913293,
0.607759213162297));
#165356=CARTESIAN_POINT('Ctrl Pts',(-7.22415246059009,0.681917290826586,
0.611705785324594));
#165357=CARTESIAN_POINT('Origin',(0.189042798006385,0.803453447834286,-0.0362419934487183));
#165358=CARTESIAN_POINT('Ctrl Pts',(-7.38963847013693,0.681884070047877,
0.789653671435307));
#165359=CARTESIAN_POINT('Ctrl Pts',(-7.38920532956846,0.681246574523939,
0.793665785717654));
#165360=CARTESIAN_POINT('Ctrl Pts',(-7.388772189,0.680609079,0.797677900000001));
#165361=CARTESIAN_POINT('Ctrl Pts',(-7.388079821,0.679590053,0.804091198));
#165362=CARTESIAN_POINT('Ctrl Pts',(-7.387376321,0.678571429,0.810503285));
#165363=CARTESIAN_POINT('Ctrl Pts',(-7.343815678,0.615498301,1.207539139));
#165364=CARTESIAN_POINT('Ctrl Pts',(-7.257951359,0.551245526,1.597619026));
#165365=CARTESIAN_POINT('Ctrl Pts',(-7.22546787182032,0.681884070047877,
0.595966473717341));
#165366=CARTESIAN_POINT('Ctrl Pts',(-7.22514000041016,0.681246574523939,
0.599889557358671));
#165367=CARTESIAN_POINT('Ctrl Pts',(-7.224812129,0.680609079,0.603812641));
#165368=CARTESIAN_POINT('Ctrl Pts',(-7.224288032,0.679590053,0.610083625));
#165369=CARTESIAN_POINT('Ctrl Pts',(-7.22375305,0.678571429,0.616353689));
#165370=CARTESIAN_POINT('Ctrl Pts',(-7.190627011,0.615498301,1.004595582));
#165371=CARTESIAN_POINT('Ctrl Pts',(-7.116079733,0.551245526,1.387050553));
#165372=CARTESIAN_POINT('',(-7.11698472798904,0.552026825929822,1.38239950192524));
#165373=CARTESIAN_POINT('Origin',(0.181669495499602,0.411147110446777,-0.0590434112763613));
#165374=CARTESIAN_POINT('Origin',(-9.25290503811619,0.3001208526991,1.5945150383709));
#165375=CARTESIAN_POINT('Ctrl Pts',(-7.328260282,0.551266351,1.235655988));
#165376=CARTESIAN_POINT('Ctrl Pts',(-7.260950543,0.615380951,1.634847424));
#165377=CARTESIAN_POINT('Ctrl Pts',(-7.150677531,0.680609079,2.024365416));
#165378=CARTESIAN_POINT('Ctrl Pts',(-7.14957171620143,0.681263184913293,
2.02827149194781));
#165379=CARTESIAN_POINT('Ctrl Pts',(-7.14846590140285,0.681917290826586,
2.03217756789561));
#165380=CARTESIAN_POINT('Ctrl Pts',(-7.117876367,0.551266351,1.377801155));
#165381=CARTESIAN_POINT('Ctrl Pts',(-7.042823572,0.615380951,1.765532373));
#165382=CARTESIAN_POINT('Ctrl Pts',(-6.926098167,0.680609079,2.14281688));
#165383=CARTESIAN_POINT('Ctrl Pts',(-6.92492764777796,0.681263184913293,
2.14660027888924));
#165384=CARTESIAN_POINT('Ctrl Pts',(-6.92375712855592,0.681917290826586,
2.15038367777849));
#165385=CARTESIAN_POINT('Origin',(0.176832129022559,0.803453450864247,-0.076033285388003));
#165386=CARTESIAN_POINT('Ctrl Pts',(-7.04712062926672,0.681884070047877,
2.35974584228104));
#165387=CARTESIAN_POINT('Ctrl Pts',(-7.04583513013336,0.681246574523938,
2.36357104314052));
#165388=CARTESIAN_POINT('Ctrl Pts',(-7.044549631,0.680609079,2.367396244));
#165389=CARTESIAN_POINT('Ctrl Pts',(-7.042494782,0.679590053,2.373510764));
#165390=CARTESIAN_POINT('Ctrl Pts',(-7.04042932,0.678571429,2.379621708));
#165391=CARTESIAN_POINT('Ctrl Pts',(-6.912536128,0.615498301,2.758010834));
#165392=CARTESIAN_POINT('Ctrl Pts',(-6.744823625,0.551245526,3.120512579));
#165393=CARTESIAN_POINT('Ctrl Pts',(-6.92842527283416,0.681884070047877,
2.13529511646555));
#165394=CARTESIAN_POINT('Ctrl Pts',(-6.92726171991709,0.681246574523938,
2.13905599823278));
#165395=CARTESIAN_POINT('Ctrl Pts',(-6.926098167,0.680609079,2.14281688));
#165396=CARTESIAN_POINT('Ctrl Pts',(-6.924238247,0.679590053,2.148828587));
#165397=CARTESIAN_POINT('Ctrl Pts',(-6.922367894,0.678571429,2.154837056));
#165398=CARTESIAN_POINT('Ctrl Pts',(-6.806555793,0.615498301,2.52688095));
#165399=CARTESIAN_POINT('Ctrl Pts',(-6.651534875,0.551245526,2.884368874));
#165400=CARTESIAN_POINT('',(-6.65341855000146,0.552026825966217,2.88002111040086));
#165401=CARTESIAN_POINT('Origin',(0.164729494829702,0.41114705736095,-0.0967165698653411));
#165402=CARTESIAN_POINT('Origin',(-8.69290291336178,0.300210269161947,3.54603265013523));
#165403=CARTESIAN_POINT('Ctrl Pts',(-6.891300118,0.551266351,2.782126377));
#165404=CARTESIAN_POINT('Ctrl Pts',(-6.739749684,0.615380951,3.157515334));
#165405=CARTESIAN_POINT('Ctrl Pts',(-6.548319939,0.680609079,3.514221174));
#165406=CARTESIAN_POINT('Ctrl Pts',(-6.54640028666558,0.681263184913293,
3.51779821057002));
#165407=CARTESIAN_POINT('Ctrl Pts',(-6.54448063433117,0.681917290826586,
3.52137524714005));
#165408=CARTESIAN_POINT('Ctrl Pts',(-6.6552766650606,0.551266351,2.87572241568554));
#165409=CARTESIAN_POINT('Ctrl Pts',(-6.49862778642101,0.615380951,3.23825449702954));
#165410=CARTESIAN_POINT('Ctrl Pts',(-6.30352632195629,0.680609079,3.58162572297104));
#165411=CARTESIAN_POINT('Ctrl Pts',(-6.30156984971784,0.681263184913293,
3.58506904038991));
#165412=CARTESIAN_POINT('Ctrl Pts',(-6.29961337747937,0.681917290826586,
3.58851235780879));
#165413=CARTESIAN_POINT('Origin',(0.156352826938365,0.803453443858178,-0.112269264913561));
#165414=CARTESIAN_POINT('Ctrl Pts',(-6.37508726444698,0.6818840700478,3.81949892020932));
#165415=CARTESIAN_POINT('Ctrl Pts',(-6.37300951372349,0.6812465745239,3.82295834560466));
#165416=CARTESIAN_POINT('Ctrl Pts',(-6.370931763,0.680609079,3.826417771));
#165417=CARTESIAN_POINT('Ctrl Pts',(-6.367610513,0.679590053,3.831947605));
#165418=CARTESIAN_POINT('Ctrl Pts',(-6.364279669,0.678571429,3.837471665));
#165419=CARTESIAN_POINT('Ctrl Pts',(-6.158034072,0.615498301,4.179521008));
#165420=CARTESIAN_POINT('Ctrl Pts',(-5.916315434,0.551245526,4.497494433));
#165421=CARTESIAN_POINT('Ctrl Pts',(-6.30741720870518,0.6818840700478,3.57477973384528));
#165422=CARTESIAN_POINT('Ctrl Pts',(-6.30547238085259,0.6812465745239,3.57820255892264));
#165423=CARTESIAN_POINT('Ctrl Pts',(-6.303527553,0.680609079,3.581625384));
#165424=CARTESIAN_POINT('Ctrl Pts',(-6.300418778,0.679590053,3.587096713));
#165425=CARTESIAN_POINT('Ctrl Pts',(-6.297300509,0.678571429,3.592562637));
#165426=CARTESIAN_POINT('Ctrl Pts',(-6.104217591,0.615498301,3.931012172));
#165427=CARTESIAN_POINT('Ctrl Pts',(-5.875971639,0.551245526,4.246817313));
#165428=CARTESIAN_POINT('',(-5.87874591598725,0.55202682617333,4.24297613144422));
#165429=CARTESIAN_POINT('Origin',(0.140086964193408,0.41114707159739,-0.129867334927797));
#165430=CARTESIAN_POINT('Origin',(-7.72986673852935,0.299963142155406,5.33334906303783));
#165431=CARTESIAN_POINT('Ctrl Pts',(-6.132110419,0.551266351,4.198507628));
#165432=CARTESIAN_POINT('Ctrl Pts',(-5.903405621,0.615380951,4.532541337));
#165433=CARTESIAN_POINT('Ctrl Pts',(-5.63977018500001,0.680609079,4.839755856));
#165434=CARTESIAN_POINT('Ctrl Pts',(-5.63712645593819,0.681263184913293,
4.84283659493409));
#165435=CARTESIAN_POINT('Ctrl Pts',(-5.63448272687637,0.681917290826586,
4.84591733386818));
#165436=CARTESIAN_POINT('Ctrl Pts',(-5.88148467891931,0.551266351,4.23917737896369));
#165437=CARTESIAN_POINT('Ctrl Pts',(-5.65056448275435,0.615380951,4.55955878216005));
#165438=CARTESIAN_POINT('Ctrl Pts',(-5.38620971812914,0.680609079,4.85296113255075));
#165439=CARTESIAN_POINT('Ctrl Pts',(-5.38355877565923,0.681263184913293,
4.85590336342949));
#165440=CARTESIAN_POINT('Ctrl Pts',(-5.38090783318931,0.681917290826586,
4.85884559430824));
#165441=CARTESIAN_POINT('Origin',(0.128560471524454,0.803452719747683,-0.143253674220777));
#165442=CARTESIAN_POINT('Ctrl Pts',(-5.40496190144401,0.68188407004776,
5.10065647404584));
#165443=CARTESIAN_POINT('Ctrl Pts',(-5.402189053722,0.68124657452388,5.10358836502292));
#165444=CARTESIAN_POINT('Ctrl Pts',(-5.399416206,0.680609079,5.106520256));
#165445=CARTESIAN_POINT('Ctrl Pts',(-5.394983855,0.679590053,5.111206835));
#165446=CARTESIAN_POINT('Ctrl Pts',(-5.390543374,0.678571429,5.115885712));
#165447=CARTESIAN_POINT('Ctrl Pts',(-5.115589186,0.615498301,5.405601425));
#165448=CARTESIAN_POINT('Ctrl Pts',(-4.811166908,0.551245526,5.664178446));
#165449=CARTESIAN_POINT('Ctrl Pts',(-5.39148132667926,0.68188407004776,
4.84711162513958));
#165450=CARTESIAN_POINT('Ctrl Pts',(-5.38884616133964,0.68124657452388,
4.8500363455698));
#165451=CARTESIAN_POINT('Ctrl Pts',(-5.386210996,0.680609079,4.852961066));
#165452=CARTESIAN_POINT('Ctrl Pts',(-5.381998728,0.679590053,4.857636183));
#165453=CARTESIAN_POINT('Ctrl Pts',(-5.377778351,0.678571429,4.862303981));
#165454=CARTESIAN_POINT('Ctrl Pts',(-5.116452959,0.615498301,5.15133363500001));
#165455=CARTESIAN_POINT('Ctrl Pts',(-4.825654501,0.551245526,5.410689294));
#165456=CARTESIAN_POINT('',(-4.82918965659591,0.552026825962079,5.4075343052009));
#165457=CARTESIAN_POINT('Origin',(0.108894174443853,0.411147075198583,-0.156945658187523));
#165458=CARTESIAN_POINT('Origin',(-6.40110697697016,0.300136499740306,6.86890405535685));
#165459=CARTESIAN_POINT('Ctrl Pts',(-5.086190052,0.551266351,5.418571329));
#165460=CARTESIAN_POINT('Ctrl Pts',(-4.791024871,0.615380951,5.695630744));
#165461=CARTESIAN_POINT('Ctrl Pts',(-4.467511046,0.680609079,5.938988933));
#165462=CARTESIAN_POINT('Ctrl Pts',(-4.46426685806371,0.681263184913293,
5.94142932237425));
#165463=CARTESIAN_POINT('Ctrl Pts',(-4.46102267012741,0.681917290826586,
5.94386971174849));
#165464=CARTESIAN_POINT('Ctrl Pts',(-4.83268101123186,0.551266351,5.40441311780555));
#165465=CARTESIAN_POINT('Ctrl Pts',(-4.53828706911003,0.615380951,5.66766316636527));
#165466=CARTESIAN_POINT('Ctrl Pts',(-4.21703993950809,0.680609079,5.89737747275712));
#165467=CARTESIAN_POINT('Ctrl Pts',(-4.21381848193228,0.681263184913293,
5.89968104164352));
#165468=CARTESIAN_POINT('Ctrl Pts',(-4.21059702435648,0.681917290826586,
5.90198461052992));
#165469=CARTESIAN_POINT('Origin',(0.0947614322425405,0.803453435370911,
-0.167543794197096));
#165470=CARTESIAN_POINT('Ctrl Pts',(-4.18210652789464,0.681884070047697,
6.14331299852755));
#165471=CARTESIAN_POINT('Ctrl Pts',(-4.17876823794732,0.681246574523849,
6.14558026326377));
#165472=CARTESIAN_POINT('Ctrl Pts',(-4.175429948,0.680609079,6.14784752800001));
#165473=CARTESIAN_POINT('Ctrl Pts',(-4.170093747,0.679590053,6.151471713));
#165474=CARTESIAN_POINT('Ctrl Pts',(-4.164751262,0.678571429,6.155086629));
#165475=CARTESIAN_POINT('Ctrl Pts',(-3.833945036,0.615498301,6.378921927));
#165476=CARTESIAN_POINT('Ctrl Pts',(-3.481053566,0.551245526,6.56601177));
#165477=CARTESIAN_POINT('Ctrl Pts',(-4.22344576855952,0.681884070047697,
5.8927979621922));
#165478=CARTESIAN_POINT('Ctrl Pts',(-4.22024348377976,0.681246574523849,
5.8950878220961));
#165479=CARTESIAN_POINT('Ctrl Pts',(-4.217041199,0.680609079,5.897377682));
#165480=CARTESIAN_POINT('Ctrl Pts',(-4.2119224,0.679590053,5.901037985));
#165481=CARTESIAN_POINT('Ctrl Pts',(-4.206797255,0.678571429,5.904689396));
#165482=CARTESIAN_POINT('Ctrl Pts',(-3.889448673,0.615498301,6.130784462));
#165483=CARTESIAN_POINT('Ctrl Pts',(-3.549695121,0.551245526,6.321563458));
#165484=CARTESIAN_POINT('',(-3.55382585594571,0.552026825906715,6.31924218473728));
#165485=CARTESIAN_POINT('Origin',(0.0726095802536447,0.411147127799279,
-0.176685306794135));
#165486=CARTESIAN_POINT('Origin',(-4.77447887405374,0.300179931536728,8.08381453320419));
#165487=CARTESIAN_POINT('Ctrl Pts',(-3.802445091,0.551266351,6.385268657));
#165488=CARTESIAN_POINT('Ctrl Pts',(-3.454621124,0.615380951,6.592398788));
#165489=CARTESIAN_POINT('Ctrl Pts',(-3.086356055,0.680609079,6.76052148800001));
#165490=CARTESIAN_POINT('Ctrl Pts',(-3.08266310279245,0.681263184913293,
6.76220741791399));
#165491=CARTESIAN_POINT('Ctrl Pts',(-3.0789701505849,0.681917290826586,
6.76389334782798));
#165492=CARTESIAN_POINT('Ctrl Pts',(-3.55790654742961,0.551266351,6.31694450745764));
#165493=CARTESIAN_POINT('Ctrl Pts',(-3.21380439414336,0.615380951,6.5107539204794));
#165494=CARTESIAN_POINT('Ctrl Pts',(-2.85068605802178,0.680609079,6.66603899693022));
#165495=CARTESIAN_POINT('Ctrl Pts',(-2.84704471711311,0.681263184913293,
6.66759619150052));
#165496=CARTESIAN_POINT('Ctrl Pts',(-2.84340337620444,0.681917290826586,
6.66915338607082));
#165497=CARTESIAN_POINT('Origin',(0.0565289924188023,0.80345341474124,-0.183997606089015));
#165498=CARTESIAN_POINT('Ctrl Pts',(-2.76370050292562,0.681884070047611,
6.89871503673943));
#165499=CARTESIAN_POINT('Ctrl Pts',(-2.75995286496281,0.681246574523805,
6.90021166036972));
#165500=CARTESIAN_POINT('Ctrl Pts',(-2.756205227,0.680609079,6.901708284));
#165501=CARTESIAN_POINT('Ctrl Pts',(-2.75021469,0.679590053,6.90410061200001));
#165502=CARTESIAN_POINT('Ctrl Pts',(-2.744220009,0.678571429,6.906482536));
#165503=CARTESIAN_POINT('Ctrl Pts',(-2.373029877,0.615498301,7.053971129));
#165504=CARTESIAN_POINT('Ctrl Pts',(-1.988170027,0.551245526,7.16082568100001));
#165505=CARTESIAN_POINT('Ctrl Pts',(-2.85792658132566,0.681884070047611,
6.66294361747932));
#165506=CARTESIAN_POINT('Ctrl Pts',(-2.85430691216284,0.681246574523805,
6.66449154473966));
#165507=CARTESIAN_POINT('Ctrl Pts',(-2.850687243,0.680609079,6.666039472));
#165508=CARTESIAN_POINT('Ctrl Pts',(-2.844901262,0.679590053,6.668513808));
#165509=CARTESIAN_POINT('Ctrl Pts',(-2.839110994,0.678571429,6.670978097));
#165510=CARTESIAN_POINT('Ctrl Pts',(-2.48057809,0.615498301,6.823566622));
#165511=CARTESIAN_POINT('Ctrl Pts',(-2.107755942,0.551245526,6.93684834));
#165512=CARTESIAN_POINT('',(-2.11228911074674,0.552026825786492,6.93546932179441));
#165513=CARTESIAN_POINT('Origin',(0.0329298365003622,0.41114712983725,-0.188163271897352));
#165514=CARTESIAN_POINT('Origin',(-2.92612069033567,0.299941709146899,8.92383548076064));
#165515=CARTESIAN_POINT('Ctrl Pts',(-2.340902024,0.551266351,7.053397919));
#165516=CARTESIAN_POINT('Ctrl Pts',(-1.956683132,0.615380951,7.180913592));
#165517=CARTESIAN_POINT('Ctrl Pts',(-1.560886485,0.680609079,7.265939572));
#165518=CARTESIAN_POINT('Ctrl Pts',(-1.55691744686872,0.681263184913293,
7.2667922102407));
#165519=CARTESIAN_POINT('Ctrl Pts',(-1.55294840873743,0.681917290826586,
7.26764484848138));
#165520=CARTESIAN_POINT('Ctrl Pts',(-2.11676832528776,0.551266351,6.93410259070982));
#165521=CARTESIAN_POINT('Ctrl Pts',(-1.73904779404177,0.615380951,7.04940905517114));
#165522=CARTESIAN_POINT('Ctrl Pts',(-1.35103726228651,0.680609079,7.12300394455444));
#165523=CARTESIAN_POINT('Ctrl Pts',(-1.3471463031095,0.681263184913293,
7.12374195212587));
#165524=CARTESIAN_POINT('Ctrl Pts',(-1.34325534393248,0.681917290826586,
7.12447995969728));
#165525=CARTESIAN_POINT('Origin',(0.0156526904332333,0.803452733533447,
-0.191844834767033));
#165526=CARTESIAN_POINT('Ctrl Pts',(-1.21606691399939,0.68188407004749,
7.33154082511757));
#165527=CARTESIAN_POINT('Ctrl Pts',(-1.21208516349969,0.681246574523745,
7.3321968275588));
#165528=CARTESIAN_POINT('Ctrl Pts',(-1.208103413,0.680609079000001,7.33285283000001));
#165529=CARTESIAN_POINT('Ctrl Pts',(-1.201738651,0.679590053,7.333901439));
#165530=CARTESIAN_POINT('Ctrl Pts',(-1.195372079,0.678571429,7.334938996));
#165531=CARTESIAN_POINT('Ctrl Pts',(-0.801154479,0.615498301,7.399184481));
#165532=CARTESIAN_POINT('Ctrl Pts',(-0.402321868,0.551245526,7.420807342));
#165533=CARTESIAN_POINT('Ctrl Pts',(-1.3587739249797,0.68188407004749,7.12153743297978));
#165534=CARTESIAN_POINT('Ctrl Pts',(-1.35490612248985,0.681246574523745,
7.12227104898989));
#165535=CARTESIAN_POINT('Ctrl Pts',(-1.35103832,0.680609079000001,7.123004665));
#165536=CARTESIAN_POINT('Ctrl Pts',(-1.344855702,0.679590053,7.124177338));
#165537=CARTESIAN_POINT('Ctrl Pts',(-1.338671059,0.678571429,7.125339276));
#165538=CARTESIAN_POINT('Ctrl Pts',(-0.955718432,0.615498301,7.19728639));
#165539=CARTESIAN_POINT('Ctrl Pts',(-0.567260438,0.551245526,7.227773903));
#165540=CARTESIAN_POINT('',(-0.571984069400262,0.552026825956257,7.22740162306855));
#165541=CARTESIAN_POINT('Origin',(-0.00828956117031529,0.41114712676337,
-0.190843312368436));
#165542=CARTESIAN_POINT('Origin',(-0.939094529349745,0.30008162841821,9.34267857849552));
#165543=CARTESIAN_POINT('Ctrl Pts',(-0.780723137064731,0.551266351,7.40094088412655));
#165544=CARTESIAN_POINT('Ctrl Pts',(-0.377572579286645,0.615380951,7.44346912117974));
#165545=CARTESIAN_POINT('Ctrl Pts',(0.0278120868452411,0.680609079,7.4419541167355));
#165546=CARTESIAN_POINT('Ctrl Pts',(0.0318772733745123,0.681263184913293,
7.44193892431167));
#165547=CARTESIAN_POINT('Ctrl Pts',(0.0359424599037835,0.681917290826586,
7.44192373188786));
#165548=CARTESIAN_POINT('Ctrl Pts',(-0.769900980000001,0.551266351,7.391718134));
#165549=CARTESIAN_POINT('Ctrl Pts',(-0.367252812,0.615380951,7.433656857));
#165550=CARTESIAN_POINT('Ctrl Pts',(0.037568402,0.680609079,7.431610398));
#165551=CARTESIAN_POINT('Ctrl Pts',(0.0416279382464465,0.681263184913293,
7.43158987616418));
#165552=CARTESIAN_POINT('Ctrl Pts',(0.0456874744928931,0.681917290826586,
7.43156935432838));
#165553=CARTESIAN_POINT('Ctrl Pts',(-0.576653346,0.551266351,7.227030574));
#165554=CARTESIAN_POINT('Ctrl Pts',(-0.182976184,0.615380951,7.258442542));
#165555=CARTESIAN_POINT('Ctrl Pts',(0.211783654,0.680609079,7.246906077));
#165556=CARTESIAN_POINT('Ctrl Pts',(0.215742295038516,0.681263184913293,
7.24679038963925));
#165557=CARTESIAN_POINT('Ctrl Pts',(0.219700936077032,0.681917290826586,
7.24667470227851));
#165558=CARTESIAN_POINT('Origin',(-0.0259542276886779,0.80345272965562,
-0.190724450753197));
#165559=CARTESIAN_POINT('Origin',(-7.084,3.7,7.084));
#165560=CARTESIAN_POINT('Ctrl Pts',(0.207089507,0.681369595,7.247041737));
#165561=CARTESIAN_POINT('Ctrl Pts',(0.215726884,0.679970133,7.246794918));
#165562=CARTESIAN_POINT('Ctrl Pts',(0.224363648,0.678571429,7.24652751));
#165563=CARTESIAN_POINT('Ctrl Pts',(0.611454754,0.615882895,7.234542573));
#165564=CARTESIAN_POINT('Ctrl Pts',(0.995066308,0.552026826,7.181388657));
#165565=CARTESIAN_POINT('Ctrl Pts',(0.056367661,0.681369595,7.406630948));
#165566=CARTESIAN_POINT('Ctrl Pts',(0.065195244,0.679970133,7.406563766));
#165567=CARTESIAN_POINT('Ctrl Pts',(0.074022642,0.678571429,7.406475542));
#165568=CARTESIAN_POINT('Ctrl Pts',(0.469657766,0.615882895,7.402521441));
#165569=CARTESIAN_POINT('Ctrl Pts',(0.86262025,0.552026826,7.356442456));
#165570=CARTESIAN_POINT('Ctrl Pts',(0.21765174455862,0.655900535668849,
7.40270156512545));
#165571=CARTESIAN_POINT('Ctrl Pts',(0.217001547613326,0.658682906707741,
7.38460695266366));
#165572=CARTESIAN_POINT('Ctrl Pts',(0.216340972118041,0.661493949096189,
7.36651709356107));
#165573=CARTESIAN_POINT('Ctrl Pts',(0.215669566035234,0.664334613017224,
7.34843231566661));
#165574=CARTESIAN_POINT('Ctrl Pts',(0.215041027322259,0.666993908621838,
7.33150219943251));
#165575=CARTESIAN_POINT('Ctrl Pts',(0.214402995011337,0.669679171588032,
7.31457648975586));
#165576=CARTESIAN_POINT('Ctrl Pts',(0.213755072783103,0.672391218148102,
7.29765547471631));
#165577=CARTESIAN_POINT('Ctrl Pts',(0.213107143282986,0.67510329514652,
7.28073426976565));
#165578=CARTESIAN_POINT('Ctrl Pts',(0.212445088585071,0.677841475225338,
7.26381776537258));
#165579=CARTESIAN_POINT('Ctrl Pts',(0.211783655068483,0.680609081981435,
7.24690609670463));
#165580=CARTESIAN_POINT('',(0.972815229604965,0.552026824384635,7.21079786933495));
#165581=CARTESIAN_POINT('Ctrl Pts',(0.627711922,0.499686101,7.275310889));
#165582=CARTESIAN_POINT('Ctrl Pts',(0.739025144,0.51775868,7.265706814));
#165583=CARTESIAN_POINT('Ctrl Pts',(0.849992445,0.535714286,7.252701816));
#165584=CARTESIAN_POINT('Ctrl Pts',(0.900321661,0.54385805,7.2468034));
#165585=CARTESIAN_POINT('Ctrl Pts',(0.950564171,0.552026826,7.240207079));
#165586=CARTESIAN_POINT('Ctrl Pts',(0.67478522,0.499686101,7.218529276));
#165587=CARTESIAN_POINT('Ctrl Pts',(0.785229676,0.51775868,7.208204972));
#165588=CARTESIAN_POINT('Ctrl Pts',(0.895306583,0.535714286,7.194506663));
#165589=CARTESIAN_POINT('Ctrl Pts',(0.945231961,0.54385805,7.188293795));
#165590=CARTESIAN_POINT('Ctrl Pts',(0.995066308,0.552026826,7.181388657));
#165591=CARTESIAN_POINT('Ctrl Pts',(0.99506630855658,0.552026826281282,
7.18138865673239));
#165592=CARTESIAN_POINT('Ctrl Pts',(0.961819032715832,0.546576979789078,
7.18599546025834));
#165593=CARTESIAN_POINT('Ctrl Pts',(0.928564162759112,0.541139220286484,
7.19036798743331));
#165594=CARTESIAN_POINT('Ctrl Pts',(0.895306583168572,0.535714286026804,
7.19450666298286));
#165595=CARTESIAN_POINT('Ctrl Pts',(0.822683552237206,0.523868108970865,
7.20354409641407));
#165596=CARTESIAN_POINT('Ctrl Pts',(0.749799676836557,0.511960760930993,
7.21149710151007));
#165597=CARTESIAN_POINT('Ctrl Pts',(0.676703532269255,0.49999999974866,
7.21834969580106));
#165598=CARTESIAN_POINT('Ctrl Pts',(0.67478522,0.499686101,7.218529276));
#165599=CARTESIAN_POINT('Ctrl Pts',(0.785229676,0.51775868,7.208204972));
#165600=CARTESIAN_POINT('Ctrl Pts',(0.895306583,0.535714286,7.194506663));
#165601=CARTESIAN_POINT('Ctrl Pts',(0.946186392,0.544013736,7.188175023));
#165602=CARTESIAN_POINT('Ctrl Pts',(0.99697156,0.552339147,7.181124404));
#165603=CARTESIAN_POINT('Ctrl Pts',(0.723670697,0.499686101,7.259056491));
#165604=CARTESIAN_POINT('Ctrl Pts',(0.834735225,0.51775868,7.247984233));
#165605=CARTESIAN_POINT('Ctrl Pts',(0.945409031,0.535714286,7.233519349));
#165606=CARTESIAN_POINT('Ctrl Pts',(0.996564739,0.544013736,7.226833383));
#165607=CARTESIAN_POINT('Ctrl Pts',(1.047620768,0.552339147,7.21942457099999));
#165608=CARTESIAN_POINT('Ctrl Pts',(0.99506631450015,0.552026827255544,
7.18138865590884));
#165609=CARTESIAN_POINT('Ctrl Pts',(0.99574332826213,0.551172308319168,
7.186567436955));
#165610=CARTESIAN_POINT('Ctrl Pts',(0.996419516854235,0.550320534977845,
7.19174677410628));
#165611=CARTESIAN_POINT('Ctrl Pts',(0.997094885402565,0.549471478062853,
7.19692666267777));
#165612=CARTESIAN_POINT('Ctrl Pts',(0.997721871981064,0.548683245783752,
7.2017354750225));
#165613=CARTESIAN_POINT('Ctrl Pts',(0.998348151970431,0.547897354469737,
7.20654476390293));
#165614=CARTESIAN_POINT('Ctrl Pts',(0.998973732569637,0.547113782422352,
7.21135452094716));
#165615=CARTESIAN_POINT('Ctrl Pts',(0.999599313800958,0.546330209583209,
7.21616428285138));
#165616=CARTESIAN_POINT('Ctrl Pts',(1.00022419579762,0.545548955818075,
7.22097451413375));
#165617=CARTESIAN_POINT('Ctrl Pts',(1.0008483868275,0.54476999986866,7.2257852066657));
#165618=CARTESIAN_POINT('Ctrl Pts',(0.993197311,0.55233793,7.181647381));
#165619=CARTESIAN_POINT('Ctrl Pts',(1.151022227,0.526068113,7.159820734));
#165620=CARTESIAN_POINT('Ctrl Pts',(1.307735906,0.49968693,7.131081741));
#165621=CARTESIAN_POINT('Ctrl Pts',(0.95487053,0.55233793,7.232276452));
#165622=CARTESIAN_POINT('Ctrl Pts',(1.113808078,0.526068113,7.21129208));
#165623=CARTESIAN_POINT('Ctrl Pts',(1.271670316,0.49968693,7.18334567));
#165624=CARTESIAN_POINT('Origin',(-0.049945526223899,0.410743194127898,
-0.190657471942941));
#165625=CARTESIAN_POINT('Ctrl Pts',(1.05073165838991,0.552548454735263,
7.22635066464236));
#165626=CARTESIAN_POINT('Ctrl Pts',(1.05230819469495,0.552287640367632,
7.22612072932118));
#165627=CARTESIAN_POINT('Ctrl Pts',(1.053884731,0.552026826,7.225890794));
#165628=CARTESIAN_POINT('Ctrl Pts',(1.211741222,0.525911829,7.202867675));
#165629=CARTESIAN_POINT('Ctrl Pts',(1.368441669,0.49968693,7.172972758));
#165630=CARTESIAN_POINT('Ctrl Pts',(0.991923006675841,0.552548454735263,
7.18181555581264));
#165631=CARTESIAN_POINT('Ctrl Pts',(0.993489831971372,0.552287640367632,
7.18159845552429));
#165632=CARTESIAN_POINT('Ctrl Pts',(0.995056657266902,0.552026826,7.18138135523595));
#165633=CARTESIAN_POINT('Ctrl Pts',(1.15194079775301,0.525911829,7.15964339106533));
#165634=CARTESIAN_POINT('Ctrl Pts',(1.30772594559837,0.49968693,7.13107486765992));
#165635=CARTESIAN_POINT('',(1.08259319807141,0.552026824387391,7.24761168748306));
#165636=CARTESIAN_POINT('Ctrl Pts',(0.987286864787933,0.550751630586317,
7.18246659083401));
#165637=CARTESIAN_POINT('Ctrl Pts',(0.991176586393967,0.551389228293159,
7.18192762391701));
#165638=CARTESIAN_POINT('Ctrl Pts',(0.995066308,0.552026826000001,7.181388657));
#165639=CARTESIAN_POINT('Ctrl Pts',(1.386277161,0.61615356,7.127181768));
#165640=CARTESIAN_POINT('Ctrl Pts',(1.769284534,0.681389364,7.030798834));
#165641=CARTESIAN_POINT('Ctrl Pts',(1.16219718885009,0.550751630586317,
7.31510228082505));
#165642=CARTESIAN_POINT('Ctrl Pts',(1.16615864842505,0.551389228293159,
7.31446849791252));
#165643=CARTESIAN_POINT('Ctrl Pts',(1.170120108,0.552026826000001,7.313834715));
#165644=CARTESIAN_POINT('Ctrl Pts',(1.568546046,0.61615356,7.250091656));
#165645=CARTESIAN_POINT('Ctrl Pts',(1.957689904,0.681389364,7.14344521600001));
#165646=CARTESIAN_POINT('Ctrl Pts',(1.76470286480055,0.680609082082805,
7.03195023316344));
#165647=CARTESIAN_POINT('Ctrl Pts',(1.76927629608276,0.677652752738448,
7.04944087630682));
#165648=CARTESIAN_POINT('Ctrl Pts',(1.77385099516534,0.67472989691538,7.06693689689647));
#165649=CARTESIAN_POINT('Ctrl Pts',(1.77841126959504,0.671836782554415,
7.08444156064863));
#165650=CARTESIAN_POINT('Ctrl Pts',(1.78268038335609,0.669128385390798,
7.10082860095926));
#165651=CARTESIAN_POINT('Ctrl Pts',(1.78694087127159,0.666446714500865,
7.11722232948892));
#165652=CARTESIAN_POINT('Ctrl Pts',(1.79119305702725,0.663790956144513,
7.13362238136369));
#165653=CARTESIAN_POINT('Ctrl Pts',(1.79544528843677,0.661135169274451,
7.15002260931861));
#165654=CARTESIAN_POINT('Ctrl Pts',(1.79968922868348,0.658505288583656,
7.16642920443237));
#165655=CARTESIAN_POINT('Ctrl Pts',(1.80392518236685,0.655900535538507,
7.18284182470367));
#165656=CARTESIAN_POINT('Ctrl Pts',(1.760147622,0.681369595,7.033091806));
#165657=CARTESIAN_POINT('Ctrl Pts',(1.768530003,0.679970133,7.030993976));
#165658=CARTESIAN_POINT('Ctrl Pts',(1.776907359,0.678571429,7.028876172));
#165659=CARTESIAN_POINT('Ctrl Pts',(2.152372083,0.615882895,6.933958291));
#165660=CARTESIAN_POINT('Ctrl Pts',(2.515588492,0.552026826,6.799581939));
#165661=CARTESIAN_POINT('Ctrl Pts',(1.647256531,0.681369595,7.22135065100001));
#165662=CARTESIAN_POINT('Ctrl Pts',(1.655863289,0.679970133,7.219387371));
#165663=CARTESIAN_POINT('Ctrl Pts',(1.664465341,0.678571429,7.21740358));
#165664=CARTESIAN_POINT('Ctrl Pts',(2.050000721,0.615882895,7.12849206600001));
#165665=CARTESIAN_POINT('Ctrl Pts',(2.423870341,0.552026826,6.999015065));
#165666=CARTESIAN_POINT('',(2.50017974262328,0.552026824384634,6.83308690443088));
#165667=CARTESIAN_POINT('Ctrl Pts',(2.177013151,0.499686101,6.970278656));
#165668=CARTESIAN_POINT('Ctrl Pts',(2.283659339,0.51775868,6.936970065));
#165669=CARTESIAN_POINT('Ctrl Pts',(2.389236596,0.535714286,6.900414428));
#165670=CARTESIAN_POINT('Ctrl Pts',(2.437121158,0.54385805,6.88383462));
#165671=CARTESIAN_POINT('Ctrl Pts',(2.484771012,0.552026826,6.866591863));
#165672=CARTESIAN_POINT('Ctrl Pts',(2.210779533,0.499686101,6.904705197));
#165673=CARTESIAN_POINT('Ctrl Pts',(2.316422439,0.51775868,6.870879977));
#165674=CARTESIAN_POINT('Ctrl Pts',(2.420981077,0.535714286,6.833838645));
#165675=CARTESIAN_POINT('Ctrl Pts',(2.468403645,0.54385805,6.81703855));
#165676=CARTESIAN_POINT('Ctrl Pts',(2.515588492,0.552026826,6.799581939));
#165677=CARTESIAN_POINT('Ctrl Pts',(2.51558848994905,0.552026825797967,
6.79958193941116));
#165678=CARTESIAN_POINT('Ctrl Pts',(2.48410884342391,0.546576979474308,
6.81122821934968));
#165679=CARTESIAN_POINT('Ctrl Pts',(2.4525714186327,0.541139220132675,6.82264733293808));
#165680=CARTESIAN_POINT('Ctrl Pts',(2.42098107697934,0.535714285996453,
6.83383864500732));
#165681=CARTESIAN_POINT('Ctrl Pts',(2.35199871315026,0.52386810886986,6.85827659379462));
#165682=CARTESIAN_POINT('Ctrl Pts',(2.28252848394537,0.511960760922405,
6.88171154060857));
#165683=CARTESIAN_POINT('Ctrl Pts',(2.21261439168748,0.499999999735721,
6.90411743489196));
#165684=CARTESIAN_POINT('Ctrl Pts',(2.210779533,0.499686101,6.904705197));
#165685=CARTESIAN_POINT('Ctrl Pts',(2.316422439,0.51775868,6.870879977));
#165686=CARTESIAN_POINT('Ctrl Pts',(2.420981077,0.535714286,6.833838645));
#165687=CARTESIAN_POINT('Ctrl Pts',(2.469310228,0.544013736,6.81671738));
#165688=CARTESIAN_POINT('Ctrl Pts',(2.517392394,0.552339147,6.798914291));
#165689=CARTESIAN_POINT('Ctrl Pts',(2.267234248,0.499686101,6.933775975));
#165690=CARTESIAN_POINT('Ctrl Pts',(2.373321941,0.51775868,6.89908699));
#165691=CARTESIAN_POINT('Ctrl Pts',(2.478298732,0.535714286,6.861168691));
#165692=CARTESIAN_POINT('Ctrl Pts',(2.526821163,0.544013736,6.843642074));
#165693=CARTESIAN_POINT('Ctrl Pts',(2.575090855,0.552339147,6.825430939));
#165694=CARTESIAN_POINT('Ctrl Pts',(2.51558849795866,0.552026827184613,
6.79958193644791));
#165695=CARTESIAN_POINT('Ctrl Pts',(2.51736296788845,0.551172308216822,
6.80449410254021));
#165696=CARTESIAN_POINT('Ctrl Pts',(2.51913675196281,0.550320534899973,
6.80940698905447));
#165697=CARTESIAN_POINT('Ctrl Pts',(2.52090985370924,0.54947147800732,6.81432059038011));
#165698=CARTESIAN_POINT('Ctrl Pts',(2.52255593423229,0.548683245737638,
6.81888219179778));
#165699=CARTESIAN_POINT('Ctrl Pts',(2.5242014271309,0.547897354431265,6.82344441050407));
#165700=CARTESIAN_POINT('Ctrl Pts',(2.52584633764004,0.5471137823873,6.82800723679375));
#165701=CARTESIAN_POINT('Ctrl Pts',(2.52749124979859,0.546330209557625,
6.83257006765872));
#165702=CARTESIAN_POINT('Ctrl Pts',(2.52913557998059,0.545548955797864,
6.83713350725973));
#165703=CARTESIAN_POINT('Ctrl Pts',(2.53077933509621,0.544770000008302,
6.84169754538297));
#165704=CARTESIAN_POINT('Ctrl Pts',(2.513818808,0.55233793,6.800236393));
#165705=CARTESIAN_POINT('Ctrl Pts',(2.663261782,0.526068113,6.744992349));
#165706=CARTESIAN_POINT('Ctrl Pts',(2.810133548,0.49968693,6.68323645));
#165707=CARTESIAN_POINT('Ctrl Pts',(2.48727184,0.55233793,6.85792091));
#165708=CARTESIAN_POINT('Ctrl Pts',(2.637982497,0.526068113,6.803260266));
#165709=CARTESIAN_POINT('Ctrl Pts',(2.786146352,0.49968693,6.742031513));
#165710=CARTESIAN_POINT('Origin',(-0.0897638160116732,0.410742936752906,
-0.175463805149405));
#165711=CARTESIAN_POINT('Ctrl Pts',(2.57961791904852,0.552548454735263,
6.83152635453666));
#165712=CARTESIAN_POINT('Ctrl Pts',(2.58110816752426,0.552287640367631,
6.83096288626833));
#165713=CARTESIAN_POINT('Ctrl Pts',(2.582598416,0.552026826,6.830399418));
#165714=CARTESIAN_POINT('Ctrl Pts',(2.731815021,0.525911829,6.773980087));
#165715=CARTESIAN_POINT('Ctrl Pts',(2.878425375,0.49968693,6.711098133));
#165716=CARTESIAN_POINT('Ctrl Pts',(2.51261044996927,0.552548454735263,
6.80067457404514));
#165717=CARTESIAN_POINT('Ctrl Pts',(2.51409397361356,0.552287640367631,
6.80012572831319));
#165718=CARTESIAN_POINT('Ctrl Pts',(2.51557749725783,0.552026826,6.79957688258125));
#165719=CARTESIAN_POINT('Ctrl Pts',(2.66412075379542,0.525911829,6.74462168677177));
#165720=CARTESIAN_POINT('Ctrl Pts',(2.8101223429279,0.49968693,6.68323187855741));
#165721=CARTESIAN_POINT('',(2.61530504560632,0.552026824384634,6.84544101758886));
#165722=CARTESIAN_POINT('Ctrl Pts',(2.50822148649275,0.550751630586317,
6.80230648424818));
#165723=CARTESIAN_POINT('Ctrl Pts',(2.51190440631477,0.551389228293159,
6.80094394353719));
#165724=CARTESIAN_POINT('Ctrl Pts',(2.51558732613678,0.552026826,6.79958140282619));
#165725=CARTESIAN_POINT('Ctrl Pts',(2.88599897792836,0.61615356,6.66254313433735));
#165726=CARTESIAN_POINT('Ctrl Pts',(3.23933234779194,0.681389364000001,
6.48607838264556));
#165727=CARTESIAN_POINT('Ctrl Pts',(2.70755642147094,0.550751630586317,
6.89424121325815));
#165728=CARTESIAN_POINT('Ctrl Pts',(2.71128901973547,0.551389228293159,
6.89277065112907));
#165729=CARTESIAN_POINT('Ctrl Pts',(2.715021618,0.552026826,6.891300089));
#165730=CARTESIAN_POINT('Ctrl Pts',(3.090429706,0.61615356,6.74339750800001));
#165731=CARTESIAN_POINT('Ctrl Pts',(3.447549765,0.681389364000001,6.555589976));
#165732=CARTESIAN_POINT('Ctrl Pts',(3.23510652986855,0.680609082082805,
6.48818819349658));
#165733=CARTESIAN_POINT('Ctrl Pts',(3.24333300793022,0.677652752623469,
6.50428676221162));
#165734=CARTESIAN_POINT('Ctrl Pts',(3.25156188047759,0.674729896811195,
6.52039031048621));
#165735=CARTESIAN_POINT('Ctrl Pts',(3.25977852354583,0.671836782445325,
6.53650540076861));
#165736=CARTESIAN_POINT('Ctrl Pts',(3.26747055705726,0.669128385297014,
6.55159158784801));
#165737=CARTESIAN_POINT('Ctrl Pts',(3.27515560416031,0.666446714422628,
6.5666861610813));
#165738=CARTESIAN_POINT('Ctrl Pts',(3.28283390253543,0.663790956081852,
6.5817886945425));
#165739=CARTESIAN_POINT('Ctrl Pts',(3.29051228334905,0.661135169227366,
6.59689139015297));
#165740=CARTESIAN_POINT('Ctrl Pts',(3.29818393559334,0.658505288552175,
6.61200208641671));
#165741=CARTESIAN_POINT('Ctrl Pts',(3.30584908284948,0.655900535589578,
6.62712038403327));
#165742=CARTESIAN_POINT('Ctrl Pts',(3.23090319,0.681369595,6.490282319));
#165743=CARTESIAN_POINT('Ctrl Pts',(3.238638624,0.679970133,6.486431571));
#165744=CARTESIAN_POINT('Ctrl Pts',(3.246364857,0.678571429,6.482562396));
#165745=CARTESIAN_POINT('Ctrl Pts',(3.592646886,0.615882895,6.30914982500001));
#165746=CARTESIAN_POINT('Ctrl Pts',(3.918484554,0.552026826,6.099834326));
#165747=CARTESIAN_POINT('Ctrl Pts',(3.161121518,0.681369595,6.698408024));
#165748=CARTESIAN_POINT('Ctrl Pts',(3.169105006,0.679970133,6.694640446));
#165749=CARTESIAN_POINT('Ctrl Pts',(3.177079491,0.678571429,6.690853848));
#165750=CARTESIAN_POINT('Ctrl Pts',(3.534487921,0.615882895,6.52114232600001));
#165751=CARTESIAN_POINT('Ctrl Pts',(3.871782949,0.552026826,6.314321508));
#165752=CARTESIAN_POINT('',(3.91063862958003,0.552026824384634,6.13586838986638));
#165753=CARTESIAN_POINT('Ctrl Pts',(3.624519664,0.499686101,6.339323939));
#165754=CARTESIAN_POINT('Ctrl Pts',(3.721512162,0.51775868,6.283868307));
#165755=CARTESIAN_POINT('Ctrl Pts',(3.816762699,0.535714286,6.225471331));
#165756=CARTESIAN_POINT('Ctrl Pts',(3.859963578,0.54385805,6.198985384));
#165757=CARTESIAN_POINT('Ctrl Pts',(3.902792722,0.552026826,6.171902443));
#165758=CARTESIAN_POINT('Ctrl Pts',(3.643400252,0.499686101,6.268024777));
#165759=CARTESIAN_POINT('Ctrl Pts',(3.739301863,0.51775868,6.21228027));
#165760=CARTESIAN_POINT('Ctrl Pts',(3.833453187,0.535714286,6.153627927));
#165761=CARTESIAN_POINT('Ctrl Pts',(3.876155517,0.54385805,6.127026159));
#165762=CARTESIAN_POINT('Ctrl Pts',(3.918484554,0.552026826,6.099834326));
#165763=CARTESIAN_POINT('Ctrl Pts',(3.91848455377917,0.552026826341472,
6.09983432539862));
#165764=CARTESIAN_POINT('Ctrl Pts',(3.8902444900359,0.546576979835352,6.11797551583042));
#165765=CARTESIAN_POINT('Ctrl Pts',(3.86189916403442,0.541139220312496,
6.13590727149343));
#165766=CARTESIAN_POINT('Ctrl Pts',(3.83345318706314,0.535714285972514,
6.15362792713793));
#165767=CARTESIAN_POINT('Ctrl Pts',(3.77133702917716,0.52386810879776,6.19232369985583));
#165768=CARTESIAN_POINT('Ctrl Pts',(3.7085287958654,0.511960760930835,6.23014479602785));
#165769=CARTESIAN_POINT('Ctrl Pts',(3.64506586129707,0.499999999748424,
6.26705631602722));
#165770=CARTESIAN_POINT('Ctrl Pts',(3.643400252,0.499686101,6.268024777));
#165771=CARTESIAN_POINT('Ctrl Pts',(3.739301863,0.51775868,6.21228027));
#165772=CARTESIAN_POINT('Ctrl Pts',(3.833453187,0.535714286,6.153627927));
#165773=CARTESIAN_POINT('Ctrl Pts',(3.876971864,0.544013736,6.126517609));
#165774=CARTESIAN_POINT('Ctrl Pts',(3.920102756,0.552339147,6.098794502));
#165775=CARTESIAN_POINT('Ctrl Pts',(3.704784445,0.499686101,6.284279802));
#165776=CARTESIAN_POINT('Ctrl Pts',(3.80093476,0.51775868,6.227596108));
#165777=CARTESIAN_POINT('Ctrl Pts',(3.895305939,0.535714286,6.16799741));
#165778=CARTESIAN_POINT('Ctrl Pts',(3.938926237,0.544013736,6.140449667));
#165779=CARTESIAN_POINT('Ctrl Pts',(3.982152555,0.552339147,6.112287742));
#165780=CARTESIAN_POINT('Ctrl Pts',(3.91848455882013,0.552026827314291,
6.09983432216034));
#165781=CARTESIAN_POINT('Ctrl Pts',(3.92127351299936,0.551172308244916,
6.10425018632747));
#165782=CARTESIAN_POINT('Ctrl Pts',(3.92406195243446,0.550320534932904,
6.10866690107976));
#165783=CARTESIAN_POINT('Ctrl Pts',(3.92684987915185,0.549471478043595,
6.11308446061508));
#165784=CARTESIAN_POINT('Ctrl Pts',(3.92943808477059,0.548683245771267,
6.11718555564713));
#165785=CARTESIAN_POINT('Ctrl Pts',(3.93202584919722,0.547897354461127,
6.12128737986063));
#165786=CARTESIAN_POINT('Ctrl Pts',(3.93461317544761,0.547113782415644,
6.12538992263642));
#165787=CARTESIAN_POINT('Ctrl Pts',(3.93720050431235,0.546330209578404,
6.1294924695576));
#165788=CARTESIAN_POINT('Ctrl Pts',(3.93978739565186,0.545548955813255,
6.13359573607793));
#165789=CARTESIAN_POINT('Ctrl Pts',(3.94237385365378,0.544769999912963,
6.13769971114459));
#165790=CARTESIAN_POINT('Ctrl Pts',(3.916896932,0.55233793,6.100853909));
#165791=CARTESIAN_POINT('Ctrl Pts',(4.050970176,0.526068113,6.014775618));
#165792=CARTESIAN_POINT('Ctrl Pts',(4.181132469,0.49968693,5.922890449));
#165793=CARTESIAN_POINT('Ctrl Pts',(3.903371084,0.55233793,6.162896608));
#165794=CARTESIAN_POINT('Ctrl Pts',(4.038807786,0.526068113,6.077115563));
#165795=CARTESIAN_POINT('Ctrl Pts',(4.170345281,0.49968693,5.985467455));
#165796=CARTESIAN_POINT('Origin',(-0.125384577725371,0.410742960799487,
-0.152064775049904));
#165797=CARTESIAN_POINT('Ctrl Pts',(3.98788411345982,0.552548454735263,
6.11726746511525));
#165798=CARTESIAN_POINT('Ctrl Pts',(3.98921839172991,0.552287640367631,
6.11639681105762));
#165799=CARTESIAN_POINT('Ctrl Pts',(3.99055267,0.552026826,6.115526157));
#165800=CARTESIAN_POINT('Ctrl Pts',(4.124152185,0.525911829,6.02834872));
#165801=CARTESIAN_POINT('Ctrl Pts',(4.253817109,0.49968693,5.935420018));
#165802=CARTESIAN_POINT('Ctrl Pts',(3.91581102107496,0.552548454735263,
6.10154160681932));
#165803=CARTESIAN_POINT('Ctrl Pts',(3.91714187514867,0.552287640367631,
6.10068667906915));
#165804=CARTESIAN_POINT('Ctrl Pts',(3.91847272922237,0.552026826,6.09983175131896));
#165805=CARTESIAN_POINT('Ctrl Pts',(4.05172938397585,0.525911829,6.01422896864239));
#165806=CARTESIAN_POINT('Ctrl Pts',(4.18112054306447,0.49968693,5.92288839317594));
#165807=CARTESIAN_POINT('',(4.02572813609744,0.552026824384634,6.12318513352432));
#165808=CARTESIAN_POINT('Ctrl Pts',(3.91187548180337,0.550751630586318,
6.10407886133619));
#165809=CARTESIAN_POINT('Ctrl Pts',(3.91517939102832,0.551389228293159,
6.10195645717512));
#165810=CARTESIAN_POINT('Ctrl Pts',(3.91848330025327,0.552026826,6.09983405301406));
#165811=CARTESIAN_POINT('Ctrl Pts',(4.25077575638218,0.61615356,5.88637210731273));
#165812=CARTESIAN_POINT('Ctrl Pts',(4.55791368301831,0.681389364000001,
5.63807677382268));
#165813=CARTESIAN_POINT('Ctrl Pts',(4.12631332540522,0.550751630586317,
6.15101308899582));
#165814=CARTESIAN_POINT('Ctrl Pts',(4.12964253020261,0.551389228293159,
6.14877450949791));
#165815=CARTESIAN_POINT('Ctrl Pts',(4.132971735,0.552026826,6.14653593));
#165816=CARTESIAN_POINT('Ctrl Pts',(4.467808307,0.61615356,5.921389587));
#165817=CARTESIAN_POINT('Ctrl Pts',(4.77620603,0.681389364000001,5.661202634));
#165818=CARTESIAN_POINT('Ctrl Pts',(4.55424020909657,0.680609082247605,
5.6410456839352));
#165819=CARTESIAN_POINT('Ctrl Pts',(4.56573507336456,0.677652752657951,
5.65499942765426));
#165820=CARTESIAN_POINT('Ctrl Pts',(4.57723334628363,0.674729896804321,
5.66895751963912));
#165821=CARTESIAN_POINT('Ctrl Pts',(4.58872215690221,0.671836782415114,
5.682929512709));
#165822=CARTESIAN_POINT('Ctrl Pts',(4.599477439182,0.669128385266211,5.69600943320442));
#165823=CARTESIAN_POINT('Ctrl Pts',(4.6102277011599,0.666446714392474,5.7090990456675));
#165824=CARTESIAN_POINT('Ctrl Pts',(4.62097308339939,0.663790956053537,
5.72219788303472));
#165825=CARTESIAN_POINT('Ctrl Pts',(4.63171858100736,0.661135169200881,
5.73529686103845));
#165826=CARTESIAN_POINT('Ctrl Pts',(4.64245922725447,0.658505288528707,
5.74840509909306));
#165827=CARTESIAN_POINT('Ctrl Pts',(4.65319515451439,0.655900535591315,
5.76152215973136));
#165828=CARTESIAN_POINT('Ctrl Pts',(4.550585316,0.681369595,5.643994444));
#165829=CARTESIAN_POINT('Ctrl Pts',(4.557312103,0.679970133,5.638570835));
#165830=CARTESIAN_POINT('Ctrl Pts',(4.564025943,0.678571429,5.633131207));
#165831=CARTESIAN_POINT('Ctrl Pts',(4.864933514,0.615882895,5.389332525));
#165832=CARTESIAN_POINT('Ctrl Pts',(5.138156632,0.552026826,5.11486524));
#165833=CARTESIAN_POINT('Ctrl Pts',(4.52717597500001,0.681369595,5.862255283));
#165834=CARTESIAN_POINT('Ctrl Pts',(4.534162896,0.679970133,5.856859574));
#165835=CARTESIAN_POINT('Ctrl Pts',(4.541136935,0.678571429,5.851447226));
#165836=CARTESIAN_POINT('Ctrl Pts',(4.853706394,0.615882895,5.608871218));
#165837=CARTESIAN_POINT('Ctrl Pts',(5.138655289,0.552026826,5.334377295));
#165838=CARTESIAN_POINT('',(5.13824039993051,0.552026824384634,5.15174348905096));
#165839=CARTESIAN_POINT('Ctrl Pts',(4.902547666,0.499686101,5.41194948));
#165840=CARTESIAN_POINT('Ctrl Pts',(4.985351212,0.51775868,5.33693985));
#165841=CARTESIAN_POINT('Ctrl Pts',(5.065821221,0.535714286,5.259432113));
#165842=CARTESIAN_POINT('Ctrl Pts',(5.102318391,0.54385805,5.224278481));
#165843=CARTESIAN_POINT('Ctrl Pts',(5.138324182,0.552026826,5.188621724));
#165844=CARTESIAN_POINT('Ctrl Pts',(4.905659624,0.499686101,5.338258485));
#165845=CARTESIAN_POINT('Ctrl Pts',(4.987335687,0.51775868,5.263201242));
#165846=CARTESIAN_POINT('Ctrl Pts',(5.066677286,0.535714286,5.185680407));
#165847=CARTESIAN_POINT('Ctrl Pts',(5.102662666,0.54385805,5.150520834));
#165848=CARTESIAN_POINT('Ctrl Pts',(5.138156632,0.552026826,5.11486524));
#165849=CARTESIAN_POINT('Ctrl Pts',(5.13815663264052,0.552026826325034,
5.11486523962076));
#165850=CARTESIAN_POINT('Ctrl Pts',(5.11447662501153,0.546576979803649,
5.13865307809982));
#165851=CARTESIAN_POINT('Ctrl Pts',(5.09064879432901,0.541139220286672,
5.1622590064672));
#165852=CARTESIAN_POINT('Ctrl Pts',(5.06667728595784,0.535714285990458,
5.1856804070412));
#165853=CARTESIAN_POINT('Ctrl Pts',(5.01433181580309,0.523868108829625,
5.23682463158345));
#165854=CARTESIAN_POINT('Ctrl Pts',(4.96112242201154,0.511960760879927,
5.28726340536358));
#165855=CARTESIAN_POINT('Ctrl Pts',(4.90707810144185,0.499999999671717,
5.3369546096604));
#165856=CARTESIAN_POINT('Ctrl Pts',(4.905659624,0.499686101,5.338258485));
#165857=CARTESIAN_POINT('Ctrl Pts',(4.987335687,0.51775868,5.263201242));
#165858=CARTESIAN_POINT('Ctrl Pts',(5.066677286,0.535714286,5.185680407));
#165859=CARTESIAN_POINT('Ctrl Pts',(5.103350603,0.544013736,5.149848684));
#165860=CARTESIAN_POINT('Ctrl Pts',(5.139513471,0.552339147,5.113501861));
#165861=CARTESIAN_POINT('Ctrl Pts',(4.969103039,0.499686101,5.340937689));
#165862=CARTESIAN_POINT('Ctrl Pts',(5.050820094,0.51775868,5.264909753));
#165863=CARTESIAN_POINT('Ctrl Pts',(5.130172969,0.535714286,5.186417426));
#165864=CARTESIAN_POINT('Ctrl Pts',(5.166851499,0.544013736,5.15013665899999));
#165865=CARTESIAN_POINT('Ctrl Pts',(5.203013228,0.552339147,5.113340763));
#165866=CARTESIAN_POINT('Ctrl Pts',(5.13815663689923,0.552026827305158,
5.11486523534265));
#165867=CARTESIAN_POINT('Ctrl Pts',(5.14182966686511,0.551172308293672,
5.11857831599279));
#165868=CARTESIAN_POINT('Ctrl Pts',(5.14550237726308,0.550320534953802,
5.12229233838852));
#165869=CARTESIAN_POINT('Ctrl Pts',(5.14917476853448,0.549471478040705,
5.12600729603646));
#165870=CARTESIAN_POINT('Ctrl Pts',(5.15258407752835,0.548683245753838,
5.12945612204244));
#165871=CARTESIAN_POINT('Ctrl Pts',(5.15599311239802,0.547897354432532,
5.13290575502544));
#165872=CARTESIAN_POINT('Ctrl Pts',(5.15940187380592,0.547113782378707,
5.13635618396623));
#165873=CARTESIAN_POINT('Ctrl Pts',(5.16281063865819,0.546330209533124,
5.1398066163935));
#165874=CARTESIAN_POINT('Ctrl Pts',(5.16621913090739,0.545548955762417,
5.1432578456512));
#165875=CARTESIAN_POINT('Ctrl Pts',(5.16962735214875,0.544769999814018,
5.14670986024279));
#165876=CARTESIAN_POINT('Ctrl Pts',(5.136825309,0.552337930000001,5.116202277));
#165877=CARTESIAN_POINT('Ctrl Pts',(5.249259707,0.526068113,5.00331466500001));
#165878=CARTESIAN_POINT('Ctrl Pts',(5.356626283,0.49968693,4.885596675));
#165879=CARTESIAN_POINT('Ctrl Pts',(5.136953033,0.552337930000001,5.17970211));
#165880=CARTESIAN_POINT('Ctrl Pts',(5.250782913,0.526068113,5.06681169));
#165881=CARTESIAN_POINT('Ctrl Pts',(5.359543499,0.49968693,4.949029591));
#165882=CARTESIAN_POINT('Origin',(-0.15514246281081,0.410743046427657,-0.121555536364255));
#165883=CARTESIAN_POINT('Ctrl Pts',(5.20968127961232,0.552548454735263,
5.11697194808294));
#165884=CARTESIAN_POINT('Ctrl Pts',(5.21079719830616,0.552287640367631,
5.11583481904148));
#165885=CARTESIAN_POINT('Ctrl Pts',(5.211913117,0.552026826,5.11469769000001));
#165886=CARTESIAN_POINT('Ctrl Pts',(5.323648577,0.525911829,5.000838466));
#165887=CARTESIAN_POINT('Ctrl Pts',(5.430305083,0.49968693,4.88220826));
#165888=CARTESIAN_POINT('Ctrl Pts',(5.13591261979726,0.552548454735263,
5.11710733610618));
#165889=CARTESIAN_POINT('Ctrl Pts',(5.13702857506005,0.552287640367631,
5.11598630179857));
#165890=CARTESIAN_POINT('Ctrl Pts',(5.13814453032285,0.552026826,5.11486526749095));
#165891=CARTESIAN_POINT('Ctrl Pts',(5.24988365192353,0.525911829,5.00261758786351));
#165892=CARTESIAN_POINT('Ctrl Pts',(5.35661419406909,0.49968693,4.88559723095795));
#165893=CARTESIAN_POINT('',(5.24791265298529,0.552026824385518,5.11461591869753));
#165894=CARTESIAN_POINT('Ctrl Pts',(5.13261580896174,0.550751630586318,
5.12043129408337));
#165895=CARTESIAN_POINT('Ctrl Pts',(5.13538622048087,0.551389228293159,
5.11764826704169));
#165896=CARTESIAN_POINT('Ctrl Pts',(5.138156632,0.552026826,5.11486524));
#165897=CARTESIAN_POINT('Ctrl Pts',(5.416792268,0.61615356,4.834960791));
#165898=CARTESIAN_POINT('Ctrl Pts',(5.663373315,0.681389364000001,4.526444819));
#165899=CARTESIAN_POINT('Ctrl Pts',(5.35212840517261,0.550751630586318,
5.12017042975023));
#165900=CARTESIAN_POINT('Ctrl Pts',(5.3548985465863,0.551389228293159,5.11726850637512));
#165901=CARTESIAN_POINT('Ctrl Pts',(5.357668688,0.552026826,5.11436658300001));
#165902=CARTESIAN_POINT('Ctrl Pts',(5.636277158,0.61615356,4.822504071));
#165903=CARTESIAN_POINT('Ctrl Pts',(5.88153221,0.681389364000001,4.50210375));
#165904=CARTESIAN_POINT('Ctrl Pts',(5.66042267728532,0.680609082247605,
4.53013414795068));
#165905=CARTESIAN_POINT('Ctrl Pts',(5.67464844079711,0.677652752733401,
4.54129060488698));
#165906=CARTESIAN_POINT('Ctrl Pts',(5.68887846756112,0.67472989689917,4.55245057562457));
#165907=CARTESIAN_POINT('Ctrl Pts',(5.70310224161805,0.6718367825388,4.56362615650412));
#165908=CARTESIAN_POINT('Ctrl Pts',(5.71641786775797,0.669128385382844,
4.57408820801682));
#165909=CARTESIAN_POINT('Ctrl Pts',(5.72973067445805,0.666446714501235,
4.58456080411605));
#165910=CARTESIAN_POINT('Ctrl Pts',(5.74304069858956,0.663790956153864,
4.59504345844241));
#165911=CARTESIAN_POINT('Ctrl Pts',(5.75635086562497,0.661135169292779,
4.60552622531643));
#165912=CARTESIAN_POINT('Ctrl Pts',(5.76965828536143,0.658505288611614,
4.61601907864229));
#165913=CARTESIAN_POINT('Ctrl Pts',(5.7829629925841,0.65590053576872,4.62652156291335));
#165914=CARTESIAN_POINT('Ctrl Pts',(5.65748713,0.681369595,4.533799662));
#165915=CARTESIAN_POINT('Ctrl Pts',(5.662890733,0.679970133,4.527056793));
#165916=CARTESIAN_POINT('Ctrl Pts',(5.668278248,0.678571429,4.520301063));
#165917=CARTESIAN_POINT('Ctrl Pts',(5.90974125700001,0.615882895,4.217516027));
#165918=CARTESIAN_POINT('Ctrl Pts',(6.11757421800001,0.552026826,3.89073074));
#165919=CARTESIAN_POINT('Ctrl Pts',(5.68154471500001,0.681369595,4.75199));
#165920=CARTESIAN_POINT('Ctrl Pts',(5.68720836800001,0.679970133,4.745218458));
#165921=CARTESIAN_POINT('Ctrl Pts',(5.692855864,0.678571429,4.738433436));
#165922=CARTESIAN_POINT('Ctrl Pts',(5.945970951,0.615882895,4.434335525));
#165923=CARTESIAN_POINT('Ctrl Pts',(6.16524982,0.552026826,4.105003528));
#165924=CARTESIAN_POINT('',(6.12558376061154,0.552026824384634,3.92672878840585));
#165925=CARTESIAN_POINT('Ctrl Pts',(5.951337988,0.499686101,4.231518279));
#165926=CARTESIAN_POINT('Ctrl Pts',(6.01608078,0.51775868,4.140462018));
#165927=CARTESIAN_POINT('Ctrl Pts',(6.078007573,0.535714286,4.047467695));
#165928=CARTESIAN_POINT('Ctrl Pts',(6.106094468,0.54385805,4.005290123));
#165929=CARTESIAN_POINT('Ctrl Pts',(6.133593314,0.552026826,3.96272682));
#165930=CARTESIAN_POINT('Ctrl Pts',(5.93853580499999,0.499686101,4.158881159));
#165931=CARTESIAN_POINT('Ctrl Pts',(6.002167238,0.51775868,4.068020773));
#165932=CARTESIAN_POINT('Ctrl Pts',(6.062989186,0.535714286,3.975256234));
#165933=CARTESIAN_POINT('Ctrl Pts',(6.090574979,0.54385805,3.93318288));
#165934=CARTESIAN_POINT('Ctrl Pts',(6.117574218,0.552026826,3.89073074));
#165935=CARTESIAN_POINT('Ctrl Pts',(6.11757421803917,0.552026826,3.89073074017603));
#165936=CARTESIAN_POINT('Ctrl Pts',(6.08891330648077,0.543355301187097,
3.93579560734626));
#165937=CARTESIAN_POINT('Ctrl Pts',(6.0597797826872,0.534726107642318,3.98050483233341));
#165938=CARTESIAN_POINT('Ctrl Pts',(6.00046156891768,0.517398613547625,
4.06937582139407));
#165939=CARTESIAN_POINT('Ctrl Pts',(5.97029013381289,0.508707842303121,
4.11351354118986));
#165940=CARTESIAN_POINT('Ctrl Pts',(5.93963516527631,0.499998391797793,
4.15731092236549));
#165941=CARTESIAN_POINT('Ctrl Pts',(5.93853580499999,0.499686101,4.158881159));
#165942=CARTESIAN_POINT('Ctrl Pts',(6.002167238,0.51775868,4.068020773));
#165943=CARTESIAN_POINT('Ctrl Pts',(6.062989186,0.535714286,3.975256234));
#165944=CARTESIAN_POINT('Ctrl Pts',(6.091102341,0.544013736,3.932378558));
#165945=CARTESIAN_POINT('Ctrl Pts',(6.118606248,0.552339147,3.889107555));
#165946=CARTESIAN_POINT('Ctrl Pts',(6.001071897,0.499686101,4.147859266));
#165947=CARTESIAN_POINT('Ctrl Pts',(6.064534695,0.51775868,4.05604207));
#165948=CARTESIAN_POINT('Ctrl Pts',(6.125158813,0.535714286,3.962326327));
#165949=CARTESIAN_POINT('Ctrl Pts',(6.153180527,0.544013736,3.919008985));
#165950=CARTESIAN_POINT('Ctrl Pts',(6.180586785,0.552339147,3.875299654));
#165951=CARTESIAN_POINT('Ctrl Pts',(6.11757422061379,0.552026827147516,
3.89073073448356));
#165952=CARTESIAN_POINT('Ctrl Pts',(6.12195958097685,0.551172308249902,
3.89356741198595));
#165953=CARTESIAN_POINT('Ctrl Pts',(6.12634483044024,0.550320534923268,
3.89640507858448));
#165954=CARTESIAN_POINT('Ctrl Pts',(6.13072996930273,0.549471478017472,
3.8992437271493));
#165955=CARTESIAN_POINT('Ctrl Pts',(6.13480096609976,0.548683245751088,
3.90187902093991));
#165956=CARTESIAN_POINT('Ctrl Pts',(6.13887186866908,0.54789735444499,3.9045151617502));
#165957=CARTESIAN_POINT('Ctrl Pts',(6.14294267528982,0.547113782401498,
3.90715213868288));
#165958=CARTESIAN_POINT('Ctrl Pts',(6.14701348601668,0.546330209567639,
3.90978911827541));
#165959=CARTESIAN_POINT('Ctrl Pts',(6.15108420182122,0.545548955803886,
3.91242693465806));
#165960=CARTESIAN_POINT('Ctrl Pts',(6.15515482213107,0.544770000002306,
3.91506557553979));
#165961=CARTESIAN_POINT('Ctrl Pts',(6.116561444,0.55233793,3.892322713));
#165962=CARTESIAN_POINT('Ctrl Pts',(6.202099688,0.526068113,3.757904278));
#165963=CARTESIAN_POINT('Ctrl Pts',(6.281650205,0.49968693,3.619857829));
#165964=CARTESIAN_POINT('Ctrl Pts',(6.130336769,0.55233793,3.954310498));
#165965=CARTESIAN_POINT('Ctrl Pts',(6.217237265,0.526068113,3.819589334));
#165966=CARTESIAN_POINT('Ctrl Pts',(6.29813542,0.49968693,3.681180604));
#165967=CARTESIAN_POINT('Origin',(-0.177646919336792,0.410743002151109,
-0.085363016941063));
#165968=CARTESIAN_POINT('Ctrl Pts',(6.18787953798209,0.552548454735263,
3.87741250926571));
#165969=CARTESIAN_POINT('Ctrl Pts',(6.18872491799105,0.552287640367631,
3.87606207613285));
#165970=CARTESIAN_POINT('Ctrl Pts',(6.189570298,0.552026826,3.874711643));
#165971=CARTESIAN_POINT('Ctrl Pts',(6.274217078,0.525911829,3.739494563));
#165972=CARTESIAN_POINT('Ctrl Pts',(6.352878027,0.49968693,3.60070987));
#165973=CARTESIAN_POINT('Ctrl Pts',(6.11586465391192,0.552548454735263,
3.89340281343582));
#165974=CARTESIAN_POINT('Ctrl Pts',(6.11671352951712,0.552287640367631,
3.89206809089803));
#165975=CARTESIAN_POINT('Ctrl Pts',(6.11756240512232,0.552026826,3.89073336836023));
#165976=CARTESIAN_POINT('Ctrl Pts',(6.20255919454128,0.525911829,3.7570893694238));
#165977=CARTESIAN_POINT('Ctrl Pts',(6.28163851817553,0.49968693,3.61986097073352));
#165978=CARTESIAN_POINT('',(6.22471060719365,0.552026824384635,3.86689294754188));
#165979=CARTESIAN_POINT('Ctrl Pts',(6.1133582207917,0.550751630586317,3.89735805329302));
#165980=CARTESIAN_POINT('Ctrl Pts',(6.11546559322124,0.551389228293159,
3.89404453597009));
#165981=CARTESIAN_POINT('Ctrl Pts',(6.1175729656508,0.552026826,3.89073101864715));
#165982=CARTESIAN_POINT('Ctrl Pts',(6.32952308683028,0.61615356,3.5574722228697));
#165983=CARTESIAN_POINT('Ctrl Pts',(6.50401741433089,0.681389364000001,
3.20316161303959));
#165984=CARTESIAN_POINT('Ctrl Pts',(6.32768390839934,0.550751630586317,
3.8499142910946));
#165985=CARTESIAN_POINT('Ctrl Pts',(6.32976545769968,0.551389228293159,
3.8464847145473));
#165986=CARTESIAN_POINT('Ctrl Pts',(6.331847007,0.552026826,3.843055138));
#165987=CARTESIAN_POINT('Ctrl Pts',(6.541199953,0.61615356,3.498123623));
#165988=CARTESIAN_POINT('Ctrl Pts',(6.71184448,0.681389364000001,3.132491498));
#165989=CARTESIAN_POINT('Ctrl Pts',(6.50193007241179,0.680609082082812,
3.20739857430726));
#165990=CARTESIAN_POINT('Ctrl Pts',(6.51822155404743,0.677652752690646,
3.21523608098733));
#165991=CARTESIAN_POINT('Ctrl Pts',(6.53451795468387,0.674729896901062,
3.22307610241689));
#165992=CARTESIAN_POINT('Ctrl Pts',(6.55081160437425,0.6718367825332,3.23093271345657));
#165993=CARTESIAN_POINT('Ctrl Pts',(6.56606495036792,0.669128385379044,
3.23828770198298));
#165994=CARTESIAN_POINT('Ctrl Pts',(6.58131780961128,0.666446714497193,
3.24565359466854));
#165995=CARTESIAN_POINT('Ctrl Pts',(6.59657011356126,0.663790956148093,
3.25302990859755));
#165996=CARTESIAN_POINT('Ctrl Pts',(6.61182258126854,0.66113516928528,3.26040630172281));
#165997=CARTESIAN_POINT('Ctrl Pts',(6.62707453419494,0.6585052886009,3.26779313607438));
#165998=CARTESIAN_POINT('Ctrl Pts',(6.64232590877187,0.655900535624813,
3.27518995864757));
#165999=CARTESIAN_POINT('Ctrl Pts',(6.499851134,0.681369595,3.211609446));
#166000=CARTESIAN_POINT('Ctrl Pts',(6.503678886,0.679970133000001,3.203862607));
#166001=CARTESIAN_POINT('Ctrl Pts',(6.507488162,0.678571429,3.196106666));
#166002=CARTESIAN_POINT('Ctrl Pts',(6.678216068,0.615882895,2.848493166));
#166003=CARTESIAN_POINT('Ctrl Pts',(6.81094083199999,0.552026826,2.484669994));
#166004=CARTESIAN_POINT('Ctrl Pts',(6.570250739,0.681369595,3.419526946));
#166005=CARTESIAN_POINT('Ctrl Pts',(6.574326298,0.679970133000001,3.411696201));
#166006=CARTESIAN_POINT('Ctrl Pts',(6.578383179,0.678571429,3.403855764));
#166007=CARTESIAN_POINT('Ctrl Pts',(6.76020851400001,0.615882895,3.052455232));
#166008=CARTESIAN_POINT('Ctrl Pts',(6.903564121,0.552026826,2.683684359));
#166009=CARTESIAN_POINT('',(6.82650163254454,0.552026824384641,2.51810461336765));
#166010=CARTESIAN_POINT('Ctrl Pts',(6.72185036,0.499686101,2.853225986));
#166011=CARTESIAN_POINT('Ctrl Pts',(6.76550509700001,0.51775868,2.750380783));
#166012=CARTESIAN_POINT('Ctrl Pts',(6.805993045,0.535714286,2.646248186));
#166013=CARTESIAN_POINT('Ctrl Pts',(6.824356353,0.54385805,2.59901885));
#166014=CARTESIAN_POINT('Ctrl Pts',(6.84206244,0.552026826,2.551539214));
#166015=CARTESIAN_POINT('Ctrl Pts',(6.693732651,0.499686101,2.785039173));
#166016=CARTESIAN_POINT('Ctrl Pts',(6.73634412,0.51775868,2.682624175));
#166017=CARTESIAN_POINT('Ctrl Pts',(6.775802451,0.535714286,2.578953498));
#166018=CARTESIAN_POINT('Ctrl Pts',(6.793698776,0.54385805,2.531933665));
#166019=CARTESIAN_POINT('Ctrl Pts',(6.81094083200001,0.552026826,2.484669994));
#166020=CARTESIAN_POINT('Ctrl Pts',(6.81094083261732,0.552026826308274,
2.48466999368684));
#166021=CARTESIAN_POINT('Ctrl Pts',(6.79943769339592,0.54657697978499,2.51620222876931));
#166022=CARTESIAN_POINT('Ctrl Pts',(6.78772401181845,0.541139220273715,
2.54763143566997));
#166023=CARTESIAN_POINT('Ctrl Pts',(6.77580245095149,0.535714285977923,
2.57895349812747));
#166024=CARTESIAN_POINT('Ctrl Pts',(6.74976989147918,0.5238681087781,2.64735003178684));
#166025=CARTESIAN_POINT('Ctrl Pts',(6.72265704507204,0.511960760856659,
2.71546906758587));
#166026=CARTESIAN_POINT('Ctrl Pts',(6.69447254313508,0.49999999963666,2.78326020476335));
#166027=CARTESIAN_POINT('Ctrl Pts',(6.693732651,0.499686101,2.785039173));
#166028=CARTESIAN_POINT('Ctrl Pts',(6.73634412,0.51775868,2.682624175));
#166029=CARTESIAN_POINT('Ctrl Pts',(6.775802451,0.535714286,2.578953498));
#166030=CARTESIAN_POINT('Ctrl Pts',(6.794040902,0.544013736,2.531034781));
#166031=CARTESIAN_POINT('Ctrl Pts',(6.811599798,0.552339147,2.482862903));
#166032=CARTESIAN_POINT('Ctrl Pts',(6.752437304,0.499686101,2.760831554));
#166033=CARTESIAN_POINT('Ctrl Pts',(6.794678393,0.51775868,2.657518367));
#166034=CARTESIAN_POINT('Ctrl Pts',(6.833739039,0.535714286,2.552961253));
#166035=CARTESIAN_POINT('Ctrl Pts',(6.851793672,0.544013736,2.504632806));
#166036=CARTESIAN_POINT('Ctrl Pts',(6.86916297300001,0.552339147,2.45605384));
#166037=CARTESIAN_POINT('Ctrl Pts',(6.81094083475798,0.552026827322456,
2.48466998781889));
#166038=CARTESIAN_POINT('Ctrl Pts',(6.81583346809674,0.551172308262818,
2.48649762393515));
#166039=CARTESIAN_POINT('Ctrl Pts',(6.82072620731759,0.550320534934142,
2.48832624838348));
#166040=CARTESIAN_POINT('Ctrl Pts',(6.82561904961501,0.549471478028082,
2.49015585562438));
#166041=CARTESIAN_POINT('Ctrl Pts',(6.8301613790905,0.548683245754012,2.49185439369157));
#166042=CARTESIAN_POINT('Ctrl Pts',(6.83470379862338,0.547897354441908,
2.49355377923814));
#166043=CARTESIAN_POINT('Ctrl Pts',(6.83924630418656,0.547113782394639,
2.49525400198954));
#166044=CARTESIAN_POINT('Ctrl Pts',(6.84378881433968,0.546330209555615,
2.49695422645892));
#166045=CARTESIAN_POINT('Ctrl Pts',(6.84833141166887,0.545548955788871,
2.49865528856461));
#166046=CARTESIAN_POINT('Ctrl Pts',(6.8528740929523,0.544769999918643,2.50035717676483));
#166047=CARTESIAN_POINT('Ctrl Pts',(6.810293963,0.55233793,2.486442465));
#166048=CARTESIAN_POINT('Ctrl Pts',(6.864936381,0.526068113,2.336778465));
#166049=CARTESIAN_POINT('Ctrl Pts',(6.912951145,0.49968693,2.184858455));
#166050=CARTESIAN_POINT('Ctrl Pts',(6.83707277,0.55233793,2.544019722));
#166051=CARTESIAN_POINT('Ctrl Pts',(6.892980514,0.526068113,2.393767227));
#166052=CARTESIAN_POINT('Ctrl Pts',(6.942233529,0.49968693,2.241203703));
#166053=CARTESIAN_POINT('Origin',(-0.191842828234754,0.410743194362546,
-0.045178034189591));
#166054=CARTESIAN_POINT('Ctrl Pts',(6.87673942742404,0.552548454735263,
2.45654957195124));
#166055=CARTESIAN_POINT('Ctrl Pts',(6.87727473971202,0.552287640367631,
2.45504897947562));
#166056=CARTESIAN_POINT('Ctrl Pts',(6.877810052,0.552026826,2.453548387));
#166057=CARTESIAN_POINT('Ctrl Pts',(6.93141016200001,0.525911829,2.303296051));
#166058=CARTESIAN_POINT('Ctrl Pts',(6.978397455,0.49968693,2.150846288));
#166059=CARTESIAN_POINT('Ctrl Pts',(6.80984565338549,0.552548454735263,
2.48764710157255));
#166060=CARTESIAN_POINT('Ctrl Pts',(6.81038775686044,0.552287640367631,
2.48616110094776));
#166061=CARTESIAN_POINT('Ctrl Pts',(6.8109298603354,0.552026826,2.48467510032297));
#166062=CARTESIAN_POINT('Ctrl Pts',(6.86520996288786,0.525911828999999,
2.33588382700963));
#166063=CARTESIAN_POINT('Ctrl Pts',(6.91294040680142,0.49968693,2.18486403559581));
#166064=CARTESIAN_POINT('',(6.91044801115398,0.552026824384643,2.43835835948284));
#166065=CARTESIAN_POINT('Ctrl Pts',(6.80824807877956,0.550751630586317,
2.49204867921741));
#166066=CARTESIAN_POINT('Ctrl Pts',(6.80959387373918,0.551389228293159,
2.48835960731475));
#166067=CARTESIAN_POINT('Ctrl Pts',(6.81093966869881,0.552026826,2.48467053541208));
#166068=CARTESIAN_POINT('Ctrl Pts',(6.94629372419259,0.61615356,2.11364013478368));
#166069=CARTESIAN_POINT('Ctrl Pts',(7.04054216339582,0.681389364000001,
1.73010198757639));
#166070=CARTESIAN_POINT('Ctrl Pts',(7.00736394446831,0.550751630586317,
2.39964043902942));
#166071=CARTESIAN_POINT('Ctrl Pts',(7.00865957073415,0.551389228293159,
2.39584357251471));
#166072=CARTESIAN_POINT('Ctrl Pts',(7.009955197,0.552026826,2.392046706));
#166073=CARTESIAN_POINT('Ctrl Pts',(7.140263509,0.61615356,2.010174804));
#166074=CARTESIAN_POINT('Ctrl Pts',(7.228318362,0.681389364000001,1.616407425));
#166075=CARTESIAN_POINT('Ctrl Pts',(7.03941444436854,0.680609082247612,
1.73468860817335));
#166076=CARTESIAN_POINT('Ctrl Pts',(7.05700987218025,0.67765275265413,1.73884069106667));
#166077=CARTESIAN_POINT('Ctrl Pts',(7.07461064485539,0.674729896832154,
1.74299417296873));
#166078=CARTESIAN_POINT('Ctrl Pts',(7.09221229723318,0.671836782470486,
1.74716444778147));
#166079=CARTESIAN_POINT('Ctrl Pts',(7.10869013358932,0.669128385327537,
1.7510684622711));
#166080=CARTESIAN_POINT('Ctrl Pts',(7.12516983864625,0.6664467144582,1.75498323062767));
#166081=CARTESIAN_POINT('Ctrl Pts',(7.14165124165079,0.663790956122426,
1.75890829596002));
#166082=CARTESIAN_POINT('Ctrl Pts',(7.15813282160895,0.661135169272935,
1.76283340343409));
#166083=CARTESIAN_POINT('Ctrl Pts',(7.17461614337578,0.658505288602688,
1.76676881869064));
#166084=CARTESIAN_POINT('Ctrl Pts',(7.19110104737666,0.655900535702375,
1.77071411332688));
#166085=CARTESIAN_POINT('Ctrl Pts',(7.038289323,0.681369595,1.739247943));
#166086=CARTESIAN_POINT('Ctrl Pts',(7.040362243,0.679970133000001,1.730859367));
#166087=CARTESIAN_POINT('Ctrl Pts',(7.042415162,0.678571429,1.722465874));
#166088=CARTESIAN_POINT('Ctrl Pts',(7.134424917,0.615882895,1.346277931));
#166089=CARTESIAN_POINT('Ctrl Pts',(7.185835423,0.552026826,0.962428841999999));
#166090=CARTESIAN_POINT('Ctrl Pts',(7.15173914100001,0.681369595,1.927170612));
#166091=CARTESIAN_POINT('Ctrl Pts',(7.154036037,0.679970133000001,1.918646822));
#166092=CARTESIAN_POINT('Ctrl Pts',(7.156312608,0.678571429,1.91011758));
#166093=CARTESIAN_POINT('Ctrl Pts',(7.258346241,0.615882895,1.527845525));
#166094=CARTESIAN_POINT('Ctrl Pts',(7.319075436,0.552026826,1.136879092));
#166095=CARTESIAN_POINT('',(7.20821987513909,0.552026824384642,0.991736666391452));
#166096=CARTESIAN_POINT('Ctrl Pts',(7.178056481,0.499686101,1.341520017));
#166097=CARTESIAN_POINT('Ctrl Pts',(7.198581915,0.51775868,1.2316948));
#166098=CARTESIAN_POINT('Ctrl Pts',(7.215737847,0.535714286,1.121293053));
#166099=CARTESIAN_POINT('Ctrl Pts',(7.22351891999999,0.54385805,1.071220344));
#166100=CARTESIAN_POINT('Ctrl Pts',(7.23060433,0.552026826,1.021044471));
#166101=CARTESIAN_POINT('Ctrl Pts',(7.135937999,0.499686101,1.28097185));
#166102=CARTESIAN_POINT('Ctrl Pts',(7.155537038,0.51775868,1.171791051));
#166103=CARTESIAN_POINT('Ctrl Pts',(7.171786724,0.535714286,1.062061763));
#166104=CARTESIAN_POINT('Ctrl Pts',(7.179156768,0.54385805,1.012294047));
#166105=CARTESIAN_POINT('Ctrl Pts',(7.185835423,0.552026826,0.962428842));
#166106=CARTESIAN_POINT('Ctrl Pts',(7.18583542290858,0.552026826224196,
0.962428841470711));
#166107=CARTESIAN_POINT('Ctrl Pts',(7.18137971978687,0.546576979749282,
0.995696704485362));
#166108=CARTESIAN_POINT('Ctrl Pts',(7.17669624816509,0.541139220265819,
1.02890920921096));
#166109=CARTESIAN_POINT('Ctrl Pts',(7.17178672409763,0.535714286068517,
1.06206176255485));
#166110=CARTESIAN_POINT('Ctrl Pts',(7.16106602474232,0.523868109155108,
1.13445545159152));
#166111=CARTESIAN_POINT('Ctrl Pts',(7.14923064057945,0.511960761034125,
1.20681036385961));
#166112=CARTESIAN_POINT('Ctrl Pts',(7.13627816756703,0.499999999904053,
1.27907541649017));
#166113=CARTESIAN_POINT('Ctrl Pts',(7.135937999,0.499686101,1.28097185));
#166114=CARTESIAN_POINT('Ctrl Pts',(7.155537038,0.51775868,1.171791051));
#166115=CARTESIAN_POINT('Ctrl Pts',(7.171786724,0.535714286,1.062061763));
#166116=CARTESIAN_POINT('Ctrl Pts',(7.179297663,0.544013736,1.01134263));
#166117=CARTESIAN_POINT('Ctrl Pts',(7.186090511,0.552339147,0.960522341));
#166118=CARTESIAN_POINT('Ctrl Pts',(7.188066246,0.499686101,1.244710427));
#166119=CARTESIAN_POINT('Ctrl Pts',(7.20711048100001,0.51775868,1.13473206));
#166120=CARTESIAN_POINT('Ctrl Pts',(7.222781222,0.535714286,1.024222548));
#166121=CARTESIAN_POINT('Ctrl Pts',(7.230024561,0.544013736,0.973142781));
#166122=CARTESIAN_POINT('Ctrl Pts',(7.236544735,0.552339147,0.921965678));
#166123=CARTESIAN_POINT('Ctrl Pts',(7.18583542372051,0.55202682721728,0.962428835408557));
#166124=CARTESIAN_POINT('Ctrl Pts',(7.19100655813224,0.551172308295944,
0.963161969826103));
#166125=CARTESIAN_POINT('Ctrl Pts',(7.1961780079224,0.550320534986493,0.96389604776062));
#166126=CARTESIAN_POINT('Ctrl Pts',(7.20134976964962,0.549471478100325,
0.964631063358087));
#166127=CARTESIAN_POINT('Ctrl Pts',(7.20615103750445,0.548683245820979,
0.96531342402106));
#166128=CARTESIAN_POINT('Ctrl Pts',(7.21095257549354,0.547897354504228,
0.965996592995543));
#166129=CARTESIAN_POINT('Ctrl Pts',(7.21575437747613,0.547113782451772,
0.966680561105015));
#166130=CARTESIAN_POINT('Ctrl Pts',(7.22055618431066,0.546330209607562,
0.967364529905598));
#166131=CARTESIAN_POINT('Ctrl Pts',(7.2253582563504,0.545548955835064,0.968049298016219));
#166132=CARTESIAN_POINT('Ctrl Pts',(7.23016058789743,0.544769999904026,
0.968734855199174));
#166133=CARTESIAN_POINT('Ctrl Pts',(7.185584706,0.55233793,0.96429893));
#166134=CARTESIAN_POINT('Ctrl Pts',(7.206776278,0.526068113,0.806387487));
#166135=CARTESIAN_POINT('Ctrl Pts',(7.221010173,0.49968693,0.647697528000001));
#166136=CARTESIAN_POINT('Ctrl Pts',(7.22411484800001,0.55233793,1.014773411));
#166137=CARTESIAN_POINT('Ctrl Pts',(7.246415654,0.526068113,0.856015224000001));
#166138=CARTESIAN_POINT('Ctrl Pts',(7.261720514,0.49968693,0.696430608));
#166139=CARTESIAN_POINT('Origin',(-0.19707097630675,0.410743212774269,-0.00288142655035101));
#166140=CARTESIAN_POINT('Ctrl Pts',(7.24405062408982,0.552548454735263,
0.920821105528827));
#166141=CARTESIAN_POINT('Ctrl Pts',(7.24425083804491,0.552287640367631,
0.919240519764414));
#166142=CARTESIAN_POINT('Ctrl Pts',(7.244451052,0.552026826,0.917659933999999));
#166143=CARTESIAN_POINT('Ctrl Pts',(7.26449821,0.525911829,0.759397976));
#166144=CARTESIAN_POINT('Ctrl Pts',(7.277614774,0.49968693,0.600411524));
#166145=CARTESIAN_POINT('Ctrl Pts',(7.18540583920389,0.552548454735263,
0.965571777466926));
#166146=CARTESIAN_POINT('Ctrl Pts',(7.18561582239313,0.552287640367631,
0.964003982485016));
#166147=CARTESIAN_POINT('Ctrl Pts',(7.18582580558238,0.552026826,0.962436187503104));
#166148=CARTESIAN_POINT('Ctrl Pts',(7.20685114405198,0.525911829,0.805454953604712));
#166149=CARTESIAN_POINT('Ctrl Pts',(7.22100088554379,0.49968693,0.647705286498134));
#166150=CARTESIAN_POINT('',(7.27306054677073,0.552026824384643,0.895808845480426));
#166151=CARTESIAN_POINT('Ctrl Pts',(7.18479182409675,0.550751630586318,
0.970213879985565));
#166152=CARTESIAN_POINT('Ctrl Pts',(7.18531311370807,0.551389228293159,
0.966321750393941));
#166153=CARTESIAN_POINT('Ctrl Pts',(7.18583440331938,0.552026826,0.962429620802318));
#166154=CARTESIAN_POINT('Ctrl Pts',(7.23826338774514,0.61615356,0.570976583350089));
#166155=CARTESIAN_POINT('Ctrl Pts',(7.24785898595394,0.681389364,0.17614471596048));
#166156=CARTESIAN_POINT('Ctrl Pts',(7.3593874306487,0.550751630586318,0.837162067481765));
#166157=CARTESIAN_POINT('Ctrl Pts',(7.35983655182435,0.551389228293159,
0.833175448240883));
#166158=CARTESIAN_POINT('Ctrl Pts',(7.360285673,0.552026826,0.829188829000001));
#166159=CARTESIAN_POINT('Ctrl Pts',(7.405456278,0.61615356,0.428232444));
#166160=CARTESIAN_POINT('Ctrl Pts',(7.406804111,0.681389364,0.024741937));
#166161=CARTESIAN_POINT('Ctrl Pts',(7.24774362022223,0.680609082082813,
0.180866530342211));
#166162=CARTESIAN_POINT('Ctrl Pts',(7.26582025148185,0.677652752743715,
0.181139042606722));
#166163=CARTESIAN_POINT('Ctrl Pts',(7.28390240363902,0.674729896880472,
0.181411772860856));
#166164=CARTESIAN_POINT('Ctrl Pts',(7.30198902492249,0.671836782520085,
0.181700714026023));
#166165=CARTESIAN_POINT('Ctrl Pts',(7.31892086638184,0.669128385362535,
0.181971207111659));
#166166=CARTESIAN_POINT('Ctrl Pts',(7.33585684461614,0.666446714477168,
0.182251800924234));
#166167=CARTESIAN_POINT('Ctrl Pts',(7.35279669464631,0.663790956124307,
0.182542085962166));
#166168=CARTESIAN_POINT('Ctrl Pts',(7.36973672655222,0.661135169257735,
0.182832374116761));
#166169=CARTESIAN_POINT('Ctrl Pts',(7.38668067541274,0.65850528856935,0.183132354621936));
#166170=CARTESIAN_POINT('Ctrl Pts',(7.40362829346862,0.655900535690581,
0.183441643835477));
#166171=CARTESIAN_POINT('Ctrl Pts',(7.247624926,0.681369595,0.185561138));
#166172=CARTESIAN_POINT('Ctrl Pts',(7.247846087,0.679970133000001,0.176923066));
#166173=CARTESIAN_POINT('Ctrl Pts',(7.248046656,0.678571429,0.168284491));
#166174=CARTESIAN_POINT('Ctrl Pts',(7.257035987,0.615882895,-0.218887764));
#166175=CARTESIAN_POINT('Ctrl Pts',(7.224728336,0.552026826,-0.604814414));
#166176=CARTESIAN_POINT('Ctrl Pts',(7.398820169,0.681369595,0.344701923));
#166177=CARTESIAN_POINT('Ctrl Pts',(7.399231002,0.679970133000001,0.335883649));
#166178=CARTESIAN_POINT('Ctrl Pts',(7.399620813,0.678571429,0.327064421));
#166179=CARTESIAN_POINT('Ctrl Pts',(7.417091764,0.615882895,-0.068204541));
#166180=CARTESIAN_POINT('Ctrl Pts',(7.39235491900001,0.552026826,-0.463085377));
#166181=CARTESIAN_POINT('',(7.25288976829728,0.552026824384642,-0.58100378604725));
#166182=CARTESIAN_POINT('Ctrl Pts',(7.298624658,0.499686101,-0.232913937));
#166183=CARTESIAN_POINT('Ctrl Pts',(7.295061043,0.51775868,-0.344583863));
#166184=CARTESIAN_POINT('Ctrl Pts',(7.288082768,0.535714286,-0.456092497));
#166185=CARTESIAN_POINT('Ctrl Pts',(7.28491777100001,0.54385805,-0.506667235));
#166186=CARTESIAN_POINT('Ctrl Pts',(7.281051199,0.552026826,-0.557193178));
#166187=CARTESIAN_POINT('Ctrl Pts',(7.244474816,0.499686101,-0.282992293));
#166188=CARTESIAN_POINT('Ctrl Pts',(7.240144997,0.51775868,-0.393833719));
#166189=CARTESIAN_POINT('Ctrl Pts',(7.23242622,0.535714286,-0.5044908));
#166190=CARTESIAN_POINT('Ctrl Pts',(7.22892537,0.54385805,-0.554679316));
#166191=CARTESIAN_POINT('Ctrl Pts',(7.224728336,0.552026826,-0.604814414));
#166192=CARTESIAN_POINT('Ctrl Pts',(7.22472833621218,0.552026825690736,
-0.604814410755777));
#166193=CARTESIAN_POINT('Ctrl Pts',(7.22752841142424,0.54657697938733,-0.571366488107131));
#166194=CARTESIAN_POINT('Ctrl Pts',(7.23009414317034,0.541139220081692,
-0.537923666472421));
#166195=CARTESIAN_POINT('Ctrl Pts',(7.23242622016378,0.535714285974483,
-0.504490800018465));
#166196=CARTESIAN_POINT('Ctrl Pts',(7.23751866907381,0.523868108761501,
-0.431484999794813));
#166197=CARTESIAN_POINT('Ctrl Pts',(7.24151415645778,0.51196076084533,-0.358277448234718));
#166198=CARTESIAN_POINT('Ctrl Pts',(7.24439935455547,0.499999999619591,
-0.284917513379212));
#166199=CARTESIAN_POINT('Ctrl Pts',(7.244474816,0.499686101,-0.282992293));
#166200=CARTESIAN_POINT('Ctrl Pts',(7.240144997,0.51775868,-0.393833719));
#166201=CARTESIAN_POINT('Ctrl Pts',(7.23242622,0.535714286,-0.5044908));
#166202=CARTESIAN_POINT('Ctrl Pts',(7.228858443,0.544013736,-0.555638777));
#166203=CARTESIAN_POINT('Ctrl Pts',(7.224567619,0.552339147,-0.606731178));
#166204=CARTESIAN_POINT('Ctrl Pts',(7.287589201,0.499686101,-0.329611976));
#166205=CARTESIAN_POINT('Ctrl Pts',(7.282546094,0.51775868,-0.441113058));
#166206=CARTESIAN_POINT('Ctrl Pts',(7.274094183,0.535714286,-0.552407665));
#166207=CARTESIAN_POINT('Ctrl Pts',(7.270187536,0.544013736,-0.603850319));
#166208=CARTESIAN_POINT('Ctrl Pts',(7.265553708,0.552339147,-0.655232575));
#166209=CARTESIAN_POINT('Ctrl Pts',(7.22472833538008,0.552026827310272,
-0.604814420695526));
#166210=CARTESIAN_POINT('Ctrl Pts',(7.22993617385133,0.551172308278917,
-0.605210067129426));
#166211=CARTESIAN_POINT('Ctrl Pts',(7.2351445231257,0.550320534943619,-0.605604860412332));
#166212=CARTESIAN_POINT('Ctrl Pts',(7.24035337861515,0.549471478034166,
-0.605998805004023));
#166213=CARTESIAN_POINT('Ctrl Pts',(7.24518908277755,0.548683245755601,
-0.606364528243161));
#166214=CARTESIAN_POINT('Ctrl Pts',(7.25002522452255,0.547897354441788,
-0.606729520133145));
#166215=CARTESIAN_POINT('Ctrl Pts',(7.25486179588049,0.547113782394678,
-0.607093788313525));
#166216=CARTESIAN_POINT('Ctrl Pts',(7.25969837212551,0.546330209555811,
-0.607458056861978));
#166217=CARTESIAN_POINT('Ctrl Pts',(7.26453537920458,0.545548955791126,
-0.607821601790319));
#166218=CARTESIAN_POINT('Ctrl Pts',(7.26937280931071,0.544769999981471,
-0.608184432575306));
#166219=CARTESIAN_POINT('Ctrl Pts',(7.224885495,0.55233793,-0.60293415));
#166220=CARTESIAN_POINT('Ctrl Pts',(7.211635327,0.526068113,-0.761709274));
#166221=CARTESIAN_POINT('Ctrl Pts',(7.19142279,0.49968693,-0.919749016));
#166222=CARTESIAN_POINT('Ctrl Pts',(7.273365344,0.55233793,-0.561922576));
#166223=CARTESIAN_POINT('Ctrl Pts',(7.261016453,0.526068113,-0.721763100000001));
#166224=CARTESIAN_POINT('Ctrl Pts',(7.241657518,0.49968693,-0.880906808));
#166225=CARTESIAN_POINT('Origin',(-0.193082213202791,0.410742918316382,
0.0395503751822959));
#166226=CARTESIAN_POINT('Ctrl Pts',(7.2726380643031,0.552548454735263,-0.657963931735703));
#166227=CARTESIAN_POINT('Ctrl Pts',(7.27249381815155,0.552287640367631,
-0.659550604367851));
#166228=CARTESIAN_POINT('Ctrl Pts',(7.272349572,0.552026826,-0.661137277));
#166229=CARTESIAN_POINT('Ctrl Pts',(7.257906396,0.525911829,-0.820008705));
#166230=CARTESIAN_POINT('Ctrl Pts',(7.236538914,0.49968693,-0.978097815));
#166231=CARTESIAN_POINT('Ctrl Pts',(7.22498443381837,0.552548454735263,
-0.601652610755724));
#166232=CARTESIAN_POINT('Ctrl Pts',(7.22485247814092,0.552287640367631,
-0.603228891742362));
#166233=CARTESIAN_POINT('Ctrl Pts',(7.22472052246348,0.552026826,-0.604805172728999));
#166234=CARTESIAN_POINT('Ctrl Pts',(7.21150797534791,0.525911829,-0.762636099034893));
#166235=CARTESIAN_POINT('Ctrl Pts',(7.19141538749405,0.49968693,-0.919739442320051));
#166236=CARTESIAN_POINT('',(7.29559285494497,0.552026824384643,-0.688627695488655));
#166237=CARTESIAN_POINT('Ctrl Pts',(7.22538351839981,0.550751630586317,
-0.596988021858047));
#166238=CARTESIAN_POINT('Ctrl Pts',(7.2250559271999,0.551389228293159,-0.600901217929023));
#166239=CARTESIAN_POINT('Ctrl Pts',(7.224728336,0.552026826,-0.604814414));
#166240=CARTESIAN_POINT('Ctrl Pts',(7.191780674,0.61615356,-0.998386224));
#166241=CARTESIAN_POINT('Ctrl Pts',(7.116274695,0.681389364000001,-1.38604995));
#166242=CARTESIAN_POINT('Ctrl Pts',(7.36729414063743,0.550751630586317,
-0.764461072856926));
#166243=CARTESIAN_POINT('Ctrl Pts',(7.36687575631872,0.551389228293159,
-0.768451034928463));
#166244=CARTESIAN_POINT('Ctrl Pts',(7.366457372,0.552026826,-0.772440997));
#166245=CARTESIAN_POINT('Ctrl Pts',(7.32437814300001,0.61615356,-1.173733589));
#166246=CARTESIAN_POINT('Ctrl Pts',(7.238955932,0.681389364000001,-1.568080456));
#166247=CARTESIAN_POINT('Ctrl Pts',(7.11717635924934,0.680609082247611,
-1.38141266504748));
#166248=CARTESIAN_POINT('Ctrl Pts',(7.13488895149141,0.677652752755135,
-1.38503246517533));
#166249=CARTESIAN_POINT('Ctrl Pts',(7.15260698192933,0.674729896880673,
-1.38865323946184));
#166250=CARTESIAN_POINT('Ctrl Pts',(7.17033286187557,0.67183678251324,-1.39225914256789));
#166251=CARTESIAN_POINT('Ctrl Pts',(7.18692699430104,0.669128385351528,
-1.39563481891437));
#166252=CARTESIAN_POINT('Ctrl Pts',(7.20352733814618,0.666446714464127,
-1.39900151995733));
#166253=CARTESIAN_POINT('Ctrl Pts',(7.22013354659556,0.663790956110893,
-1.40235958866437));
#166254=CARTESIAN_POINT('Ctrl Pts',(7.23673993333856,0.661135169243937,
-1.40571769342553));
#166255=CARTESIAN_POINT('Ctrl Pts',(7.25335222903067,0.658505288556828,
-1.40906717445963));
#166256=CARTESIAN_POINT('Ctrl Pts',(7.26997010890117,0.655900535569512,
-1.41240835399411));
#166257=CARTESIAN_POINT('Ctrl Pts',(7.118069642,0.681369595,-1.376802299));
#166258=CARTESIAN_POINT('Ctrl Pts',(7.116428702,0.679970133000001,-1.385285961));
#166259=CARTESIAN_POINT('Ctrl Pts',(7.114767544,0.678571429,-1.393765687));
#166260=CARTESIAN_POINT('Ctrl Pts',(7.040316119,0.615882895,-1.77381851));
#166261=CARTESIAN_POINT('Ctrl Pts',(6.925800981,0.552026826,-2.14377722));
#166262=CARTESIAN_POINT('Ctrl Pts',(7.299940589,0.681369595,-1.253884645));
#166263=CARTESIAN_POINT('Ctrl Pts',(7.298446148,0.679970133000001,-1.262585069));
#166264=CARTESIAN_POINT('Ctrl Pts',(7.296930973,0.678571429,-1.271281907));
#166265=CARTESIAN_POINT('Ctrl Pts',(7.22902232,0.615882895,-1.661065438));
#166266=CARTESIAN_POINT('Ctrl Pts',(7.119976101,0.552026826,-2.04139649));
#166267=CARTESIAN_POINT('',(6.95842259591819,0.552026824384643,-2.12657714645134));
#166268=CARTESIAN_POINT('Ctrl Pts',(7.077917257,0.499686101,-1.796457094));
#166269=CARTESIAN_POINT('Ctrl Pts',(7.050431225,0.51775868,-1.904750168));
#166270=CARTESIAN_POINT('Ctrl Pts',(7.019645038,0.535714286,-2.012151669));
#166271=CARTESIAN_POINT('Ctrl Pts',(7.005681963,0.54385805,-2.060863616));
#166272=CARTESIAN_POINT('Ctrl Pts',(6.99104420499999,0.552026826,-2.109377092));
#166273=CARTESIAN_POINT('Ctrl Pts',(7.014268043,0.499686101,-1.833724031));
#166274=CARTESIAN_POINT('Ctrl Pts',(6.986211822,0.51775868,-1.941043263));
#166275=CARTESIAN_POINT('Ctrl Pts',(6.954885505,0.535714286,-2.047453934));
#166276=CARTESIAN_POINT('Ctrl Pts',(6.940677455,0.54385805,-2.095716491));
#166277=CARTESIAN_POINT('Ctrl Pts',(6.925800981,0.552026826,-2.14377722));
#166278=CARTESIAN_POINT('Ctrl Pts',(6.92580098083625,0.55202682637027,-2.14377722018393));
#166279=CARTESIAN_POINT('Ctrl Pts',(6.93572590766086,0.546576979840938,
-2.11171322393334));
#166280=CARTESIAN_POINT('Ctrl Pts',(6.94542087273066,0.541139220308697,
-2.07960383231208));
#166281=CARTESIAN_POINT('Ctrl Pts',(6.95488550522624,0.53571428595539,-2.04745393400787));
#166282=CARTESIAN_POINT('Ctrl Pts',(6.97555298415123,0.523868108737258,
-1.97724969495729));
#166283=CARTESIAN_POINT('Ctrl Pts',(6.99519251853477,0.511960760918926,
-1.9066126073206));
#166284=CARTESIAN_POINT('Ctrl Pts',(7.01378048014667,0.499999999730479,
-1.83558801947582));
#166285=CARTESIAN_POINT('Ctrl Pts',(7.014268043,0.499686101,-1.833724031));
#166286=CARTESIAN_POINT('Ctrl Pts',(6.986211822,0.51775868,-1.941043263));
#166287=CARTESIAN_POINT('Ctrl Pts',(6.954885505,0.535714286,-2.047453934));
#166288=CARTESIAN_POINT('Ctrl Pts',(6.94040583800001,0.544013736,-2.096639133));
#166289=CARTESIAN_POINT('Ctrl Pts',(6.925231974,0.552339147,-2.145614621));
#166290=CARTESIAN_POINT('Ctrl Pts',(7.04635258300001,0.499686101,-1.88852209));
#166291=CARTESIAN_POINT('Ctrl Pts',(7.017457945,0.51775868,-1.99633222));
#166292=CARTESIAN_POINT('Ctrl Pts',(6.985278584,0.535714286,-2.103207909));
#166293=CARTESIAN_POINT('Ctrl Pts',(6.970404623,0.544013736,-2.152608049));
#166294=CARTESIAN_POINT('Ctrl Pts',(6.954833465,0.552339147,-2.20179288));
#166295=CARTESIAN_POINT('Ctrl Pts',(6.92580097903057,0.552026827361778,
-2.14377722601744));
#166296=CARTESIAN_POINT('Ctrl Pts',(6.93080200909239,0.551172308314244,
-2.14528315383995));
#166297=CARTESIAN_POINT('Ctrl Pts',(6.9358037212145,0.550320534985776,-2.14678835817033));
#166298=CARTESIAN_POINT('Ctrl Pts',(6.94080611015387,0.549471478079757,
-2.14829284249159));
#166299=CARTESIAN_POINT('Ctrl Pts',(6.94545013861374,0.548683245800462,
-2.14968954876334));
#166300=CARTESIAN_POINT('Ctrl Pts',(6.95009475163883,0.547897354483067,
-2.15108563486804));
#166301=CARTESIAN_POINT('Ctrl Pts',(6.95473993980467,0.547113782430111,
-2.15248110655001));
#166302=CARTESIAN_POINT('Ctrl Pts',(6.9593851326642,0.546330209585403,-2.15387657964202));
#166303=CARTESIAN_POINT('Ctrl Pts',(6.96403090183774,0.545548955812596,
-2.1552714386612));
#166304=CARTESIAN_POINT('Ctrl Pts',(6.96867723771985,0.544769999946634,
-2.1566656908487));
#166305=CARTESIAN_POINT('Ctrl Pts',(6.926358667,0.55233793,-2.1419747));
#166306=CARTESIAN_POINT('Ctrl Pts',(6.879286323,0.526068113,-2.294189355));
#166307=CARTESIAN_POINT('Ctrl Pts',(6.825572471,0.49968693,-2.444189118));
#166308=CARTESIAN_POINT('Ctrl Pts',(6.982521361,0.55233793,-2.112343688));
#166309=CARTESIAN_POINT('Ctrl Pts',(6.936100192,0.526068113,-2.265792583));
#166310=CARTESIAN_POINT('Ctrl Pts',(6.882982665,0.49968693,-2.417054001));
#166311=CARTESIAN_POINT('Origin',(-0.180065547040584,0.41074306335028,0.0801325185607973));
#166312=CARTESIAN_POINT('Ctrl Pts',(6.96116503193409,0.552548454735263,
-2.20598330608988));
#166313=CARTESIAN_POINT('Ctrl Pts',(6.96068307046704,0.552287640367631,
-2.20750187454494));
#166314=CARTESIAN_POINT('Ctrl Pts',(6.96020110900001,0.552026826,-2.209020443));
#166315=CARTESIAN_POINT('Ctrl Pts',(6.911942946,0.525911829,-2.36107269));
#166316=CARTESIAN_POINT('Ctrl Pts',(6.857090538,0.49968693,-2.510872388));
#166317=CARTESIAN_POINT('Ctrl Pts',(6.92673078560947,0.552548454735263,
-2.14074439141193));
#166318=CARTESIAN_POINT('Ctrl Pts',(6.92626306117155,0.552287640367631,
-2.14225545325307));
#166319=CARTESIAN_POINT('Ctrl Pts',(6.92579533673362,0.552026826,-2.1437665150942));
#166320=CARTESIAN_POINT('Ctrl Pts',(6.87896270859259,0.525911829,-2.29506713478976));
#166321=CARTESIAN_POINT('Ctrl Pts',(6.82556729961327,0.49968693,-2.44417817681576));
#166322=CARTESIAN_POINT('',(6.97699134907502,0.552026824384643,-2.24086477042585));
#166323=CARTESIAN_POINT('Ctrl Pts',(6.92812268768848,0.550751630586317,
-2.13627351282754));
#166324=CARTESIAN_POINT('Ctrl Pts',(6.9269615345349,0.551389228293159,-2.14002479779588));
#166325=CARTESIAN_POINT('Ctrl Pts',(6.92580038138132,0.552026826,-2.14377608276421));
#166326=CARTESIAN_POINT('Ctrl Pts',(6.80901677533298,0.61615356,-2.52106359609959));
#166327=CARTESIAN_POINT('Ctrl Pts',(6.65193990646636,0.681389364000001,
-2.88343238035801));
#166328=CARTESIAN_POINT('Ctrl Pts',(7.03071436425428,0.550751630586317,
-2.33033886258751));
#166329=CARTESIAN_POINT('Ctrl Pts',(7.02944803762714,0.551389228293159,
-2.33414560129375));
#166330=CARTESIAN_POINT('Ctrl Pts',(7.028181711,0.552026826,-2.33795234));
#166331=CARTESIAN_POINT('Ctrl Pts',(6.900820226,0.61615356,-2.720817143));
#166332=CARTESIAN_POINT('Ctrl Pts',(6.73262222,0.681389364000001,-3.08758115));
#166333=CARTESIAN_POINT('Ctrl Pts',(6.65381784291963,0.680609082082813,
-2.87909853969064));
#166334=CARTESIAN_POINT('Ctrl Pts',(6.67033817410484,0.6776527527603,-2.88644139503094));
#166335=CARTESIAN_POINT('Ctrl Pts',(6.68686360748815,0.67472989688632,-2.89378637035385));
#166336=CARTESIAN_POINT('Ctrl Pts',(6.70339990372129,0.671836782516796,
-2.9011185095998));
#166337=CARTESIAN_POINT('Ctrl Pts',(6.71888040393973,0.669128385364379,
-2.90798251237273));
#166338=CARTESIAN_POINT('Ctrl Pts',(6.73436889977625,0.666446714484579,
-2.91483908496629));
#166339=CARTESIAN_POINT('Ctrl Pts',(6.74986497879715,0.663790956137697,
-2.92168848777209));
#166340=CARTESIAN_POINT('Ctrl Pts',(6.76536122419264,0.661135169277106,
-2.9285379641169));
#166341=CARTESIAN_POINT('Ctrl Pts',(6.78086509422994,0.658505288595116,
-2.93538028861438));
#166342=CARTESIAN_POINT('Ctrl Pts',(6.79637620244565,0.655900535687991,
-2.94221570577926));
#166343=CARTESIAN_POINT('Ctrl Pts',(6.655681333,0.681369595,-2.874787991));
#166344=CARTESIAN_POINT('Ctrl Pts',(6.652255021,0.679970133000001,-2.882720556));
#166345=CARTESIAN_POINT('Ctrl Pts',(6.64880981,0.678571429,-2.890644931));
#166346=CARTESIAN_POINT('Ctrl Pts',(6.494398894,0.615882895,-3.245807475));
#166347=CARTESIAN_POINT('Ctrl Pts',(6.30303087,0.552026826,-3.582499385));
#166348=CARTESIAN_POINT('Ctrl Pts',(6.859723901,0.681369595,-2.793840961));
#166349=CARTESIAN_POINT('Ctrl Pts',(6.856394065,0.679970133000001,-2.802016714));
#166350=CARTESIAN_POINT('Ctrl Pts',(6.853044751,0.678571429,-2.810184506));
#166351=CARTESIAN_POINT('Ctrl Pts',(6.702931827,0.615882895,-3.176256762));
#166352=CARTESIAN_POINT('Ctrl Pts',(6.51467511499999,0.552026826,-3.524254171));
#166353=CARTESIAN_POINT('',(6.33858731690264,0.552026824384642,-3.57271412280189));
#166354=CARTESIAN_POINT('Ctrl Pts',(6.526254313,0.499686101,-3.275999914));
#166355=CARTESIAN_POINT('Ctrl Pts',(6.476131079,0.51775868,-3.375852472));
#166356=CARTESIAN_POINT('Ctrl Pts',(6.422976508,0.535714286,-3.474124865));
#166357=CARTESIAN_POINT('Ctrl Pts',(6.39886825300001,0.54385805,-3.518696306));
#166358=CARTESIAN_POINT('Ctrl Pts',(6.374143754,0.552026826,-3.562928878));
#166359=CARTESIAN_POINT('Ctrl Pts',(6.45608189200001,0.499686101,-3.298712871));
#166360=CARTESIAN_POINT('Ctrl Pts',(6.405611147,0.51775868,-3.397491781));
#166361=CARTESIAN_POINT('Ctrl Pts',(6.352142073,0.535714286,-3.494680397));
#166362=CARTESIAN_POINT('Ctrl Pts',(6.327891176,0.54385805,-3.538760292));
#166363=CARTESIAN_POINT('Ctrl Pts',(6.30303087,0.552026826,-3.582499385));
#166364=CARTESIAN_POINT('Ctrl Pts',(6.30303087087216,0.552026826,-3.58249938475998));
#166365=CARTESIAN_POINT('Ctrl Pts',(6.32942119521346,0.543355306040699,
-3.53606838697893));
#166366=CARTESIAN_POINT('Ctrl Pts',(6.35527595402902,0.534726110167779,
-3.48938637654263));
#166367=CARTESIAN_POINT('Ctrl Pts',(6.40600783888725,0.517399146342283,
-3.39535297685708));
#166368=CARTESIAN_POINT('Ctrl Pts',(6.43086999537852,0.508708910289016,
-3.3480245948714));
#166369=CARTESIAN_POINT('Ctrl Pts',(6.45520502561422,0.499999999749251,
-3.30042846896563));
#166370=CARTESIAN_POINT('Ctrl Pts',(6.45608189200001,0.499686101,-3.298712871));
#166371=CARTESIAN_POINT('Ctrl Pts',(6.405611147,0.51775868,-3.397491781));
#166372=CARTESIAN_POINT('Ctrl Pts',(6.352142073,0.535714286,-3.494680397));
#166373=CARTESIAN_POINT('Ctrl Pts',(6.327427568,0.544013736,-3.539602974));
#166374=CARTESIAN_POINT('Ctrl Pts',(6.30208017899999,0.552339147,-3.58417151));
#166375=CARTESIAN_POINT('Ctrl Pts',(6.475636351,0.499686101,-3.35912701));
#166376=CARTESIAN_POINT('Ctrl Pts',(6.424241261,0.51775868,-3.458205105));
#166377=CARTESIAN_POINT('Ctrl Pts',(6.369839123,0.535714286,-3.555664489));
#166378=CARTESIAN_POINT('Ctrl Pts',(6.344693336,0.544013736,-3.600712219));
#166379=CARTESIAN_POINT('Ctrl Pts',(6.318912939,0.552339147,-3.645399798));
#166380=CARTESIAN_POINT('Ctrl Pts',(6.30303086689364,0.552026827262453,
-3.58249939102387));
#166381=CARTESIAN_POINT('Ctrl Pts',(6.30759124515631,0.551172308355064,
-3.58504518515021));
#166382=CARTESIAN_POINT('Ctrl Pts',(6.31215244552515,0.550320535040699,
-3.58759041886908));
#166383=CARTESIAN_POINT('Ctrl Pts',(6.31671446167628,0.549471478150372,
-3.59013509489443));
#166384=CARTESIAN_POINT('Ctrl Pts',(6.32094966483229,0.548683245863939,
-3.59249747581913));
#166385=CARTESIAN_POINT('Ctrl Pts',(6.32518557221104,0.547897354540814,
-3.59485937672857));
#166386=CARTESIAN_POINT('Ctrl Pts',(6.32942217337293,0.547113782483501,
-3.59722080120781));
#166387=CARTESIAN_POINT('Ctrl Pts',(6.33365877881568,0.546330209634431,
-3.59958222807314));
#166388=CARTESIAN_POINT('Ctrl Pts',(6.33789607911214,0.545548955858564,
-3.60194317910222));
#166389=CARTESIAN_POINT('Ctrl Pts',(6.34213406360472,0.544769999909168,
-3.60430365896608));
#166390=CARTESIAN_POINT('Ctrl Pts',(6.303963006,0.55233793,-3.580858894));
#166391=CARTESIAN_POINT('Ctrl Pts',(6.22526953600001,0.526068113,-3.719395692));
#166392=CARTESIAN_POINT('Ctrl Pts',(6.140565969,0.49968693,-3.854341653));
#166393=CARTESIAN_POINT('Ctrl Pts',(6.365182439,0.55233793,-3.563993958));
#166394=CARTESIAN_POINT('Ctrl Pts',(6.286859595,0.526068113,-3.703876123));
#166395=CARTESIAN_POINT('Ctrl Pts',(6.202467193,0.49968693,-3.840182435));
#166396=CARTESIAN_POINT('Origin',(-0.1586294734711,0.410743067797852,0.116967770955398));
#166397=CARTESIAN_POINT('Ctrl Pts',(6.3241956596213,0.552548454735263,-3.65085335360889));
#166398=CARTESIAN_POINT('Ctrl Pts',(6.32339851881064,0.552287640367631,
-3.65223281130445));
#166399=CARTESIAN_POINT('Ctrl Pts',(6.322601378,0.552026826,-3.653612269));
#166400=CARTESIAN_POINT('Ctrl Pts',(6.242784725,0.525911829,-3.79173554));
#166401=CARTESIAN_POINT('Ctrl Pts',(6.157012229,0.49968693,-3.926241358));
#166402=CARTESIAN_POINT('Ctrl Pts',(6.30459090479817,0.552548454735263,
-3.57973734278873));
#166403=CARTESIAN_POINT('Ctrl Pts',(6.3038092818689,0.552287640367631,-3.58111252991794));
#166404=CARTESIAN_POINT('Ctrl Pts',(6.30302765893962,0.552026826,-3.58248771704715));
#166405=CARTESIAN_POINT('Ctrl Pts',(6.22476479083738,0.525911829,-3.72018338189855));
#166406=CARTESIAN_POINT('Ctrl Pts',(6.14056327055529,0.49968693,-3.85432985594832));
#166407=CARTESIAN_POINT('',(6.33215348256128,0.552026824384643,-3.68832149831073));
#166408=CARTESIAN_POINT('Ctrl Pts',(6.30691137181769,0.550751630586317,
-3.57567020898544));
#166409=CARTESIAN_POINT('Ctrl Pts',(6.3049709503943,0.551389228293159,-3.5790841773981));
#166410=CARTESIAN_POINT('Ctrl Pts',(6.30303052897091,0.552026826,-3.58249814581076));
#166411=CARTESIAN_POINT('Ctrl Pts',(6.10787159547656,0.61615356,-3.92585986423298));
#166412=CARTESIAN_POINT('Ctrl Pts',(5.87656852060082,0.681389364,-4.24598978409819));
#166413=CARTESIAN_POINT('Ctrl Pts',(6.36538619882949,0.550751630586317,
-3.78725259602702));
#166414=CARTESIAN_POINT('Ctrl Pts',(6.36333114191475,0.551389228293159,
-3.79069811251351));
#166415=CARTESIAN_POINT('Ctrl Pts',(6.361276085,0.552026826,-3.794143629));
#166416=CARTESIAN_POINT('Ctrl Pts',(6.154587625,0.61615356,-4.140678312));
#166417=CARTESIAN_POINT('Ctrl Pts',(5.911478575,0.681389364000001,-4.462709981));
#166418=CARTESIAN_POINT('Ctrl Pts',(5.87933419858893,0.680609082082812,
-4.24216096607059));
#166419=CARTESIAN_POINT('Ctrl Pts',(5.89388979747093,0.677652752742843,
-4.2528835319381));
#166420=CARTESIAN_POINT('Ctrl Pts',(5.90844992258692,0.674729896907878,
-4.26360926566706));
#166421=CARTESIAN_POINT('Ctrl Pts',(5.92302341609071,0.671836782544818,
-4.27432479842803));
#166422=CARTESIAN_POINT('Ctrl Pts',(5.93666643311042,0.669128385379447,
-4.28435617462449));
#166423=CARTESIAN_POINT('Ctrl Pts',(5.95031885609289,0.666446714488034,
-4.29438201316498));
#166424=CARTESIAN_POINT('Ctrl Pts',(5.96398022626894,0.663790956130785,
-4.30440247969411));
#166425=CARTESIAN_POINT('Ctrl Pts',(5.97764174312116,0.661135169259816,
-4.31442305380862));
#166426=CARTESIAN_POINT('Ctrl Pts',(5.99131224379848,0.658505288568692,
-4.3244382823449));
#166427=CARTESIAN_POINT('Ctrl Pts',(6.00499129856053,0.655900535637417,
-4.33444832106312));
#166428=CARTESIAN_POINT('Ctrl Pts',(5.882080762,0.681369595,-4.238351791));
#166429=CARTESIAN_POINT('Ctrl Pts',(5.87702928800001,0.679970133000001,
-4.245362341));
#166430=CARTESIAN_POINT('Ctrl Pts',(5.871961118,0.678571429,-4.25236083));
#166431=CARTESIAN_POINT('Ctrl Pts',(5.64481079600001,0.615882895,-4.566026089));
#166432=CARTESIAN_POINT('Ctrl Pts',(5.38553804100001,0.552026826,-4.853707861));
#166433=CARTESIAN_POINT('Ctrl Pts',(6.098754147,0.681369595,-4.203160378));
#166434=CARTESIAN_POINT('Ctrl Pts',(6.093744616,0.679970133000001,-4.21042917));
#166435=CARTESIAN_POINT('Ctrl Pts',(6.088717772,0.678571429,-4.217686));
#166436=CARTESIAN_POINT('Ctrl Pts',(5.863419691,0.615882895,-4.542929849));
#166437=CARTESIAN_POINT('Ctrl Pts',(5.60475516,0.552026826,-4.842321644));
#166438=CARTESIAN_POINT('',(5.42236674015786,0.552026824384643,-4.85179495805918));
#166439=CARTESIAN_POINT('Ctrl Pts',(5.66943097000001,0.499686101,-4.60236062));
#166440=CARTESIAN_POINT('Ctrl Pts',(5.599014242,0.51775868,-4.68910366600001));
#166441=CARTESIAN_POINT('Ctrl Pts',(5.525976735,0.535714286,-4.773651843));
#166442=CARTESIAN_POINT('Ctrl Pts',(5.492850576,0.54385805,-4.811998667));
#166443=CARTESIAN_POINT('Ctrl Pts',(5.459195426,0.552026826,-4.84988207));
#166444=CARTESIAN_POINT('Ctrl Pts',(5.596016527,0.499686101,-4.609457563));
#166445=CARTESIAN_POINT('Ctrl Pts',(5.52549121500001,0.51775868,-4.695077359));
#166446=CARTESIAN_POINT('Ctrl Pts',(5.452379538,0.535714286,-4.77849949));
#166447=CARTESIAN_POINT('Ctrl Pts',(5.419219739,0.54385805,-4.81633559500001));
#166448=CARTESIAN_POINT('Ctrl Pts',(5.385538041,0.552026826,-4.853707861));
#166449=CARTESIAN_POINT('Ctrl Pts',(5.38553804122079,0.552026826358493,
-4.85370786189697));
#166450=CARTESIAN_POINT('Ctrl Pts',(5.40800898309041,0.546576979810991,
-4.82877473554052));
#166451=CARTESIAN_POINT('Ctrl Pts',(5.4302902785008,0.541139220283038,-4.80370385122636));
#166452=CARTESIAN_POINT('Ctrl Pts',(5.45237953827665,0.535714285934403,
-4.77849948984032));
#166453=CARTESIAN_POINT('Ctrl Pts',(5.50061482983329,0.523868108611029,
-4.72346189596191));
#166454=CARTESIAN_POINT('Ctrl Pts',(5.54809893182974,0.511960760799632,
-4.66759983813293));
#166455=CARTESIAN_POINT('Ctrl Pts',(5.5947913592018,0.499999999550736,-4.61094454995047));
#166456=CARTESIAN_POINT('Ctrl Pts',(5.596016527,0.499686101,-4.609457563));
#166457=CARTESIAN_POINT('Ctrl Pts',(5.52549121500001,0.51775868,-4.695077359));
#166458=CARTESIAN_POINT('Ctrl Pts',(5.452379538,0.535714286,-4.77849949));
#166459=CARTESIAN_POINT('Ctrl Pts',(5.418585819,0.544013736,-4.817058913));
#166460=CARTESIAN_POINT('Ctrl Pts',(5.38425012,0.552339147,-4.855136522));
#166461=CARTESIAN_POINT('Ctrl Pts',(5.602126559,0.499686101,-4.672662884));
#166462=CARTESIAN_POINT('Ctrl Pts',(5.530634197,0.51775868,-4.758376164));
#166463=CARTESIAN_POINT('Ctrl Pts',(5.456553063,0.535714286,-4.84186215));
#166464=CARTESIAN_POINT('Ctrl Pts',(5.422311241,0.544013736,-4.880451088));
#166465=CARTESIAN_POINT('Ctrl Pts',(5.387527066,0.552339147,-4.918551872));
#166466=CARTESIAN_POINT('Ctrl Pts',(5.38553803705753,0.552026827368203,
-4.85370786651641));
#166467=CARTESIAN_POINT('Ctrl Pts',(5.38944452605589,0.551172308341726,
-4.85717448718889));
#166468=CARTESIAN_POINT('Ctrl Pts',(5.39335193808722,0.550320534996839,
-4.86064073811492));
#166469=CARTESIAN_POINT('Ctrl Pts',(5.39726026672052,0.549471478077806,
-4.86410661975057));
#166470=CARTESIAN_POINT('Ctrl Pts',(5.40088861101123,0.548683245788842,
-4.86732421300458));
#166471=CARTESIAN_POINT('Ctrl Pts',(5.40451774625319,0.547897354464642,
-4.87054148884905));
#166472=CARTESIAN_POINT('Ctrl Pts',(5.40814766147832,0.547113782407049,
-4.87375844854294));
#166473=CARTESIAN_POINT('Ctrl Pts',(5.41177758037128,0.546330209557698,
-4.8769754114874));
#166474=CARTESIAN_POINT('Ctrl Pts',(5.41540828016522,0.545548955782291,
-4.88019205909147));
#166475=CARTESIAN_POINT('Ctrl Pts',(5.41903974970139,0.54476999977346,-4.88340839344506));
#166476=CARTESIAN_POINT('Ctrl Pts',(5.386801042,0.55233793,-4.852306105));
#166477=CARTESIAN_POINT('Ctrl Pts',(5.280166064,0.526068113,-4.97068722));
#166478=CARTESIAN_POINT('Ctrl Pts',(5.168433427,0.49968693,-5.084269457));
#166479=CARTESIAN_POINT('Ctrl Pts',(5.450214661,0.55233793,-4.84899583));
#166480=CARTESIAN_POINT('Ctrl Pts',(5.343652431,0.526068113,-4.968770532));
#166481=CARTESIAN_POINT('Ctrl Pts',(5.231931248,0.49968693,-5.083748206));
#166482=CARTESIAN_POINT('Origin',(-0.129777259309849,0.410742903792786,
0.148334819574623));
#166483=CARTESIAN_POINT('Ctrl Pts',(5.39151392645153,0.552548454735263,
-4.92501355593251));
#166484=CARTESIAN_POINT('Ctrl Pts',(5.39043887972577,0.552287640367631,
-4.92618940096626));
#166485=CARTESIAN_POINT('Ctrl Pts',(5.389363833,0.552026826,-4.927365246));
#166486=CARTESIAN_POINT('Ctrl Pts',(5.281720829,0.525911829,-5.045101051));
#166487=CARTESIAN_POINT('Ctrl Pts',(5.16903887200001,0.49968693,-5.158023646));
#166488=CARTESIAN_POINT('Ctrl Pts',(5.38765536049434,0.552548454735263,
-4.85134575520336));
#166489=CARTESIAN_POINT('Ctrl Pts',(5.3865963868867,0.552287640367631,-4.8525207653942));
#166490=CARTESIAN_POINT('Ctrl Pts',(5.38553741327904,0.552026826,-4.85369577558505));
#166491=CARTESIAN_POINT('Ctrl Pts',(5.2795037892965,0.525911828999999,-4.97134798887189));
#166492=CARTESIAN_POINT('Ctrl Pts',(5.16843332766096,0.49968693,-5.08425735570182));
#166493=CARTESIAN_POINT('',(5.39123115681089,0.552026824384643,-4.96331641310191));
#166494=CARTESIAN_POINT('Ctrl Pts',(5.39079595785797,0.550751630586318,
-4.84787382396709));
#166495=CARTESIAN_POINT('Ctrl Pts',(5.38816699942899,0.551389228293159,
-4.85079084248355));
#166496=CARTESIAN_POINT('Ctrl Pts',(5.38553804100001,0.552026826,-4.853707861));
#166497=CARTESIAN_POINT('Ctrl Pts',(5.121129126,0.61615356,-5.147088575));
#166498=CARTESIAN_POINT('Ctrl Pts',(4.826415248,0.681389364,-5.41001070799999));
#166499=CARTESIAN_POINT('Ctrl Pts',(5.40241964904355,0.550751630586318,
-5.06707860853673));
#166500=CARTESIAN_POINT('Ctrl Pts',(5.39967195402178,0.551389228293159,
-5.07000179426836));
#166501=CARTESIAN_POINT('Ctrl Pts',(5.396924259,0.552026826,-5.07292498));
#166502=CARTESIAN_POINT('Ctrl Pts',(5.120573347,0.61615356,-5.366925965));
#166503=CARTESIAN_POINT('Ctrl Pts',(4.813920762,0.681389364,-5.62916745300001));
#166504=CARTESIAN_POINT('Ctrl Pts',(4.82993942163327,0.680609082082812,
-5.4068646610752));
#166505=CARTESIAN_POINT('Ctrl Pts',(4.84184968410275,0.677652752784265,
-5.42046556271524));
#166506=CARTESIAN_POINT('Ctrl Pts',(4.85376368616349,0.674729896895564,
-5.43407053107029));
#166507=CARTESIAN_POINT('Ctrl Pts',(4.86569293671695,0.671836782532443,
-5.44766841099454));
#166508=CARTESIAN_POINT('Ctrl Pts',(4.87686053821691,0.669128385374017,
-5.46039810457904));
#166509=CARTESIAN_POINT('Ctrl Pts',(4.88803851620062,0.66644671448801,-5.47312441198304));
#166510=CARTESIAN_POINT('Ctrl Pts',(4.89922638701745,0.663790956134898,
-5.48584739635545));
#166511=CARTESIAN_POINT('Ctrl Pts',(4.91041437795354,0.661135169268071,
-5.49857051732898));
#166512=CARTESIAN_POINT('Ctrl Pts',(4.92161229181551,0.65850528857982,-5.51129034896074));
#166513=CARTESIAN_POINT('Ctrl Pts',(4.93281967474729,0.655900535551958,
-5.52400695138184));
#166514=CARTESIAN_POINT('Ctrl Pts',(4.833440632,0.681369595,-5.403734972));
#166515=CARTESIAN_POINT('Ctrl Pts',(4.827000198,0.679970133000001,-5.409495702));
#166516=CARTESIAN_POINT('Ctrl Pts',(4.82054605,0.678571429,-5.415241063));
#166517=CARTESIAN_POINT('Ctrl Pts',(4.531277618,0.615882895,-5.672742398));
#166518=CARTESIAN_POINT('Ctrl Pts',(4.216223439,0.552026826,-5.897962352));
#166519=CARTESIAN_POINT('Ctrl Pts',(5.052613427,0.681369595,-5.415944688));
#166520=CARTESIAN_POINT('Ctrl Pts',(5.046158441,0.679970133000001,-5.421966639));
#166521=CARTESIAN_POINT('Ctrl Pts',(5.039689118,0.678571429,-5.427973185));
#166522=CARTESIAN_POINT('Ctrl Pts',(4.749740568,0.615882895,-5.697180586));
#166523=CARTESIAN_POINT('Ctrl Pts',(4.432763084,0.552026826,-5.933967539));
#166524=CARTESIAN_POINT('',(4.25260232110177,0.552026824384641,-5.90401125316438));
#166525=CARTESIAN_POINT('Ctrl Pts',(4.547511336,0.499686101,-5.713520057));
#166526=CARTESIAN_POINT('Ctrl Pts',(4.460093721,0.51775868,-5.783097584));
#166527=CARTESIAN_POINT('Ctrl Pts',(4.370588431,0.535714286,-5.849968167));
#166528=CARTESIAN_POINT('Ctrl Pts',(4.32999331,0.54385805,-5.880297318));
#166529=CARTESIAN_POINT('Ctrl Pts',(4.288981187,0.552026826,-5.910060166));
#166530=CARTESIAN_POINT('Ctrl Pts',(4.474287649,0.499686101,-5.704669143));
#166531=CARTESIAN_POINT('Ctrl Pts',(4.387005454,0.51775868,-5.773126338));
#166532=CARTESIAN_POINT('Ctrl Pts',(4.297669796,0.535714286,-5.838881257));
#166533=CARTESIAN_POINT('Ctrl Pts',(4.25715161,0.54385805,-5.868704398));
#166534=CARTESIAN_POINT('Ctrl Pts',(4.216223439,0.552026826,-5.897962352));
#166535=CARTESIAN_POINT('Ctrl Pts',(4.21622343978821,0.552026826,-5.89796235213106));
#166536=CARTESIAN_POINT('Ctrl Pts',(4.25967050727171,0.543355308490836,
-5.86690373837236));
#166537=CARTESIAN_POINT('Ctrl Pts',(4.30273690686368,0.534726114959304,
-5.83539243414648));
#166538=CARTESIAN_POINT('Ctrl Pts',(4.38826616643414,0.517398614624112,
-5.77134981348705));
#166539=CARTESIAN_POINT('Ctrl Pts',(4.43069788664702,0.50870945045658,-5.73883909642985));
#166540=CARTESIAN_POINT('Ctrl Pts',(4.47277146633137,0.499999999626732,
-5.70585799044219));
#166541=CARTESIAN_POINT('Ctrl Pts',(4.474287649,0.499686101,-5.704669143));
#166542=CARTESIAN_POINT('Ctrl Pts',(4.387005454,0.51775868,-5.773126338));
#166543=CARTESIAN_POINT('Ctrl Pts',(4.297669796,0.535714286,-5.838881257));
#166544=CARTESIAN_POINT('Ctrl Pts',(4.256377018,0.544013736,-5.869274531));
#166545=CARTESIAN_POINT('Ctrl Pts',(4.214658508,0.552339147,-5.899080747));
#166546=CARTESIAN_POINT('Ctrl Pts',(4.466667556,0.499686101,-5.767710235));
#166547=CARTESIAN_POINT('Ctrl Pts',(4.378420824,0.51775868,-5.836050841));
#166548=CARTESIAN_POINT('Ctrl Pts',(4.288124647,0.535714286,-5.901659717));
#166549=CARTESIAN_POINT('Ctrl Pts',(4.246387899,0.544013736,-5.931985488));
#166550=CARTESIAN_POINT('Ctrl Pts',(4.204226416,0.552339147,-5.961717928));
#166551=CARTESIAN_POINT('Ctrl Pts',(4.21622343369513,0.552026827225121,
-5.8979623562474));
#166552=CARTESIAN_POINT('Ctrl Pts',(4.21929336986428,0.551172308280893,
-5.90218770933082));
#166553=CARTESIAN_POINT('Ctrl Pts',(4.2223642873589,0.550320534952158,-5.90641289924824));
#166554=CARTESIAN_POINT('Ctrl Pts',(4.22543617940756,0.549471478050236,
-5.91063792555498));
#166555=CARTESIAN_POINT('Ctrl Pts',(4.22828800767696,0.548683245769649,
-5.91456028000939));
#166556=CARTESIAN_POINT('Ctrl Pts',(4.23114067663525,0.547897354454663,
-5.91848249450931));
#166557=CARTESIAN_POINT('Ctrl Pts',(4.23399417529381,0.547113782405765,
-5.92240456793084));
#166558=CARTESIAN_POINT('Ctrl Pts',(4.23684767683566,0.546330209565113,
-5.92632664531538));
#166559=CARTESIAN_POINT('Ctrl Pts',(4.23970200880008,0.545548955798003,
-5.93024858261012));
#166560=CARTESIAN_POINT('Ctrl Pts',(4.24255715914079,0.544769999937507,
-5.93417037982135));
#166561=CARTESIAN_POINT('Ctrl Pts',(4.217758247,0.55233793,-5.89686487600001));
#166562=CARTESIAN_POINT('Ctrl Pts',(4.088167896,0.526068113,-5.989554938));
#166563=CARTESIAN_POINT('Ctrl Pts',(3.954630682,0.49968693,-6.076462471));
#166564=CARTESIAN_POINT('Ctrl Pts',(4.280400903,0.55233793,-5.907264047));
#166565=CARTESIAN_POINT('Ctrl Pts',(4.150582018,0.526068113,-6.001330754));
#166566=CARTESIAN_POINT('Ctrl Pts',(4.016756013,0.49968693,-6.089603562));
#166567=CARTESIAN_POINT('Origin',(-0.0948546780510573,0.410743245677191,
0.172763753115606));
#166568=CARTESIAN_POINT('Ctrl Pts',(4.20673099430623,0.552548454735263,
-5.9688855986822));
#166569=CARTESIAN_POINT('Ctrl Pts',(4.20542830965312,0.552287640367631,
-5.9698028498411));
#166570=CARTESIAN_POINT('Ctrl Pts',(4.204125625,0.552026826,-5.970720101));
#166571=CARTESIAN_POINT('Ctrl Pts',(4.073689537,0.525911829,-6.062563244));
#166572=CARTESIAN_POINT('Ctrl Pts',(3.939367001,0.49968693,-6.148622482));
#166573=CARTESIAN_POINT('Ctrl Pts',(4.21879903966101,0.552548454735263,
-5.89611063196322));
#166574=CARTESIAN_POINT('Ctrl Pts',(4.21751223181639,0.552287640367631,
-5.89703052304883));
#166575=CARTESIAN_POINT('Ctrl Pts',(4.21622542397176,0.552026826,-5.89795041413444));
#166576=CARTESIAN_POINT('Ctrl Pts',(4.08737905976591,0.525911829,-5.99005788949816));
#166577=CARTESIAN_POINT('Ctrl Pts',(3.95463318641739,0.49968693,-6.07645063120944));
#166578=CARTESIAN_POINT('',(4.198220854242,0.552026824384649,-6.00623216873903));
#166579=CARTESIAN_POINT('Ctrl Pts',(4.22261278365116,0.550751630586318,
-5.89339374004824));
#166580=CARTESIAN_POINT('Ctrl Pts',(4.21941821673891,0.551389228293159,
-5.89567741205534));
#166581=CARTESIAN_POINT('Ctrl Pts',(4.21622364982665,0.552026826,-5.89796108406243));
#166582=CARTESIAN_POINT('Ctrl Pts',(3.89492835589839,0.61615356,-6.12764263054736));
#166583=CARTESIAN_POINT('Ctrl Pts',(3.55058430531378,0.681389364000001,
-6.3210630364675));
#166584=CARTESIAN_POINT('Ctrl Pts',(4.18684196093688,0.550751630586318,
-6.10997365687232));
#166585=CARTESIAN_POINT('Ctrl Pts',(4.18353010696844,0.551389228293159,
-6.11223782693617));
#166586=CARTESIAN_POINT('Ctrl Pts',(4.180218253,0.552026826,-6.114501997));
#166587=CARTESIAN_POINT('Ctrl Pts',(3.84712675,0.61615356,-6.342222125));
#166588=CARTESIAN_POINT('Ctrl Pts',(3.491269364,0.681389364000001,-6.532411311));
#166589=CARTESIAN_POINT('Ctrl Pts',(3.55470204599018,0.680609082082816,
-6.31874937382084));
#166590=CARTESIAN_POINT('Ctrl Pts',(3.5634100609705,0.677652752713562,-6.33459264818729));
#166591=CARTESIAN_POINT('Ctrl Pts',(3.5721208539121,0.674729896887179,-6.35044069837409));
#166592=CARTESIAN_POINT('Ctrl Pts',(3.5808480629607,0.671836782527383,-6.36628510364611));
#166593=CARTESIAN_POINT('Ctrl Pts',(3.58901806429499,0.669128385369925,
-6.38111788827318));
#166594=CARTESIAN_POINT('Ctrl Pts',(3.59719892743867,0.666446714485906,
-6.3959495965279));
#166595=CARTESIAN_POINT('Ctrl Pts',(3.60539016647564,0.663790956135505,
-6.41078018611097));
#166596=CARTESIAN_POINT('Ctrl Pts',(3.61358149345834,0.661135169271393,
-6.42561093492357));
#166597=CARTESIAN_POINT('Ctrl Pts',(3.62178321848122,0.658505288586583,
-6.44044060443574));
#166598=CARTESIAN_POINT('Ctrl Pts',(3.62999488593847,0.655900535633648,
-6.45526915564017));
#166599=CARTESIAN_POINT('Ctrl Pts',(3.558794191,0.681369595,-6.316445512));
#166600=CARTESIAN_POINT('Ctrl Pts',(3.551265944,0.679970133000001,-6.320687056));
#166601=CARTESIAN_POINT('Ctrl Pts',(3.543727607,0.678571429,-6.324910643));
#166602=CARTESIAN_POINT('Ctrl Pts',(3.205866935,0.615882895,-6.514207577));
#166603=CARTESIAN_POINT('Ctrl Pts',(2.849762915,0.552026826,-6.666434679));
#166604=CARTESIAN_POINT('Ctrl Pts',(3.770218119,0.681369595,-6.375485444));
#166605=CARTESIAN_POINT('Ctrl Pts',(3.762619505,0.679970133000001,-6.379978973));
#166606=CARTESIAN_POINT('Ctrl Pts',(3.755010202,0.678571429,-6.384454377));
#166607=CARTESIAN_POINT('Ctrl Pts',(3.413968854,0.615882895,-6.585037491));
#166608=CARTESIAN_POINT('Ctrl Pts',(3.053499932,0.552026826,-6.74814770699999));
#166609=CARTESIAN_POINT('',(2.88399094416683,0.552026824384642,-6.68016254454245));
#166610=CARTESIAN_POINT('Ctrl Pts',(3.212955126,0.499686101,-6.557521647));
#166611=CARTESIAN_POINT('Ctrl Pts',(3.112624175,0.51775868,-6.606680287));
#166612=CARTESIAN_POINT('Ctrl Pts',(3.01083627,0.535714286,-6.652746481));
#166613=CARTESIAN_POINT('Ctrl Pts',(2.964670369,0.54385805,-6.673639803));
#166614=CARTESIAN_POINT('Ctrl Pts',(2.918218955,0.552026826,-6.693890418));
#166615=CARTESIAN_POINT('Ctrl Pts',(3.143346053,0.499686101,-6.533136734));
#166616=CARTESIAN_POINT('Ctrl Pts',(3.043388194,0.51775868,-6.581230346));
#166617=CARTESIAN_POINT('Ctrl Pts',(2.94200579,0.535714286,-6.626243425));
#166618=CARTESIAN_POINT('Ctrl Pts',(2.896023804,0.54385805,-6.646659106));
#166619=CARTESIAN_POINT('Ctrl Pts',(2.849762915,0.552026826,-6.666434679));
#166620=CARTESIAN_POINT('Ctrl Pts',(2.84976291891813,0.552026825495856,
-6.6664346782059));
#166621=CARTESIAN_POINT('Ctrl Pts',(2.89887089484146,0.543355309227961,
-6.64544203478179));
#166622=CARTESIAN_POINT('Ctrl Pts',(2.94770444479558,0.534726112122594,
-6.62392544096408));
#166623=CARTESIAN_POINT('Ctrl Pts',(3.04500134496897,0.517398612370645,
-6.57976636581241));
#166624=CARTESIAN_POINT('Ctrl Pts',(3.09342989164506,0.508709445676462,
-6.55713728981927));
#166625=CARTESIAN_POINT('Ctrl Pts',(3.14160975114555,0.499999999561346,
-6.53397185222096));
#166626=CARTESIAN_POINT('Ctrl Pts',(3.143346053,0.499686101,-6.533136734));
#166627=CARTESIAN_POINT('Ctrl Pts',(3.043388194,0.51775868,-6.581230346));
#166628=CARTESIAN_POINT('Ctrl Pts',(2.94200579,0.535714286,-6.626243425));
#166629=CARTESIAN_POINT('Ctrl Pts',(2.895144759,0.544013736,-6.647049396));
#166630=CARTESIAN_POINT('Ctrl Pts',(2.84799415,0.552339147,-6.667190512));
#166631=CARTESIAN_POINT('Ctrl Pts',(3.122352143,0.499686101,-6.593065866));
#166632=CARTESIAN_POINT('Ctrl Pts',(3.02147736,0.51775868,-6.640838268));
#166633=CARTESIAN_POINT('Ctrl Pts',(2.919188289,0.535714286,-6.685502236));
#166634=CARTESIAN_POINT('Ctrl Pts',(2.871908178,0.544013736,-6.70614684));
#166635=CARTESIAN_POINT('Ctrl Pts',(2.824340811,0.552339147,-6.72612067900001));
#166636=CARTESIAN_POINT('Ctrl Pts',(2.84976290889703,0.55202682733598,-6.66643468166387));
#166637=CARTESIAN_POINT('Ctrl Pts',(2.85185274604644,0.551172308275351,
-6.67122119378965));
#166638=CARTESIAN_POINT('Ctrl Pts',(2.85394357611775,0.550320534936221,
-6.67600775770568));
#166639=CARTESIAN_POINT('Ctrl Pts',(2.85603539316663,0.549471478025613,
-6.68079437132065));
#166640=CARTESIAN_POINT('Ctrl Pts',(2.85797735687409,0.54868324575317,-6.68523808207772));
#166641=CARTESIAN_POINT('Ctrl Pts',(2.85992017173335,0.547897354447752,
-6.68968183686207));
#166642=CARTESIAN_POINT('Ctrl Pts',(2.86186382725496,0.547113782410433,
-6.6941256322136));
#166643=CARTESIAN_POINT('Ctrl Pts',(2.86380748474054,0.546330209581352,
-6.69856943205538));
#166644=CARTESIAN_POINT('Ctrl Pts',(2.86575198338132,0.545548955827773,
-6.70301327358507));
#166645=CARTESIAN_POINT('Ctrl Pts',(2.86769731172646,0.544769999923278,
-6.70745715414584));
#166646=CARTESIAN_POINT('Ctrl Pts',(2.851497765,0.55233793,-6.665692799));
#166647=CARTESIAN_POINT('Ctrl Pts',(2.705011541,0.526068113,-6.728357725));
#166648=CARTESIAN_POINT('Ctrl Pts',(2.555913802,0.49968693,-6.784526854));
#166649=CARTESIAN_POINT('Ctrl Pts',(2.910440355,0.55233793,-6.689315163));
#166650=CARTESIAN_POINT('Ctrl Pts',(2.763435003,0.526068113,-6.753275419));
#166651=CARTESIAN_POINT('Ctrl Pts',(2.613761731,0.49968693,-6.810715823));
#166652=CARTESIAN_POINT('Origin',(-0.0554976071978636,0.410743109954222,
0.189114824533242));
#166653=CARTESIAN_POINT('Ctrl Pts',(2.82524599699793,0.552548454735263,
-6.73365918371557));
#166654=CARTESIAN_POINT('Ctrl Pts',(2.82377658649897,0.552287640367631,
-6.73427495135779));
#166655=CARTESIAN_POINT('Ctrl Pts',(2.822307176,0.552026826,-6.734890719));
#166656=CARTESIAN_POINT('Ctrl Pts',(2.67517705,0.525911829,-6.796546717));
#166657=CARTESIAN_POINT('Ctrl Pts',(2.525494709,0.49968693,-6.851718563));
#166658=CARTESIAN_POINT('Ctrl Pts',(2.85267636463054,0.552548454735263,
-6.66517992915994));
#166659=CARTESIAN_POINT('Ctrl Pts',(2.85122189224375,0.552287640367631,
-6.66580168804706));
#166660=CARTESIAN_POINT('Ctrl Pts',(2.84976741985695,0.552026826,-6.66642344693418));
#166661=CARTESIAN_POINT('Ctrl Pts',(2.70413302723223,0.525911829,-6.72867934034711));
#166662=CARTESIAN_POINT('Ctrl Pts',(2.55591879307536,0.49968693,-6.7845158293819));
#166663=CARTESIAN_POINT('',(2.80890641028778,0.552026824384643,-6.76830318364549));
#166664=CARTESIAN_POINT('Ctrl Pts',(2.85698451967886,0.550751630586318,
-6.66334759239431));
#166665=CARTESIAN_POINT('Ctrl Pts',(2.85337371733943,0.551389228293159,
-6.66489113569716));
#166666=CARTESIAN_POINT('Ctrl Pts',(2.849762915,0.552026826,-6.666434679));
#166667=CARTESIAN_POINT('Ctrl Pts',(2.486604518,0.61615356,-6.821677381));
#166668=CARTESIAN_POINT('Ctrl Pts',(2.108731308,0.681389364000001,-6.93655190100001));
#166669=CARTESIAN_POINT('Ctrl Pts',(2.77549219559838,0.550751630586318,
-6.86717312735757));
#166670=CARTESIAN_POINT('Ctrl Pts',(2.77177104129919,0.551389228293159,
-6.86867241167878));
#166671=CARTESIAN_POINT('Ctrl Pts',(2.768049887,0.552026826,-6.87017169600001));
#166672=CARTESIAN_POINT('Ctrl Pts',(2.393792782,0.61615356,-7.020963027));
#166673=CARTESIAN_POINT('Ctrl Pts',(2.005370091,0.681389364000001,-7.130206877));
#166674=CARTESIAN_POINT('Ctrl Pts',(2.11325075290579,0.680609082082812,
-6.93517638941795));
#166675=CARTESIAN_POINT('Ctrl Pts',(2.11834934301391,0.6776527527642,-6.95252122234189));
#166676=CARTESIAN_POINT('Ctrl Pts',(2.12344962078689,0.674729896829384,
-6.96987131670069));
#166677=CARTESIAN_POINT('Ctrl Pts',(2.12856671375807,0.671836782472668,
-6.98722138055105));
#166678=CARTESIAN_POINT('Ctrl Pts',(2.13335709474363,0.669128385325786,
-7.00346369165135));
#166679=CARTESIAN_POINT('Ctrl Pts',(2.13815831498433,0.666446714451452,
-7.01970728651192));
#166680=CARTESIAN_POINT('Ctrl Pts',(2.14296990901684,0.663790956109898,
-7.03595201936503));
#166681=CARTESIAN_POINT('Ctrl Pts',(2.14778155470932,0.661135169254634,
-7.05219692663069));
#166682=CARTESIAN_POINT('Ctrl Pts',(2.15260358735908,0.658505288577833,
-7.06844301510056));
#166683=CARTESIAN_POINT('Ctrl Pts',(2.15743557081923,0.655900535694669,
-7.08469014864916));
#166684=CARTESIAN_POINT('Ctrl Pts',(2.117742488,0.681369595,-6.93380608));
#166685=CARTESIAN_POINT('Ctrl Pts',(2.10947844,0.679970133000001,-6.936330109));
#166686=CARTESIAN_POINT('Ctrl Pts',(2.1012084,0.678571429,-6.938834431));
#166687=CARTESIAN_POINT('Ctrl Pts',(1.730553477,0.615882895,-7.05107565));
#166688=CARTESIAN_POINT('Ctrl Pts',(1.350050644,0.552026826,-7.123191929));
#166689=CARTESIAN_POINT('Ctrl Pts',(2.311531602,0.681369595,-7.036915586));
#166690=CARTESIAN_POINT('Ctrl Pts',(2.303144664,0.679970133000001,-7.039670582));
#166691=CARTESIAN_POINT('Ctrl Pts',(2.294751182,0.678571429,-7.042405578));
#166692=CARTESIAN_POINT('Ctrl Pts',(1.918563751,0.615882895,-7.164985361));
#166693=CARTESIAN_POINT('Ctrl Pts',(1.531458517,0.552026826,-7.24679198800001));
#166694=CARTESIAN_POINT('',(1.38052735580328,0.552026824384641,-7.14395685910557));
#166695=CARTESIAN_POINT('Ctrl Pts',(1.728164706,0.499686101,-7.094900813));
#166696=CARTESIAN_POINT('Ctrl Pts',(1.619611782,0.51775868,-7.121341962));
#166697=CARTESIAN_POINT('Ctrl Pts',(1.510300752,0.535714286,-7.144449764));
#166698=CARTESIAN_POINT('Ctrl Pts',(1.460722737,0.54385805,-7.154930307));
#166699=CARTESIAN_POINT('Ctrl Pts',(1.411004048,0.552026826,-7.164721793));
#166700=CARTESIAN_POINT('Ctrl Pts',(1.665425089,0.499686101,-7.056122113));
#166701=CARTESIAN_POINT('Ctrl Pts',(1.557465485,0.51775868,-7.081603338));
#166702=CARTESIAN_POINT('Ctrl Pts',(1.448776863,0.535714286,-7.103769816));
#166703=CARTESIAN_POINT('Ctrl Pts',(1.399481142,0.54385805,-7.11382342199999));
#166704=CARTESIAN_POINT('Ctrl Pts',(1.350050644,0.552026826,-7.12319192899999));
#166705=CARTESIAN_POINT('Ctrl Pts',(1.35005064358211,0.55202682632986,-7.12319192927199));
#166706=CARTESIAN_POINT('Ctrl Pts',(1.38302848960185,0.546576979806139,
-7.11694167477289));
#166707=CARTESIAN_POINT('Ctrl Pts',(1.41593872707709,0.541139220287456,
-7.11046698299128));
#166708=CARTESIAN_POINT('Ctrl Pts',(1.44877686332883,0.53571428591939,-7.10376981614113));
#166709=CARTESIAN_POINT('Ctrl Pts',(1.52048397699588,0.523868108620023,
-7.08914552447919));
#166710=CARTESIAN_POINT('Ctrl Pts',(1.59209201781199,0.511960760913898,
-7.07341028179112));
#166711=CARTESIAN_POINT('Ctrl Pts',(1.66354985423408,0.499999999722903,
-7.05656445327241));
#166712=CARTESIAN_POINT('Ctrl Pts',(1.665425089,0.499686101,-7.056122113));
#166713=CARTESIAN_POINT('Ctrl Pts',(1.557465485,0.51775868,-7.081603338));
#166714=CARTESIAN_POINT('Ctrl Pts',(1.448776863,0.535714286,-7.103769816));
#166715=CARTESIAN_POINT('Ctrl Pts',(1.398538749,0.544013736,-7.114015618));
#166716=CARTESIAN_POINT('Ctrl Pts',(1.34816075,0.552339147,-7.12354985899999));
#166717=CARTESIAN_POINT('Ctrl Pts',(1.632039014,0.499686101,-7.110137064));
#166718=CARTESIAN_POINT('Ctrl Pts',(1.523252973,0.51775868,-7.13510747800001));
#166719=CARTESIAN_POINT('Ctrl Pts',(1.41375393,0.535714286,-7.1567381));
#166720=CARTESIAN_POINT('Ctrl Pts',(1.363141222,0.544013736,-7.166736219));
#166721=CARTESIAN_POINT('Ctrl Pts',(1.312392169,0.552339147,-7.176017503));
#166722=CARTESIAN_POINT('Ctrl Pts',(1.35005063742863,0.552026827346769,
-7.12319193043825));
#166723=CARTESIAN_POINT('Ctrl Pts',(1.35106265669364,0.551172308311127,
-7.12831578970783));
#166724=CARTESIAN_POINT('Ctrl Pts',(1.35207563461735,0.550320534970049,
-7.13343991304482));
#166725=CARTESIAN_POINT('Ctrl Pts',(1.35308956573833,0.549471478056719,
-7.13856429709401));
#166726=CARTESIAN_POINT('Ctrl Pts',(1.354030860992,0.548683245773404,-7.14332158117741));
#166727=CARTESIAN_POINT('Ctrl Pts',(1.35497297801486,0.547897354456482,
-7.1480790912348));
#166728=CARTESIAN_POINT('Ctrl Pts',(1.35591590731123,0.547113782407415,
-7.1528368216312));
#166729=CARTESIAN_POINT('Ctrl Pts',(1.35685883756039,0.546330209566589,
-7.15759455683505));
#166730=CARTESIAN_POINT('Ctrl Pts',(1.35780258032342,0.545548955800985,
-7.16235251357834));
#166731=CARTESIAN_POINT('Ctrl Pts',(1.35874712535521,0.544769999826398,
-7.16711068672649));
#166732=CARTESIAN_POINT('Ctrl Pts',(1.351904417,0.55233793,-7.122840336));
#166733=CARTESIAN_POINT('Ctrl Pts',(1.195371852,0.526068113,-7.152549982));
#166734=CARTESIAN_POINT('Ctrl Pts',(1.037685233,0.49968693,-7.175354302));
#166735=CARTESIAN_POINT('Ctrl Pts',(1.404390852,0.55233793,-7.158581336));
#166736=CARTESIAN_POINT('Ctrl Pts',(1.247072838,0.526068113,-7.189444432));
#166737=CARTESIAN_POINT('Ctrl Pts',(1.088550856,0.49968693,-7.213366582));
#166738=CARTESIAN_POINT('Origin',(-0.0135462466738689,0.410742949663908,
0.196625407235529));
#166739=CARTESIAN_POINT('Ctrl Pts',(1.31165563666942,0.552548454735263,
-7.18357434997127));
#166740=CARTESIAN_POINT('Ctrl Pts',(1.31008820833471,0.552287640367631,
-7.18385984148563));
#166741=CARTESIAN_POINT('Ctrl Pts',(1.30852078,0.552026826,-7.184145333));
#166742=CARTESIAN_POINT('Ctrl Pts',(1.151576258,0.525911829,-7.21273122));
#166743=CARTESIAN_POINT('Ctrl Pts',(0.99353309,0.49968693,-7.2344359));
#166744=CARTESIAN_POINT('Ctrl Pts',(1.35316571288421,0.552548454735263,
-7.12259282012464));
#166745=CARTESIAN_POINT('Ctrl Pts',(1.35161158546938,0.552287640367631,
-7.12288737406653));
#166746=CARTESIAN_POINT('Ctrl Pts',(1.35005745805455,0.552026826,-7.12318192800843));
#166747=CARTESIAN_POINT('Ctrl Pts',(1.19444473953571,0.525911829,-7.15267522386804));
#166748=CARTESIAN_POINT('Ctrl Pts',(1.03769247730763,0.49968693,-7.1753446081269));
#166749=CARTESIAN_POINT('',(1.28825062439923,0.552026824384644,-7.21389586373221));
#166750=CARTESIAN_POINT('Ctrl Pts',(1.35776776537411,0.550751630586317,
-7.12172838697859));
#166751=CARTESIAN_POINT('Ctrl Pts',(1.3539095659827,0.551389228293159,-7.12245962771548));
#166752=CARTESIAN_POINT('Ctrl Pts',(1.35005136659128,0.552026826,-7.12319086845238));
#166753=CARTESIAN_POINT('Ctrl Pts',(0.962010877365314,0.61615356,-7.19673580081601));
#166754=CARTESIAN_POINT('Ctrl Pts',(0.568277560521424,0.681389364000001,
-7.22769309322264));
#166755=CARTESIAN_POINT('Ctrl Pts',(1.23436350016688,0.550751630586317,
-7.30327121457896));
#166756=CARTESIAN_POINT('Ctrl Pts',(1.23040704258344,0.551389228293159,
-7.30393550828948));
#166757=CARTESIAN_POINT('Ctrl Pts',(1.226450585,0.552026826,-7.304599802));
#166758=CARTESIAN_POINT('Ctrl Pts',(0.828527725,0.61615356,-7.371411501));
#166759=CARTESIAN_POINT('Ctrl Pts',(0.425701942,0.681389364000001,-7.394601894));
#166760=CARTESIAN_POINT('Ctrl Pts',(0.572986203939546,0.680609082082812,
-7.22732226364026));
#166761=CARTESIAN_POINT('Ctrl Pts',(0.574236965657701,0.677652752658241,
-7.24535763046556));
#166762=CARTESIAN_POINT('Ctrl Pts',(0.575488243539233,0.674729896865504,
-7.2633984982882));
#166763=CARTESIAN_POINT('Ctrl Pts',(0.57675595093358,0.671836782506211,
-7.28144295100099));
#166764=CARTESIAN_POINT('Ctrl Pts',(0.577942718780051,0.669128385353143,
-7.29833531621256));
#166765=CARTESIAN_POINT('Ctrl Pts',(0.579139796495504,0.666446714472475,
-7.31523126529016));
#166766=CARTESIAN_POINT('Ctrl Pts',(0.580346760832762,0.663790956124645,
-7.33213055581337));
#166767=CARTESIAN_POINT('Ctrl Pts',(0.581553738128665,0.661135169263106,
-7.34903002777682));
#166768=CARTESIAN_POINT('Ctrl Pts',(0.582770605614792,0.658505288580088,
-7.36593288621745));
#166769=CARTESIAN_POINT('Ctrl Pts',(0.583996965696794,0.655900535579078,
-7.3828389043069));
#166770=CARTESIAN_POINT('Ctrl Pts',(0.5776675,0.681369595,-7.226949582));
#166771=CARTESIAN_POINT('Ctrl Pts',(0.56905407,0.679970133000001,-7.22763807400001));
#166772=CARTESIAN_POINT('Ctrl Pts',(0.560439023,0.678571429,-7.228306033));
#166773=CARTESIAN_POINT('Ctrl Pts',(0.174321262,0.615882895,-7.25824326300001));
#166774=CARTESIAN_POINT('Ctrl Pts',(-0.212788494,0.552026826,-7.246876641));
#166775=CARTESIAN_POINT('Ctrl Pts',(0.744760437,0.681369595,-7.36930737600001));
#166776=CARTESIAN_POINT('Ctrl Pts',(0.735977338,0.679970133000001,-7.37019501800001));
#166777=CARTESIAN_POINT('Ctrl Pts',(0.727192148,0.678571429,-7.371061721));
#166778=CARTESIAN_POINT('Ctrl Pts',(0.33344874,0.615882895,-7.409906479));
#166779=CARTESIAN_POINT('Ctrl Pts',(-0.062192196,0.552026826,-7.40658433));
#166780=CARTESIAN_POINT('',(-0.187488157518674,0.552026824384641,-7.27370769075728));
#166781=CARTESIAN_POINT('Ctrl Pts',(0.162567224,0.499686101,-7.300530302));
#166782=CARTESIAN_POINT('Ctrl Pts',(0.050868142,0.51775868,-7.30301760200001));
#166783=CARTESIAN_POINT('Ctrl Pts',(-0.060854751,0.535714286,-7.302086516));
#166784=CARTESIAN_POINT('Ctrl Pts',(-0.111526666,0.54385805,-7.301664223));
#166785=CARTESIAN_POINT('Ctrl Pts',(-0.162187841,0.552026826,-7.30053874));
#166786=CARTESIAN_POINT('Ctrl Pts',(0.1096307,0.499686101,-7.249171064));
#166787=CARTESIAN_POINT('Ctrl Pts',(-0.00128258,0.51775868,-7.250848428));
#166788=CARTESIAN_POINT('Ctrl Pts',(-0.112195259,0.535714286,-7.249131826));
#166789=CARTESIAN_POINT('Ctrl Pts',(-0.162499702,0.54385805,-7.248353261));
#166790=CARTESIAN_POINT('Ctrl Pts',(-0.212788494,0.552026826,-7.246876641));
#166791=CARTESIAN_POINT('Ctrl Pts',(-0.212788494593637,0.552026826142908,
-7.24687664176387));
#166792=CARTESIAN_POINT('Ctrl Pts',(-0.179238032192001,0.546576979665154,
-7.24786177688672));
#166793=CARTESIAN_POINT('Ctrl Pts',(-0.145705350411296,0.541139220209299,
-7.24861318818257));
#166794=CARTESIAN_POINT('Ctrl Pts',(-0.112195259273809,0.535714286044326,
-7.24913182599576));
#166795=CARTESIAN_POINT('Ctrl Pts',(-0.0390208298560378,0.523868109072172,
-7.2502643509093));
#166796=CARTESIAN_POINT('Ctrl Pts',(0.0342956684092109,0.511960761022386,
-7.25029060206938));
#166797=CARTESIAN_POINT('Ctrl Pts',(0.107704216070513,0.499999999886365,
-7.24919994256545));
#166798=CARTESIAN_POINT('Ctrl Pts',(0.1096307,0.499686101,-7.249171064));
#166799=CARTESIAN_POINT('Ctrl Pts',(-0.00128258,0.51775868,-7.250848428));
#166800=CARTESIAN_POINT('Ctrl Pts',(-0.112195259,0.535714286,-7.249131826));
#166801=CARTESIAN_POINT('Ctrl Pts',(-0.163461379,0.544013736,-7.248338377));
#166802=CARTESIAN_POINT('Ctrl Pts',(-0.214711149,0.552339147,-7.24681993199999));
#166803=CARTESIAN_POINT('Ctrl Pts',(0.0654135539999999,0.499686101,-7.29474615600001));
#166804=CARTESIAN_POINT('Ctrl Pts',(-0.0461970310000001,0.51775868,-7.29574699200001));
#166805=CARTESIAN_POINT('Ctrl Pts',(-0.157785991,0.535714286,-7.293332845));
#166806=CARTESIAN_POINT('Ctrl Pts',(-0.209364702,0.544013736,-7.292216977));
#166807=CARTESIAN_POINT('Ctrl Pts',(-0.260922472,0.552339147,-7.290371724));
#166808=CARTESIAN_POINT('Ctrl Pts',(-0.212788500831279,0.552026827156134,
-7.24687664158071));
#166809=CARTESIAN_POINT('Ctrl Pts',(-0.212901620729526,0.55117230828004,
-7.25209826172077));
#166810=CARTESIAN_POINT('Ctrl Pts',(-0.213013860674674,0.550320534954775,
-7.25732034620402));
#166811=CARTESIAN_POINT('Ctrl Pts',(-0.213125225767415,0.549471478053454,
-7.26254289021273));
#166812=CARTESIAN_POINT('Ctrl Pts',(-0.213228612902325,0.548683245778484,
-7.26739130230232));
#166813=CARTESIAN_POINT('Ctrl Pts',(-0.213331246070747,0.547897354466547,
-7.27224011173801));
#166814=CARTESIAN_POINT('Ctrl Pts',(-0.213433133333021,0.547113782419621,
-7.27708931097543));
#166815=CARTESIAN_POINT('Ctrl Pts',(-0.213535020698245,0.54633020958094,
-7.2819385151127));
#166816=CARTESIAN_POINT('Ctrl Pts',(-0.21363616218058,0.545548955814703,
-7.28678811027582));
#166817=CARTESIAN_POINT('Ctrl Pts',(-0.213736567463141,0.544769999955344,
-7.29163808927306));
#166818=CARTESIAN_POINT('Ctrl Pts',(-0.21090248,0.55233793,-7.246931774));
#166819=CARTESIAN_POINT('Ctrl Pts',(-0.370162096,0.526068113,-7.24229695100001));
#166820=CARTESIAN_POINT('Ctrl Pts',(-0.529064344,0.49968693,-7.230670157));
#166821=CARTESIAN_POINT('Ctrl Pts',(-0.167326407,0.55233793,-7.293120202));
#166822=CARTESIAN_POINT('Ctrl Pts',(-0.327601066,0.526068113,-7.289443013));
#166823=CARTESIAN_POINT('Ctrl Pts',(-0.487559448,0.49968693,-7.278728336));
#166824=CARTESIAN_POINT('Origin',(0.029039077562356,0.410742974322117,0.194940242366671));
#166825=CARTESIAN_POINT('Ctrl Pts',(-0.263266283044498,0.552548454735263,
-7.2975935627527));
#166826=CARTESIAN_POINT('Ctrl Pts',(-0.264858438022249,0.552287640367631,
-7.29753542887635));
#166827=CARTESIAN_POINT('Ctrl Pts',(-0.266450593,0.552026826,-7.297477295));
#166828=CARTESIAN_POINT('Ctrl Pts',(-0.425870961,0.525911829,-7.291656427));
#166829=CARTESIAN_POINT('Ctrl Pts',(-0.584885032,0.49968693,-7.278879055));
#166830=CARTESIAN_POINT('Ctrl Pts',(-0.209617462986227,0.552548454735263,
-7.2469611866814));
#166831=CARTESIAN_POINT('Ctrl Pts',(-0.21119857615827,0.552287640367631,
-7.24691476266089));
#166832=CARTESIAN_POINT('Ctrl Pts',(-0.212779689330313,0.552026826,-7.24686833864037));
#166833=CARTESIAN_POINT('Ctrl Pts',(-0.371094455957274,0.525911829,-7.24221996298682));
#166834=CARTESIAN_POINT('Ctrl Pts',(-0.529055185157377,0.49968693,-7.23066224707044));
#166835=CARTESIAN_POINT('',(-0.292642328452178,0.552026824384643,-7.32217479090157));
#166836=CARTESIAN_POINT('Ctrl Pts',(-0.204938109066285,0.550751630586317,
-7.24710715016635));
#166837=CARTESIAN_POINT('Ctrl Pts',(-0.208863301533143,0.551389228293159,
-7.24699189558317));
#166838=CARTESIAN_POINT('Ctrl Pts',(-0.212788494,0.552026826,-7.246876641));
#166839=CARTESIAN_POINT('Ctrl Pts',(-0.607566848,0.61615356,-7.23528484900001));
#166840=CARTESIAN_POINT('Ctrl Pts',(-0.998749843,0.681389364000001,-7.180877297));
#166841=CARTESIAN_POINT('Ctrl Pts',(-0.364482660369832,0.550751630586317,
-7.39787645705584));
#166842=CARTESIAN_POINT('Ctrl Pts',(-0.368489421684916,0.551389228293159,
-7.39767469852792));
#166843=CARTESIAN_POINT('Ctrl Pts',(-0.372496183,0.552026826,-7.39747294));
#166844=CARTESIAN_POINT('Ctrl Pts',(-0.775478368000001,0.61615356,-7.377180967));
#166845=CARTESIAN_POINT('Ctrl Pts',(-1.173871557,0.681389364000001,-7.313233544));
#166846=CARTESIAN_POINT('Ctrl Pts',(-0.994070543983947,0.680609082247612,
-7.18152658128588));
#166847=CARTESIAN_POINT('Ctrl Pts',(-0.996726094868221,0.677652752727981,
-7.19940916869543));
#166848=CARTESIAN_POINT('Ctrl Pts',(-0.999382324343535,0.674729896879857,
-7.21729723888549));
#166849=CARTESIAN_POINT('Ctrl Pts',(-1.00202327928226,0.671836782506551,
-7.23519234198709));
#166850=CARTESIAN_POINT('Ctrl Pts',(-1.00449561666871,0.669128385356906,
-7.25194489303733));
#166851=CARTESIAN_POINT('Ctrl Pts',(-1.00695865563338,0.666446714481601,
-7.26870316048478));
#166852=CARTESIAN_POINT('Ctrl Pts',(-1.00941275741744,0.663790956140528,
-7.28546681659049));
#166853=CARTESIAN_POINT('Ctrl Pts',(-1.01186688555012,0.661135169285732,
-7.3022306526803));
#166854=CARTESIAN_POINT('Ctrl Pts',(-1.01431208269765,0.65850528861085,
-7.31899992217427));
#166855=CARTESIAN_POINT('Ctrl Pts',(-1.01674868797125,0.655900535661223,
-7.33577431833995));
#166856=CARTESIAN_POINT('Ctrl Pts',(-0.989418577999999,0.681369595,-7.182168954));
#166857=CARTESIAN_POINT('Ctrl Pts',(-0.997978637,0.679970133000001,-7.180989716));
#166858=CARTESIAN_POINT('Ctrl Pts',(-1.00653586,0.678571429,-7.179790078));
#166859=CARTESIAN_POINT('Ctrl Pts',(-1.390062022,0.615882895,-7.126023487));
#166860=CARTESIAN_POINT('Ctrl Pts',(-1.76567788,0.552026826,-7.031705456));
#166861=CARTESIAN_POINT('Ctrl Pts',(-0.856834899,0.681369595,-7.357118544));
#166862=CARTESIAN_POINT('Ctrl Pts',(-0.865603471,0.679970133000001,-7.356097326));
#166863=CARTESIAN_POINT('Ctrl Pts',(-0.874369584,0.678571429,-7.35505521));
#166864=CARTESIAN_POINT('Ctrl Pts',(-1.267257964,0.615882895,-7.30834860600001));
#166865=CARTESIAN_POINT('Ctrl Pts',(-1.652934871,0.552026826,-7.220053021));
#166866=CARTESIAN_POINT('',(-1.74673693330736,0.552026824384643,-7.06334803539695));
#166867=CARTESIAN_POINT('Ctrl Pts',(-1.41063172,0.499686101,-7.16479510800001));
#166868=CARTESIAN_POINT('Ctrl Pts',(-1.520254036,0.51775868,-7.143212256));
#166869=CARTESIAN_POINT('Ctrl Pts',(-1.629164754,0.535714286,-7.118285819));
#166870=CARTESIAN_POINT('Ctrl Pts',(-1.678561207,0.54385805,-7.106980434));
#166871=CARTESIAN_POINT('Ctrl Pts',(-1.727796006,0.552026826,-7.09499061));
#166872=CARTESIAN_POINT('Ctrl Pts',(-1.4512899,0.499686101,-7.103256832));
#166873=CARTESIAN_POINT('Ctrl Pts',(-1.559970672,0.51775868,-7.081051904));
#166874=CARTESIAN_POINT('Ctrl Pts',(-1.667921256,0.535714286,-7.055532488));
#166875=CARTESIAN_POINT('Ctrl Pts',(-1.71688224,0.54385805,-7.043958157));
#166876=CARTESIAN_POINT('Ctrl Pts',(-1.76567788,0.552026826,-7.031705456));
#166877=CARTESIAN_POINT('Ctrl Pts',(-1.76567787792048,0.552026825801985,
-7.03170545779501));
#166878=CARTESIAN_POINT('Ctrl Pts',(-1.71387913432024,0.543355306566488,
-7.04471224566189));
#166879=CARTESIAN_POINT('Ctrl Pts',(-1.66198181461837,0.534726112489088,
-7.05713583498964));
#166880=CARTESIAN_POINT('Ctrl Pts',(-1.55780050367311,0.517398614477502,
-7.08086267381247));
#166881=CARTESIAN_POINT('Ctrl Pts',(-1.50555235354915,0.508709450041202,
-7.09215552884824));
#166882=CARTESIAN_POINT('Ctrl Pts',(-1.45317754991343,0.499999999567749,
-7.10287089870231));
#166883=CARTESIAN_POINT('Ctrl Pts',(-1.4512899,0.499686101,-7.103256832));
#166884=CARTESIAN_POINT('Ctrl Pts',(-1.559970672,0.51775868,-7.081051904));
#166885=CARTESIAN_POINT('Ctrl Pts',(-1.667921256,0.535714286,-7.055532488));
#166886=CARTESIAN_POINT('Ctrl Pts',(-1.717818234,0.544013736,-7.043736889));
#166887=CARTESIAN_POINT('Ctrl Pts',(-1.767543392,0.552339147,-7.031236759));
#166888=CARTESIAN_POINT('Ctrl Pts',(-1.504270571,0.499686101,-7.138261025));
#166889=CARTESIAN_POINT('Ctrl Pts',(-1.613486912,0.51775868,-7.11524548600001));
#166890=CARTESIAN_POINT('Ctrl Pts',(-1.721948015,0.535714286,-7.088899452));
#166891=CARTESIAN_POINT('Ctrl Pts',(-1.772080965,0.544013736,-7.076721774));
#166892=CARTESIAN_POINT('Ctrl Pts',(-1.822036668,0.552339147,-7.06383626599999));
#166893=CARTESIAN_POINT('Ctrl Pts',(-1.76567788662873,0.552026827401467,
-7.03170545488938));
#166894=CARTESIAN_POINT('Ctrl Pts',(-1.76691085502878,0.551172308331837,
-7.03678067949942));
#166895=CARTESIAN_POINT('Ctrl Pts',(-1.76814306468081,0.550320534997803,
-7.04185654629875));
#166896=CARTESIAN_POINT('Ctrl Pts',(-1.7693745187319,0.549471478087945,
-7.04693304994408));
#166897=CARTESIAN_POINT('Ctrl Pts',(-1.77051775403243,0.548683245810301,
-7.0516458836592));
#166898=CARTESIAN_POINT('Ctrl Pts',(-1.77166033842302,0.547897354495996,
-7.05635926750844));
#166899=CARTESIAN_POINT('Ctrl Pts',(-1.77280227815134,0.547113782447071,
-7.0610731923917));
#166900=CARTESIAN_POINT('Ctrl Pts',(-1.77394421903353,0.546330209606392,
-7.0657871220381));
#166901=CARTESIAN_POINT('Ctrl Pts',(-1.77508551553932,0.545548955838506,
-7.07050159390896));
#166902=CARTESIAN_POINT('Ctrl Pts',(-1.77622617503589,0.544769999908563,
-7.07521659892975));
#166903=CARTESIAN_POINT('Ctrl Pts',(-1.763847811,0.55233793,-7.032164738));
#166904=CARTESIAN_POINT('Ctrl Pts',(-1.918387675,0.526068113,-6.99340216400001));
#166905=CARTESIAN_POINT('Ctrl Pts',(-2.07107546,0.49968693,-6.947887912));
#166906=CARTESIAN_POINT('Ctrl Pts',(-1.731219669,0.55233793,-7.086640874));
#166907=CARTESIAN_POINT('Ctrl Pts',(-1.886956709,0.526068113,-7.048595341));
#166908=CARTESIAN_POINT('Ctrl Pts',(-2.040872013,0.49968693,-7.003744844));
#166909=CARTESIAN_POINT('Origin',(0.0702668821091162,0.410743074016567,
0.18414131516602));
#166910=CARTESIAN_POINT('Ctrl Pts',(-1.82587816458829,0.552548454735263,
-7.07038541198959));
#166911=CARTESIAN_POINT('Ctrl Pts',(-1.82742059879414,0.552287640367631,
-7.0699863709948));
#166912=CARTESIAN_POINT('Ctrl Pts',(-1.828963033,0.552026826,-7.06958733));
#166913=CARTESIAN_POINT('Ctrl Pts',(-1.983404926,0.525911829,-7.029631884));
#166914=CARTESIAN_POINT('Ctrl Pts',(-2.135954579,0.49968693,-6.982969915));
#166915=CARTESIAN_POINT('Ctrl Pts',(-1.7625991607403,0.552548454735263,
-7.03246970296457));
#166916=CARTESIAN_POINT('Ctrl Pts',(-1.76413332856506,0.552287640367631,
-7.0320844717185));
#166917=CARTESIAN_POINT('Ctrl Pts',(-1.76566749638983,0.552026826,-7.03169924047245));
#166918=CARTESIAN_POINT('Ctrl Pts',(-1.91928168760564,0.525911829,-6.99312654631239));
#166919=CARTESIAN_POINT('Ctrl Pts',(-2.07106481485737,0.49968693,-6.94788215586565));
#166920=CARTESIAN_POINT('',(-1.85985165227342,0.552026824384643,-7.08807696305218));
#166921=CARTESIAN_POINT('Ctrl Pts',(-1.75806058539698,0.550751630586318,
-7.03361817669735));
#166922=CARTESIAN_POINT('Ctrl Pts',(-1.76186923269849,0.551389228293159,
-7.03266181634868));
#166923=CARTESIAN_POINT('Ctrl Pts',(-1.76567788,0.552026826,-7.031705456));
#166924=CARTESIAN_POINT('Ctrl Pts',(-2.148734641,0.61615356,-6.935518997));
#166925=CARTESIAN_POINT('Ctrl Pts',(-2.519075981,0.681389364000001,-6.798290683));
#166926=CARTESIAN_POINT('Ctrl Pts',(-1.94628601731659,0.550751630586318,
-7.14656521854563));
#166927=CARTESIAN_POINT('Ctrl Pts',(-1.9501557306583,0.551389228293159,
-7.14550684177282));
#166928=CARTESIAN_POINT('Ctrl Pts',(-1.954025444,0.552026826,-7.14444846500001));
#166929=CARTESIAN_POINT('Ctrl Pts',(-2.343223955,0.61615356,-7.038001649));
#166930=CARTESIAN_POINT('Ctrl Pts',(-2.718556127,0.681389364000001,-6.889906523));
#166931=CARTESIAN_POINT('Ctrl Pts',(-2.51464565778637,0.680609082082812,
-6.79993069840003));
#166932=CARTESIAN_POINT('Ctrl Pts',(-2.52108335059132,0.677652752711293,
-6.8168243355651));
#166933=CARTESIAN_POINT('Ctrl Pts',(-2.52752288517147,0.674729896859141,
-6.83372318185063));
#166934=CARTESIAN_POINT('Ctrl Pts',(-2.533949014258,0.671836782489221,-6.85063218017266));
#166935=CARTESIAN_POINT('Ctrl Pts',(-2.5399648530648,0.669128385339904,
-6.86646158647935));
#166936=CARTESIAN_POINT('Ctrl Pts',(-2.54597283970899,0.666446714463603,
-6.88229857441854));
#166937=CARTESIAN_POINT('Ctrl Pts',(-2.5519732565292,0.663790956120468,
-6.89814274625858));
#166938=CARTESIAN_POINT('Ctrl Pts',(-2.55797373777326,0.66113516926362,
-6.91398708821056));
#166939=CARTESIAN_POINT('Ctrl Pts',(-2.563966664863,0.658505288585621,-6.9298386564313));
#166940=CARTESIAN_POINT('Ctrl Pts',(-2.56995230272842,0.655900535691932,
-6.94569707849852));
#166941=CARTESIAN_POINT('Ctrl Pts',(-2.510240543,0.681369595,-6.801558087));
#166942=CARTESIAN_POINT('Ctrl Pts',(-2.518346971,0.679970133000001,-6.79856626));
#166943=CARTESIAN_POINT('Ctrl Pts',(-2.526446244,0.678571429,-6.795555119));
#166944=CARTESIAN_POINT('Ctrl Pts',(-2.88944755,0.615882895,-6.660598773));
#166945=CARTESIAN_POINT('Ctrl Pts',(-3.236006129,0.552026826,-6.487739539));
#166946=CARTESIAN_POINT('Ctrl Pts',(-2.418365587,0.681369595,-7.000919025));
#166947=CARTESIAN_POINT('Ctrl Pts',(-2.426709623,0.679970133000001,-6.998036699));
#166948=CARTESIAN_POINT('Ctrl Pts',(-2.435046765,0.678571429,-6.995134492));
#166949=CARTESIAN_POINT('Ctrl Pts',(-2.808709094,0.615882895,-6.865060475));
#166950=CARTESIAN_POINT('Ctrl Pts',(-3.166388148,0.552026826,-6.695920057));
#166951=CARTESIAN_POINT('',(-3.22431023054923,0.552026824384642,-6.52271407592455));
#166952=CARTESIAN_POINT('Ctrl Pts',(-2.917871093,0.499686101,-6.694042058));
#166953=CARTESIAN_POINT('Ctrl Pts',(-3.020290825,0.51775868,-6.649398243));
#166954=CARTESIAN_POINT('Ctrl Pts',(-3.121296823,0.535714286,-6.601641988));
#166955=CARTESIAN_POINT('Ctrl Pts',(-3.167108091,0.54385805,-6.579982139));
#166956=CARTESIAN_POINT('Ctrl Pts',(-3.21261435,0.552026826,-6.557688604));
#166957=CARTESIAN_POINT('Ctrl Pts',(-2.944349797,0.499686101,-6.625202206));
#166958=CARTESIAN_POINT('Ctrl Pts',(-3.04571627,0.51775868,-6.580153264));
#166959=CARTESIAN_POINT('Ctrl Pts',(-3.145657109,0.535714286,-6.532024292));
#166960=CARTESIAN_POINT('Ctrl Pts',(-3.190985273,0.54385805,-6.510195399));
#166961=CARTESIAN_POINT('Ctrl Pts',(-3.236006129,0.552026826,-6.487739539));
#166962=CARTESIAN_POINT('Ctrl Pts',(-3.2360061284921,0.552026826,-6.48773954051878));
#166963=CARTESIAN_POINT('Ctrl Pts',(-3.18821448041655,0.543355305714346,
-6.51157743867596));
#166964=CARTESIAN_POINT('Ctrl Pts',(-3.14020118219395,0.534726109198169,
-6.53486696721718));
#166965=CARTESIAN_POINT('Ctrl Pts',(-3.04355912310762,0.517399145757902,
-6.58043358288906));
#166966=CARTESIAN_POINT('Ctrl Pts',(-2.99495413992492,0.50870890930923,
-6.60269697061331));
#166967=CARTESIAN_POINT('Ctrl Pts',(-2.94611035073431,0.499999999616657,
-6.62441950656244));
#166968=CARTESIAN_POINT('Ctrl Pts',(-2.944349797,0.499686101,-6.625202206));
#166969=CARTESIAN_POINT('Ctrl Pts',(-3.04571627,0.51775868,-6.580153264));
#166970=CARTESIAN_POINT('Ctrl Pts',(-3.145657109,0.535714286,-6.532024292));
#166971=CARTESIAN_POINT('Ctrl Pts',(-3.191851818,0.544013736,-6.50977809300001));
#166972=CARTESIAN_POINT('Ctrl Pts',(-3.237727271,0.552339147,-6.48688077));
#166973=CARTESIAN_POINT('Ctrl Pts',(-3.003616676,0.499686101,-6.64799874200001));
#166974=CARTESIAN_POINT('Ctrl Pts',(-3.105331939,0.51775868,-6.602043008));
#166975=CARTESIAN_POINT('Ctrl Pts',(-3.205593663,0.535714286,-6.552997));
#166976=CARTESIAN_POINT('Ctrl Pts',(-3.251936692,0.544013736,-6.530326927));
#166977=CARTESIAN_POINT('Ctrl Pts',(-3.297954455,0.552339147,-6.507003675));
#166978=CARTESIAN_POINT('Ctrl Pts',(-3.23600613543338,0.552026827322425,
-6.4877395367674));
#166979=CARTESIAN_POINT('Ctrl Pts',(-3.23830130142427,0.551172308398161,
-6.49243105314736));
#166980=CARTESIAN_POINT('Ctrl Pts',(-3.24059586393105,0.550320535064447,
-6.49712336031143));
#166981=CARTESIAN_POINT('Ctrl Pts',(-3.24288982539976,0.549471478157348,
-6.50181645186762));
#166982=CARTESIAN_POINT('Ctrl Pts',(-3.24501945239908,0.548683245862265,
-6.50617334043121));
#166983=CARTESIAN_POINT('Ctrl Pts',(-3.24714856196406,0.547897354532626,
-6.51053090619626));
#166984=CARTESIAN_POINT('Ctrl Pts',(-3.24927715823825,0.547113782470724,
-6.51488913893324));
#166985=CARTESIAN_POINT('Ctrl Pts',(-3.25140575666327,0.546330209617065,
-6.51924737607399));
#166986=CARTESIAN_POINT('Ctrl Pts',(-3.25353384233262,0.545548955838543,
-6.52360628128781));
#166987=CARTESIAN_POINT('Ctrl Pts',(-3.25566142035481,0.544769999879411,
-6.52796584418262));
#166988=CARTESIAN_POINT('Ctrl Pts',(-3.234317579,0.55233793,-6.48858149400001));
#166989=CARTESIAN_POINT('Ctrl Pts',(-3.376911579,0.526068113,-6.417503665));
#166990=CARTESIAN_POINT('Ctrl Pts',(-3.51624539,0.49968693,-6.34023015));
#166991=CARTESIAN_POINT('Ctrl Pts',(-3.214163023,0.55233793,-6.548798094));
#166992=CARTESIAN_POINT('Ctrl Pts',(-3.358080353,0.526068113,-6.478163184));
#166993=CARTESIAN_POINT('Ctrl Pts',(-3.498755672,0.49968693,-6.401274026));
#166994=CARTESIAN_POINT('Origin',(0.108208885721304,0.410743218181082,0.164730669642488));
#166995=CARTESIAN_POINT('Ctrl Pts',(-3.30311401212512,0.552548454735263,
-6.5125738978046));
#166996=CARTESIAN_POINT('Ctrl Pts',(-3.30453460306256,0.552287640367631,
-6.5118526084023));
#166997=CARTESIAN_POINT('Ctrl Pts',(-3.305955194,0.552026826,-6.511131319));
#166998=CARTESIAN_POINT('Ctrl Pts',(-3.448197082,0.525911829,-6.438909567));
#166999=CARTESIAN_POINT('Ctrl Pts',(-3.587149265,0.49968693,-6.360544862));
#167000=CARTESIAN_POINT('Ctrl Pts',(-3.23316367901391,0.552548454735263,
-6.48914775193897));
#167001=CARTESIAN_POINT('Ctrl Pts',(-3.234579165521,0.552287640367631,-6.48844172645311));
#167002=CARTESIAN_POINT('Ctrl Pts',(-3.2359946520281,0.552026826,-6.48773570096726));
#167003=CARTESIAN_POINT('Ctrl Pts',(-3.37772544018258,0.525911829,-6.41704230469282));
#167004=CARTESIAN_POINT('Ctrl Pts',(-3.51623375636657,0.49968693,-6.34022681684067));
#167005=CARTESIAN_POINT('',(-3.34009637854947,0.552026824384643,-6.52254853458343));
#167006=CARTESIAN_POINT('Ctrl Pts',(-3.22897810090943,0.550751630586318,
-6.49124503453278));
#167007=CARTESIAN_POINT('Ctrl Pts',(-3.23249211495472,0.551389228293159,
-6.48949228676639));
#167008=CARTESIAN_POINT('Ctrl Pts',(-3.236006129,0.552026826,-6.487739539));
#167009=CARTESIAN_POINT('Ctrl Pts',(-3.589429991,0.61615356,-6.311455985));
#167010=CARTESIAN_POINT('Ctrl Pts',(-3.921612925,0.681389364,-6.09782355200001));
#167011=CARTESIAN_POINT('Ctrl Pts',(-3.43708320223719,0.550751630586318,
-6.56108853400832));
#167012=CARTESIAN_POINT('Ctrl Pts',(-3.44063492411859,0.551389228293159,
-6.55922302750416));
#167013=CARTESIAN_POINT('Ctrl Pts',(-3.444186646,0.552026826,-6.557357521));
#167014=CARTESIAN_POINT('Ctrl Pts',(-3.801402994,0.61615356,-6.369733196));
#167015=CARTESIAN_POINT('Ctrl Pts',(-4.136124034,0.681389364,-6.14441513));
#167016=CARTESIAN_POINT('Ctrl Pts',(-3.91763873527765,0.680609082082812,
-6.10037761323453));
#167017=CARTESIAN_POINT('Ctrl Pts',(-3.9275575515231,0.6776527527834,-6.11549237277444));
#167018=CARTESIAN_POINT('Ctrl Pts',(-3.9374792857128,0.67472989692545,-6.13061182384924));
#167019=CARTESIAN_POINT('Ctrl Pts',(-3.94739011022992,0.671836782553413,
-6.1457440713838));
#167020=CARTESIAN_POINT('Ctrl Pts',(-3.95666815648968,0.669128385393101,
-6.15991016749386));
#167021=CARTESIAN_POINT('Ctrl Pts',(-3.96594016399478,0.666446714505989,
-6.17408535596371));
#167022=CARTESIAN_POINT('Ctrl Pts',(-3.97520632298163,0.663790956152371,
-6.18826918766651));
#167023=CARTESIAN_POINT('Ctrl Pts',(-3.98447258145517,0.66113516928504,
-6.2024531716549));
#167024=CARTESIAN_POINT('Ctrl Pts',(-3.99373301582162,0.658505288596885,
-6.2166458368851));
#167025=CARTESIAN_POINT('Ctrl Pts',(-4.00298780534354,0.655900535589649,
-6.23084676214381));
#167026=CARTESIAN_POINT('Ctrl Pts',(-3.91368645,0.681369595,-6.102913924));
#167027=CARTESIAN_POINT('Ctrl Pts',(-3.9209602,0.679970133000001,-6.098249402));
#167028=CARTESIAN_POINT('Ctrl Pts',(-3.928222811,0.678571429,-6.093567555));
#167029=CARTESIAN_POINT('Ctrl Pts',(-4.253725723,0.615882895,-5.883731863));
#167030=CARTESIAN_POINT('Ctrl Pts',(-4.55502232900001,0.552026826,-5.640414132));
#167031=CARTESIAN_POINT('Ctrl Pts',(-3.866816188,0.681369595,-6.317364314));
#167032=CARTESIAN_POINT('Ctrl Pts',(-3.874345531,0.679970133000001,-6.312755654));
#167033=CARTESIAN_POINT('Ctrl Pts',(-3.881863866,0.678571429,-6.30812906));
#167034=CARTESIAN_POINT('Ctrl Pts',(-4.218828109,0.615882895,-6.100769745));
#167035=CARTESIAN_POINT('Ctrl Pts',(-4.531784635,0.552026826,-5.85869331300001));
#167036=CARTESIAN_POINT('',(-4.55111836570588,0.552026824383862,-5.67708525624827));
#167037=CARTESIAN_POINT('Ctrl Pts',(-4.288674056,0.499686101,-5.910283042));
#167038=CARTESIAN_POINT('Ctrl Pts',(-4.379102171,0.51775868,-5.844665759));
#167039=CARTESIAN_POINT('Ctrl Pts',(-4.467480522,0.535714286,-5.776312715));
#167040=CARTESIAN_POINT('Ctrl Pts',(-4.507564521,0.54385805,-5.745311193));
#167041=CARTESIAN_POINT('Ctrl Pts',(-4.547214418,0.552026826,-5.713756368));
#167042=CARTESIAN_POINT('Ctrl Pts',(-4.29973517,0.499686101,-5.837360488));
#167043=CARTESIAN_POINT('Ctrl Pts',(-4.38904756,0.51775868,-5.77157397));
#167044=CARTESIAN_POINT('Ctrl Pts',(-4.476305531,0.535714286,-5.703085901));
#167045=CARTESIAN_POINT('Ctrl Pts',(-4.51588138099999,0.54385805,-5.672023139));
#167046=CARTESIAN_POINT('Ctrl Pts',(-4.555022329,0.552026826,-5.640414132));
#167047=CARTESIAN_POINT('Ctrl Pts',(-4.55502232574641,0.552026825573623,
-5.64041413432871));
#167048=CARTESIAN_POINT('Ctrl Pts',(-4.5289092151985,0.546576979320718,
-5.66150226752041));
#167049=CARTESIAN_POINT('Ctrl Pts',(-4.50266881557143,0.541139220053964,
-5.68239357447142));
#167050=CARTESIAN_POINT('Ctrl Pts',(-4.47630553125182,0.535714286005299,
-5.70308590100704));
#167051=CARTESIAN_POINT('Ctrl Pts',(-4.41873725026094,0.523868108875745,
-5.74827077517669));
#167052=CARTESIAN_POINT('Ctrl Pts',(-4.36038638074774,0.511960760877559,
-5.79266092730607));
#167053=CARTESIAN_POINT('Ctrl Pts',(-4.30128630597295,0.499999999668149,
-5.8362176204432));
#167054=CARTESIAN_POINT('Ctrl Pts',(-4.29973517,0.499686101,-5.837360488));
#167055=CARTESIAN_POINT('Ctrl Pts',(-4.38904756,0.51775868,-5.77157397));
#167056=CARTESIAN_POINT('Ctrl Pts',(-4.476305531,0.535714286,-5.703085901));
#167057=CARTESIAN_POINT('Ctrl Pts',(-4.516637959,0.544013736,-5.671429308));
#167058=CARTESIAN_POINT('Ctrl Pts',(-4.556518621,0.552339147,-5.639205445));
#167059=CARTESIAN_POINT('Ctrl Pts',(-4.362517003,0.499686101,-5.84688342700001));
#167060=CARTESIAN_POINT('Ctrl Pts',(-4.451975096,0.51775868,-5.780136338));
#167061=CARTESIAN_POINT('Ctrl Pts',(-4.539349314,0.535714286,-5.710683691));
#167062=CARTESIAN_POINT('Ctrl Pts',(-4.579735474,0.544013736,-5.67858125));
#167063=CARTESIAN_POINT('Ctrl Pts',(-4.619663557,0.552339147,-5.645910824));
#167064=CARTESIAN_POINT('Ctrl Pts',(-4.55502233394114,0.552026827283876,
-5.6404141277109));
#167065=CARTESIAN_POINT('Ctrl Pts',(-4.55827237826771,0.551172308283001,
-5.64450256670423));
#167066=CARTESIAN_POINT('Ctrl Pts',(-4.56152200254063,0.550320534963249,
-5.64859190724774));
#167067=CARTESIAN_POINT('Ctrl Pts',(-4.56477120845016,0.549471478067904,
-5.65268214304781));
#167068=CARTESIAN_POINT('Ctrl Pts',(-4.56778764820871,0.548683245789709,
-5.65647936311718));
#167069=CARTESIAN_POINT('Ctrl Pts',(-4.57080372820987,0.547897354475107,
-5.66027735578707));
#167070=CARTESIAN_POINT('Ctrl Pts',(-4.57381945031748,0.547113782422384,
-5.66407611019601));
#167071=CARTESIAN_POINT('Ctrl Pts',(-4.57683517544067,0.546330209586128,
-5.66787486840351));
#167072=CARTESIAN_POINT('Ctrl Pts',(-4.57985054342965,0.545548955819245,
-5.67167438931052));
#167073=CARTESIAN_POINT('Ctrl Pts',(-4.58286555741887,0.544770000006238,
-5.67547466108768));
#167074=CARTESIAN_POINT('Ctrl Pts',(-4.553554251,0.55233793,-5.641599391));
#167075=CARTESIAN_POINT('Ctrl Pts',(-4.677534851,0.526068113,-5.541529827));
#167076=CARTESIAN_POINT('Ctrl Pts',(-4.796999593,0.49968693,-5.436110273));
#167077=CARTESIAN_POINT('Ctrl Pts',(-4.546815687,0.55233793,-5.704740794));
#167078=CARTESIAN_POINT('Ctrl Pts',(-4.672183892,0.526068113,-5.604819318));
#167079=CARTESIAN_POINT('Ctrl Pts',(-4.793041404,0.49968693,-5.49948675));
#167080=CARTESIAN_POINT('Origin',(0.141090736557263,0.410743122402995,0.137617013932505));
#167081=CARTESIAN_POINT('Ctrl Pts',(-4.62589992017682,0.552548454735263,
-5.65024166521514));
#167082=CARTESIAN_POINT('Ctrl Pts',(-4.62713224258841,0.552287640367631,
-5.64923185410757));
#167083=CARTESIAN_POINT('Ctrl Pts',(-4.628364565,0.552026826,-5.64822204299999));
#167084=CARTESIAN_POINT('Ctrl Pts',(-4.751755375,0.525911829,-5.547110995));
#167085=CARTESIAN_POINT('Ctrl Pts',(-4.870612837,0.49968693,-5.440707802));
#167086=CARTESIAN_POINT('Ctrl Pts',(-4.55254905799952,0.552548454735263,
-5.64240046442604));
#167087=CARTESIAN_POINT('Ctrl Pts',(-4.55377967661359,0.552287640367631,
-5.6414066576638));
#167088=CARTESIAN_POINT('Ctrl Pts',(-4.55501029522768,0.552026826,-5.64041285090157));
#167089=CARTESIAN_POINT('Ctrl Pts',(-4.67823050624091,0.525911829,-5.54090429679079));
#167090=CARTESIAN_POINT('Ctrl Pts',(-4.79698751476151,0.49968693,-5.43610951865134));
#167091=CARTESIAN_POINT('',(-4.66416191124399,0.552026824384635,-5.65203298540041));
#167092=CARTESIAN_POINT('Ctrl Pts',(-4.54891219022449,0.550751630586317,
-5.64534848929436));
#167093=CARTESIAN_POINT('Ctrl Pts',(-4.55196725961225,0.551389228293159,
-5.64288131064718));
#167094=CARTESIAN_POINT('Ctrl Pts',(-4.555022329,0.552026826,-5.640414132));
#167095=CARTESIAN_POINT('Ctrl Pts',(-4.862287584,0.61615356,-5.392276306));
#167096=CARTESIAN_POINT('Ctrl Pts',(-5.14077960699999,0.681389364000001,
-5.112228969));
#167097=CARTESIAN_POINT('Ctrl Pts',(-4.76716619730485,0.550751630586317,
-5.66882264040786));
#167098=CARTESIAN_POINT('Ctrl Pts',(-4.77023385315242,0.551389228293159,
-5.66623723320393));
#167099=CARTESIAN_POINT('Ctrl Pts',(-4.773301509,0.552026826,-5.663651826));
#167100=CARTESIAN_POINT('Ctrl Pts',(-5.081832654,0.61615356,-5.403623099));
#167101=CARTESIAN_POINT('Ctrl Pts',(-5.360291378,0.681389364000001,-5.11161771400001));
#167102=CARTESIAN_POINT('Ctrl Pts',(-5.137447379847,0.680609082082805,-5.11557765142985));
#167103=CARTESIAN_POINT('Ctrl Pts',(-5.15038352582319,0.677652752674818,
-5.12820678402029));
#167104=CARTESIAN_POINT('Ctrl Pts',(-5.16332353063032,0.674729896868104,
-5.14083987093191));
#167105=CARTESIAN_POINT('Ctrl Pts',(-5.17625563150039,0.67183678250658,
-5.15348780056847));
#167106=CARTESIAN_POINT('Ctrl Pts',(-5.18836205414182,0.669128385351123,
-5.16532819550953));
#167107=CARTESIAN_POINT('Ctrl Pts',(-5.20046453379357,0.666446714469152,
-5.17717876839636));
#167108=CARTESIAN_POINT('Ctrl Pts',(-5.21256315969722,0.663790956120692,
-5.18903903970536));
#167109=CARTESIAN_POINT('Ctrl Pts',(-5.22466191549854,0.661135169258514,
-5.20089943835291));
#167110=CARTESIAN_POINT('Ctrl Pts',(-5.23675684956298,0.658505288575528,
-5.21276956729518));
#167111=CARTESIAN_POINT('Ctrl Pts',(-5.24884804614103,0.655900535635267,
-5.2246489769404));
#167112=CARTESIAN_POINT('Ctrl Pts',(-5.134132729,0.681369595,-5.118904289));
#167113=CARTESIAN_POINT('Ctrl Pts',(-5.140233688,0.679970133,-5.11278518));
#167114=CARTESIAN_POINT('Ctrl Pts',(-5.146320044,0.678571429,-5.106651545));
#167115=CARTESIAN_POINT('Ctrl Pts',(-5.419104408,0.615882895,-4.831748191));
#167116=CARTESIAN_POINT('Ctrl Pts',(-5.661050747,0.552026826,-4.529349229));
#167117=CARTESIAN_POINT('Ctrl Pts',(-5.134458762,0.681369595,-5.338416669));
#167118=CARTESIAN_POINT('Ctrl Pts',(-5.140821347,0.679970133,-5.33229717100001));
#167119=CARTESIAN_POINT('Ctrl Pts',(-5.147169327,0.678571429,-5.326162524));
#167120=CARTESIAN_POINT('Ctrl Pts',(-5.43167941,0.615882895,-5.051213803));
#167121=CARTESIAN_POINT('Ctrl Pts',(-5.685279909,0.552026826,-4.747520581));
#167122=CARTESIAN_POINT('',(-5.66512126373428,0.552026824384634,-4.56600223927398));
#167123=CARTESIAN_POINT('Ctrl Pts',(-5.458943387,0.499686101,-4.85016575900001));
#167124=CARTESIAN_POINT('Ctrl Pts',(-5.533151567,0.51775868,-4.766643201));
#167125=CARTESIAN_POINT('Ctrl Pts',(-5.604769797,0.535714286,-4.680889479));
#167126=CARTESIAN_POINT('Ctrl Pts',(-5.637252244,0.54385805,-4.641995881));
#167127=CARTESIAN_POINT('Ctrl Pts',(-5.669191793,0.552026826,-4.602655234));
#167128=CARTESIAN_POINT('Ctrl Pts',(-5.454069705,0.499686101,-4.776570282));
#167129=CARTESIAN_POINT('Ctrl Pts',(-5.527151864,0.51775868,-4.69312229100001));
#167130=CARTESIAN_POINT('Ctrl Pts',(-5.597646882,0.535714286,-4.607477551));
#167131=CARTESIAN_POINT('Ctrl Pts',(-5.629619895,0.54385805,-4.568633382));
#167132=CARTESIAN_POINT('Ctrl Pts',(-5.661050747,0.552026826,-4.529349229));
#167133=CARTESIAN_POINT('Ctrl Pts',(-5.66105074078458,0.552026824384634,
-4.52934923676839));
#167134=CARTESIAN_POINT('Ctrl Pts',(-5.64008146987551,0.546576979226268,
-4.55555788184023));
#167135=CARTESIAN_POINT('Ctrl Pts',(-5.61894557098121,0.541139220351658,
-4.58160167019615));
#167136=CARTESIAN_POINT('Ctrl Pts',(-5.59764688197218,0.535714285992477,
-4.6074775510536));
#167137=CARTESIAN_POINT('Ctrl Pts',(-5.55113792654149,0.523868108732891,
-4.66398150703629));
#167138=CARTESIAN_POINT('Ctrl Pts',(-5.50369384036136,0.511960761028742,
-4.71987755304587));
#167139=CARTESIAN_POINT('Ctrl Pts',(-5.45533889445124,0.499999999895942,
-4.7751206845917));
#167140=CARTESIAN_POINT('Ctrl Pts',(-5.454069705,0.499686101,-4.776570282));
#167141=CARTESIAN_POINT('Ctrl Pts',(-5.527151864,0.51775868,-4.69312229100001));
#167142=CARTESIAN_POINT('Ctrl Pts',(-5.597646882,0.535714286,-4.607477551));
#167143=CARTESIAN_POINT('Ctrl Pts',(-5.630231128,0.544013736,-4.567890792));
#167144=CARTESIAN_POINT('Ctrl Pts',(-5.662252225,0.552339147,-4.527847142));
#167145=CARTESIAN_POINT('Ctrl Pts',(-5.517430884,0.499686101,-4.772374341));
#167146=CARTESIAN_POINT('Ctrl Pts',(-5.590448845,0.51775868,-4.68795691599999));
#167147=CARTESIAN_POINT('Ctrl Pts',(-5.660850037,0.535714286,-4.601345159));
#167148=CARTESIAN_POINT('Ctrl Pts',(-5.693390914,0.544013736,-4.561311425));
#167149=CARTESIAN_POINT('Ctrl Pts',(-5.725362325,0.552339147,-4.520821458));
#167150=CARTESIAN_POINT('Ctrl Pts',(-5.6610507513522,0.552026827290018,
-4.52934922382194));
#167151=CARTESIAN_POINT('Ctrl Pts',(-5.66510370465548,0.551172308350208,
-4.5326434135973));
#167152=CARTESIAN_POINT('Ctrl Pts',(-5.66915644181873,0.550320535011006,
-4.53593857447903));
#167153=CARTESIAN_POINT('Ctrl Pts',(-5.67320896285281,0.549471478098695,
-4.53923469962419));
#167154=CARTESIAN_POINT('Ctrl Pts',(-5.67697116994167,0.548683245808849,
-4.54229469740892));
#167155=CARTESIAN_POINT('Ctrl Pts',(-5.68073319176982,0.547897354484637,
-4.54535552706958));
#167156=CARTESIAN_POINT('Ctrl Pts',(-5.68449502780371,0.547113782428027,
-4.54841717758078));
#167157=CARTESIAN_POINT('Ctrl Pts',(-5.68825686763873,0.54633020957966,
-4.55147883118561));
#167158=CARTESIAN_POINT('Ctrl Pts',(-5.69201852262752,0.545548955806292,
-4.5545413064157));
#167159=CARTESIAN_POINT('Ctrl Pts',(-5.69577999340436,0.544769999894628,
-4.55760459146533));
#167160=CARTESIAN_POINT('Ctrl Pts',(-5.659871788,0.55233793,-4.53082237));
#167161=CARTESIAN_POINT('Ctrl Pts',(-5.759441792,0.526068113,-4.406440213));
#167162=CARTESIAN_POINT('Ctrl Pts',(-5.853451427,0.49968693,-4.277803922));
#167163=CARTESIAN_POINT('Ctrl Pts',(-5.666864302,0.55233793,-4.593936154));
#167164=CARTESIAN_POINT('Ctrl Pts',(-5.767821305,0.526068113,-4.469400329));
#167165=CARTESIAN_POINT('Ctrl Pts',(-5.863209847,0.49968693,-4.340549585));
#167166=CARTESIAN_POINT('Origin',(0.167376173419037,0.410743101075361,0.104069638273634));
#167167=CARTESIAN_POINT('Ctrl Pts',(-5.73238388827847,0.552548454735263,
-4.52371041336006));
#167168=CARTESIAN_POINT('Ctrl Pts',(-5.73337032013923,0.552287640367632,
-4.52245929818003));
#167169=CARTESIAN_POINT('Ctrl Pts',(-5.734356752,0.552026826,-4.521208183));
#167170=CARTESIAN_POINT('Ctrl Pts',(-5.833126867,0.525911829,-4.395935678));
#167171=CARTESIAN_POINT('Ctrl Pts',(-5.926331967,0.49968693,-4.266469291));
#167172=CARTESIAN_POINT('Ctrl Pts',(-5.65906230248553,0.552548454735263,
-4.53182080222694));
#167173=CARTESIAN_POINT('Ctrl Pts',(-5.6600505108422,0.552287640367632,
-4.5305856834911));
#167174=CARTESIAN_POINT('Ctrl Pts',(-5.66103871919887,0.552026826,-4.52935056475526));
#167175=CARTESIAN_POINT('Ctrl Pts',(-5.75998671237974,0.525911829,-4.40567976251412));
#167176=CARTESIAN_POINT('Ctrl Pts',(-5.85343946900773,0.49968693,-4.27780578174788));
#167177=CARTESIAN_POINT('',(-5.77013641680195,0.552026824384827,-4.51723465591715));
#167178=CARTESIAN_POINT('Ctrl Pts',(-5.65614292522696,0.550751630586318,
-4.53548186325545));
#167179=CARTESIAN_POINT('Ctrl Pts',(-5.65859619839297,0.551389228293159,
-4.53241561695019));
#167180=CARTESIAN_POINT('Ctrl Pts',(-5.66104947155899,0.552026826000001,
-4.52934937064493));
#167181=CARTESIAN_POINT('Ctrl Pts',(-5.9077887462752,0.61615356,-4.22095999112541));
#167182=CARTESIAN_POINT('Ctrl Pts',(-6.11956789649333,0.681389364,-3.88759252035654));
#167183=CARTESIAN_POINT('Ctrl Pts',(-5.87434179975964,0.550751630586318,
-4.51148890129795));
#167184=CARTESIAN_POINT('Ctrl Pts',(-5.87678194937982,0.551389228293159,
-4.50830448414898));
#167185=CARTESIAN_POINT('Ctrl Pts',(-5.879222099,0.552026826000001,-4.505120067));
#167186=CARTESIAN_POINT('Ctrl Pts',(-6.124641466,0.61615356,-4.184845591));
#167187=CARTESIAN_POINT('Ctrl Pts',(-6.333817454,0.681389364000001,-3.839806735));
#167188=CARTESIAN_POINT('Ctrl Pts',(-6.11703469536907,0.680609082247603,
-3.89157896392074));
#167189=CARTESIAN_POINT('Ctrl Pts',(-6.13238329170514,0.677652752674814,
-3.90113194489534));
#167190=CARTESIAN_POINT('Ctrl Pts',(-6.14773650636248,0.674729896768819,
-3.91068795923836));
#167191=CARTESIAN_POINT('Ctrl Pts',(-6.16308519293365,0.671836782400283,
-3.92026016792834));
#167192=CARTESIAN_POINT('Ctrl Pts',(-6.17745390895607,0.669128385262255,
-3.92922121796579));
#167193=CARTESIAN_POINT('Ctrl Pts',(-6.19182096212797,0.666446714395948,
-3.93819305562519));
#167194=CARTESIAN_POINT('Ctrl Pts',(-6.20618633652179,0.663790956061759,
-3.94717519340858));
#167195=CARTESIAN_POINT('Ctrl Pts',(-6.22055186515037,0.661135169213851,
-3.95615742762927));
#167196=CARTESIAN_POINT('Ctrl Pts',(-6.23491575311536,0.658505288543741,
-3.96514998621989));
#167197=CARTESIAN_POINT('Ctrl Pts',(-6.24927798598832,0.655900535655765,
-3.97415241251114));
#167198=CARTESIAN_POINT('Ctrl Pts',(-6.114512667,0.681369595,-3.895540379));
#167199=CARTESIAN_POINT('Ctrl Pts',(-6.119155562,0.679970133,-3.888252805));
#167200=CARTESIAN_POINT('Ctrl Pts',(-6.123781072,0.678571429,-3.880954185));
#167201=CARTESIAN_POINT('Ctrl Pts',(-6.331091794,0.615882895,-3.553837343));
#167202=CARTESIAN_POINT('Ctrl Pts',(-6.502374724,0.552026826,-3.20649699));
#167203=CARTESIAN_POINT('Ctrl Pts',(-6.162019751,0.681369595,-4.109850593));
#167204=CARTESIAN_POINT('Ctrl Pts',(-6.166918071,0.679970133,-4.102506398));
#167205=CARTESIAN_POINT('Ctrl Pts',(-6.171798871,0.678571429,-4.095150548));
#167206=CARTESIAN_POINT('Ctrl Pts',(-6.390551418,0.615882895,-3.765468718));
#167207=CARTESIAN_POINT('Ctrl Pts',(-6.572937813,0.552026826,-3.414359063));
#167208=CARTESIAN_POINT('',(-6.51422938855193,0.552026824384625,-3.24141803243923));
#167209=CARTESIAN_POINT('Ctrl Pts',(-6.373958593,0.499686101,-3.563260116));
#167210=CARTESIAN_POINT('Ctrl Pts',(-6.42847694499999,0.51775868,-3.465737703));
#167211=CARTESIAN_POINT('Ctrl Pts',(-6.479986266,0.535714286,-3.366593053));
#167212=CARTESIAN_POINT('Ctrl Pts',(-6.503348317,0.54385805,-3.321626));
#167213=CARTESIAN_POINT('Ctrl Pts',(-6.526084062,0.552026826000001,-3.276339057));
#167214=CARTESIAN_POINT('Ctrl Pts',(-6.353378002,0.499686101,-3.492432958));
#167215=CARTESIAN_POINT('Ctrl Pts',(-6.40681269,0.51775868,-3.395225431));
#167216=CARTESIAN_POINT('Ctrl Pts',(-6.457248486,0.535714286,-3.296428672));
#167217=CARTESIAN_POINT('Ctrl Pts',(-6.48012364,0.54385805,-3.251619405));
#167218=CARTESIAN_POINT('Ctrl Pts',(-6.502374724,0.552026826000001,-3.20649699));
#167219=CARTESIAN_POINT('Ctrl Pts',(-6.50237472430817,0.552026826188107,
-3.20649698942514));
#167220=CARTESIAN_POINT('Ctrl Pts',(-6.48752978291789,0.546576979715855,
-3.23660067292705));
#167221=CARTESIAN_POINT('Ctrl Pts',(-6.47248667262769,0.541139220244448,
-3.26657916856151));
#167222=CARTESIAN_POINT('Ctrl Pts',(-6.45724848592935,0.535714285974849,
-3.29642867213839));
#167223=CARTESIAN_POINT('Ctrl Pts',(-6.42397356473939,0.523868108816351,
-3.36160964736033));
#167224=CARTESIAN_POINT('Ctrl Pts',(-6.38965469195533,0.511960760953255,
-3.42639795188723));
#167225=CARTESIAN_POINT('Ctrl Pts',(-6.35430589758883,0.499999999782203,
-3.49074441377444));
#167226=CARTESIAN_POINT('Ctrl Pts',(-6.353378002,0.499686101,-3.492432958));
#167227=CARTESIAN_POINT('Ctrl Pts',(-6.40681269,0.51775868,-3.395225431));
#167228=CARTESIAN_POINT('Ctrl Pts',(-6.457248486,0.535714286,-3.296428672));
#167229=CARTESIAN_POINT('Ctrl Pts',(-6.48056094700001,0.544013736,-3.25076278));
#167230=CARTESIAN_POINT('Ctrl Pts',(-6.503225208,0.552339147,-3.204771738));
#167231=CARTESIAN_POINT('Ctrl Pts',(-6.414355829,0.499686101,-3.474714335));
#167232=CARTESIAN_POINT('Ctrl Pts',(-6.46751942,0.51775868,-3.376573839));
#167233=CARTESIAN_POINT('Ctrl Pts',(-6.517655703,0.535714286,-3.276852842));
#167234=CARTESIAN_POINT('Ctrl Pts',(-6.54082972400001,0.544013736,-3.230759748));
#167235=CARTESIAN_POINT('Ctrl Pts',(-6.563349515,0.552339147,-3.184343505));
#167236=CARTESIAN_POINT('Ctrl Pts',(-6.50237472702647,0.552026827186047,
-3.20649698391275));
#167237=CARTESIAN_POINT('Ctrl Pts',(-6.50704107826924,0.551172308290511,
-3.20884289203978));
#167238=CARTESIAN_POINT('Ctrl Pts',(-6.51170742690672,0.55032053497357,
-3.21118979521659));
#167239=CARTESIAN_POINT('Ctrl Pts',(-6.51637377175448,0.549471478080048,
-3.21353768657626));
#167240=CARTESIAN_POINT('Ctrl Pts',(-6.52070582963712,0.548683245806524,
-3.21571738002029));
#167241=CARTESIAN_POINT('Ctrl Pts',(-6.52503788541765,0.547897354495662,
-3.2178979257188));
#167242=CARTESIAN_POINT('Ctrl Pts',(-6.52936993621104,0.547113782448559,
-3.22007931301918));
#167243=CARTESIAN_POINT('Ctrl Pts',(-6.53370199137159,0.546330209611536,
-3.22226070251861));
#167244=CARTESIAN_POINT('Ctrl Pts',(-6.53803404263738,0.545548955845697,
-3.2244429341727));
#167245=CARTESIAN_POINT('Ctrl Pts',(-6.54236608770616,0.544769999912445,
-3.22662599655894));
#167246=CARTESIAN_POINT('Ctrl Pts',(-6.50154001000001,0.552337930000001,
-3.208189131));
#167247=CARTESIAN_POINT('Ctrl Pts',(-6.572043636,0.526068113,-3.065310352));
#167248=CARTESIAN_POINT('Ctrl Pts',(-6.636202377,0.49968693,-2.919472213));
#167249=CARTESIAN_POINT('Ctrl Pts',(-6.521936642,0.552337930000001,-3.268324166));
#167250=CARTESIAN_POINT('Ctrl Pts',(-6.593761804,0.526068113,-3.124997148));
#167251=CARTESIAN_POINT('Ctrl Pts',(-6.659221114,0.49968693,-2.978653146));
#167252=CARTESIAN_POINT('Origin',(0.185833727268683,0.410743087570367,0.0656550491000485));
#167253=CARTESIAN_POINT('Ctrl Pts',(-6.570827957299,0.552548454735263,-3.18565548897648));
#167254=CARTESIAN_POINT('Ctrl Pts',(-6.57152237414949,0.552287640367631,
-3.18422157048824));
#167255=CARTESIAN_POINT('Ctrl Pts',(-6.572216791,0.552026826,-3.182787652));
#167256=CARTESIAN_POINT('Ctrl Pts',(-6.64174783,0.525911829,-3.039211294));
#167257=CARTESIAN_POINT('Ctrl Pts',(-6.704942401,0.49968693,-2.892735418));
#167258=CARTESIAN_POINT('Ctrl Pts',(-6.50096408335731,0.552548454735263,
-3.20933823603486));
#167259=CARTESIAN_POINT('Ctrl Pts',(-6.50166367393037,0.552287640367631,
-3.2079195580993));
#167260=CARTESIAN_POINT('Ctrl Pts',(-6.50236326450344,0.552026826,-3.20650088016375));
#167261=CARTESIAN_POINT('Ctrl Pts',(-6.57241234148776,0.525911829,-3.06445053850729));
#167262=CARTESIAN_POINT('Ctrl Pts',(-6.63619109832366,0.49968693,-2.91947659990067));
#167263=CARTESIAN_POINT('',(-6.6063057566483,0.552026824384635,-3.17121545456552));
#167264=CARTESIAN_POINT('Ctrl Pts',(-6.4988999771904,0.550751630586317,
-3.2135412840469));
#167265=CARTESIAN_POINT('Ctrl Pts',(-6.500636741881,0.551389228293159,-3.2100193436641));
#167266=CARTESIAN_POINT('Ctrl Pts',(-6.50237350657161,0.552026826,-3.2064974032813));
#167267=CARTESIAN_POINT('Ctrl Pts',(-6.67704955408538,0.61615356,-2.85227634560151));
#167268=CARTESIAN_POINT('Ctrl Pts',(-6.81221327267021,0.681389364,-2.48117656408361));
#167269=CARTESIAN_POINT('Ctrl Pts',(-6.7068397085662,0.550751630586317,
-3.14320295556554));
#167270=CARTESIAN_POINT('Ctrl Pts',(-6.7085382532831,0.551389228293159,
-3.13956842828277));
#167271=CARTESIAN_POINT('Ctrl Pts',(-6.710236798,0.552026826,-3.135933901));
#167272=CARTESIAN_POINT('Ctrl Pts',(-6.88106885100001,0.61615356,-2.770389355));
#167273=CARTESIAN_POINT('Ctrl Pts',(-7.011181266,0.681389364000001,-2.388450661));
#167274=CARTESIAN_POINT('Ctrl Pts',(-6.81059626604927,0.680609082247605,
-2.48561436902554));
#167275=CARTESIAN_POINT('Ctrl Pts',(-6.82763962922413,0.67765275263127,
-2.49164451250911));
#167276=CARTESIAN_POINT('Ctrl Pts',(-6.84468815497496,0.674729896800113,
-2.49767662485867));
#167277=CARTESIAN_POINT('Ctrl Pts',(-6.86173573966136,0.671836782439133,
-2.50372552673111));
#167278=CARTESIAN_POINT('Ctrl Pts',(-6.87769488401706,0.669128385292337,
-2.50938822323339));
#167279=CARTESIAN_POINT('Ctrl Pts',(-6.89365472342022,0.666446714418226,
-2.51506181260851));
#167280=CARTESIAN_POINT('Ctrl Pts',(-6.90961513751775,0.663790956077136,
-2.52074582218071));
#167281=CARTESIAN_POINT('Ctrl Pts',(-6.92557572297528,0.661135169222328,
-2.52642989277963));
#167282=CARTESIAN_POINT('Ctrl Pts',(-6.94153692556273,0.658505288546222,
-2.53212439906121));
#167283=CARTESIAN_POINT('Ctrl Pts',(-6.95749863316843,0.655900535537742,
-2.53782889725405));
#167284=CARTESIAN_POINT('Ctrl Pts',(-6.808984789,0.681369595,-2.49002533));
#167285=CARTESIAN_POINT('Ctrl Pts',(-6.811952522,0.679970133,-2.48191005));
#167286=CARTESIAN_POINT('Ctrl Pts',(-6.814900903,0.678571429,-2.47378772));
#167287=CARTESIAN_POINT('Ctrl Pts',(-6.947044364,0.615882895,-2.109753011));
#167288=CARTESIAN_POINT('Ctrl Pts',(-7.039654886,0.552026826,-1.733712515));
#167289=CARTESIAN_POINT('Ctrl Pts',(-6.901451545,0.681369595,-2.689112472));
#167290=CARTESIAN_POINT('Ctrl Pts',(-6.90465656,0.679970133,-2.680886986));
#167291=CARTESIAN_POINT('Ctrl Pts',(-6.907841959,0.678571429,-2.672653884));
#167292=CARTESIAN_POINT('Ctrl Pts',(-7.050608345,0.615882895,-2.3036545));
#167293=CARTESIAN_POINT('Ctrl Pts',(-7.153252451,0.552026826,-1.92154591));
#167294=CARTESIAN_POINT('',(-7.0587393865776,0.552026824384634,-1.76526872068638));
#167295=CARTESIAN_POINT('Ctrl Pts',(-6.990934579,0.499686101,-2.10974039));
#167296=CARTESIAN_POINT('Ctrl Pts',(-7.023213887,0.51775868,-2.002778163));
#167297=CARTESIAN_POINT('Ctrl Pts',(-7.052205779,0.535714286,-1.894878478));
#167298=CARTESIAN_POINT('Ctrl Pts',(-7.065355051,0.54385805,-1.845940579));
#167299=CARTESIAN_POINT('Ctrl Pts',(-7.077823892,0.552026826,-1.796824907));
#167300=CARTESIAN_POINT('Ctrl Pts',(-6.955609405,0.499686101,-2.04499335));
#167301=CARTESIAN_POINT('Ctrl Pts',(-6.986898075,0.51775868,-1.938571603));
#167302=CARTESIAN_POINT('Ctrl Pts',(-7.014916327,0.535714286,-1.831242452));
#167303=CARTESIAN_POINT('Ctrl Pts',(-7.02762400500001,0.54385805,-1.782563319));
#167304=CARTESIAN_POINT('Ctrl Pts',(-7.039654886,0.552026826,-1.733712515));
#167305=CARTESIAN_POINT('Ctrl Pts',(-7.03965488562795,0.552026825462645,
-1.7337125189069));
#167306=CARTESIAN_POINT('Ctrl Pts',(-7.02688357095935,0.543355306279276,
-1.7855698223019));
#167307=CARTESIAN_POINT('Ctrl Pts',(-7.01355081405543,0.534726109137552,
-1.83724106183393));
#167308=CARTESIAN_POINT('Ctrl Pts',(-6.98571521390196,0.517399144305422,
-1.94039718220693));
#167309=CARTESIAN_POINT('Ctrl Pts',(-6.97121732082761,0.508708906297517,
-1.99185507680409));
#167310=CARTESIAN_POINT('Ctrl Pts',(-6.95615261946262,0.499999999579507,
-2.04314481407824));
#167311=CARTESIAN_POINT('Ctrl Pts',(-6.955609405,0.499686101,-2.04499335));
#167312=CARTESIAN_POINT('Ctrl Pts',(-6.986898075,0.51775868,-1.938571603));
#167313=CARTESIAN_POINT('Ctrl Pts',(-7.014916327,0.535714286,-1.831242452));
#167314=CARTESIAN_POINT('Ctrl Pts',(-7.02786694,0.544013736,-1.781632713));
#167315=CARTESIAN_POINT('Ctrl Pts',(-7.040114608,0.552339147,-1.73184477));
#167316=CARTESIAN_POINT('Ctrl Pts',(-7.011352625,0.499686101,-2.014580548));
#167317=CARTESIAN_POINT('Ctrl Pts',(-7.042175974,0.51775868,-1.907305922));
#167318=CARTESIAN_POINT('Ctrl Pts',(-7.069703033,0.535714286,-1.799138528));
#167319=CARTESIAN_POINT('Ctrl Pts',(-7.082426605,0.544013736,-1.749141335));
#167320=CARTESIAN_POINT('Ctrl Pts',(-7.09444177600001,0.552339147,-1.698969189));
#167321=CARTESIAN_POINT('Ctrl Pts',(-7.03965488779841,0.552026827256097,
-1.73371250846653));
#167322=CARTESIAN_POINT('Ctrl Pts',(-7.04471644281915,0.551172308291889,
-1.73500044361819));
#167323=CARTESIAN_POINT('Ctrl Pts',(-7.04977820962006,0.550320534980668,
-1.73628935044783));
#167324=CARTESIAN_POINT('Ctrl Pts',(-7.05484018515242,0.549471478091212,
-1.73757922316128));
#167325=CARTESIAN_POINT('Ctrl Pts',(-7.05953953160199,0.548683245818368,
-1.73877669215685));
#167326=CARTESIAN_POINT('Ctrl Pts',(-7.06423905921018,0.547897354506795,
-1.73997499392441));
#167327=CARTESIAN_POINT('Ctrl Pts',(-7.0689387628729,0.547113782458042,
-1.74117411869096));
#167328=CARTESIAN_POINT('Ctrl Pts',(-7.07363847126248,0.546330209621188,
-1.74237324466356));
#167329=CARTESIAN_POINT('Ctrl Pts',(-7.0783383568923,0.545548955854658,
-1.74357319394025));
#167330=CARTESIAN_POINT('Ctrl Pts',(-7.08303841523824,0.544770000053604,
-1.74477395507826));
#167331=CARTESIAN_POINT('Ctrl Pts',(-7.03920344700001,0.55233793,-1.735544534));
#167332=CARTESIAN_POINT('Ctrl Pts',(-7.077344024,0.526068113,-1.580849986));
#167333=CARTESIAN_POINT('Ctrl Pts',(-7.108651881,0.49968693,-1.424629229));
#167334=CARTESIAN_POINT('Ctrl Pts',(-7.072050472,0.55233793,-1.789888972));
#167335=CARTESIAN_POINT('Ctrl Pts',(-7.11138533,0.526068113,-1.634472573));
#167336=CARTESIAN_POINT('Ctrl Pts',(-7.143854603,0.49968693,-1.477478196));
#167337=CARTESIAN_POINT('Origin',(0.195602985683564,0.410743067885095,0.0241713514715394));
#167338=CARTESIAN_POINT('Ctrl Pts',(-7.10202741463771,0.552548454735263,
-1.69864285574175));
#167339=CARTESIAN_POINT('Ctrl Pts',(-7.10239734631885,0.552287640367631,
-1.69709318237088));
#167340=CARTESIAN_POINT('Ctrl Pts',(-7.102767278,0.552026826,-1.695543509));
#167341=CARTESIAN_POINT('Ctrl Pts',(-7.139808047,0.525911829,-1.540376768));
#167342=CARTESIAN_POINT('Ctrl Pts',(-7.17003718,0.49968693,-1.383740452));
#167343=CARTESIAN_POINT('Ctrl Pts',(-7.03888800934273,0.552548454735263,
-1.73679058026029));
#167344=CARTESIAN_POINT('Ctrl Pts',(-7.03926627005464,0.552287640367631,
-1.73525467894045));
#167345=CARTESIAN_POINT('Ctrl Pts',(-7.03964453076656,0.552026826,-1.73371877762062));
#167346=CARTESIAN_POINT('Ctrl Pts',(-7.07751927457942,0.525911829,-1.57993101384067));
#167347=CARTESIAN_POINT('Ctrl Pts',(-7.10864180914119,0.49968693,-1.42463593786997));
#167348=CARTESIAN_POINT('',(-7.13357158119885,0.552026824384635,-1.67691374278907));
#167349=CARTESIAN_POINT('Ctrl Pts',(-7.03777679268802,0.550751630586317,
-1.74133842106059));
#167350=CARTESIAN_POINT('Ctrl Pts',(-7.03871583934401,0.551389228293159,
-1.73752546803029));
#167351=CARTESIAN_POINT('Ctrl Pts',(-7.039654886,0.552026826,-1.733712515));
#167352=CARTESIAN_POINT('Ctrl Pts',(-7.134100011,0.61615356,-1.350222703));
#167353=CARTESIAN_POINT('Ctrl Pts',(-7.186328152,0.681389364000001,-0.958742768));
#167354=CARTESIAN_POINT('Ctrl Pts',(-7.22573324546068,0.550751630586317,
-1.62794433293448));
#167355=CARTESIAN_POINT('Ctrl Pts',(-7.22661076323034,0.551389228293159,
-1.62402964196724));
#167356=CARTESIAN_POINT('Ctrl Pts',(-7.22748828100001,0.552026826,-1.620114951));
#167357=CARTESIAN_POINT('Ctrl Pts',(-7.315745105,0.61615356,-1.226392791));
#167358=CARTESIAN_POINT('Ctrl Pts',(-7.360710034,0.681389364000001,-0.825413289));
#167359=CARTESIAN_POINT('Ctrl Pts',(-7.18570192502824,0.680609082247603,
-0.963425208969651));
#167360=CARTESIAN_POINT('Ctrl Pts',(-7.20364312653453,0.677652752724234,
-0.965650551686538));
#167361=CARTESIAN_POINT('Ctrl Pts',(-7.22158979302487,0.674729896867849,
-0.967876707642936));
#167362=CARTESIAN_POINT('Ctrl Pts',(-7.23953914972131,0.671836782501652,
-0.970119462776265));
#167363=CARTESIAN_POINT('Ctrl Pts',(-7.25634249050251,0.669128385346457,
-0.972219024305487));
#167364=CARTESIAN_POINT('Ctrl Pts',(-7.27314885172766,0.666446714465226,
-0.974329074620163));
#167365=CARTESIAN_POINT('Ctrl Pts',(-7.28995801424599,0.663790956117991,
-0.976449177968538));
#167366=CARTESIAN_POINT('Ctrl Pts',(-7.30676735723696,0.661135169257037,
-0.978569304079536));
#167367=CARTESIAN_POINT('Ctrl Pts',(-7.32357954629348,0.658505288575763,
-0.980699489225385));
#167368=CARTESIAN_POINT('Ctrl Pts',(-7.34039437668371,0.655900535573722,
-0.98283932438691));
#167369=CARTESIAN_POINT('Ctrl Pts',(-7.18507635,0.681369595,-0.968079464000001));
#167370=CARTESIAN_POINT('Ctrl Pts',(-7.186230154,0.679970133,-0.959515940000001));
#167371=CARTESIAN_POINT('Ctrl Pts',(-7.187363542,0.678571429,-0.95094969));
#167372=CARTESIAN_POINT('Ctrl Pts',(-7.238160861,0.615882895,-0.567018973000001));
#167373=CARTESIAN_POINT('Ctrl Pts',(-7.247768609,0.552026826,-0.17986157));
#167374=CARTESIAN_POINT('Ctrl Pts',(-7.318179135,0.681369595,-1.14263444));
#167375=CARTESIAN_POINT('Ctrl Pts',(-7.319540982,0.679970133,-1.133912278));
#167376=CARTESIAN_POINT('Ctrl Pts',(-7.320882034,0.678571429,-1.125186894));
#167377=CARTESIAN_POINT('Ctrl Pts',(-7.38098666200001,0.615882895,-0.734123958000001));
#167378=CARTESIAN_POINT('Ctrl Pts',(-7.399088954,0.552026826,-0.338883407));
#167379=CARTESIAN_POINT('',(-7.27319057621652,0.552026824384633,-0.206577405480668));
#167380=CARTESIAN_POINT('Ctrl Pts',(-7.281022233,0.499686101,-0.557571548));
#167381=CARTESIAN_POINT('Ctrl Pts',(-7.289553152,0.51775868,-0.446170941));
#167382=CARTESIAN_POINT('Ctrl Pts',(-7.294671987,0.535714286,-0.334561492));
#167383=CARTESIAN_POINT('Ctrl Pts',(-7.296993635,0.54385805,-0.283941029));
#167384=CARTESIAN_POINT('Ctrl Pts',(-7.298612544,0.552026826,-0.233293221));
#167385=CARTESIAN_POINT('Ctrl Pts',(-7.232604243,0.499686101,-0.501932126));
#167386=CARTESIAN_POINT('Ctrl Pts',(-7.240283871,0.51775868,-0.391272321));
#167387=CARTESIAN_POINT('Ctrl Pts',(-7.244574478,0.535714286,-0.28042937));
#167388=CARTESIAN_POINT('Ctrl Pts',(-7.246520483,0.54385805,-0.230156553));
#167389=CARTESIAN_POINT('Ctrl Pts',(-7.247768609,0.552026826,-0.17986157));
#167390=CARTESIAN_POINT('Ctrl Pts',(-7.24776860911075,0.552026825539334,
-0.179861574560902));
#167391=CARTESIAN_POINT('Ctrl Pts',(-7.24693591438939,0.546576979279491,
-0.213416164634367));
#167392=CARTESIAN_POINT('Ctrl Pts',(-7.24587080090455,0.541139220024475,
-0.246940346863208));
#167393=CARTESIAN_POINT('Ctrl Pts',(-7.24457447812535,0.535714285988153,
-0.280429369954506));
#167394=CARTESIAN_POINT('Ctrl Pts',(-7.24174375852935,0.52386810879308,
-0.35355779757423));
#167395=CARTESIAN_POINT('Ctrl Pts',(-7.23780069555822,0.511960760818452,
-0.426768191841702));
#167396=CARTESIAN_POINT('Ctrl Pts',(-7.23273737687419,0.499999999575121,
-0.500010032745376));
#167397=CARTESIAN_POINT('Ctrl Pts',(-7.232604243,0.499686101,-0.501932126));
#167398=CARTESIAN_POINT('Ctrl Pts',(-7.240283871,0.51775868,-0.391272321));
#167399=CARTESIAN_POINT('Ctrl Pts',(-7.244574478,0.535714286,-0.28042937));
#167400=CARTESIAN_POINT('Ctrl Pts',(-7.246557685,0.544013736,-0.22919548));
#167401=CARTESIAN_POINT('Ctrl Pts',(-7.247816073,0.552339147,-0.177938666));
#167402=CARTESIAN_POINT('Ctrl Pts',(-7.28050636400001,0.499686101,-0.460247214));
#167403=CARTESIAN_POINT('Ctrl Pts',(-7.287548207,0.51775868,-0.348854501));
#167404=CARTESIAN_POINT('Ctrl Pts',(-7.291178906,0.535714286,-0.237298496));
#167405=CARTESIAN_POINT('Ctrl Pts',(-7.292857089,0.544013736,-0.185735018));
#167406=CARTESIAN_POINT('Ctrl Pts',(-7.293805824,0.552339147,-0.134152962));
#167407=CARTESIAN_POINT('Ctrl Pts',(-7.24776860938908,0.552026827360936,
-0.179861563345339));
#167408=CARTESIAN_POINT('Ctrl Pts',(-7.25298869621631,0.551172308315565,
-0.180031302772311));
#167409=CARTESIAN_POINT('Ctrl Pts',(-7.25820919857855,0.550320534990502,
-0.180201945437676));
#167410=CARTESIAN_POINT('Ctrl Pts',(-7.26343011242881,0.549471478090142,
-0.180373486544556));
#167411=CARTESIAN_POINT('Ctrl Pts',(-7.26827701119779,0.548683245806835,
-0.180532738814102));
#167412=CARTESIAN_POINT('Ctrl Pts',(-7.27312426591151,0.547897354487421,
-0.180692765451291));
#167413=CARTESIAN_POINT('Ctrl Pts',(-7.27797186947297,0.547113782434519,
-0.180853558004141));
#167414=CARTESIAN_POINT('Ctrl Pts',(-7.28281947793267,0.546330209589859,
-0.181014350719461));
#167415=CARTESIAN_POINT('Ctrl Pts',(-7.28766743646369,0.545548955819146,
-0.18117590939348));
#167416=CARTESIAN_POINT('Ctrl Pts',(-7.29251573835091,0.544769999940509,
-0.181338224129734));
#167417=CARTESIAN_POINT('Ctrl Pts',(-7.247721555,0.55233793,-0.181747804));
#167418=CARTESIAN_POINT('Ctrl Pts',(-7.251715671,0.526068113,-0.022470832));
#167419=CARTESIAN_POINT('Ctrl Pts',(-7.248708723,0.49968693,0.136827835));
#167420=CARTESIAN_POINT('Ctrl Pts',(-7.291483082,0.55233793,-0.22776056));
#167421=CARTESIAN_POINT('Ctrl Pts',(-7.296488381,0.526068113,-0.067521878));
#167422=CARTESIAN_POINT('Ctrl Pts',(-7.294449391,0.49968693,0.092781992));
#167423=CARTESIAN_POINT('Origin',(0.196226715612283,0.410743175436658,-0.0184426066818074));
#167424=CARTESIAN_POINT('Ctrl Pts',(-7.30114396216113,0.552548454735263,
-0.132203570485142));
#167425=CARTESIAN_POINT('Ctrl Pts',(-7.30117211108057,0.552287640367631,
-0.130610603242571));
#167426=CARTESIAN_POINT('Ctrl Pts',(-7.30120026,0.552026826,-0.129017636));
#167427=CARTESIAN_POINT('Ctrl Pts',(-7.304018774,0.525911829,0.030484063));
#167428=CARTESIAN_POINT('Ctrl Pts',(-7.299868989,0.49968693,0.18995668));
#167429=CARTESIAN_POINT('Ctrl Pts',(-7.24768135452721,0.552548454735263,
-0.183032527619515));
#167430=CARTESIAN_POINT('Ctrl Pts',(-7.24772059833278,0.552287640367631,
-0.181451219949218));
#167431=CARTESIAN_POINT('Ctrl Pts',(-7.24775984213834,0.552026826,-0.179869912278921));
#167432=CARTESIAN_POINT('Ctrl Pts',(-7.25168927238334,0.525911829,-0.0215356707994777));
#167433=CARTESIAN_POINT('Ctrl Pts',(-7.24870032881853,0.49968693,0.13681911782159));
#167434=CARTESIAN_POINT('',(-7.32727952735701,0.552026824384635,-0.104201408054877));
#167435=CARTESIAN_POINT('Ctrl Pts',(-7.24757376884405,0.550751630586317,
-0.187712921172618));
#167436=CARTESIAN_POINT('Ctrl Pts',(-7.24767118892203,0.551389228293159,
-0.183787245586309));
#167437=CARTESIAN_POINT('Ctrl Pts',(-7.247768609,0.552026826,-0.17986157));
#167438=CARTESIAN_POINT('Ctrl Pts',(-7.257566686,0.61615356,0.214965374));
#167439=CARTESIAN_POINT('Ctrl Pts',(-7.224417148,0.681389364000001,0.608520231));
#167440=CARTESIAN_POINT('Ctrl Pts',(-7.40675952790616,0.550751630586317,
-0.0365648420981692));
#167441=CARTESIAN_POINT('Ctrl Pts',(-7.40677498695308,0.551389228293159,
-0.0325530340490846));
#167442=CARTESIAN_POINT('Ctrl Pts',(-7.406790446,0.552026826,-0.028541226));
#167443=CARTESIAN_POINT('Ctrl Pts',(-7.408345248,0.61615356,0.374948537));
#167444=CARTESIAN_POINT('Ctrl Pts',(-7.366060182,0.681389364000001,0.776219491));
#167445=CARTESIAN_POINT('Ctrl Pts',(-7.22481214824486,0.680609082247605,
0.603812642854019));
#167446=CARTESIAN_POINT('Ctrl Pts',(-7.24281227785518,0.677652752599059,
0.605496154954779));
#167447=CARTESIAN_POINT('Ctrl Pts',(-7.26081791900121,0.674729896792423,
0.607180048451818));
#167448=CARTESIAN_POINT('Ctrl Pts',(-7.27882975580833,0.671836782432773,
0.608848308897028));
#167449=CARTESIAN_POINT('Ctrl Pts',(-7.29569158745369,0.669128385294513,
0.610410055601098));
#167450=CARTESIAN_POINT('Ctrl Pts',(-7.31255862370623,0.666446714429166,
0.611962208038781));
#167451=CARTESIAN_POINT('Ctrl Pts',(-7.32943055686501,0.663790956096888,
0.613505144663944));
#167452=CARTESIAN_POINT('Ctrl Pts',(-7.34630267117038,0.661135169250888,
0.615048097854947));
#167453=CARTESIAN_POINT('Ctrl Pts',(-7.36317972739769,0.658505288583637,
0.616581838997317));
#167454=CARTESIAN_POINT('Ctrl Pts',(-7.38006143764124,0.655900535683362,
0.618106723046989));
#167455=CARTESIAN_POINT('Ctrl Pts',(-7.225201726,0.681369595,0.599132722));
#167456=CARTESIAN_POINT('Ctrl Pts',(-7.22448765,0.679970133000001,0.607744069));
#167457=CARTESIAN_POINT('Ctrl Pts',(-7.22375305,0.678571429,0.616353689));
#167458=CARTESIAN_POINT('Ctrl Pts',(-7.190829,0.615882895,1.002228242));
#167459=CARTESIAN_POINT('Ctrl Pts',(-7.116984728,0.552026826,1.382399502));
#167460=CARTESIAN_POINT('Ctrl Pts',(-7.392716802,0.681369595,0.457271909));
#167461=CARTESIAN_POINT('Ctrl Pts',(-7.39217180299999,0.679970133000001,
0.466082908));
#167462=CARTESIAN_POINT('Ctrl Pts',(-7.391605803,0.678571429,0.474892584));
#167463=CARTESIAN_POINT('Ctrl Pts',(-7.366238246,0.615882895,0.869733404));
#167464=CARTESIAN_POINT('Ctrl Pts',(-7.298952281,0.552026826,1.259624909));
#167465=CARTESIAN_POINT('',(-7.1475554583687,0.552026824384634,1.36177323919174));
#167466=CARTESIAN_POINT('Ctrl Pts',(-7.230657381,0.499686101,1.02066872));
#167467=CARTESIAN_POINT('Ctrl Pts',(-7.215041014,0.51775868,1.131298737));
#167468=CARTESIAN_POINT('Ctrl Pts',(-7.196047441,0.535714286,1.241399218));
#167469=CARTESIAN_POINT('Ctrl Pts',(-7.187432907,0.54385805,1.291335288));
#167470=CARTESIAN_POINT('Ctrl Pts',(-7.178126185,0.552026826,1.341146996));
#167471=CARTESIAN_POINT('Ctrl Pts',(-7.171410545,0.499686101,1.064598886));
#167472=CARTESIAN_POINT('Ctrl Pts',(-7.155122041,0.51775868,1.174322419));
#167473=CARTESIAN_POINT('Ctrl Pts',(-7.135484378,0.535714286,1.283496277));
#167474=CARTESIAN_POINT('Ctrl Pts',(-7.126577716,0.54385805,1.333012078));
#167475=CARTESIAN_POINT('Ctrl Pts',(-7.116984728,0.552026826,1.382399502));
#167476=CARTESIAN_POINT('Ctrl Pts',(-7.11698472856132,0.552026826,1.38239950162127));
#167477=CARTESIAN_POINT('Ctrl Pts',(-7.1271681177084,0.54335530340197,1.32997253191968));
#167478=CARTESIAN_POINT('Ctrl Pts',(-7.13676382120383,0.534726110048207,
1.27747872812076));
#167479=CARTESIAN_POINT('Ctrl Pts',(-7.15481559744862,0.517398614706748,
1.17216567942275));
#167480=CARTESIAN_POINT('Ctrl Pts',(-7.16326323260566,0.508709450442465,
1.11938277393001));
#167481=CARTESIAN_POINT('Ctrl Pts',(-7.17112737305294,0.499999999526768,
1.06650466127345));
#167482=CARTESIAN_POINT('Ctrl Pts',(-7.171410545,0.499686101,1.064598886));
#167483=CARTESIAN_POINT('Ctrl Pts',(-7.155122041,0.51775868,1.174322419));
#167484=CARTESIAN_POINT('Ctrl Pts',(-7.135484378,0.535714286,1.283496277));
#167485=CARTESIAN_POINT('Ctrl Pts',(-7.126407446,0.544013736,1.333958678));
#167486=CARTESIAN_POINT('Ctrl Pts',(-7.11661771399999,0.552339147,1.384287653));
#167487=CARTESIAN_POINT('Ctrl Pts',(-7.209231717,0.499686101,1.115606768));
#167488=CARTESIAN_POINT('Ctrl Pts',(-7.192162786,0.51775868,1.22590897));
#167489=CARTESIAN_POINT('Ctrl Pts',(-7.171727357,0.535714286,1.33563735));
#167490=CARTESIAN_POINT('Ctrl Pts',(-7.162281682,0.544013736,1.386356063));
#167491=CARTESIAN_POINT('Ctrl Pts',(-7.152119618,0.552339147,1.436936109));
#167492=CARTESIAN_POINT('Ctrl Pts',(-7.11698472626396,0.552026827255857,
1.38239950799491));
#167493=CARTESIAN_POINT('Ctrl Pts',(-7.1221192597115,0.551172308251233,
1.38335590228193));
#167494=CARTESIAN_POINT('Ctrl Pts',(-7.12725439282643,0.550320534923491,
1.38431150292089));
#167495=CARTESIAN_POINT('Ctrl Pts',(-7.13239012095014,0.549471478020002,
1.38526631456333));
#167496=CARTESIAN_POINT('Ctrl Pts',(-7.13715793640245,0.548683245752477,
1.38615272552458));
#167497=CARTESIAN_POINT('Ctrl Pts',(-7.14192626594669,0.547897354448274,
1.3870384567244));
#167498=CARTESIAN_POINT('Ctrl Pts',(-7.146695100838,0.547113782408566,1.38792351489902));
#167499=CARTESIAN_POINT('Ctrl Pts',(-7.15146394053894,0.546330209578583,
1.38880857396627));
#167500=CARTESIAN_POINT('Ctrl Pts',(-7.15623328679112,0.545548955820519,
1.38969296022934));
#167501=CARTESIAN_POINT('Ctrl Pts',(-7.16100313085534,0.544769999895332,
1.39057668139717));
#167502=CARTESIAN_POINT('Ctrl Pts',(-7.117344258,0.55233793,1.380547252));
#167503=CARTESIAN_POINT('Ctrl Pts',(-7.087005153,0.526068113,1.536959034));
#167504=CARTESIAN_POINT('Ctrl Pts',(-7.049824001,0.49968693,1.691886981));
#167505=CARTESIAN_POINT('Ctrl Pts',(-7.169974048,0.55233793,1.345017684));
#167506=CARTESIAN_POINT('Ctrl Pts',(-7.140415745,0.526068113,1.502586065));
#167507=CARTESIAN_POINT('Ctrl Pts',(-7.103963832,0.49968693,1.658703797));
#167508=CARTESIAN_POINT('Origin',(0.187673976996539,0.410743035001748,-0.0601943055948376));
#167509=CARTESIAN_POINT('Ctrl Pts',(-7.15886713411727,0.552548454735263,
1.44041740752365));
#167510=CARTESIAN_POINT('Ctrl Pts',(-7.15855218405863,0.552287640367631,
1.44197918326182));
#167511=CARTESIAN_POINT('Ctrl Pts',(-7.158237234,0.552026826,1.443540959));
#167512=CARTESIAN_POINT('Ctrl Pts',(-7.126701702,0.525911829,1.599919494));
#167513=CARTESIAN_POINT('Ctrl Pts',(-7.088367037,0.49968693,1.754771648));
#167514=CARTESIAN_POINT('Ctrl Pts',(-7.11758117562899,0.552548454735263,
1.37928392241786));
#167515=CARTESIAN_POINT('Ctrl Pts',(-7.11727956752418,0.552287640367631,
1.38083669626055));
#167516=CARTESIAN_POINT('Ctrl Pts',(-7.11697795941937,0.552026826,1.38238947010324));
#167517=CARTESIAN_POINT('Ctrl Pts',(-7.08677833957566,0.525911829,1.53786665723719));
#167518=CARTESIAN_POINT('Ctrl Pts',(-7.04981767698064,0.49968693,1.69187666308286));
#167519=CARTESIAN_POINT('',(-7.17837202652185,0.552026824384635,1.47338326864946));
#167520=CARTESIAN_POINT('Ctrl Pts',(-7.11848153267414,0.550751630586317,
1.37468876324479));
#167521=CARTESIAN_POINT('Ctrl Pts',(-7.11773277148763,0.551389228293159,
1.37854360076192));
#167522=CARTESIAN_POINT('Ctrl Pts',(-7.11698401030112,0.552026826,1.38239843827904));
#167523=CARTESIAN_POINT('Ctrl Pts',(-7.04167694924802,0.61615356,1.77010080518193));
#167524=CARTESIAN_POINT('Ctrl Pts',(-6.9246998300991,0.681389364000001,
2.14732836561089));
#167525=CARTESIAN_POINT('Ctrl Pts',(-7.24145396603117,0.550751630586317,
1.55652438013174));
#167526=CARTESIAN_POINT('Ctrl Pts',(-7.24060664351558,0.551389228293159,
1.56044571756587));
#167527=CARTESIAN_POINT('Ctrl Pts',(-7.239759321,0.552026826,1.564367055));
#167528=CARTESIAN_POINT('Ctrl Pts',(-7.15453940100001,0.61615356,1.958757687));
#167529=CARTESIAN_POINT('Ctrl Pts',(-7.026981543,0.681389364000001,2.341557111));
#167530=CARTESIAN_POINT('Ctrl Pts',(-6.92609818588287,0.680609082082805,
2.14281688694626));
#167531=CARTESIAN_POINT('Ctrl Pts',(-6.94331557651135,0.67765275266803,
2.14833053518668));
#167532=CARTESIAN_POINT('Ctrl Pts',(-6.96053826846024,0.674729896853169,
2.15384574070214));
#167533=CARTESIAN_POINT('Ctrl Pts',(-6.97777037186197,0.671836782485758,
2.15934701054552));
#167534=CARTESIAN_POINT('Ctrl Pts',(-6.99390225394025,0.669128385331562,
2.16449703978601));
#167535=CARTESIAN_POINT('Ctrl Pts',(-7.01004128142473,0.666446714452519,
2.16963881791848));
#167536=CARTESIAN_POINT('Ctrl Pts',(-7.02618707245249,0.663790956108138,
2.17477264840016));
#167537=CARTESIAN_POINT('Ctrl Pts',(-7.04233303683055,0.661135169250039,
2.17990653400152));
#167538=CARTESIAN_POINT('Ctrl Pts',(-7.05848580790602,0.658505288572285,
2.18503248530502));
#167539=CARTESIAN_POINT('Ctrl Pts',(-7.07464502826342,0.655900535710891,
2.19015078679768));
#167540=CARTESIAN_POINT('Ctrl Pts',(-6.9274847,0.681369595,2.138330128));
#167541=CARTESIAN_POINT('Ctrl Pts',(-6.924936134,0.679970133,2.146586641));
#167542=CARTESIAN_POINT('Ctrl Pts',(-6.922367894,0.678571429,2.154837056));
#167543=CARTESIAN_POINT('Ctrl Pts',(-6.807261968,0.615882895,2.524612378));
#167544=CARTESIAN_POINT('Ctrl Pts',(-6.65341854999999,0.552026826,2.88002111));
#167545=CARTESIAN_POINT('Ctrl Pts',(-7.12157924800001,0.681369595,2.035796731));
#167546=CARTESIAN_POINT('Ctrl Pts',(-7.119152886,0.679970133,2.044284575));
#167547=CARTESIAN_POINT('Ctrl Pts',(-7.116706299,0.678571429,2.052766612));
#167548=CARTESIAN_POINT('Ctrl Pts',(-7.007052717,0.615882895,2.432922999));
#167549=CARTESIAN_POINT('Ctrl Pts',(-6.857524711,0.552026826,2.799234563));
#167550=CARTESIAN_POINT('',(-6.68770859093351,0.55202682438463,2.86644888132274));
#167551=CARTESIAN_POINT('Ctrl Pts',(-6.842195025,0.499686101,2.551183652));
#167552=CARTESIAN_POINT('Ctrl Pts',(-6.803161577,0.51775868,2.655870144));
#167553=CARTESIAN_POINT('Ctrl Pts',(-6.760943714,0.535714286,2.759313481));
#167554=CARTESIAN_POINT('Ctrl Pts',(-6.741795804,0.54385805,2.806230203));
#167555=CARTESIAN_POINT('Ctrl Pts',(-6.721998624,0.552026826000001,2.852876671));
#167556=CARTESIAN_POINT('Ctrl Pts',(-6.774889661,0.499686101,2.581350438));
#167557=CARTESIAN_POINT('Ctrl Pts',(-6.735394657,0.51775868,2.685007149));
#167558=CARTESIAN_POINT('Ctrl Pts',(-6.692746959,0.535714286,2.787407065));
#167559=CARTESIAN_POINT('Ctrl Pts',(-6.673404096,0.54385805,2.833850545));
#167560=CARTESIAN_POINT('Ctrl Pts',(-6.65341855,0.552026826000001,2.88002111));
#167561=CARTESIAN_POINT('Ctrl Pts',(-6.65341855027456,0.552026826354219,
2.88002111045043));
#167562=CARTESIAN_POINT('Ctrl Pts',(-6.66675202404212,0.546576979816255,
2.84921814757175));
#167563=CARTESIAN_POINT('Ctrl Pts',(-6.67986179275827,0.541139220289782,
2.81834519245283));
#167564=CARTESIAN_POINT('Ctrl Pts',(-6.69274695885586,0.535714286060686,
2.78740706534609));
#167565=CARTESIAN_POINT('Ctrl Pts',(-6.72088369664735,0.523868109091399,
2.71984891517481));
#167566=CARTESIAN_POINT('Ctrl Pts',(-6.74804531683569,0.51196076095622,
2.65174931160051));
#167567=CARTESIAN_POINT('Ctrl Pts',(-6.77420342353812,0.499999999786669,
2.58315078520083));
#167568=CARTESIAN_POINT('Ctrl Pts',(-6.774889661,0.499686101,2.581350438));
#167569=CARTESIAN_POINT('Ctrl Pts',(-6.735394657,0.51775868,2.685007149));
#167570=CARTESIAN_POINT('Ctrl Pts',(-6.692746959,0.535714286,2.787407065));
#167571=CARTESIAN_POINT('Ctrl Pts',(-6.673034316,0.544013736,2.834738411));
#167572=CARTESIAN_POINT('Ctrl Pts',(-6.652654221,0.552339147,2.88178622));
#167573=CARTESIAN_POINT('Ctrl Pts',(-6.800861408,0.499686101,2.639296217));
#167574=CARTESIAN_POINT('Ctrl Pts',(-6.760479825,0.51775868,2.743350299));
#167575=CARTESIAN_POINT('Ctrl Pts',(-6.716933807,0.535714286,2.846120278));
#167576=CARTESIAN_POINT('Ctrl Pts',(-6.696805943,0.544013736,2.893622674));
#167577=CARTESIAN_POINT('Ctrl Pts',(-6.676008248,0.552339147,2.940835644));
#167578=CARTESIAN_POINT('Ctrl Pts',(-6.65341854774275,0.552026827389055,
2.8800211162994));
#167579=CARTESIAN_POINT('Ctrl Pts',(-6.65822744166486,0.551172308368387,
2.88205892227521));
#167580=CARTESIAN_POINT('Ctrl Pts',(-6.66303709220779,0.550320535046825,
2.88409608323122));
#167581=CARTESIAN_POINT('Ctrl Pts',(-6.66784749345554,0.549471478151479,
2.88613260155777));
#167582=CARTESIAN_POINT('Ctrl Pts',(-6.67231328794614,0.548683245858544,
2.88802322810935));
#167583=CARTESIAN_POINT('Ctrl Pts',(-6.67677973063417,0.547897354530828,
2.8899133013166));
#167584=CARTESIAN_POINT('Ctrl Pts',(-6.68124681152564,0.547113782469392,
2.89180282587923));
#167585=CARTESIAN_POINT('Ctrl Pts',(-6.68571389693085,0.5463302096162,2.89369235235111));
#167586=CARTESIAN_POINT('Ctrl Pts',(-6.69018162166811,0.545548955836741,
2.89558133065308));
#167587=CARTESIAN_POINT('Ctrl Pts',(-6.6946499753884,0.54476999999312,2.89746976725727));
#167588=CARTESIAN_POINT('Ctrl Pts',(-6.654167854,0.55233793,2.878289453));
#167589=CARTESIAN_POINT('Ctrl Pts',(-6.59091415000001,0.526068113,3.024522403));
#167590=CARTESIAN_POINT('Ctrl Pts',(-6.521297344,0.49968693,3.167835372));
#167591=CARTESIAN_POINT('Ctrl Pts',(-6.71320499500001,0.55233793,2.854904395));
#167592=CARTESIAN_POINT('Ctrl Pts',(-6.650465205,0.526068113,3.002434754));
#167593=CARTESIAN_POINT('Ctrl Pts',(-6.58130482,0.49968693,3.147066456));
#167594=CARTESIAN_POINT('Origin',(0.17034727884052,0.410743050246431,-0.0991318348672909));
#167595=CARTESIAN_POINT('Ctrl Pts',(-6.68184963465256,0.552548454735263,
2.94568606831802));
#167596=CARTESIAN_POINT('Ctrl Pts',(-6.68120631232628,0.552287640367631,
2.94714362565901));
#167597=CARTESIAN_POINT('Ctrl Pts',(-6.68056299,0.552026826,2.948601183));
#167598=CARTESIAN_POINT('Ctrl Pts',(-6.616147978,0.525911829,3.094544468));
#167599=CARTESIAN_POINT('Ctrl Pts',(-6.545420922,0.49968693,3.237535445));
#167600=CARTESIAN_POINT('Ctrl Pts',(-6.654670810517,0.552548454735263,2.87710658956354));
#167601=CARTESIAN_POINT('Ctrl Pts',(-6.65404245337249,0.552287640367631,
2.87855822358338));
#167602=CARTESIAN_POINT('Ctrl Pts',(-6.653414096228,0.552026826,2.88000985760322));
#167603=CARTESIAN_POINT('Ctrl Pts',(-6.59049752804749,0.525911829,3.02536004830619));
#167604=CARTESIAN_POINT('Ctrl Pts',(-6.52129338588128,0.49968693,3.16782393583724));
#167605=CARTESIAN_POINT('',(-6.69381182758831,0.552026824386152,2.98207418132302));
#167606=CARTESIAN_POINT('Ctrl Pts',(-6.65653794114433,0.550751630586317,
2.87281241291839));
#167607=CARTESIAN_POINT('Ctrl Pts',(-6.65497800947308,0.551389228293159,
2.87641616495792));
#167608=CARTESIAN_POINT('Ctrl Pts',(-6.65341807780182,0.552026826,2.88001991699745));
#167609=CARTESIAN_POINT('Ctrl Pts',(-6.49652710679142,0.61615356,3.24246922627415));
#167610=CARTESIAN_POINT('Ctrl Pts',(-6.30119207219073,0.681389364000001,
3.58573079276282));
#167611=CARTESIAN_POINT('Ctrl Pts',(-6.73754606545278,0.550751630586317,
3.07683225208979));
#167612=CARTESIAN_POINT('Ctrl Pts',(-6.7358755812264,0.551389228293159,
3.08047976154489));
#167613=CARTESIAN_POINT('Ctrl Pts',(-6.734205097,0.552026826,3.084127271));
#167614=CARTESIAN_POINT('Ctrl Pts',(-6.566195243,0.61615356,3.450977506));
#167615=CARTESIAN_POINT('Ctrl Pts',(-6.359329057,0.681389364000001,3.797406123));
#167616=CARTESIAN_POINT('Ctrl Pts',(-6.30352756992328,0.68060908208268,
3.58162539475483));
#167617=CARTESIAN_POINT('Ctrl Pts',(-6.31915715586046,0.677652752700977,
3.59071136724813));
#167618=CARTESIAN_POINT('Ctrl Pts',(-6.33479158467919,0.674729896894376,
3.59979999996222));
#167619=CARTESIAN_POINT('Ctrl Pts',(-6.35043820069918,0.671836782521917,
3.60887704594859));
#167620=CARTESIAN_POINT('Ctrl Pts',(-6.3650858243296,0.669128385358378,
3.61737454809949));
#167621=CARTESIAN_POINT('Ctrl Pts',(-6.37974220004862,0.666446714467875,
3.62586552810993));
#167622=CARTESIAN_POINT('Ctrl Pts',(-6.39440688968761,0.663790956110878,
3.63435020025209));
#167623=CARTESIAN_POINT('Ctrl Pts',(-6.40907173677491,0.661135169240174,
3.64283496349042));
#167624=CARTESIAN_POINT('Ctrl Pts',(-6.4237449370569,0.658505288548661,
3.65131344117807));
#167625=CARTESIAN_POINT('Ctrl Pts',(-6.43842607969659,0.655900535543649,
3.65978583507949));
#167626=CARTESIAN_POINT('Ctrl Pts',(-6.30584618800001,0.681369595,3.577541593));
#167627=CARTESIAN_POINT('Ctrl Pts',(-6.3015823,0.679970133,3.585057207));
#167628=CARTESIAN_POINT('Ctrl Pts',(-6.297300509,0.678571429,3.592562637));
#167629=CARTESIAN_POINT('Ctrl Pts',(-6.105394932,0.615882895,3.928948446));
#167630=CARTESIAN_POINT('Ctrl Pts',(-5.878745916,0.552026826,4.242976131));
#167631=CARTESIAN_POINT('Ctrl Pts',(-6.51744456300001,0.681369595,3.51912996));
#167632=CARTESIAN_POINT('Ctrl Pts',(-6.513250293,0.679970133,3.526897768));
#167633=CARTESIAN_POINT('Ctrl Pts',(-6.509037518,0.678571429,3.534655555));
#167634=CARTESIAN_POINT('Ctrl Pts',(-6.32022519000001,0.615882895,3.882351818));
#167635=CARTESIAN_POINT('Ctrl Pts',(-6.095446908,0.552026826,4.207955121));
#167636=CARTESIAN_POINT('',(-5.91515190281437,0.552026824384634,4.23709255888292));
#167637=CARTESIAN_POINT('Ctrl Pts',(-6.133799235,0.499686101,3.962408073));
#167638=CARTESIAN_POINT('Ctrl Pts',(-6.073173866,0.51775868,4.056256015));
#167639=CARTESIAN_POINT('Ctrl Pts',(-6.009705774,0.535714286,4.148205311));
#167640=CARTESIAN_POINT('Ctrl Pts',(-5.980919823,0.54385805,4.189908912));
#167641=CARTESIAN_POINT('Ctrl Pts',(-5.951557878,0.552026826,4.231209003));
#167642=CARTESIAN_POINT('Ctrl Pts',(-6.061582466,0.499686101,3.977400912));
#167643=CARTESIAN_POINT('Ctrl Pts',(-6.000727704,0.51775868,4.07014392800001));
#167644=CARTESIAN_POINT('Ctrl Pts',(-5.93706413,0.535714286,4.160981797));
#167645=CARTESIAN_POINT('Ctrl Pts',(-5.908189518,0.54385805,4.20218131));
#167646=CARTESIAN_POINT('Ctrl Pts',(-5.878745916,0.552026826,4.242976131));
#167647=CARTESIAN_POINT('Ctrl Pts',(-5.87874591253852,0.552026827331392,
4.24297613682539));
#167648=CARTESIAN_POINT('Ctrl Pts',(-5.90818951603908,0.543858051066734,
4.20218131293737));
#167649=CARTESIAN_POINT('Ctrl Pts',(-5.93706413,0.535714286,4.160981797));
#167650=CARTESIAN_POINT('Ctrl Pts',(-6.00017468145858,0.51791465388332,
4.07093300385634));
#167651=CARTESIAN_POINT('Ctrl Pts',(-6.06052525045423,0.499999999933982,
3.97901164806512));
#167652=CARTESIAN_POINT('Ctrl Pts',(-6.06052525045423,0.499999999933982,
3.97901164806512));
#167653=CARTESIAN_POINT('Ctrl Pts',(-6.00017468145858,0.51791465388332,
4.07093300385634));
#167654=CARTESIAN_POINT('Ctrl Pts',(-5.93706413,0.535714286,4.160981797));
#167655=CARTESIAN_POINT('Ctrl Pts',(-5.90818951603908,0.543858051066734,
4.20218131293737));
#167656=CARTESIAN_POINT('Ctrl Pts',(-5.87874591253852,0.552026827331392,
4.24297613682539));
#167657=CARTESIAN_POINT('Ctrl Pts',(-6.07333975208833,0.499999999933982,
4.0408184325369));
#167658=CARTESIAN_POINT('Ctrl Pts',(-6.01205174511351,0.51791465388332,
4.1329341489989));
#167659=CARTESIAN_POINT('Ctrl Pts',(-5.94799829402805,0.535714286,4.22314878315257));
#167660=CARTESIAN_POINT('Ctrl Pts',(-5.91869227907855,0.543858051066734,
4.26442417559135));
#167661=CARTESIAN_POINT('Ctrl Pts',(-5.88881626406081,0.552026827331392,
4.30528888183963));
#167662=CARTESIAN_POINT('Ctrl Pts',(-5.87874591253852,0.552026827331392,
4.24297613682539));
#167663=CARTESIAN_POINT('Ctrl Pts',(-5.88300430884132,0.551172308387581,
4.24600007043486));
#167664=CARTESIAN_POINT('Ctrl Pts',(-5.88726358305087,0.550320535056991,
4.24902353649116));
#167665=CARTESIAN_POINT('Ctrl Pts',(-5.89152372856485,0.549471478151584,
4.25204653631538));
#167666=CARTESIAN_POINT('Ctrl Pts',(-5.89547868642776,0.548683245854569,
4.25485297494176));
#167667=CARTESIAN_POINT('Ctrl Pts',(-5.89943439628991,0.547897354521786,
4.25765901249858));
#167668=CARTESIAN_POINT('Ctrl Pts',(-5.90339084739567,0.547113782454407,
4.26046465142468));
#167669=CARTESIAN_POINT('Ctrl Pts',(-5.90734730248218,0.546330209598645,
4.26327029317365));
#167670=CARTESIAN_POINT('Ctrl Pts',(-5.91130449981241,0.545548955815742,
4.2660755369981));
#167671=CARTESIAN_POINT('Ctrl Pts',(-5.91526242801923,0.544769999921413,
4.26888038644755));
#167672=CARTESIAN_POINT('Ctrl Pts',(-5.879849956,0.55233793,4.241446038));
#167673=CARTESIAN_POINT('Ctrl Pts',(-5.78663932800001,0.526068113,4.370662467));
#167674=CARTESIAN_POINT('Ctrl Pts',(-5.687842072,0.49968693,4.495659303));
#167675=CARTESIAN_POINT('Ctrl Pts',(-5.942533939,0.55233793,4.23129895));
#167676=CARTESIAN_POINT('Ctrl Pts',(-5.849546304,0.526068113,4.361892931));
#167677=CARTESIAN_POINT('Ctrl Pts',(-5.750911309,0.49968693,4.488275785));
#167678=CARTESIAN_POINT('Origin',(0.145053107207914,0.41074311058109,-0.133432913130858));
#167679=CARTESIAN_POINT('Ctrl Pts',(-5.8923962720813,0.552548454735263,
4.31321772265892));
#167680=CARTESIAN_POINT('Ctrl Pts',(-5.89145465854065,0.552287640367631,
4.31450290782946));
#167681=CARTESIAN_POINT('Ctrl Pts',(-5.890513045,0.552026826,4.315788093));
#167682=CARTESIAN_POINT('Ctrl Pts',(-5.796230529,0.525911829,4.444471981));
#167683=CARTESIAN_POINT('Ctrl Pts',(-5.696418198,0.49968693,4.568915682));
#167684=CARTESIAN_POINT('Ctrl Pts',(-5.88059543510538,0.552548454735263,
4.24039894946615));
#167685=CARTESIAN_POINT('Ctrl Pts',(-5.87966971019993,0.552287640367631,
4.24168156687897));
#167686=CARTESIAN_POINT('Ctrl Pts',(-5.87874398529449,0.552026826,4.24296418429179));
#167687=CARTESIAN_POINT('Ctrl Pts',(-5.78605237728176,0.525911829,4.37139096611371));
#167688=CARTESIAN_POINT('Ctrl Pts',(-5.68784066486205,0.49968693,4.49564728337354));
#167689=CARTESIAN_POINT('',(-5.89625642747112,0.552026824384635,4.35132661890885));
#167690=CARTESIAN_POINT('Ctrl Pts',(-5.88334203389657,0.550751630586317,
4.23660654365286));
#167691=CARTESIAN_POINT('Ctrl Pts',(-5.88104387239856,0.551389228293159,
4.23979070277515));
#167692=CARTESIAN_POINT('Ctrl Pts',(-5.87874571090055,0.552026826,4.24297486189745));
#167693=CARTESIAN_POINT('Ctrl Pts',(-5.64760687603574,0.61615356,4.56322338672453));
#167694=CARTESIAN_POINT('Ctrl Pts',(-5.38304757597552,0.681389364000001,
4.8564684301278));
#167695=CARTESIAN_POINT('Ctrl Pts',(-5.91859799888374,0.550751630586317,
4.45327086703888));
#167696=CARTESIAN_POINT('Ctrl Pts',(-5.91618246294187,0.551389228293159,
4.45647399501944));
#167697=CARTESIAN_POINT('Ctrl Pts',(-5.913766927,0.552026826,4.459677123));
#167698=CARTESIAN_POINT('Ctrl Pts',(-5.670823094,0.61615356,4.781833451));
#167699=CARTESIAN_POINT('Ctrl Pts',(-5.394321411,0.681389364000001,5.07569264400001));
#167700=CARTESIAN_POINT('Ctrl Pts',(-5.3862110102017,0.680609082082614,
4.85296107987893));
#167701=CARTESIAN_POINT('Ctrl Pts',(-5.39952197013657,0.677652752615266,
4.86519452629108));
#167702=CARTESIAN_POINT('Ctrl Pts',(-5.41283708726114,0.674729896815345,
4.87743161198875));
#167703=CARTESIAN_POINT('Ctrl Pts',(-5.42616659749073,0.671836782445242,
4.88966000170458));
#167704=CARTESIAN_POINT('Ctrl Pts',(-5.43864505594036,0.669128385299696,
4.90110764309173));
#167705=CARTESIAN_POINT('Ctrl Pts',(-5.45113346393363,0.666446714428098,
4.91255079625585));
#167706=CARTESIAN_POINT('Ctrl Pts',(-5.46363134748315,0.663790956090451,
4.92398957626689));
#167707=CARTESIAN_POINT('Ctrl Pts',(-5.47612936521697,0.661135169239089,
4.93542847909109));
#167708=CARTESIAN_POINT('Ctrl Pts',(-5.4886368920659,0.658505288567361,
4.94686303900093));
#167709=CARTESIAN_POINT('Ctrl Pts',(-5.50115348400725,0.655900535618631,
4.95829336454301));
#167710=CARTESIAN_POINT('Ctrl Pts',(-5.38935331700001,0.681369595,4.84947119));
#167711=CARTESIAN_POINT('Ctrl Pts',(-5.383573482,0.679970133,4.855894483));
#167712=CARTESIAN_POINT('Ctrl Pts',(-5.377778351,0.678571429,4.862303981));
#167713=CARTESIAN_POINT('Ctrl Pts',(-5.118046414,0.615882895,5.149571251));
#167714=CARTESIAN_POINT('Ctrl Pts',(-4.829189657,0.552026826,5.407534305));
#167715=CARTESIAN_POINT('Ctrl Pts',(-5.608561414,0.681369595,4.837912584));
#167716=CARTESIAN_POINT('Ctrl Pts',(-5.602795355,0.679970133,4.844597141));
#167717=CARTESIAN_POINT('Ctrl Pts',(-5.597013377,0.678571429,4.851267933));
#167718=CARTESIAN_POINT('Ctrl Pts',(-5.33787095800001,0.615882895,5.150246182));
#167719=CARTESIAN_POINT('Ctrl Pts',(-5.048352782,0.552026826,5.419916374));
#167720=CARTESIAN_POINT('',(-4.86600928592336,0.552026824384634,5.40961449782261));
#167721=CARTESIAN_POINT('Ctrl Pts',(-5.13859381,0.499686101,5.188354696));
#167722=CARTESIAN_POINT('Ctrl Pts',(-5.059211294,0.51775868,5.266975863));
#167723=CARTESIAN_POINT('Ctrl Pts',(-4.977460671,0.535714286,5.343131672));
#167724=CARTESIAN_POINT('Ctrl Pts',(-4.940382678,0.54385805,5.377672137));
#167725=CARTESIAN_POINT('Ctrl Pts',(-4.9028289,0.552026826,5.41169470400001));
#167726=CARTESIAN_POINT('Ctrl Pts',(-5.064842411,0.499686101,5.18747254));
#167727=CARTESIAN_POINT('Ctrl Pts',(-4.985473393,0.51775868,5.264965301));
#167728=CARTESIAN_POINT('Ctrl Pts',(-4.903770781,0.535714286,5.339993645));
#167729=CARTESIAN_POINT('Ctrl Pts',(-4.866714564,0.54385805,5.374022748));
#167730=CARTESIAN_POINT('Ctrl Pts',(-4.829189657,0.552026826,5.40753430500001));
#167731=CARTESIAN_POINT('Ctrl Pts',(-4.82918965683727,0.552026826325504,
5.40753430538259));
#167732=CARTESIAN_POINT('Ctrl Pts',(-4.85422461787804,0.546576979803602,
5.38517687395041));
#167733=CARTESIAN_POINT('Ctrl Pts',(-4.87908593870346,0.54113922028644,
5.36266198795457));
#167734=CARTESIAN_POINT('Ctrl Pts',(-4.90377078115005,0.535714285967023,
5.33999364486221));
#167735=CARTESIAN_POINT('Ctrl Pts',(-4.95767392528447,0.523868108781526,
5.29049383644694));
#167736=CARTESIAN_POINT('Ctrl Pts',(-5.01091942444511,0.511960760933383,
5.24009317944469));
#167737=CARTESIAN_POINT('Ctrl Pts',(-5.06346365273142,0.49999999975226,
5.18881834708339));
#167738=CARTESIAN_POINT('Ctrl Pts',(-5.064842411,0.499686101,5.18747254));
#167739=CARTESIAN_POINT('Ctrl Pts',(-4.985473393,0.51775868,5.264965301));
#167740=CARTESIAN_POINT('Ctrl Pts',(-4.903770781,0.535714286,5.339993645));
#167741=CARTESIAN_POINT('Ctrl Pts',(-4.866006155,0.544013736,5.374673287));
#167742=CARTESIAN_POINT('Ctrl Pts',(-4.82775482,0.552339147,5.408815342));
#167743=CARTESIAN_POINT('Ctrl Pts',(-5.064082929,0.499686101,5.250967958));
#167744=CARTESIAN_POINT('Ctrl Pts',(-4.983742422,0.51775868,5.328449099));
#167745=CARTESIAN_POINT('Ctrl Pts',(-4.901069133,0.535714286,5.403436108));
#167746=CARTESIAN_POINT('Ctrl Pts',(-4.862855839,0.544013736,5.438096644));
#167747=CARTESIAN_POINT('Ctrl Pts',(-4.824156151,0.552339147,5.472213249));
#167748=CARTESIAN_POINT('Ctrl Pts',(-4.82918965212967,0.5520268273503,5.4075343095867));
#167749=CARTESIAN_POINT('Ctrl Pts',(-4.8326984334768,0.551172308320109,
5.41140297452869));
#167750=CARTESIAN_POINT('Ctrl Pts',(-4.83620817239363,0.550320534982899,
5.41527137164601));
#167751=CARTESIAN_POINT('Ctrl Pts',(-4.83971886247769,0.549471478073663,
5.41913950073001));
#167752=CARTESIAN_POINT('Ctrl Pts',(-4.84297805423243,0.548683245785531,
5.42273052531918));
#167753=CARTESIAN_POINT('Ctrl Pts',(-4.84623806662961,0.547897354464017,
5.42632131986788));
#167754=CARTESIAN_POINT('Ctrl Pts',(-4.84949888862985,0.547113782411179,
5.42991188444141));
#167755=CARTESIAN_POINT('Ctrl Pts',(-4.85275971392499,0.546330209566579,
5.43350245264303));
#167756=CARTESIAN_POINT('Ctrl Pts',(-4.85602134964807,0.545548955798043,
5.43709279177419));
#167757=CARTESIAN_POINT('Ctrl Pts',(-4.85928378415849,0.544769999867977,
5.44068290297567));
#167758=CARTESIAN_POINT('Ctrl Pts',(-4.83059681,0.55233793,5.40627732));
#167759=CARTESIAN_POINT('Ctrl Pts',(-4.71178768100001,0.526068113,5.512435211));
#167760=CARTESIAN_POINT('Ctrl Pts',(-4.588429626,0.49968693,5.613271201));
#167761=CARTESIAN_POINT('Ctrl Pts',(-4.893996599,0.55233793,5.40984266800001));
#167762=CARTESIAN_POINT('Ctrl Pts',(-4.775109118,0.526068113,5.517393842));
#167763=CARTESIAN_POINT('Ctrl Pts',(-4.651611577,0.49968693,5.619618328));
#167764=CARTESIAN_POINT('Origin',(0.112978642611034,0.410742823000216,-0.161496613303563));
#167765=CARTESIAN_POINT('Ctrl Pts',(-4.82742100891798,0.552548454735263,
5.47906810964861));
#167766=CARTESIAN_POINT('Ctrl Pts',(-4.82622513295899,0.552287640367631,
5.48012082882431));
#167767=CARTESIAN_POINT('Ctrl Pts',(-4.825029257,0.552026826,5.481173548));
#167768=CARTESIAN_POINT('Ctrl Pts',(-4.705287782,0.525911829,5.586580924));
#167769=CARTESIAN_POINT('Ctrl Pts',(-4.581057291,0.49968693,5.68665850000001));
#167770=CARTESIAN_POINT('Ctrl Pts',(-4.83154995323541,0.552548454735263,
5.40541496848023));
#167771=CARTESIAN_POINT('Ctrl Pts',(-4.830370146429,0.552287640367631,5.40646859551687));
#167772=CARTESIAN_POINT('Ctrl Pts',(-4.82919033962259,0.552026826,5.4075222225535));
#167773=CARTESIAN_POINT('Ctrl Pts',(-4.71105784757507,0.525911829,5.51302050146606));
#167774=CARTESIAN_POINT('Ctrl Pts',(-4.58843083562465,0.49968693,5.61325915989151));
#167775=CARTESIAN_POINT('',(-4.82299863007088,0.552026824384634,5.51711586088163));
#167776=CARTESIAN_POINT('Ctrl Pts',(-4.83504759308386,0.550751630586317,
5.40230166699065));
#167777=CARTESIAN_POINT('Ctrl Pts',(-4.83211866123137,0.551389228293159,
5.40491734544072));
#167778=CARTESIAN_POINT('Ctrl Pts',(-4.82918972937888,0.552026826,5.4075330238908));
#167779=CARTESIAN_POINT('Ctrl Pts',(-4.53461082516816,0.61615356,5.67060629783368));
#167780=CARTESIAN_POINT('Ctrl Pts',(-4.21319775811611,0.681389364,5.90012300633437));
#167781=CARTESIAN_POINT('Ctrl Pts',(-4.82290286777508,0.550751630586317,
5.62147948639974));
#167782=CARTESIAN_POINT('Ctrl Pts',(-4.81985522788754,0.551389228293159,
5.62408845819987));
#167783=CARTESIAN_POINT('Ctrl Pts',(-4.816807588,0.552026826,5.62669743));
#167784=CARTESIAN_POINT('Ctrl Pts',(-4.510289559,0.61615356,5.889096179));
#167785=CARTESIAN_POINT('Ctrl Pts',(-4.177081292,0.681389364000001,6.116645419));
#167786=CARTESIAN_POINT('Ctrl Pts',(-4.21704120998561,0.680609082247451,
5.89737769848892));
#167787=CARTESIAN_POINT('Ctrl Pts',(-4.22741113718361,0.677652752732438,
5.91218659723743));
#167788=CARTESIAN_POINT('Ctrl Pts',(-4.2377843429517,0.674729896861193,
5.92699994298084));
#167789=CARTESIAN_POINT('Ctrl Pts',(-4.24817347433186,0.671836782492805,
5.94180789041485));
#167790=CARTESIAN_POINT('Ctrl Pts',(-4.25789928888653,0.669128385341709,
5.95567039204358));
#167791=CARTESIAN_POINT('Ctrl Pts',(-4.26763578519879,0.666446714464492,
5.96953064924376));
#167792=CARTESIAN_POINT('Ctrl Pts',(-4.27738247562702,0.663790956121092,
5.9833886725012));
#167793=CARTESIAN_POINT('Ctrl Pts',(-4.28712927070118,0.661135169263983,
5.99724684454615));
#167794=CARTESIAN_POINT('Ctrl Pts',(-4.29688628616516,0.658505288586374,
6.01110281939429));
#167795=CARTESIAN_POINT('Ctrl Pts',(-4.30665306547384,0.655900535733099,
6.02495660721441));
#167796=CARTESIAN_POINT('Ctrl Pts',(-4.220860275,0.681369595,5.89464490299999));
#167797=CARTESIAN_POINT('Ctrl Pts',(-4.213834751,0.679970133,5.89967553000001));
#167798=CARTESIAN_POINT('Ctrl Pts',(-4.206797255,0.678571429,5.904689396));
#167799=CARTESIAN_POINT('Ctrl Pts',(-3.891383734,0.615882895,6.129405827));
#167800=CARTESIAN_POINT('Ctrl Pts',(-3.553825856,0.552026826,6.319242184));
#167801=CARTESIAN_POINT('Ctrl Pts',(-4.437428167,0.681369595,5.930479793));
#167802=CARTESIAN_POINT('Ctrl Pts',(-4.430359933,0.679970133,5.935768535));
#167803=CARTESIAN_POINT('Ctrl Pts',(-4.423279112,0.678571429,5.941040415));
#167804=CARTESIAN_POINT('Ctrl Pts',(-4.105923812,0.615882895,6.177320758));
#167805=CARTESIAN_POINT('Ctrl Pts',(-3.765203291,0.552026826,6.378448361));
#167806=CARTESIAN_POINT('',(-3.58933748268525,0.552026824384634,6.32918887507452));
#167807=CARTESIAN_POINT('Ctrl Pts',(-3.903113449,0.499686101,6.17169962));
#167808=CARTESIAN_POINT('Ctrl Pts',(-3.808685626,0.51775868,6.231417774));
#167809=CARTESIAN_POINT('Ctrl Pts',(-3.712475039,0.535714286,6.288219134));
#167810=CARTESIAN_POINT('Ctrl Pts',(-3.668838729,0.54385805,6.31398139));
#167811=CARTESIAN_POINT('Ctrl Pts',(-3.624849092,0.552026826,6.339135576));
#167812=CARTESIAN_POINT('Ctrl Pts',(-3.831275955,0.499686101,6.154983717));
#167813=CARTESIAN_POINT('Ctrl Pts',(-3.737103887,0.51775868,6.213602748));
#167814=CARTESIAN_POINT('Ctrl Pts',(-3.641182561,0.535714286,6.269313324));
#167815=CARTESIAN_POINT('Ctrl Pts',(-3.597677446,0.54385805,6.294580855));
#167816=CARTESIAN_POINT('Ctrl Pts',(-3.553825856,0.552026826,6.319242184));
#167817=CARTESIAN_POINT('Ctrl Pts',(-3.55382585773626,0.552026826,6.31924218448633));
#167818=CARTESIAN_POINT('Ctrl Pts',(-3.60037628942064,0.543355303658993,
6.29306307716329));
#167819=CARTESIAN_POINT('Ctrl Pts',(-3.64659721603784,0.534726107585227,
6.26639278095636));
#167820=CARTESIAN_POINT('Ctrl Pts',(-3.73854930035679,0.517398611874174,
6.21197293578532));
#167821=CARTESIAN_POINT('Ctrl Pts',(-3.78424732666389,0.508709444526294,
6.184240463273));
#167822=CARTESIAN_POINT('Ctrl Pts',(-3.8296401228719,0.499999999696683,
6.15600166741686));
#167823=CARTESIAN_POINT('Ctrl Pts',(-3.831275955,0.499686101,6.154983717));
#167824=CARTESIAN_POINT('Ctrl Pts',(-3.737103887,0.51775868,6.213602748));
#167825=CARTESIAN_POINT('Ctrl Pts',(-3.641182561,0.535714286,6.269313324));
#167826=CARTESIAN_POINT('Ctrl Pts',(-3.596845753,0.544013736,6.295063898));
#167827=CARTESIAN_POINT('Ctrl Pts',(-3.55214918,0.552339147,6.320184824));
#167828=CARTESIAN_POINT('Ctrl Pts',(-3.816884591,0.499686101,6.216831382));
#167829=CARTESIAN_POINT('Ctrl Pts',(-3.721766245,0.51775868,6.275230223));
#167830=CARTESIAN_POINT('Ctrl Pts',(-3.624905821,0.535714286,6.330691763));
#167831=CARTESIAN_POINT('Ctrl Pts',(-3.580134942,0.544013736,6.356327227));
#167832=CARTESIAN_POINT('Ctrl Pts',(-3.53500597,0.552339147,6.381326915));
#167833=CARTESIAN_POINT('Ctrl Pts',(-3.55382585052444,0.552026827376882,
6.31924218800207));
#167834=CARTESIAN_POINT('Ctrl Pts',(-3.55642095025658,0.551172308303609,
6.32377468954546));
#167835=CARTESIAN_POINT('Ctrl Pts',(-3.55901704240399,0.550320534962719,
6.32830713585479));
#167836=CARTESIAN_POINT('Ctrl Pts',(-3.56161412108933,0.549471478046711,
6.33283952487593));
#167837=CARTESIAN_POINT('Ctrl Pts',(-3.56402515059284,0.548683245758558,
6.33704722320754));
#167838=CARTESIAN_POINT('Ctrl Pts',(-3.56643703099503,0.54789735443435,
6.34125487329571));
#167839=CARTESIAN_POINT('Ctrl Pts',(-3.56884975150297,0.547113782376603,
6.34546247282981));
#167840=CARTESIAN_POINT('Ctrl Pts',(-3.57126247444884,0.546330209527098,
6.34967007661546));
#167841=CARTESIAN_POINT('Ctrl Pts',(-3.57367603811166,0.545548955751532,
6.35387763090795));
#167842=CARTESIAN_POINT('Ctrl Pts',(-3.57609043026655,0.544769999930891,
6.35808513457863));
#167843=CARTESIAN_POINT('Ctrl Pts',(-3.555470326,0.55233793,6.318317083));
#167844=CARTESIAN_POINT('Ctrl Pts',(-3.41661808,0.526068113,6.39645261100001));
#167845=CARTESIAN_POINT('Ctrl Pts',(-3.27446731,0.49968693,6.468412776));
#167846=CARTESIAN_POINT('Ctrl Pts',(-3.616621419,0.55233793,6.335428156));
#167847=CARTESIAN_POINT('Ctrl Pts',(-3.477393138,0.526068113,6.414907549));
#167848=CARTESIAN_POINT('Ctrl Pts',(-3.334807658,0.49968693,6.488193762));
#167849=CARTESIAN_POINT('Origin',(0.075619904091393,0.410742926312177,-0.182007274607002));
#167850=CARTESIAN_POINT('Ctrl Pts',(-3.53672090509896,0.552548454735263,
6.38872336160058));
#167851=CARTESIAN_POINT('Ctrl Pts',(-3.53532668454948,0.552287640367631,
6.38949439080029));
#167852=CARTESIAN_POINT('Ctrl Pts',(-3.533932464,0.552026826,6.39026542));
#167853=CARTESIAN_POINT('Ctrl Pts',(-3.394331008,0.525911829,6.467467552));
#167854=CARTESIAN_POINT('Ctrl Pts',(-3.251491236,0.49968693,6.538499487));
#167855=CARTESIAN_POINT('Ctrl Pts',(-3.55658656450835,0.552548454735263,
6.31767979036095));
#167856=CARTESIAN_POINT('Ctrl Pts',(-3.55520784226221,0.552287640367631,
6.31845516059789));
#167857=CARTESIAN_POINT('Ctrl Pts',(-3.55382912001605,0.552026826,6.31923053083484));
#167858=CARTESIAN_POINT('Ctrl Pts',(-3.41577948859051,0.525911829,6.39686732514053));
#167859=CARTESIAN_POINT('Ctrl Pts',(-3.27447107980831,0.49968693,6.46840127649554));
#167860=CARTESIAN_POINT('',(-3.52422277681663,0.552026824384635,6.42493089616388));
#167861=CARTESIAN_POINT('Ctrl Pts',(-3.56067169923797,0.550751630586317,
6.31539116543644));
#167862=CARTESIAN_POINT('Ctrl Pts',(-3.55724895063607,0.551389228293159,
6.31731605701395));
#167863=CARTESIAN_POINT('Ctrl Pts',(-3.55382620203417,0.552026826,6.31924094859146));
#167864=CARTESIAN_POINT('Ctrl Pts',(-3.20958141133387,0.61615356,6.51283795944189));
#167865=CARTESIAN_POINT('Ctrl Pts',(-2.8463434961876,0.681389364000001,
6.66789438649148));
#167866=CARTESIAN_POINT('Ctrl Pts',(-3.5016941591658,0.550751630586317,
6.52683397198676));
#167867=CARTESIAN_POINT('Ctrl Pts',(-3.4981569195829,0.551389228293159,
6.52872679499338));
#167868=CARTESIAN_POINT('Ctrl Pts',(-3.49461968,0.552026826,6.530619618));
#167869=CARTESIAN_POINT('Ctrl Pts',(-3.138859897,0.61615356,6.720991315));
#167870=CARTESIAN_POINT('Ctrl Pts',(-2.764525494,0.681389364000001,6.871590653));
#167871=CARTESIAN_POINT('Ctrl Pts',(-2.85068725011335,0.680609082082589,
6.66603949042971));
#167872=CARTESIAN_POINT('Ctrl Pts',(-2.85763125915416,0.677652752703801,
6.68273139310465));
#167873=CARTESIAN_POINT('Ctrl Pts',(-2.8645775133876,0.67472989686154,6.69942834382325));
#167874=CARTESIAN_POINT('Ctrl Pts',(-2.87154048165055,0.6718367824759,6.71612344585627));
#167875=CARTESIAN_POINT('Ctrl Pts',(-2.8780588839478,0.669128385317478,
6.73175261251841));
#167876=CARTESIAN_POINT('Ctrl Pts',(-2.8845882007636,0.66644671443324,6.74738188348409));
#167877=CARTESIAN_POINT('Ctrl Pts',(-2.89112795360198,0.66379095608324,
6.76301116416583));
#167878=CARTESIAN_POINT('Ctrl Pts',(-2.89766777665485,0.661135169219524,
6.77864061265232));
#167879=CARTESIAN_POINT('Ctrl Pts',(-2.90421805349058,0.658505288535728,
6.79427011238982));
#167880=CARTESIAN_POINT('Ctrl Pts',(-2.91077833515283,0.655900535563285,
6.80989957534335));
#167881=CARTESIAN_POINT('Ctrl Pts',(-2.855004498,0.681369595,6.664191573));
#167882=CARTESIAN_POINT('Ctrl Pts',(-2.84706179,0.679970133,6.667594306));
#167883=CARTESIAN_POINT('Ctrl Pts',(-2.839110994,0.678571429,6.670978097));
#167884=CARTESIAN_POINT('Ctrl Pts',(-2.482764276,0.615882895,6.8226362));
#167885=CARTESIAN_POINT('Ctrl Pts',(-2.112289109,0.552026826,6.935469322));
#167886=CARTESIAN_POINT('Ctrl Pts',(-3.058805711,0.681369595,6.745744357));
#167887=CARTESIAN_POINT('Ctrl Pts',(-3.050765805,0.679970133,6.749389991));
#167888=CARTESIAN_POINT('Ctrl Pts',(-3.042717231,0.678571429,6.753016449));
#167889=CARTESIAN_POINT('Ctrl Pts',(-2.681988233,0.615882895,6.915550681));
#167890=CARTESIAN_POINT('Ctrl Pts',(-2.305997078,0.552026826,7.038731191));
#167891=CARTESIAN_POINT('',(-2.14483224854103,0.552026824384634,6.95281741505674));
#167892=CARTESIAN_POINT('Ctrl Pts',(-2.485127842,0.499686101,6.866462729));
#167893=CARTESIAN_POINT('Ctrl Pts',(-2.380070051,0.51775868,6.904485514));
#167894=CARTESIAN_POINT('Ctrl Pts',(-2.2738982,0.535714286,6.939276459));
#167895=CARTESIAN_POINT('Ctrl Pts',(-2.22574396,0.54385805,6.95505589100001));
#167896=CARTESIAN_POINT('Ctrl Pts',(-2.177375369,0.552026826,6.970165514));
#167897=CARTESIAN_POINT('Ctrl Pts',(-2.418563293,0.499686101,6.834694697));
#167898=CARTESIAN_POINT('Ctrl Pts',(-2.313991557,0.51775868,6.871699036));
#167899=CARTESIAN_POINT('Ctrl Pts',(-2.208336691,0.535714286,6.905486881));
#167900=CARTESIAN_POINT('Ctrl Pts',(-2.16041693,0.54385805,6.920811357));
#167901=CARTESIAN_POINT('Ctrl Pts',(-2.112289109,0.552026826,6.93546932199999));
#167902=CARTESIAN_POINT('Ctrl Pts',(-2.11228911851721,0.552026824384636,
6.9354693191014));
#167903=CARTESIAN_POINT('Ctrl Pts',(-2.14439786744358,0.546576979114217,
6.92569017451321));
#167904=CARTESIAN_POINT('Ctrl Pts',(-2.17641514314413,0.541139220240677,
6.91569521643116));
#167905=CARTESIAN_POINT('Ctrl Pts',(-2.20833669128259,0.535714285951975,
6.90548688090963));
#167906=CARTESIAN_POINT('Ctrl Pts',(-2.27804228996729,0.523868108739421,
6.88319541385762));
#167907=CARTESIAN_POINT('Ctrl Pts',(-2.34752928232983,0.511960760974455,
6.85981022134622));
#167908=CARTESIAN_POINT('Ctrl Pts',(-2.41674687579387,0.499999999814145,
6.83533719297713));
#167909=CARTESIAN_POINT('Ctrl Pts',(-2.418563293,0.499686101,6.834694697));
#167910=CARTESIAN_POINT('Ctrl Pts',(-2.313991557,0.51775868,6.871699036));
#167911=CARTESIAN_POINT('Ctrl Pts',(-2.208336691,0.535714286,6.905486881));
#167912=CARTESIAN_POINT('Ctrl Pts',(-2.159500841,0.544013736,6.921104317));
#167913=CARTESIAN_POINT('Ctrl Pts',(-2.110448992,0.552339147,6.936029488));
#167914=CARTESIAN_POINT('Ctrl Pts',(-2.391212971,0.499686101,6.89200268));
#167915=CARTESIAN_POINT('Ctrl Pts',(-2.285764415,0.51775868,6.928588556));
#167916=CARTESIAN_POINT('Ctrl Pts',(-2.179245942,0.535714286,6.961931308));
#167917=CARTESIAN_POINT('Ctrl Pts',(-2.130010915,0.544013736,6.977343013));
#167918=CARTESIAN_POINT('Ctrl Pts',(-2.080562839,0.552339147,6.99205682800001));
#167919=CARTESIAN_POINT('Ctrl Pts',(-2.11228910270316,0.55202682722255,
6.93546932462214));
#167920=CARTESIAN_POINT('Ctrl Pts',(-2.11384917561811,0.551172308325923,
6.94045372896119));
#167921=CARTESIAN_POINT('Ctrl Pts',(-2.11541023070314,0.550320534981382,
6.9454382922976));
#167922=CARTESIAN_POINT('Ctrl Pts',(-2.11697226156282,0.549471478060439,
6.95042301176581));
#167923=CARTESIAN_POINT('Ctrl Pts',(-2.11842239183661,0.548683245780907,
6.95505063647782));
#167924=CARTESIAN_POINT('Ctrl Pts',(-2.11987336347447,0.547897354464024,
6.95967839699587));
#167925=CARTESIAN_POINT('Ctrl Pts',(-2.12132516643249,0.547113782412266,
6.96430628874322));
#167926=CARTESIAN_POINT('Ctrl Pts',(-2.12277697085747,0.546330209568754,
6.96893418516678));
#167927=CARTESIAN_POINT('Ctrl Pts',(-2.12422960697141,0.545548955797813,
6.97356221398711));
#167928=CARTESIAN_POINT('Ctrl Pts',(-2.12568306337267,0.544769999930616,
6.97819037138624));
#167929=CARTESIAN_POINT('Ctrl Pts',(-2.114094,0.55233793,6.934919362));
#167930=CARTESIAN_POINT('Ctrl Pts',(-1.961691214,0.526068113,6.981378996));
#167931=CARTESIAN_POINT('Ctrl Pts',(-1.807394542,0.49968693,7.021098559));
#167932=CARTESIAN_POINT('Ctrl Pts',(-2.17013704,0.55233793,6.964776065));
#167933=CARTESIAN_POINT('Ctrl Pts',(-2.017078119,0.526068113,7.012467309));
#167934=CARTESIAN_POINT('Ctrl Pts',(-1.862071839,0.49968693,7.053388468));
#167935=CARTESIAN_POINT('Origin',(0.0347259231310537,0.410742962889062,
-0.194008600247233));
#167936=CARTESIAN_POINT('Ctrl Pts',(-2.0806476628918,0.552548454735263,
6.99964900947168));
#167937=CARTESIAN_POINT('Ctrl Pts',(-2.0791202899459,0.552287640367631,
7.00010229623584));
#167938=CARTESIAN_POINT('Ctrl Pts',(-2.077592917,0.552026826,7.000555583));
#167939=CARTESIAN_POINT('Ctrl Pts',(-1.924659088,0.525911829,7.045942586));
#167940=CARTESIAN_POINT('Ctrl Pts',(-1.769889065,0.49968693,7.084607504));
#167941=CARTESIAN_POINT('Ctrl Pts',(-2.11532114214784,0.552548454735263,
6.93453692693789));
#167942=CARTESIAN_POINT('Ctrl Pts',(-2.11380797197949,0.552287640367631,
6.93499778492344));
#167943=CARTESIAN_POINT('Ctrl Pts',(-2.11229480181114,0.552026826,6.935458642909));
#167944=CARTESIAN_POINT('Ctrl Pts',(-1.96078307810616,0.525911829,6.98160374227399));
#167945=CARTESIAN_POINT('Ctrl Pts',(-1.80740069574729,0.49968693,7.02108813870865));
#167946=CARTESIAN_POINT('',(-2.06065818415013,0.552026824384635,7.03232330417225));
#167947=CARTESIAN_POINT('Ctrl Pts',(-2.11980275666774,0.550751630586317,
6.93317998964714));
#167948=CARTESIAN_POINT('Ctrl Pts',(-2.11604623522881,0.551389228293159,
6.93432408856375));
#167949=CARTESIAN_POINT('Ctrl Pts',(-2.11228971378988,0.552026826,6.93546818748035));
#167950=CARTESIAN_POINT('Ctrl Pts',(-1.73447553959357,0.61615356,7.05053655442669));
#167951=CARTESIAN_POINT('Ctrl Pts',(-1.34639737645262,0.681389364000001,
7.12388243289172));
#167952=CARTESIAN_POINT('Ctrl Pts',(-2.01675012375466,0.550751630586317,
7.12700095619441));
#167953=CARTESIAN_POINT('Ctrl Pts',(-2.01288868187733,0.551389228293159,
7.12808912409721));
#167954=CARTESIAN_POINT('Ctrl Pts',(-2.00902724,0.552026826,7.129177292));
#167955=CARTESIAN_POINT('Ctrl Pts',(-1.620660636,0.61615356,7.238620367));
#167956=CARTESIAN_POINT('Ctrl Pts',(-1.222703557,0.681389364000001,7.30522794400001));
#167957=CARTESIAN_POINT('Ctrl Pts',(-1.35103832261866,0.680609082082491,
7.12300468506535));
#167958=CARTESIAN_POINT('Ctrl Pts',(-1.35423171894373,0.677652752598905,
7.14079909641027));
#167959=CARTESIAN_POINT('Ctrl Pts',(-1.35742622271479,0.674729896796178,
7.15859892100758));
#167960=CARTESIAN_POINT('Ctrl Pts',(-1.36063744721483,0.671836782439989,
7.1764005331519));
#167961=CARTESIAN_POINT('Ctrl Pts',(-1.36364364406078,0.669128385299764,
7.19306556242043));
#167962=CARTESIAN_POINT('Ctrl Pts',(-1.36666047782784,0.666446714432678,
7.20973303985256));
#167963=CARTESIAN_POINT('Ctrl Pts',(-1.36968750153995,0.663790956098867,
7.22640277020986));
#167964=CARTESIAN_POINT('Ctrl Pts',(-1.3727145577519,0.661135169251343,
7.24307267954276));
#167965=CARTESIAN_POINT('Ctrl Pts',(-1.37575181232518,0.658505288582776,
7.25974488618265));
#167966=CARTESIAN_POINT('Ctrl Pts',(-1.37879884614972,0.655900535669628,
7.27641920769329));
#167967=CARTESIAN_POINT('Ctrl Pts',(-1.355651883,0.681369595,7.12212805100001));
#167968=CARTESIAN_POINT('Ctrl Pts',(-1.347163385,0.679970133,7.12374378300001));
#167969=CARTESIAN_POINT('Ctrl Pts',(-1.338671059,0.678571429,7.125339276));
#167970=CARTESIAN_POINT('Ctrl Pts',(-0.95805352,0.615882895,7.196847686));
#167971=CARTESIAN_POINT('Ctrl Pts',(-0.57198407,0.552026826,7.227401623));
#167972=CARTESIAN_POINT('Ctrl Pts',(-1.537156899,0.681369595,7.245585413));
#167973=CARTESIAN_POINT('Ctrl Pts',(-1.528521258,0.679970133,7.247417471));
#167974=CARTESIAN_POINT('Ctrl Pts',(-1.519881274,0.678571429,7.24922894));
#167975=CARTESIAN_POINT('Ctrl Pts',(-1.132645864,0.615882895,7.33041714));
#167976=CARTESIAN_POINT('Ctrl Pts',(-0.738965005000001,0.552026826,7.369890775));
#167977=CARTESIAN_POINT('',(-0.600037041950673,0.552026824384634,7.2513399406766));
#167978=CARTESIAN_POINT('Ctrl Pts',(-0.950940417999999,0.499686101,7.240157672));
#167979=CARTESIAN_POINT('Ctrl Pts',(-0.840165045,0.51775868,7.254707187));
#167980=CARTESIAN_POINT('Ctrl Pts',(-0.728996408,0.535714286,7.265860928));
#167981=CARTESIAN_POINT('Ctrl Pts',(-0.678575876,0.54385805,7.270919708));
#167982=CARTESIAN_POINT('Ctrl Pts',(-0.628089994,0.552026826,7.27527826));
#167983=CARTESIAN_POINT('Ctrl Pts',(-0.892761299,0.499686101,7.194822949));
#167984=CARTESIAN_POINT('Ctrl Pts',(-0.782679553,0.51775868,7.20848231500001));
#167985=CARTESIAN_POINT('Ctrl Pts',(-0.672231452,0.535714286,7.218767545));
#167986=CARTESIAN_POINT('Ctrl Pts',(-0.622137718,0.54385805,7.223432411));
#167987=CARTESIAN_POINT('Ctrl Pts',(-0.57198407,0.552026826,7.227401623));
#167988=CARTESIAN_POINT('Ctrl Pts',(-0.571984069433409,0.552026826253397,
7.22740162287586));
#167989=CARTESIAN_POINT('Ctrl Pts',(-0.605444369191663,0.546576979769284,
7.22475354004018));
#167990=CARTESIAN_POINT('Ctrl Pts',(-0.638861722984283,0.541139220276039,
7.22187502581563));
#167991=CARTESIAN_POINT('Ctrl Pts',(-0.672231451613071,0.535714286045145,
7.21876754515753));
#167992=CARTESIAN_POINT('Ctrl Pts',(-0.745099376405783,0.523868109062359,
7.21198188447546));
#167993=CARTESIAN_POINT('Ctrl Pts',(-0.817988928543338,0.511960760997416,
7.20408107381268));
#167994=CARTESIAN_POINT('Ctrl Pts',(-0.890849230764474,0.499999999848742,
7.19505994779791));
#167995=CARTESIAN_POINT('Ctrl Pts',(-0.892761299,0.499686101,7.194822949));
#167996=CARTESIAN_POINT('Ctrl Pts',(-0.782679553,0.51775868,7.20848231500001));
#167997=CARTESIAN_POINT('Ctrl Pts',(-0.672231452,0.535714286,7.218767545));
#167998=CARTESIAN_POINT('Ctrl Pts',(-0.621180069,0.544013736,7.22352159));
#167999=CARTESIAN_POINT('Ctrl Pts',(-0.570066555,0.552339147,7.227553121));
#168000=CARTESIAN_POINT('Ctrl Pts',(-0.853730891,0.499686101,7.244911592));
#168001=CARTESIAN_POINT('Ctrl Pts',(-0.742882782,0.51775868,7.257973788));
#168002=CARTESIAN_POINT('Ctrl Pts',(-0.631686945,0.535714286,7.267638682));
#168003=CARTESIAN_POINT('Ctrl Pts',(-0.580289944,0.544013736,7.27210599500001));
#168004=CARTESIAN_POINT('Ctrl Pts',(-0.528834902,0.552339147,7.275845934));
#168005=CARTESIAN_POINT('Ctrl Pts',(-0.57198406339264,0.552026827237287,
7.22740162335393));
#168006=CARTESIAN_POINT('Ctrl Pts',(-0.572436162740008,0.551172308319716,
7.23260486523954));
#168007=CARTESIAN_POINT('Ctrl Pts',(-0.572889187449938,0.550320535000218,
7.23780847285861));
#168008=CARTESIAN_POINT('Ctrl Pts',(-0.573343131559291,0.54947147810482,
7.24301244272147));
#168009=CARTESIAN_POINT('Ctrl Pts',(-0.573764556088678,0.548683245819846,
7.24784361137244));
#168010=CARTESIAN_POINT('Ctrl Pts',(-0.57418677311898,0.547897354498187,
7.25267509352273));
#168011=CARTESIAN_POINT('Ctrl Pts',(-0.574609773822212,0.547113782441845,
7.25750688254363));
#168012=CARTESIAN_POINT('Ctrl Pts',(-0.575032774952862,0.546330209593747,
7.26233867644677));
#168013=CARTESIAN_POINT('Ctrl Pts',(-0.57545655986563,0.545548955818372,
7.26717077843991));
#168014=CARTESIAN_POINT('Ctrl Pts',(-0.57588111869972,0.544769999874258,
7.27200318229781));
#168015=CARTESIAN_POINT('Ctrl Pts',(-0.573864989,0.55233793,7.227252519));
#168016=CARTESIAN_POINT('Ctrl Pts',(-0.415037848,0.526068113,7.239863859));
#168017=CARTESIAN_POINT('Ctrl Pts',(-0.255810014,0.49968693,7.24548557600001));
#168018=CARTESIAN_POINT('Ctrl Pts',(-0.622179465,0.55233793,7.268458786));
#168019=CARTESIAN_POINT('Ctrl Pts',(-0.462446769,0.526068113,7.282131892));
#168020=CARTESIAN_POINT('Ctrl Pts',(-0.30226761,0.49968693,7.288774568));
#168021=CARTESIAN_POINT('Origin',(-0.00779214677240493,0.410743181043314,
-0.196936069540853));
#168022=CARTESIAN_POINT('Ctrl Pts',(-0.527285648139283,0.552548454735263,
7.28327884871706));
#168023=CARTESIAN_POINT('Ctrl Pts',(-0.525696541069641,0.552287640367631,
7.28339319785853));
#168024=CARTESIAN_POINT('Ctrl Pts',(-0.524107434,0.552026826,7.283507547));
#168025=CARTESIAN_POINT('Ctrl Pts',(-0.364992249,0.525911829,7.294957175));
#168026=CARTESIAN_POINT('Ctrl Pts',(-0.205528848,0.49968693,7.299447149));
#168027=CARTESIAN_POINT('Ctrl Pts',(-0.575145653328268,0.552548454735263,
7.22714282424931));
#168028=CARTESIAN_POINT('Ctrl Pts',(-0.573568789395868,0.552287640367631,
7.22726762077373));
#168029=CARTESIAN_POINT('Ctrl Pts',(-0.571991925463469,0.552026826,7.22739241729816));
#168030=CARTESIAN_POINT('Ctrl Pts',(-0.414102629570901,0.525911829,7.23988812790829));
#168031=CARTESIAN_POINT('Ctrl Pts',(-0.255818263991973,0.49968693,7.24547672213723));
#168032=CARTESIAN_POINT('',(-0.500739504532394,0.552026824384634,7.31089209031286));
#168033=CARTESIAN_POINT('Ctrl Pts',(-0.5798133580548,0.550751630586317,
7.22678200501259));
#168034=CARTESIAN_POINT('Ctrl Pts',(-0.575898714027401,0.551389228293159,
7.2270918140063));
#168035=CARTESIAN_POINT('Ctrl Pts',(-0.57198407,0.552026826,7.227401623));
#168036=CARTESIAN_POINT('Ctrl Pts',(-0.178266631,0.61615356,7.25856083));
#168037=CARTESIAN_POINT('Ctrl Pts',(0.216505724,0.681389364000001,7.246766539));
#168038=CARTESIAN_POINT('Ctrl Pts',(-0.437505093897724,0.550751630586317,
7.39391729643459));
#168039=CARTESIAN_POINT('Ctrl Pts',(-0.433500006448862,0.551389228293159,
7.39414992771729));
#168040=CARTESIAN_POINT('Ctrl Pts',(-0.429494919,0.552026826,7.394382559));
#168041=CARTESIAN_POINT('Ctrl Pts',(-0.026681084,0.61615356,7.41777957600001));
#168042=CARTESIAN_POINT('Ctrl Pts',(0.37629064,0.681389364000001,7.397280897));
#168043=CARTESIAN_POINT('Origin',(-7.084,1.2,-7.084));
#168044=CARTESIAN_POINT('Origin',(-6.831,0.,6.831));
#168045=CARTESIAN_POINT('',(0.,0.,0.));
#168046=CARTESIAN_POINT('Origin',(-1.00994955198656E-15,1.2,8.96986209700434E-15));
#168047=CARTESIAN_POINT('',(6.99999999999999,1.7,8.13905003589241E-15));
#168048=CARTESIAN_POINT('Origin',(-9.8350885369411E-16,1.7,8.99630279529556E-15));
#168049=CARTESIAN_POINT('',(6.99999999999999,1.2,8.1126093376012E-15));
#168050=CARTESIAN_POINT('',(6.99999999999999,1.2,8.1126093376012E-15));
#168051=CARTESIAN_POINT('Origin',(-1.00994955198656E-15,1.2,8.96986209700434E-15));
#168052=CARTESIAN_POINT('Origin',(-2.75545529808154E-16,8.2,0.));
#168053=CARTESIAN_POINT('',(3.35410196653775,3.2,-2.99999999967796));
#168054=CARTESIAN_POINT('',(-3.35410196599079,3.2,-3.00000000028945));
#168055=CARTESIAN_POINT('Origin',(-2.75545529808154E-16,3.2,0.));
#168056=CARTESIAN_POINT('',(-3.35410196587205,7.72506281421231,-3.00000000013276));
#168057=CARTESIAN_POINT('',(-3.35410196573189,8.2,-3.00000000057891));
#168058=CARTESIAN_POINT('',(-3.9686269655808,8.2,-2.12132034546057));
#168059=CARTESIAN_POINT('Ctrl Pts',(-3.3541019659917,7.72506281429298,-3.00000000028843));
#168060=CARTESIAN_POINT('Ctrl Pts',(-3.58710885370055,7.8821560259217,-2.7394903802622));
#168061=CARTESIAN_POINT('Ctrl Pts',(-3.79652270311249,8.04821830647437,
-2.44329793762419));
#168062=CARTESIAN_POINT('Ctrl Pts',(-3.96862696573053,8.19999999923597,
-2.12132034518044));
#168063=CARTESIAN_POINT('',(-3.96862696601141,8.19999999948366,2.12132034465497));
#168064=CARTESIAN_POINT('Origin',(-2.75545529808154E-16,8.2,0.));
#168065=CARTESIAN_POINT('',(-3.35410196620117,7.72506281443419,3.00000000011756));
#168066=CARTESIAN_POINT('Ctrl Pts',(-3.96862696601141,8.19999999948366,
2.12132034465497));
#168067=CARTESIAN_POINT('Ctrl Pts',(-3.79654026724857,8.04823379656728,
2.44326507823699));
#168068=CARTESIAN_POINT('Ctrl Pts',(-3.58713416135787,7.88217308835326,
2.73946208540911));
#168069=CARTESIAN_POINT('Ctrl Pts',(-3.35410196617499,7.72506281441655,
3.00000000008351));
#168070=CARTESIAN_POINT('',(-3.35410196614453,3.2,3.00000000011756));
#168071=CARTESIAN_POINT('',(-3.35410196603938,8.2,3.00000000023512));
#168072=CARTESIAN_POINT('',(-8.26636589424463E-16,3.2,4.5));
#168073=CARTESIAN_POINT('Origin',(-2.75545529808154E-16,3.2,0.));
#168074=CARTESIAN_POINT('',(-8.26636589424463E-16,1.2,4.5));
#168075=CARTESIAN_POINT('',(-8.26636589424463E-16,8.2,4.5));
#168076=CARTESIAN_POINT('Origin',(-2.75545529808154E-16,1.2,0.));
#168077=CARTESIAN_POINT('',(3.35410196626425,3.20000000000001,2.9999999999837));
#168078=CARTESIAN_POINT('Origin',(-2.75545529808154E-16,3.2,0.));
#168079=CARTESIAN_POINT('',(3.35410196633334,7.7250628145233,2.99999999999999));
#168080=CARTESIAN_POINT('',(3.35410196627882,8.19999999999999,2.99999999996742));
#168081=CARTESIAN_POINT('',(3.96862696647739,8.19999999977888,2.12132034378318));
#168082=CARTESIAN_POINT('Ctrl Pts',(3.35410196629467,7.72506281449723,2.9999999999497));
#168083=CARTESIAN_POINT('Ctrl Pts',(3.58710885421097,7.88215602628645,2.73949037963858));
#168084=CARTESIAN_POINT('Ctrl Pts',(3.79652270377537,8.04821830700949,2.44329793664967));
#168085=CARTESIAN_POINT('Ctrl Pts',(3.96862696645806,8.19999999987757,2.12132034381937));
#168086=CARTESIAN_POINT('',(3.96862696629539,8.19999999973411,-2.12132034412369));
#168087=CARTESIAN_POINT('Origin',(-7.51257911368137E-16,8.2,-5.73912088018113E-15));
#168088=CARTESIAN_POINT('',(3.35410196681833,7.72506281485028,-2.99999999967796));
#168089=CARTESIAN_POINT('Ctrl Pts',(3.96862696629539,8.19999999973411,-2.12132034412369));
#168090=CARTESIAN_POINT('Ctrl Pts',(3.79654026760466,8.04823379686202,-2.44326507767448));
#168091=CARTESIAN_POINT('Ctrl Pts',(3.58713416179472,7.88217308868278,-2.73946208483092));
#168092=CARTESIAN_POINT('Ctrl Pts',(3.35410196668864,7.72506281476285,-2.99999999950923));
#168093=CARTESIAN_POINT('',(3.35410196682577,8.20000000000001,-2.99999999935591));
#168094=CARTESIAN_POINT('Origin',(0.,1.7,-3.98010209722891E-16));
#168095=CARTESIAN_POINT('',(7.9602041944578E-16,4.6,6.5));
#168096=CARTESIAN_POINT('',(-7.9602041944578E-16,4.6,-6.5));
#168097=CARTESIAN_POINT('Origin',(0.,4.6,-4.49477084187968E-16));
#168098=CARTESIAN_POINT('Origin',(0.,4.6,-4.49477084187968E-16));
#168099=CARTESIAN_POINT('',(-7.9602041944578E-16,1.7,-6.5));
#168100=CARTESIAN_POINT('',(-7.9602041944578E-16,1.7,-6.5));
#168101=CARTESIAN_POINT('Origin',(0.,1.7,-3.98010209722891E-16));
#168102=CARTESIAN_POINT('Origin',(6.07153216591882E-15,12.7,-5.92306788700001));
#168103=CARTESIAN_POINT('',(3.31662479106209,7.70000000046876,-4.87954915902201));
#168104=CARTESIAN_POINT('',(-3.31662479061361,7.70000000017128,-4.87954915911973));
#168105=CARTESIAN_POINT('Ctrl Pts',(3.31662479106319,7.7000000004695,-4.87954915902126));
#168106=CARTESIAN_POINT('Ctrl Pts',(3.02283773840257,7.50512371602168,-5.07923593138345));
#168107=CARTESIAN_POINT('Ctrl Pts',(2.69989199164368,7.32869287193907,-5.2594505282712));
#168108=CARTESIAN_POINT('Ctrl Pts',(1.99447655600236,7.02761131950198,-5.56659302751097));
#168109=CARTESIAN_POINT('Ctrl Pts',(1.60896441674793,6.90553799888819,-5.69087246377536));
#168110=CARTESIAN_POINT('Ctrl Pts',(0.81436889005366,6.74169825447987,-5.85761036662907));
#168111=CARTESIAN_POINT('Ctrl Pts',(0.405257005850959,6.7,-5.9));
#168112=CARTESIAN_POINT('Ctrl Pts',(-0.40525700585096,6.7,-5.9));
#168113=CARTESIAN_POINT('Ctrl Pts',(-0.814368890053663,6.74169825447987,
-5.85761036662907));
#168114=CARTESIAN_POINT('Ctrl Pts',(-1.60896441674793,6.9055379988882,-5.69087246377536));
#168115=CARTESIAN_POINT('Ctrl Pts',(-1.99447655600236,7.02761131950198,
-5.56659302751097));
#168116=CARTESIAN_POINT('Ctrl Pts',(-2.69989199149733,7.32869287187661,
-5.25945052833492));
#168117=CARTESIAN_POINT('Ctrl Pts',(-3.02283773812843,7.50512371587152,
-5.07923593153682));
#168118=CARTESIAN_POINT('Ctrl Pts',(-3.31662479068874,7.70000000022112,
-4.87954915927577));
#168119=CARTESIAN_POINT('',(-3.96862696539036,8.19999999978668,-3.66196668634223));
#168120=CARTESIAN_POINT('Ctrl Pts',(-3.31662479061361,7.70000000017128,
-4.87954915911973));
#168121=CARTESIAN_POINT('Ctrl Pts',(-3.45417031520138,7.79123737951156,
-4.67574192153527));
#168122=CARTESIAN_POINT('Ctrl Pts',(-3.57693048224706,7.88087036673549,
-4.46762441021359));
#168123=CARTESIAN_POINT('Ctrl Pts',(-3.78526630624945,8.04294279611343,
-4.07348751507535));
#168124=CARTESIAN_POINT('Ctrl Pts',(-3.880589771382,8.1223584918038,-3.87186781082631));
#168125=CARTESIAN_POINT('Ctrl Pts',(-3.96862696589172,8.19999999937811,
-3.66196668640138));
#168126=CARTESIAN_POINT('',(-3.96862696466762,8.2,3.705910285));
#168127=CARTESIAN_POINT('Origin',(6.07153216583313E-15,12.7,-3.00000000000001));
#168128=CARTESIAN_POINT('',(3.96862696634616,8.19999999999999,-3.66196668499183));
#168129=CARTESIAN_POINT('',(3.96862696609543,8.19999999955775,-5.923067887));
#168130=CARTESIAN_POINT('Ctrl Pts',(3.96862696647649,8.19999999989382,-3.66196668500722));
#168131=CARTESIAN_POINT('Ctrl Pts',(3.88058977180391,8.12235849215553,-3.87186780993351));
#168132=CARTESIAN_POINT('Ctrl Pts',(3.78526630647339,8.04294279628764,-4.07348751465177));
#168133=CARTESIAN_POINT('Ctrl Pts',(3.57693048230356,7.88087036677944,-4.46762441010679));
#168134=CARTESIAN_POINT('Ctrl Pts',(3.45417031533094,7.79123737960611,-4.67574192131607));
#168135=CARTESIAN_POINT('Ctrl Pts',(3.31662479083111,7.70000000031555,-4.87954915879754));
#168136=CARTESIAN_POINT('Origin',(0.,5.2,-3.61270805748469E-16));
#168137=CARTESIAN_POINT('',(-7.22541611496938E-16,5.2,5.9));
#168138=CARTESIAN_POINT('',(-7.22541611496938E-16,5.2,5.9));
#168139=CARTESIAN_POINT('Origin',(0.,5.2,-1.28008620615991E-15));
#168140=CARTESIAN_POINT('Origin',(-1.99493199737333E-14,8.20000000000005,
-1.07349914972576E-14));
#168141=CARTESIAN_POINT('',(3.96862696634616,8.19999999977888,3.6619666853179));
#168142=CARTESIAN_POINT('Origin',(1.73472347597681E-14,8.19999999999999,
-2.12531425647619E-14));
#168143=CARTESIAN_POINT('',(3.31662479023432,7.69999999991968,4.87954915968175));
#168144=CARTESIAN_POINT('Ctrl Pts',(3.31662479023432,7.69999999991968,4.87954915968175));
#168145=CARTESIAN_POINT('Ctrl Pts',(3.53703437758293,7.84620318019848,4.55295860532687));
#168146=CARTESIAN_POINT('Ctrl Pts',(3.72403639169807,7.99140810117883,4.20771033743069));
#168147=CARTESIAN_POINT('Ctrl Pts',(3.90713471909885,8.14631670002404,3.8055381686148));
#168148=CARTESIAN_POINT('Ctrl Pts',(3.93825718793793,8.17321637276845,3.73437529255024));
#168149=CARTESIAN_POINT('Ctrl Pts',(3.96862696634616,8.19999999977888,3.66196668531789));
#168150=CARTESIAN_POINT('Origin',(0.,7.7,3.61270805748469E-16));
#168151=CARTESIAN_POINT('Origin',(0.,7.7,3.61270805748469E-16));
#168152=CARTESIAN_POINT('',(-4.90205800726441E-17,6.7,5.9));
#168153=CARTESIAN_POINT('',(-7.22541611496938E-16,7.7,5.9));
#168154=CARTESIAN_POINT('',(-3.3166247905171,7.70000000010726,4.87954915939243));
#168155=CARTESIAN_POINT('Ctrl Pts',(6.93889390390723E-16,6.7,5.9));
#168156=CARTESIAN_POINT('Ctrl Pts',(-0.405257005850958,6.7,5.9));
#168157=CARTESIAN_POINT('Ctrl Pts',(-0.81436889005366,6.74169825447987,
5.85761036662908));
#168158=CARTESIAN_POINT('Ctrl Pts',(-1.60896441674793,6.9055379988882,5.69087246377536));
#168159=CARTESIAN_POINT('Ctrl Pts',(-1.99447655600236,7.02761131950198,
5.56659302751097));
#168160=CARTESIAN_POINT('Ctrl Pts',(-2.69989199143067,7.32869287184816,
5.25945052836394));
#168161=CARTESIAN_POINT('Ctrl Pts',(-3.02283773800358,7.50512371580314,
5.07923593160667));
#168162=CARTESIAN_POINT('Ctrl Pts',(-3.3166247905182,7.700000000108,4.87954915939168));
#168163=CARTESIAN_POINT('Origin',(3.33197214177239E-15,7.70000000000001,
2.60208521393186E-15));
#168164=CARTESIAN_POINT('Ctrl Pts',(3.31662479020071,7.69999999989739,4.87954915960748));
#168165=CARTESIAN_POINT('Ctrl Pts',(3.02283773777115,7.50512371567581,5.07923593173671));
#168166=CARTESIAN_POINT('Ctrl Pts',(2.69989199130658,7.32869287179519,5.25945052841797));
#168167=CARTESIAN_POINT('Ctrl Pts',(1.99447655600236,7.02761131950198,5.56659302751097));
#168168=CARTESIAN_POINT('Ctrl Pts',(1.60896441674793,6.90553799888819,5.69087246377536));
#168169=CARTESIAN_POINT('Ctrl Pts',(0.814368890053661,6.74169825447987,
5.85761036662908));
#168170=CARTESIAN_POINT('Ctrl Pts',(0.405257005850959,6.7,5.9));
#168171=CARTESIAN_POINT('Ctrl Pts',(6.24500451351651E-16,6.7,5.9));
#168172=CARTESIAN_POINT('Origin',(-7.084,1.2,7.084));
#168173=CARTESIAN_POINT('Origin',(-7.084,1.7,7.084));
#168174=CARTESIAN_POINT('Origin',(3.354101966,3.2,3.));
#168175=CARTESIAN_POINT('Origin',(3.03576608295941E-15,12.7,3.));
#168176=CARTESIAN_POINT('',(3.354101966,3.2,3.));
#168177=CARTESIAN_POINT('Origin',(3.03576608295941E-15,12.7,2.098645905));
#168178=CARTESIAN_POINT('',(-3.96862696596741,8.19999999960437,3.66196668531925));
#168179=CARTESIAN_POINT('',(-3.96862696551168,8.19999999904294,2.098645905));
#168180=CARTESIAN_POINT('Ctrl Pts',(-3.96862696627435,8.19999999971555,
3.66196668548911));
#168181=CARTESIAN_POINT('Ctrl Pts',(-3.88058977165807,8.12235849203395,
3.87186781024209));
#168182=CARTESIAN_POINT('Ctrl Pts',(-3.78526630639598,8.04294279622742,
4.07348751479814));
#168183=CARTESIAN_POINT('Ctrl Pts',(-3.57693048220827,7.88087036670531,
4.467624410287));
#168184=CARTESIAN_POINT('Ctrl Pts',(-3.45417031511241,7.79123737944662,
4.67574192168587));
#168185=CARTESIAN_POINT('Ctrl Pts',(-3.31662479046424,7.7000000000722,4.87954915934106));
#168186=CARTESIAN_POINT('',(3.96862696609543,8.19999999955776,2.098645905));
#168187=CARTESIAN_POINT('Origin',(-5.408588238,8.2,3.705910285));
#168188=CARTESIAN_POINT('Origin',(2.60208521396521E-15,8.20000000000001,
2.60208521396521E-15));
#168189=CARTESIAN_POINT('Origin',(-3.354101966,3.2,-3.));
#168190=CARTESIAN_POINT('',(-3.354101966,3.2,-3.));
#168191=CARTESIAN_POINT('Origin',(-3.39435119,3.2,-4.509));
#168192=CARTESIAN_POINT('Origin',(-3.39435119,3.2,3.));
#168193=CARTESIAN_POINT('Origin',(3.968626967,8.2,3.705910285));
#168194=CARTESIAN_POINT('Origin',(2.60208521396521E-15,8.20000000000001,
2.60208521396521E-15));
#168195=CARTESIAN_POINT('Origin',(-1.06251812903579E-14,12.7,3.));
#168196=CARTESIAN_POINT('',(3.35410196856641,7.72506281602885,3.));
#168197=CARTESIAN_POINT('',(-3.3541019674191,7.72506281525532,3.));
#168198=CARTESIAN_POINT('Origin',(-1.06251812903579E-14,12.7,3.));
#168199=CARTESIAN_POINT('',(-1.78706256720332E-9,6.7,4.49999994459035));
#168200=CARTESIAN_POINT('Ctrl Pts',(-1.78706256720332E-9,6.7,4.49999994459035));
#168201=CARTESIAN_POINT('Ctrl Pts',(0.129339864826736,6.69999999996148,
4.50000046715268));
#168202=CARTESIAN_POINT('Ctrl Pts',(0.257887038991172,6.70417800065084,
4.4945561472941));
#168203=CARTESIAN_POINT('Ctrl Pts',(0.385634752023517,6.71240567188861,
4.48366782762931));
#168204=CARTESIAN_POINT('Ctrl Pts',(0.514978836758675,6.72073615844284,
4.47264344442968));
#168205=CARTESIAN_POINT('Ctrl Pts',(0.643504005298411,6.73321809239324,
4.45603815176915));
#168206=CARTESIAN_POINT('Ctrl Pts',(0.771213641489143,6.74977063306119,
4.43385282424746));
#168207=CARTESIAN_POINT('Ctrl Pts',(0.834706337055075,6.75799996842555,
4.42282306730522));
#168208=CARTESIAN_POINT('Ctrl Pts',(0.897997554075187,6.76723625943253,
4.41041407905336));
#168209=CARTESIAN_POINT('Ctrl Pts',(0.961087886286797,6.77747435000635,
4.39662596696742));
#168210=CARTESIAN_POINT('Ctrl Pts',(1.12537190708357,6.80413381788023,4.3607224233773));
#168211=CARTESIAN_POINT('Ctrl Pts',(1.28792473919659,6.83753175897511,4.31546645455455));
#168212=CARTESIAN_POINT('Ctrl Pts',(1.44821965309347,6.87740093803517,4.26085806049916));
#168213=CARTESIAN_POINT('Ctrl Pts',(1.59559285693051,6.91405617873864,4.21065176391313));
#168214=CARTESIAN_POINT('Ctrl Pts',(1.74105777043341,6.95618076529,4.15254010445229));
#168215=CARTESIAN_POINT('Ctrl Pts',(1.88423172912276,7.00353874840116,4.08652308211663));
#168216=CARTESIAN_POINT('Ctrl Pts',(1.90575246534007,7.01065721234285,4.07659994430202));
#168217=CARTESIAN_POINT('Ctrl Pts',(1.92586056099981,7.01743886839554,4.06714396610388));
#168218=CARTESIAN_POINT('Ctrl Pts',(1.94570126342584,7.0242404390687,4.05763019846389));
#168219=CARTESIAN_POINT('Ctrl Pts',(1.96030649260708,7.029247242575,4.05062688004424));
#168220=CARTESIAN_POINT('Ctrl Pts',(1.97476648543564,7.03426595278277,4.04359224671478));
#168221=CARTESIAN_POINT('Ctrl Pts',(1.98953237657893,7.03945577505624,4.03631690113625));
#168222=CARTESIAN_POINT('Ctrl Pts',(2.02435722390795,7.05169579271482,4.01915824836145));
#168223=CARTESIAN_POINT('Ctrl Pts',(2.05894905106974,7.064214991415,4.00155625212987));
#168224=CARTESIAN_POINT('Ctrl Pts',(2.09330430396177,7.07700461577505,3.98351091244152));
#168225=CARTESIAN_POINT('Ctrl Pts',(2.16201480974582,7.10258386449517,3.94742023306482));
#168226=CARTESIAN_POINT('Ctrl Pts',(2.22977900041436,7.12924486558745,3.90955617986103));
#168227=CARTESIAN_POINT('Ctrl Pts',(2.29657229433863,7.15691821304465,3.86991875283014));
#168228=CARTESIAN_POINT('Ctrl Pts',(2.43015888218718,7.21226490795906,3.79064389876838));
#168229=CARTESIAN_POINT('Ctrl Pts',(2.55985804007038,7.27166009599461,3.70427554939825));
#168230=CARTESIAN_POINT('Ctrl Pts',(2.68552125332657,7.3345572784782,3.61081370471976));
#168231=CARTESIAN_POINT('Ctrl Pts',(2.717569407263,7.35059807939496,3.58697793363111));
#168232=CARTESIAN_POINT('Ctrl Pts',(2.74838045933184,7.36637365233043,3.56343889776758));
#168233=CARTESIAN_POINT('Ctrl Pts',(2.77863399377477,7.38218154421955,3.53970081047817));
#168234=CARTESIAN_POINT('Ctrl Pts',(2.807693647199,7.39736561669651,3.51689948817693));
#168235=CARTESIAN_POINT('Ctrl Pts',(2.83623879778978,7.4125800305368,3.49391451461461));
#168236=CARTESIAN_POINT('Ctrl Pts',(2.86485150554233,7.42812880931336,3.47030651234304));
#168237=CARTESIAN_POINT('Ctrl Pts',(2.96506503774409,7.48258706108384,3.38762152788363));
#168238=CARTESIAN_POINT('Ctrl Pts',(3.06126197540171,7.53856247314563,3.30094146245984));
#168239=CARTESIAN_POINT('Ctrl Pts',(3.15352787595008,7.59556448413679,3.21026631607167));
#168240=CARTESIAN_POINT('Ctrl Pts',(3.22256997475172,7.63821879576605,3.14241457042591));
#168241=CARTESIAN_POINT('Ctrl Pts',(3.28941180762198,7.68144871837357,3.07232579840202));
#168242=CARTESIAN_POINT('Ctrl Pts',(3.35410196856641,7.72506281602885,3.));
#168243=CARTESIAN_POINT('Ctrl Pts',(-3.3541019674191,7.72506281525532,3.));
#168244=CARTESIAN_POINT('Ctrl Pts',(-3.26710242501228,7.66640773570053,
3.09726844444298));
#168245=CARTESIAN_POINT('Ctrl Pts',(-3.17621168160488,7.60844716360588,
3.19048950554114));
#168246=CARTESIAN_POINT('Ctrl Pts',(-3.08131599749725,7.55165155379247,
3.27966318329446));
#168247=CARTESIAN_POINT('Ctrl Pts',(-2.98857273444298,7.49614418029296,
3.36681422637049));
#168248=CARTESIAN_POINT('Ctrl Pts',(-2.89200380684714,7.44174972026469,
3.4500994090919));
#168249=CARTESIAN_POINT('Ctrl Pts',(-2.79153720797724,7.38894360635489,
3.52951873145868));
#168250=CARTESIAN_POINT('Ctrl Pts',(-2.75687850682911,7.37072669305851,
3.55691659891175));
#168251=CARTESIAN_POINT('Ctrl Pts',(-2.72175627382409,7.35269911657902,
3.5838543927489));
#168252=CARTESIAN_POINT('Ctrl Pts',(-2.68616864279695,7.33488135989013,
3.61033211297012));
#168253=CARTESIAN_POINT('Ctrl Pts',(-2.65488489637762,7.31921844089472,
3.63360767982455));
#168254=CARTESIAN_POINT('Ctrl Pts',(-2.62249728780483,7.30334972819107,
3.65704953038831));
#168255=CARTESIAN_POINT('Ctrl Pts',(-2.58964713218308,7.28763196643318,
3.68017390982419));
#168256=CARTESIAN_POINT('Ctrl Pts',(-2.55836408346407,7.27266401582474,
3.70219514761736));
#168257=CARTESIAN_POINT('Ctrl Pts',(-2.52666178411185,7.25783281963418,
3.72392848153279));
#168258=CARTESIAN_POINT('Ctrl Pts',(-2.49511365736935,7.24340693868336,
3.74495613869445));
#168259=CARTESIAN_POINT('Ctrl Pts',(-2.37311356381492,7.18762046235878,
3.82627241340996));
#168260=CARTESIAN_POINT('Ctrl Pts',(-2.24760162082057,7.13517639097339,
3.90130500603833));
#168261=CARTESIAN_POINT('Ctrl Pts',(-2.11872653965801,7.08653423897956,
3.97005391657957));
#168262=CARTESIAN_POINT('Ctrl Pts',(-2.04263766794184,7.05781552602381,
4.01064381951201));
#168263=CARTESIAN_POINT('Ctrl Pts',(-1.96537740734312,7.030422274254,4.0490433468627));
#168264=CARTESIAN_POINT('Ctrl Pts',(-1.88698486775426,7.00445014868043,
4.08525249863165));
#168265=CARTESIAN_POINT('Ctrl Pts',(-1.87314229568395,6.99986398497203,
4.09164631870172));
#168266=CARTESIAN_POINT('Ctrl Pts',(-1.85790374859226,6.99487575477689,
4.09859060754196));
#168267=CARTESIAN_POINT('Ctrl Pts',(-1.84288700566157,6.99002911703013,
4.10533727720876));
#168268=CARTESIAN_POINT('Ctrl Pts',(-1.83881362303491,6.98871443713673,
4.10716735228798));
#168269=CARTESIAN_POINT('Ctrl Pts',(-1.83475665416027,6.98740989272774,
4.10898288657729));
#168270=CARTESIAN_POINT('Ctrl Pts',(-1.83074859655393,6.98612569474828,
4.11076894900306));
#168271=CARTESIAN_POINT('Ctrl Pts',(-1.81196462019843,6.98010723222821,
4.11913942609453));
#168272=CARTESIAN_POINT('Ctrl Pts',(-1.7931423680753,6.97417864231932,4.1273748968128));
#168273=CARTESIAN_POINT('Ctrl Pts',(-1.77428267600905,6.96834046844946,
4.13547536115787));
#168274=CARTESIAN_POINT('Ctrl Pts',(-1.73656329187656,6.95666412070975,
4.15167628984802));
#168275=CARTESIAN_POINT('Ctrl Pts',(-1.69869414511969,6.94534944605757,
4.1673371930454));
#168276=CARTESIAN_POINT('Ctrl Pts',(-1.66068201913898,6.93440070493028,
4.18245807074999));
#168277=CARTESIAN_POINT('Ctrl Pts',(-1.58465776717757,6.9125032226757,4.21269982615919));
#168278=CARTESIAN_POINT('Ctrl Pts',(-1.50806156814689,6.89206961886207,
4.24078147959728));
#168279=CARTESIAN_POINT('Ctrl Pts',(-1.43094874001203,6.87313242784273,
4.26670303106426));
#168280=CARTESIAN_POINT('Ctrl Pts',(-1.27672308374233,6.83525804580405,
4.31854613399822));
#168281=CARTESIAN_POINT('Ctrl Pts',(-1.12043027200512,6.80337178019105,
4.36174882904776));
#168282=CARTESIAN_POINT('Ctrl Pts',(-0.962538453685088,6.77770992561345,
4.39631111621286));
#168283=CARTESIAN_POINT('Ctrl Pts',(-0.800364978502917,6.75135218155331,
4.43181065177745));
#168284=CARTESIAN_POINT('Ctrl Pts',(-0.636504623877591,6.73156143174531,
4.45819481027176));
#168285=CARTESIAN_POINT('Ctrl Pts',(-0.471495848535052,6.71855438336064,
4.47546359169579));
#168286=CARTESIAN_POINT('Ctrl Pts',(-0.315200100455022,6.70623415158282,
4.49182052244385));
#168287=CARTESIAN_POINT('Ctrl Pts',(-0.157874403365117,6.70000000004702,
4.49999930674204));
#168288=CARTESIAN_POINT('Ctrl Pts',(-1.78706256720332E-9,6.7,4.49999994459035));
#168289=CARTESIAN_POINT('Origin',(-1.06251812903579E-14,12.7,-4.50927590902132));
#168290=CARTESIAN_POINT('',(1.78651616390521E-9,6.7,-4.4999999445903));
#168291=CARTESIAN_POINT('',(-3.3541019674191,7.72506281525532,-3.));
#168292=CARTESIAN_POINT('Ctrl Pts',(1.78651616390521E-9,6.7,-4.4999999445903));
#168293=CARTESIAN_POINT('Ctrl Pts',(-0.1293400059774,6.69999999996149,-4.50000046715798));
#168294=CARTESIAN_POINT('Ctrl Pts',(-0.257887320736992,6.70417800978038,
-4.4945561354334));
#168295=CARTESIAN_POINT('Ctrl Pts',(-0.385635172884763,6.71240569899445,
-4.48366779203622));
#168296=CARTESIAN_POINT('Ctrl Pts',(-0.514979403716141,6.72073620408728,
-4.47264338436081));
#168297=CARTESIAN_POINT('Ctrl Pts',(-0.643504716769734,6.73321816598151,
-4.4560380546073));
#168298=CARTESIAN_POINT('Ctrl Pts',(-0.771214494975836,6.7497707436823,
-4.43385267738071));
#168299=CARTESIAN_POINT('Ctrl Pts',(-0.834706907564031,6.75800005162989,
-4.42282295715034));
#168300=CARTESIAN_POINT('Ctrl Pts',(-0.897997843233306,6.76723630625431,
-4.41041401785453));
#168301=CARTESIAN_POINT('Ctrl Pts',(-0.961087895601655,6.77747435151793,
-4.39662596696768));
#168302=CARTESIAN_POINT('Ctrl Pts',(-1.12537190818166,6.80413381832361,
-4.36072242527897));
#168303=CARTESIAN_POINT('Ctrl Pts',(-1.28792473154021,6.83753175756272,
-4.31546645934819));
#168304=CARTESIAN_POINT('Ctrl Pts',(-1.44821963626535,6.87740093384961,
-4.26085806917535));
#168305=CARTESIAN_POINT('Ctrl Pts',(-1.59559284796386,6.91405617605614,
-4.21065177060798));
#168306=CARTESIAN_POINT('Ctrl Pts',(-1.74105776855341,6.95618076454506,
-4.15254010825504));
#168307=CARTESIAN_POINT('Ctrl Pts',(-1.88423173353724,7.00353874986135,
-4.08652308211651));
#168308=CARTESIAN_POINT('Ctrl Pts',(-1.90575247663866,7.01065721609861,
-4.0765999409923));
#168309=CARTESIAN_POINT('Ctrl Pts',(-1.92586057997639,7.01743887479533,
-4.06714395901082));
#168310=CARTESIAN_POINT('Ctrl Pts',(-1.94570129044311,7.02424044833046,
-4.05763018730582));
#168311=CARTESIAN_POINT('Ctrl Pts',(-1.96030651405485,7.02924725000518,
-4.05062687140262));
#168312=CARTESIAN_POINT('Ctrl Pts',(-1.97476650173835,7.03426595848241,
-4.04359224048625));
#168313=CARTESIAN_POINT('Ctrl Pts',(-1.98953238692627,7.03945577869306,
-4.0363168977882));
#168314=CARTESIAN_POINT('Ctrl Pts',(-2.02435723598812,7.05169579703221,
-4.0191582440327));
#168315=CARTESIAN_POINT('Ctrl Pts',(-2.05894906457989,7.06421499634263,
-4.00155624698302));
#168316=CARTESIAN_POINT('Ctrl Pts',(-2.09330431860398,7.07700462122599,
-3.98351090663917));
#168317=CARTESIAN_POINT('Ctrl Pts',(-2.16201482665217,7.10258387099271,
-3.94742022595146));
#168318=CARTESIAN_POINT('Ctrl Pts',(-2.2297790183933,7.12924487278354,-3.90955617208706));
#168319=CARTESIAN_POINT('Ctrl Pts',(-2.29657231224609,7.15691822046394,
-3.86991874504595));
#168320=CARTESIAN_POINT('Ctrl Pts',(-2.43015889995167,7.21226491582476,
-3.79064389096373));
#168321=CARTESIAN_POINT('Ctrl Pts',(-2.55985805310911,7.27166010239785,
-3.7042755441747));
#168322=CARTESIAN_POINT('Ctrl Pts',(-2.68552125752396,7.33455728057908,
-3.61081370467886));
#168323=CARTESIAN_POINT('Ctrl Pts',(-2.71756942591652,7.3505980887628,-3.5869779224832));
#168324=CARTESIAN_POINT('Ctrl Pts',(-2.74838049300034,7.36637366956853,
-3.56343887448938));
#168325=CARTESIAN_POINT('Ctrl Pts',(-2.7786340426751,7.38218156977065,-3.53970077428726));
#168326=CARTESIAN_POINT('Ctrl Pts',(-2.80769367980225,7.39736563407233,
-3.51689946385006));
#168327=CARTESIAN_POINT('Ctrl Pts',(-2.83623881538779,7.41258004008775,
-3.4939145018208));
#168328=CARTESIAN_POINT('Ctrl Pts',(-2.86485150727639,7.42812881025568,
-3.47030651236767));
#168329=CARTESIAN_POINT('Ctrl Pts',(-2.96506504253387,7.4825870637294,-3.38762152443886));
#168330=CARTESIAN_POINT('Ctrl Pts',(-3.06126198327615,7.5385624777365,-3.30094145520137));
#168331=CARTESIAN_POINT('Ctrl Pts',(-3.1535278869199,7.59556449091396,-3.21026630465519));
#168332=CARTESIAN_POINT('Ctrl Pts',(-3.22256998125089,7.63821879998625,
-3.14241456256791));
#168333=CARTESIAN_POINT('Ctrl Pts',(-3.28941181008927,7.68144872005871,
-3.07232579434951));
#168334=CARTESIAN_POINT('Ctrl Pts',(-3.3541019674191,7.72506281525532,-3.));
#168335=CARTESIAN_POINT('',(3.35410196856641,7.72506281602885,-3.));
#168336=CARTESIAN_POINT('Ctrl Pts',(3.35410196856641,7.72506281602885,-3.));
#168337=CARTESIAN_POINT('Ctrl Pts',(3.26710242611272,7.66640773641328,-3.09726844451049));
#168338=CARTESIAN_POINT('Ctrl Pts',(3.17621168265789,7.60844716426129,-3.19048950566652));
#168339=CARTESIAN_POINT('Ctrl Pts',(3.08131599850246,7.55165155439411,-3.27966318346809));
#168340=CARTESIAN_POINT('Ctrl Pts',(2.98857273540257,7.49614418084271,-3.36681422659025));
#168341=CARTESIAN_POINT('Ctrl Pts',(2.89200380776084,7.44174972076591,-3.45009940934867));
#168342=CARTESIAN_POINT('Ctrl Pts',(2.79153720884502,7.38894360681101,-3.52951873174336));
#168343=CARTESIAN_POINT('Ctrl Pts',(2.75687850781638,7.37072669357022,-3.55691659909906));
#168344=CARTESIAN_POINT('Ctrl Pts',(2.72175627493448,7.35269911714525,-3.58385439284135));
#168345=CARTESIAN_POINT('Ctrl Pts',(2.68616864403411,7.33488136050956,-3.61033211297022));
#168346=CARTESIAN_POINT('Ctrl Pts',(2.65488489768749,7.31921844154152,-3.63360767977228));
#168347=CARTESIAN_POINT('Ctrl Pts',(2.62249728918549,7.30334972886251,-3.657049530288));
#168348=CARTESIAN_POINT('Ctrl Pts',(2.58964713363384,7.28763196712734,-3.68017390967919));
#168349=CARTESIAN_POINT('Ctrl Pts',(2.55836408484669,7.27266401647599,-3.70219514752476));
#168350=CARTESIAN_POINT('Ctrl Pts',(2.52666178542208,7.25783282024199,-3.72392848149313));
#168351=CARTESIAN_POINT('Ctrl Pts',(2.49511365861142,7.24340693925133,-3.74495613870205));
#168352=CARTESIAN_POINT('Ctrl Pts',(2.37311356491555,7.18762046282849,-3.82627241351892));
#168353=CARTESIAN_POINT('Ctrl Pts',(2.24760162177669,7.13517639135551,-3.90130500623051));
#168354=CARTESIAN_POINT('Ctrl Pts',(2.11872654046758,7.08653423928513,-3.97005391683681));
#168355=CARTESIAN_POINT('Ctrl Pts',(2.04263766891244,7.05781552637762,-4.01064381967561));
#168356=CARTESIAN_POINT('Ctrl Pts',(1.96537740848167,7.03042227465128,-4.04904334694059));
#168357=CARTESIAN_POINT('Ctrl Pts',(1.8869848690675,7.00445014911552,-4.08525249863175));
#168358=CARTESIAN_POINT('Ctrl Pts',(1.87314229700001,6.99986398540452,-4.09164631870103));
#168359=CARTESIAN_POINT('Ctrl Pts',(1.85790374991078,6.99487575520629,-4.09859060754057));
#168360=CARTESIAN_POINT('Ctrl Pts',(1.84288700698222,6.99002911745638,-4.10533727720669));
#168361=CARTESIAN_POINT('Ctrl Pts',(1.83881362435573,6.98871443756199,-4.10716735228591));
#168362=CARTESIAN_POINT('Ctrl Pts',(1.83475665548124,6.98740989315202,-4.10898288657522));
#168363=CARTESIAN_POINT('Ctrl Pts',(1.83074859787505,6.98612569517158,-4.11076894900098));
#168364=CARTESIAN_POINT('Ctrl Pts',(1.81196462152168,6.98010723264741,-4.11913942609173));
#168365=CARTESIAN_POINT('Ctrl Pts',(1.79314236940019,6.97417864273424,-4.12737489680932));
#168366=CARTESIAN_POINT('Ctrl Pts',(1.77428267733507,6.96834046885995,-4.13547536115374));
#168367=CARTESIAN_POINT('Ctrl Pts',(1.73656329320483,6.95666412111137,-4.15167628984257));
#168368=CARTESIAN_POINT('Ctrl Pts',(1.69869414644819,6.9453494464497,-4.16733719303872));
#168369=CARTESIAN_POINT('Ctrl Pts',(1.66068202046566,6.93440070531241,-4.18245807074219));
#168370=CARTESIAN_POINT('Ctrl Pts',(1.5846577685006,6.91250322303784,-4.21269982614912));
#168371=CARTESIAN_POINT('Ctrl Pts',(1.50806156945806,6.89206961920218,-4.24078147958532));
#168372=CARTESIAN_POINT('Ctrl Pts',(1.43094874130287,6.87313242815974,-4.26670303105079));
#168373=CARTESIAN_POINT('Ctrl Pts',(1.27672308499251,6.83525804607485,-4.31854613398173));
#168374=CARTESIAN_POINT('Ctrl Pts',(1.12043027318078,6.80337178041132,-4.36174882902975));
#168375=CARTESIAN_POINT('Ctrl Pts',(0.96253845475154,6.77770992578678,-4.39631111619484));
#168376=CARTESIAN_POINT('Ctrl Pts',(0.800364980059648,6.75135218177635,
-4.43181065162754));
#168377=CARTESIAN_POINT('Ctrl Pts',(0.636504625900533,6.73156143197304,
-4.45819481005927));
#168378=CARTESIAN_POINT('Ctrl Pts',(0.471495850994567,6.71855438355452,
-4.47546359149004));
#168379=CARTESIAN_POINT('Ctrl Pts',(0.315200102134448,6.70623415165054,
-4.4918205223694));
#168380=CARTESIAN_POINT('Ctrl Pts',(0.157874404222107,6.70000000004701,
-4.49999930673615));
#168381=CARTESIAN_POINT('Ctrl Pts',(1.78651616390521E-9,6.7,-4.4999999445903));
#168382=CARTESIAN_POINT('Origin',(-1.06251812903579E-14,12.7,-3.));
#168383=CARTESIAN_POINT('',(0.,0.,0.));
#168384=CARTESIAN_POINT('Origin',(0.0261679780000001,13.199314767,-5.7));
#168385=CARTESIAN_POINT('',(0.0261679780000018,10.699314766933,-5.69999999993301));
#168386=CARTESIAN_POINT('',(0.0261679779999998,15.699314767,-5.7));
#168387=CARTESIAN_POINT('Origin',(0.026167978,13.199314767,-5.7));
#168388=CARTESIAN_POINT('',(0.0261679779999998,15.699314767,-3.));
#168389=CARTESIAN_POINT('',(0.0261679779999998,15.699314767,-5.7));
#168390=CARTESIAN_POINT('Origin',(0.0261679780000001,13.199314767,-3.));
#168391=CARTESIAN_POINT('Origin',(0.026167978,13.199314767,-5.7));
#168392=CARTESIAN_POINT('Origin',(0.0261679780000001,13.199314767,5.7));
#168393=CARTESIAN_POINT('',(0.0261679779999998,15.6993147670816,5.69999999999998));
#168394=CARTESIAN_POINT('Origin',(0.026167978,13.199314767,5.7));
#168395=CARTESIAN_POINT('',(0.0261679779999998,15.9993147666625,6.00000000000001));
#168396=CARTESIAN_POINT('',(0.0261679779999998,15.6993147670816,5.7));
#168397=CARTESIAN_POINT('Origin',(0.026167978,13.199314767,6.));
#168398=CARTESIAN_POINT('Origin',(0.0261679780000001,13.199314767,3.));
#168399=CARTESIAN_POINT('',(0.0261679779999998,15.699314767,3.));
#168400=CARTESIAN_POINT('Origin',(0.0261679780000001,13.199314767,3.));
#168401=CARTESIAN_POINT('',(0.0261679779999998,15.699314767,3.));
#168402=CARTESIAN_POINT('Origin',(35.6555372325844,21.0677405729214,-4.33680868994202E-16));
#168403=CARTESIAN_POINT('',(43.8189844867682,11.730667947175,-3.90000000000325));
#168404=CARTESIAN_POINT('',(43.8189844868826,11.7306679470941,3.89999999937797));
#168405=CARTESIAN_POINT('Ctrl Pts',(43.8189844868367,11.7306679473376,-3.89999999999328));
#168406=CARTESIAN_POINT('Ctrl Pts',(43.9921002135057,11.6184247178878,-3.26642536031861));
#168407=CARTESIAN_POINT('Ctrl Pts',(44.1237435983594,11.5342903200696,-2.6179058686186));
#168408=CARTESIAN_POINT('Ctrl Pts',(44.2980963496193,11.4231842651665,-1.3114086441359));
#168409=CARTESIAN_POINT('Ctrl Pts',(44.3417418637512,11.3956060716702,-0.656384194552197));
#168410=CARTESIAN_POINT('Ctrl Pts',(44.3417382179344,11.3956083818323,0.656451728908009));
#168411=CARTESIAN_POINT('Ctrl Pts',(44.2980910327637,11.4231876412423,1.31146115586157));
#168412=CARTESIAN_POINT('Ctrl Pts',(44.1237385818983,11.5342935290692,2.61793059663588));
#168413=CARTESIAN_POINT('Ctrl Pts',(43.9920969099076,11.6184268598461,3.26643745082936));
#168414=CARTESIAN_POINT('Ctrl Pts',(43.8189844870025,11.7306679472301,3.89999999938663));
#168415=CARTESIAN_POINT('',(41.8585587172852,9.96549265511137,3.89999999906035));
#168416=CARTESIAN_POINT('',(42.899814893435,10.9030439275682,3.89999999977706));
#168417=CARTESIAN_POINT('',(41.8585587171356,9.9654926551616,-3.89999999979706));
#168418=CARTESIAN_POINT('Ctrl Pts',(41.8585587170749,9.96549265526622,3.89999999897544));
#168419=CARTESIAN_POINT('Ctrl Pts',(42.0425841023629,9.84617591879291,3.22649783117755));
#168420=CARTESIAN_POINT('Ctrl Pts',(42.1797151875545,9.75863037516518,2.53619779817488));
#168421=CARTESIAN_POINT('Ctrl Pts',(42.3430786805369,9.65460011496585,1.22769191823626));
#168422=CARTESIAN_POINT('Ctrl Pts',(42.3813156568265,9.63043105679415,0.614404332577125));
#168423=CARTESIAN_POINT('Ctrl Pts',(42.381312885009,9.63043281314897,-0.614474833094867));
#168424=CARTESIAN_POINT('Ctrl Pts',(42.3430726881961,9.65460391064827,-1.22776580224464));
#168425=CARTESIAN_POINT('Ctrl Pts',(42.1797051458808,9.75863679307803,-2.53624838517435));
#168426=CARTESIAN_POINT('Ctrl Pts',(42.0425773519183,9.84618029558489,-3.2265225368096));
#168427=CARTESIAN_POINT('Ctrl Pts',(41.8585587168806,9.96549265539219,-3.89999999968654));
#168428=CARTESIAN_POINT('',(42.7547095826604,10.7723905189662,-3.90000000032325));
#168429=CARTESIAN_POINT('Origin',(0.0261679780000021,13.199314767,-5.7));
#168430=CARTESIAN_POINT('',(0.0261679780000023,10.3993147672851,-5.99999999999998));
#168431=CARTESIAN_POINT('',(0.0261679780000018,10.699314766866,-5.69999999999999));
#168432=CARTESIAN_POINT('Origin',(0.026167978,13.199314767,-6.));
#168433=CARTESIAN_POINT('Origin',(-3.0444397003393E-13,12.7,6.));
#168434=CARTESIAN_POINT('',(0.0871991420266949,18.6993663254969,5.99999999999862));
#168435=CARTESIAN_POINT('',(5.86033332496759,11.41295170178,6.));
#168436=CARTESIAN_POINT('Origin',(-3.0444397003393E-13,12.7,6.));
#168437=CARTESIAN_POINT('',(-0.481485079125861,18.6806498075813,3.0000000012892));
#168438=CARTESIAN_POINT('Ctrl Pts',(0.0871991550143243,18.6993663259332,
5.99999999693977));
#168439=CARTESIAN_POINT('Ctrl Pts',(-0.0465256260974608,18.7013099791932,
5.43225701180379));
#168440=CARTESIAN_POINT('Ctrl Pts',(-0.170111683726753,18.698530803951,
4.85911197841162));
#168441=CARTESIAN_POINT('Ctrl Pts',(-0.354890542940252,18.6900112704791,
3.85702009702669));
#168442=CARTESIAN_POINT('Ctrl Pts',(-0.42398963631069,18.6852786018039,
3.42948219354828));
#168443=CARTESIAN_POINT('Ctrl Pts',(-0.481485043323748,18.6806498107172,
2.99999999710726));
#168444=CARTESIAN_POINT('',(4.74822287554126,9.0319787999811,3.));
#168445=CARTESIAN_POINT('Origin',(-3.04557785278657E-13,12.7,3.));
#168446=CARTESIAN_POINT('',(4.74822287554126,9.0319787999811,-3.));
#168447=CARTESIAN_POINT('',(4.74822287494953,9.03197880000176,3.));
#168448=CARTESIAN_POINT('',(-0.481484270649411,18.6806498727476,-2.99999999903635));
#168449=CARTESIAN_POINT('Origin',(-1.90684057085888E-14,12.7,-3.));
#168450=CARTESIAN_POINT('',(0.087199142033475,18.6993663256232,-6.00000000133027));
#168451=CARTESIAN_POINT('Ctrl Pts',(-0.48148424584236,18.6806498749201,
-2.99999999521028));
#168452=CARTESIAN_POINT('Ctrl Pts',(-0.423989360136962,18.6852786163215,
-3.42948205870502));
#168453=CARTESIAN_POINT('Ctrl Pts',(-0.35489187828681,18.6900111859768,
-3.85701912903971));
#168454=CARTESIAN_POINT('Ctrl Pts',(-0.185541740556634,18.697819402295,
-4.77544283505271));
#168455=CARTESIAN_POINT('Ctrl Pts',(-0.0909082385386381,18.7019550683862,
-5.24382584688238));
#168456=CARTESIAN_POINT('Ctrl Pts',(0.0871991554604803,18.6993663259267,
-5.99999999883431));
#168457=CARTESIAN_POINT('',(5.86033332447927,11.4129517005848,-6.0000000006689));
#168458=CARTESIAN_POINT('Origin',(-3.04899231012839E-13,12.7,-6.));
#168459=CARTESIAN_POINT('Ctrl Pts',(5.86033332441326,11.412951699256,6.));
#168460=CARTESIAN_POINT('Ctrl Pts',(5.86261002860425,11.4233182474286,5.8983154161611));
#168461=CARTESIAN_POINT('Ctrl Pts',(5.86485847361021,11.4336874083783,5.79662961576286));
#168462=CARTESIAN_POINT('Ctrl Pts',(5.868448699,11.450459003,5.632194411));
#168463=CARTESIAN_POINT('Ctrl Pts',(5.869807969,11.456859941,5.569445715));
#168464=CARTESIAN_POINT('Ctrl Pts',(5.871830748,11.466462662,5.475322));
#168465=CARTESIAN_POINT('Ctrl Pts',(5.87250232,11.469663788,5.443947316));
#168466=CARTESIAN_POINT('Ctrl Pts',(5.873505647,11.474465796,5.39688512));
#168467=CARTESIAN_POINT('Ctrl Pts',(5.873839418,11.476066519,5.381197693));
#168468=CARTESIAN_POINT('Ctrl Pts',(5.874339066,11.478467682,5.357666509));
#168469=CARTESIAN_POINT('Ctrl Pts',(5.874505448,11.479268083,5.349822774));
#168470=CARTESIAN_POINT('Ctrl Pts',(5.874754768,11.480468704,5.338057161));
#168471=CARTESIAN_POINT('Ctrl Pts',(5.874837833,11.480868914,5.334135288));
#168472=CARTESIAN_POINT('Ctrl Pts',(5.874962367,11.481469234,5.328252476));
#168473=CARTESIAN_POINT('Ctrl Pts',(5.87500386,11.481669303,5.326291527));
#168474=CARTESIAN_POINT('Ctrl Pts',(5.875086766,11.482069161,5.322369546));
#168475=CARTESIAN_POINT('Ctrl Pts',(5.875128186,11.482268981,5.320408522));
#168476=CARTESIAN_POINT('Ctrl Pts',(5.880467048,11.508031537,5.067432231));
#168477=CARTESIAN_POINT('Ctrl Pts',(5.885220146,11.531803076,4.815812574));
#168478=CARTESIAN_POINT('Ctrl Pts',(5.898038406,11.597664362,4.059816839));
#168479=CARTESIAN_POINT('Ctrl Pts',(5.904669074,11.634275422,3.5546825));
#168480=CARTESIAN_POINT('Ctrl Pts',(5.914950781,11.692903678,2.542161979));
#168481=CARTESIAN_POINT('Ctrl Pts',(5.918600378,11.714915645,2.03477498));
#168482=CARTESIAN_POINT('Ctrl Pts',(5.922211942,11.736952169,1.272010148));
#168483=CARTESIAN_POINT('Ctrl Pts',(5.923102816,11.742468341,1.017360989));
#168484=CARTESIAN_POINT('Ctrl Pts',(5.924286082,11.749816719,0.508071237));
#168485=CARTESIAN_POINT('Ctrl Pts',(5.924578584,11.751649539,0.253521895));
#168486=CARTESIAN_POINT('Ctrl Pts',(5.924576429,11.751636075,-0.509840295));
#168487=CARTESIAN_POINT('Ctrl Pts',(5.923413308,11.744282385,-1.01836763));
#168488=CARTESIAN_POINT('Ctrl Pts',(5.919803707,11.722258,-1.780587582));
#168489=CARTESIAN_POINT('Ctrl Pts',(5.918286894,11.713083094,-2.034565643));
#168490=CARTESIAN_POINT('Ctrl Pts',(5.91457177,11.691057231,-2.542330331));
#168491=CARTESIAN_POINT('Ctrl Pts',(5.912372151,11.678198728,-2.796229212));
#168492=CARTESIAN_POINT('Ctrl Pts',(5.904645385,11.634142573,-3.556755763));
#168493=CARTESIAN_POINT('Ctrl Pts',(5.898005992,11.597492508,-4.061961581));
#168494=CARTESIAN_POINT('Ctrl Pts',(5.885197279,11.531688249,-4.817044188));
#168495=CARTESIAN_POINT('Ctrl Pts',(5.880449993,11.50794786,-5.068283718));
#168496=CARTESIAN_POINT('Ctrl Pts',(5.875073803,11.48200658,-5.322984668));
#168497=CARTESIAN_POINT('Ctrl Pts',(5.874990938,11.481606943,-5.326903007));
#168498=CARTESIAN_POINT('Ctrl Pts',(5.874825036,11.480807249,-5.334739577));
#168499=CARTESIAN_POINT('Ctrl Pts',(5.874742043,11.480407405,-5.338657861));
#168500=CARTESIAN_POINT('Ctrl Pts',(5.874492938,11.479207884,-5.35041271));
#168501=CARTESIAN_POINT('Ctrl Pts',(5.8743267,11.478408216,-5.35824927));
#168502=CARTESIAN_POINT('Ctrl Pts',(5.873827484,11.47600925,-5.381758936));
#168503=CARTESIAN_POINT('Ctrl Pts',(5.873494003,11.474409991,-5.397432027));
#168504=CARTESIAN_POINT('Ctrl Pts',(5.872491546,11.469612372,-5.44445124));
#168505=CARTESIAN_POINT('Ctrl Pts',(5.871820559,11.466414169,-5.475797302));
#168506=CARTESIAN_POINT('Ctrl Pts',(5.869799547,11.456820204,-5.569835256));
#168507=CARTESIAN_POINT('Ctrl Pts',(5.868441471,11.450425087,-5.632526913));
#168508=CARTESIAN_POINT('Ctrl Pts',(5.86485441801766,11.4336687031271,-5.79681304737971));
#168509=CARTESIAN_POINT('Ctrl Pts',(5.86260797772381,11.4233089067647,-5.8984070333042));
#168510=CARTESIAN_POINT('Ctrl Pts',(5.86033332291787,11.4129516980425,-6.00000000037477));
#168511=CARTESIAN_POINT('Ctrl Pts',(42.0911037142801,9.36912484717797,6.00000101283007));
#168512=CARTESIAN_POINT('Ctrl Pts',(39.3678508886227,12.3936035172147,6.00000101283007));
#168513=CARTESIAN_POINT('Ctrl Pts',(42.4790155504863,9.71840223321708,2.01993501455923));
#168514=CARTESIAN_POINT('Ctrl Pts',(39.7557627238316,12.7428809032538,2.01993501455923));
#168515=CARTESIAN_POINT('Ctrl Pts',(42.479015550558,9.71840223328166,-2.01993501234435));
#168516=CARTESIAN_POINT('Ctrl Pts',(39.7557627239033,12.7428809033184,-2.01993501234435));
#168517=CARTESIAN_POINT('Ctrl Pts',(42.091103714491,9.36912484736789,-6.00000101066592));
#168518=CARTESIAN_POINT('Ctrl Pts',(39.3678508888336,12.3936035174046,-6.00000101066592));
#168519=CARTESIAN_POINT('',(39.775504930057,11.9408580355491,5.99999999959819));
#168520=CARTESIAN_POINT('Ctrl Pts',(41.8585587171188,9.96549265521474,3.89999999899657));
#168521=CARTESIAN_POINT('Ctrl Pts',(41.7915034664367,10.0089693400172,4.14541101470715));
#168522=CARTESIAN_POINT('Ctrl Pts',(41.7027507173744,10.0749332406404,4.37982730885032));
#168523=CARTESIAN_POINT('Ctrl Pts',(41.437560283558,10.2895240148895,4.91537047100115));
#168524=CARTESIAN_POINT('Ctrl Pts',(41.2418079413878,10.460439951812,5.19304888977805));
#168525=CARTESIAN_POINT('Ctrl Pts',(40.8236778904308,10.850802708163,5.61258586872592));
#168526=CARTESIAN_POINT('Ctrl Pts',(40.610008609833,11.0595809772413,5.76374643619597));
#168527=CARTESIAN_POINT('Ctrl Pts',(40.1857028808254,11.4944486152704,5.95378049605652));
#168528=CARTESIAN_POINT('Ctrl Pts',(39.9789697604729,11.7148874485651,5.99999999926869));
#168529=CARTESIAN_POINT('Ctrl Pts',(39.7755049300962,11.9408580355844,5.99999999919638));
#168530=CARTESIAN_POINT('',(39.5935147935475,12.1429785621987,5.99999995227989));
#168531=CARTESIAN_POINT('',(39.5935147984967,12.1429785532113,6.));
#168532=CARTESIAN_POINT('',(39.5935148013839,12.1429785439757,-6.00000000014651));
#168533=CARTESIAN_POINT('Ctrl Pts',(39.5935148013912,12.1429785692612,5.99999985683968));
#168534=CARTESIAN_POINT('Ctrl Pts',(39.593592075,12.1435858512692,5.99646324807023));
#168535=CARTESIAN_POINT('Ctrl Pts',(39.5936896902506,12.1442118064789,5.99271350326619));
#168536=CARTESIAN_POINT('Ctrl Pts',(39.5937765000117,12.144828628235,5.98906773188485));
#168537=CARTESIAN_POINT('Ctrl Pts',(39.5938699396201,12.1454925579887,5.98514352514079));
#168538=CARTESIAN_POINT('Ctrl Pts',(39.5939626032986,12.1461563824849,5.98122029151821));
#168539=CARTESIAN_POINT('Ctrl Pts',(39.5940544909761,12.146820102571,5.97729802528116));
#168540=CARTESIAN_POINT('Ctrl Pts',(39.5944224915473,12.1494782323389,5.96158975780617));
#168541=CARTESIAN_POINT('Ctrl Pts',(39.5947780568862,12.1521346914483,5.94589701242429));
#168542=CARTESIAN_POINT('Ctrl Pts',(39.5951212720585,12.1547895263954,5.93021947088647));
#168543=CARTESIAN_POINT('Ctrl Pts',(39.5952931292047,12.156118874263,5.92236930060117));
#168544=CARTESIAN_POINT('Ctrl Pts',(39.5954610237497,12.1574487481375,5.91452309125952));
#168545=CARTESIAN_POINT('Ctrl Pts',(39.5956281799399,12.1587756919312,5.90668024908748));
#168546=CARTESIAN_POINT('Ctrl Pts',(39.5957954963177,12.1601039073498,5.89882989103356));
#168547=CARTESIAN_POINT('Ctrl Pts',(39.5959623996781,12.1614288363532,5.89098285012388));
#168548=CARTESIAN_POINT('Ctrl Pts',(39.5961288904336,12.1627504920826,5.88313908742715));
#168549=CARTESIAN_POINT('Ctrl Pts',(39.5974664033537,12.1733680882849,5.82012577528396));
#168550=CARTESIAN_POINT('Ctrl Pts',(39.5987773377349,12.1837745082137,5.75732404899093));
#168551=CARTESIAN_POINT('Ctrl Pts',(39.6000625634968,12.1939769494452,5.69471380270722));
#168552=CARTESIAN_POINT('Ctrl Pts',(39.6026595696063,12.2145926288025,5.56819969372396));
#168553=CARTESIAN_POINT('Ctrl Pts',(39.6051517709515,12.2343767961233,5.44246194528457));
#168554=CARTESIAN_POINT('Ctrl Pts',(39.6075453455177,12.2533801427068,5.31735075584711));
#168555=CARTESIAN_POINT('Ctrl Pts',(39.6114116087659,12.2840756311731,5.11526271543155));
#168556=CARTESIAN_POINT('Ctrl Pts',(39.6150182208478,12.3127158898712,4.91494819176507));
#168557=CARTESIAN_POINT('Ctrl Pts',(39.6183889244826,12.3394911559076,4.71569049103997));
#168558=CARTESIAN_POINT('Ctrl Pts',(39.6192601312818,12.3464116082377,4.66418947449));
#168559=CARTESIAN_POINT('Ctrl Pts',(39.6201155446289,12.3532072031859,4.61275903935556));
#168560=CARTESIAN_POINT('Ctrl Pts',(39.620955504257,12.3598806685914,4.5613867724762));
#168561=CARTESIAN_POINT('Ctrl Pts',(39.6242419008288,12.3859910352066,4.36038944341434));
#168562=CARTESIAN_POINT('Ctrl Pts',(39.6272921168251,12.4102367492395,4.16028291618282));
#168563=CARTESIAN_POINT('Ctrl Pts',(39.6301229565858,12.4327441129628,3.96032108945468));
#168564=CARTESIAN_POINT('Ctrl Pts',(39.6329590026703,12.4552928709844,3.75999150399772));
#168565=CARTESIAN_POINT('Ctrl Pts',(39.6355748578746,12.476096858426,3.55980715906955));
#168566=CARTESIAN_POINT('Ctrl Pts',(39.6379808835292,12.4952314004158,3.35901407164543));
#168567=CARTESIAN_POINT('Ctrl Pts',(39.6392292102487,12.5051590418709,3.25483589065287));
#168568=CARTESIAN_POINT('Ctrl Pts',(39.6404209470369,12.51463644471,3.15049378121363));
#168569=CARTESIAN_POINT('Ctrl Pts',(39.6415568549947,12.5236686576725,3.0458820293338));
#168570=CARTESIAN_POINT('Ctrl Pts',(39.6417868028536,12.5254970963389,3.02470491881986));
#168571=CARTESIAN_POINT('Ctrl Pts',(39.6420144594068,12.5273073143591,3.00351675988397));
#168572=CARTESIAN_POINT('Ctrl Pts',(39.6422398267747,12.5290993285967,2.98231667365158));
#168573=CARTESIAN_POINT('Ctrl Pts',(39.6465168551583,12.5631082262811,2.5799808280661));
#168574=CARTESIAN_POINT('Ctrl Pts',(39.6499129052792,12.5901115475324,2.17860979623499));
#168575=CARTESIAN_POINT('Ctrl Pts',(39.6524433523305,12.610231922441,1.77858172671342));
#168576=CARTESIAN_POINT('Ctrl Pts',(39.6549216196748,12.6299374002015,1.3868025345575));
#168577=CARTESIAN_POINT('Ctrl Pts',(39.6565696544995,12.6430411851066,0.996314889485204));
#168578=CARTESIAN_POINT('Ctrl Pts',(39.6574078822912,12.6497060239315,0.607453803531702));
#168579=CARTESIAN_POINT('Ctrl Pts',(39.6577121126954,12.6521249924141,0.466318700987944));
#168580=CARTESIAN_POINT('Ctrl Pts',(39.6579097212539,12.6536961879894,0.32539765540149));
#168581=CARTESIAN_POINT('Ctrl Pts',(39.6580018598091,12.6544287847528,0.184705849465022));
#168582=CARTESIAN_POINT('Ctrl Pts',(39.6580386759582,12.6547215111974,0.128489095319149));
#168583=CARTESIAN_POINT('Ctrl Pts',(39.6580585448889,12.6548794892148,0.0732962827061743));
#168584=CARTESIAN_POINT('Ctrl Pts',(39.6580618011315,12.6549058756015,0.0164255705731008));
#168585=CARTESIAN_POINT('Ctrl Pts',(39.6580621134569,12.6549084064748,0.0109707664936554));
#168586=CARTESIAN_POINT('Ctrl Pts',(39.6580622680239,12.6549096875733,0.00550052285318253));
#168587=CARTESIAN_POINT('Ctrl Pts',(39.6580622619614,12.654909696507,1.24535000317211E-5));
#168588=CARTESIAN_POINT('Ctrl Pts',(39.6580622573028,12.6549097033719,-0.00420478650620587));
#168589=CARTESIAN_POINT('Ctrl Pts',(39.6580621581765,12.6549089583405,-0.00842206125982745));
#168590=CARTESIAN_POINT('Ctrl Pts',(39.6580619645721,12.654907461339,-0.0126393699191901));
#168591=CARTESIAN_POINT('Ctrl Pts',(39.6580434310409,12.6547641550369,-0.416357675171431));
#168592=CARTESIAN_POINT('Ctrl Pts',(39.6571585579766,12.6477254839266,-0.82038760970862));
#168593=CARTESIAN_POINT('Ctrl Pts',(39.6554014196392,12.6337528094906,-1.22436402282335));
#168594=CARTESIAN_POINT('Ctrl Pts',(39.6549935243686,12.6305092471041,-1.3181415386889));
#168595=CARTESIAN_POINT('Ctrl Pts',(39.6545386527295,12.6268922498283,-1.41191618938065));
#168596=CARTESIAN_POINT('Ctrl Pts',(39.6540367805458,12.6229017314022,-1.50568344113572));
#168597=CARTESIAN_POINT('Ctrl Pts',(39.6518789316225,12.6057441040828,-1.90884498271349));
#168598=CARTESIAN_POINT('Ctrl Pts',(39.6488521168538,12.5816768701136,-2.3118683700991));
#168599=CARTESIAN_POINT('Ctrl Pts',(39.6449594170072,12.550724154806,-2.71439124863566));
#168600=CARTESIAN_POINT('Ctrl Pts',(39.64415731637,12.5443462696235,-2.79733210461966));
#168601=CARTESIAN_POINT('Ctrl Pts',(39.6433184742028,12.537676217345,-2.88025173026906));
#168602=CARTESIAN_POINT('Ctrl Pts',(39.6424429513847,12.5307144788084,-2.96314699548041));
#168603=CARTESIAN_POINT('Ctrl Pts',(39.642277643315,12.5294000281332,-2.97879850792345));
#168604=CARTESIAN_POINT('Ctrl Pts',(39.6420987002013,12.5279771573245,-2.99559802050964));
#168605=CARTESIAN_POINT('Ctrl Pts',(39.641943068,12.5267399763259,-3.01009890988096));
#168606=CARTESIAN_POINT('Ctrl Pts',(39.6418152351274,12.5257237830207,-3.02200962198725));
#168607=CARTESIAN_POINT('Ctrl Pts',(39.6416865140263,12.5247005122664,-3.03393218069561));
#168608=CARTESIAN_POINT('Ctrl Pts',(39.6415569002152,12.5236701289684,-3.04586656515235));
#168609=CARTESIAN_POINT('Ctrl Pts',(39.6366369001502,12.484557893538,-3.49888288974479));
#168610=CARTESIAN_POINT('Ctrl Pts',(39.6304319642937,12.4351816259025,-3.96893688438699));
#168611=CARTESIAN_POINT('Ctrl Pts',(39.6226760900002,12.3735511564761,-4.45488827013432));
#168612=CARTESIAN_POINT('Ctrl Pts',(39.6221096259592,12.3690498657854,-4.49038059185758));
#168613=CARTESIAN_POINT('Ctrl Pts',(39.6215362581397,12.3644940511062,-4.52587230177962));
#168614=CARTESIAN_POINT('Ctrl Pts',(39.6209556744651,12.3598812745533,-4.56138140435976));
#168615=CARTESIAN_POINT('Ctrl Pts',(39.6187047513006,12.3419975378079,-4.69905021084013));
#168616=CARTESIAN_POINT('Ctrl Pts',(39.6163459195903,12.3232611011816,-4.83698069681983));
#168617=CARTESIAN_POINT('Ctrl Pts',(39.6138572018242,12.3034969681751,-4.97621973194427));
#168618=CARTESIAN_POINT('Ctrl Pts',(39.6118433777902,12.287504200091,-5.08888936416476));
#168619=CARTESIAN_POINT('Ctrl Pts',(39.609744395501,12.2708376377433,-5.20241573595815));
#168620=CARTESIAN_POINT('Ctrl Pts',(39.6075454849006,12.2533798111742,-5.31735177347078));
#168621=CARTESIAN_POINT('Ctrl Pts',(39.6051735931911,12.2345486344544,-5.44132945335634));
#168622=CARTESIAN_POINT('Ctrl Pts',(39.6026865372115,12.2148054121144,-5.56689293064617));
#168623=CARTESIAN_POINT('Ctrl Pts',(39.6000626637871,12.1939767452097,-5.69471430525968));
#168624=CARTESIAN_POINT('Ctrl Pts',(39.5987849050625,12.1838337213083,-5.75696001996335));
#168625=CARTESIAN_POINT('Ctrl Pts',(39.5974746226702,12.1734326499498,-5.81974212209882));
#168626=CARTESIAN_POINT('Ctrl Pts',(39.5961289372154,12.1627504039713,-5.88313927508247));
#168627=CARTESIAN_POINT('Ctrl Pts',(39.5959625743245,12.1614297912558,-5.89097686715119));
#168628=CARTESIAN_POINT('Ctrl Pts',(39.5957956701409,12.1601048790975,-5.89882385904714));
#168629=CARTESIAN_POINT('Ctrl Pts',(39.5956282185228,12.1587756206009,-5.90668039857604));
#168630=CARTESIAN_POINT('Ctrl Pts',(39.5954611918017,12.1574497350065,-5.91451700267563));
#168631=CARTESIAN_POINT('Ctrl Pts',(39.5952932983793,12.1561198748105,-5.92236316287808));
#168632=CARTESIAN_POINT('Ctrl Pts',(39.59512130112,12.154789472191,-5.93021958221744));
#168633=CARTESIAN_POINT('Ctrl Pts',(39.5947786320197,12.1521389190903,-5.94587187899884));
#168634=CARTESIAN_POINT('Ctrl Pts',(39.5944231052091,12.1494825187348,-5.96156430842148));
#168635=CARTESIAN_POINT('Ctrl Pts',(39.5940545004811,12.1468200840298,-5.97729806109937));
#168636=CARTESIAN_POINT('Ctrl Pts',(39.5939626487262,12.1461566381176,-5.98121871833759));
#168637=CARTESIAN_POINT('Ctrl Pts',(39.5938699849262,12.145492817321,-5.98514194177266));
#168638=CARTESIAN_POINT('Ctrl Pts',(39.5937765051849,12.1448286191576,-5.98906774952607));
#168639=CARTESIAN_POINT('Ctrl Pts',(39.5936897256473,12.1442120277047,-5.99271217319373));
#168640=CARTESIAN_POINT('Ctrl Pts',(39.5935921036083,12.1435860636139,-5.99646200266368));
#168641=CARTESIAN_POINT('Ctrl Pts',(39.5935147981916,12.1429785445163,-6.0000000001696));
#168642=CARTESIAN_POINT('',(39.7755049294992,11.9408580361687,-5.99999999959826));
#168643=CARTESIAN_POINT('',(39.775504929821,11.9408580357326,-6.));
#168644=CARTESIAN_POINT('Ctrl Pts',(39.7755049295383,11.9408580362039,-5.99999999919652));
#168645=CARTESIAN_POINT('Ctrl Pts',(39.9785184064207,11.7153887280077,-5.999999999353));
#168646=CARTESIAN_POINT('Ctrl Pts',(40.1847882503583,11.4954233907689,-5.95398529746107));
#168647=CARTESIAN_POINT('Ctrl Pts',(40.6081030675166,11.0614933541335,-5.76482235717356));
#168648=CARTESIAN_POINT('Ctrl Pts',(40.821279662875,10.8531281619462,-5.61439945620298));
#168649=CARTESIAN_POINT('Ctrl Pts',(41.2398722620509,10.4621498268799,-5.19565760275282));
#168650=CARTESIAN_POINT('Ctrl Pts',(41.4363530791327,10.2905364126708,-4.91747536111852));
#168651=CARTESIAN_POINT('Ctrl Pts',(41.702384420184,10.0752054541128,-4.38079376061105));
#168652=CARTESIAN_POINT('Ctrl Pts',(41.7913649514247,10.0090591491603,-4.14591795633693));
#168653=CARTESIAN_POINT('Ctrl Pts',(41.8585587169246,9.96549265534065,-3.89999999970769));
#168654=CARTESIAN_POINT('Origin',(41.9168260374617,13.8689122198355,-3.00000000000006));
#168655=CARTESIAN_POINT('',(41.7359306988266,13.7060333280929,-5.99999999959819));
#168656=CARTESIAN_POINT('',(41.7359306985475,13.7060333266355,-6.));
#168657=CARTESIAN_POINT('Ctrl Pts',(41.7359306988658,13.7060333281281,-5.99999999919639));
#168658=CARTESIAN_POINT('Ctrl Pts',(41.9400453487107,13.479341043567,-5.99999999940487));
#168659=CARTESIAN_POINT('Ctrl Pts',(42.1474454711246,13.2582206593349,-5.95348484309781));
#168660=CARTESIAN_POINT('Ctrl Pts',(42.5706384879709,12.8246056488402,-5.76333393612528));
#168661=CARTESIAN_POINT('Ctrl Pts',(42.7826771038137,12.6173958832382,-5.61342743869922));
#168662=CARTESIAN_POINT('Ctrl Pts',(43.1952883029083,12.2320043595518,-5.20066911826413));
#168663=CARTESIAN_POINT('Ctrl Pts',(43.3879766152324,12.0634062250566,-4.92990914760786));
#168664=CARTESIAN_POINT('Ctrl Pts',(43.6569747522941,11.8447245299816,-4.39611142481161));
#168665=CARTESIAN_POINT('Ctrl Pts',(43.7495964127534,11.7756569415571,-4.15395117442176));
#168666=CARTESIAN_POINT('Ctrl Pts',(43.8189870849516,11.7306662627757,-3.89999049146802));
#168667=CARTESIAN_POINT('Origin',(41.9168260374619,13.8689122198355,3.00000000000002));
#168668=CARTESIAN_POINT('',(41.7359306996812,13.7060333271437,5.99999999959818));
#168669=CARTESIAN_POINT('',(39.7755049300089,11.9408580353737,6.));
#168670=CARTESIAN_POINT('Ctrl Pts',(43.8189844870475,11.7306679471774,3.89999999940828));
#168671=CARTESIAN_POINT('Ctrl Pts',(43.7497368818761,11.7755660912359,4.1534346662405));
#168672=CARTESIAN_POINT('Ctrl Pts',(43.6573576179347,11.8444391213823,4.39511093543262));
#168673=CARTESIAN_POINT('Ctrl Pts',(43.3892130900103,12.0623655059657,4.92778647249781));
#168674=CARTESIAN_POINT('Ctrl Pts',(43.1972403553305,12.2302769996148,5.19805904759368));
#168675=CARTESIAN_POINT('Ctrl Pts',(42.7850817396402,12.6150648732738,5.61160449838341));
#168676=CARTESIAN_POINT('Ctrl Pts',(42.572559062314,12.822679247634,5.76224353382663));
#168677=CARTESIAN_POINT('Ctrl Pts',(42.1483768580881,13.2572282605142,5.95327516155663));
#168678=CARTESIAN_POINT('Ctrl Pts',(41.9405049600971,13.4788305934348,5.99999999927515));
#168679=CARTESIAN_POINT('Ctrl Pts',(41.7359306997204,13.706033327179,5.99999999919635));
#168680=CARTESIAN_POINT('Ctrl Pts',(39.592093664,12.131166347,6.068318707));
#168681=CARTESIAN_POINT('Ctrl Pts',(39.076055002,12.687534913,6.153779637));
#168682=CARTESIAN_POINT('Ctrl Pts',(38.316324576,12.76466494,6.151311746));
#168683=CARTESIAN_POINT('Ctrl Pts',(39.59240577,12.133760521,6.053314685));
#168684=CARTESIAN_POINT('Ctrl Pts',(39.076369283,12.690126742,6.138775261));
#168685=CARTESIAN_POINT('Ctrl Pts',(38.31664227,12.767258547,6.136307738));
#168686=CARTESIAN_POINT('Ctrl Pts',(39.592717877,12.136354695,6.038310664));
#168687=CARTESIAN_POINT('Ctrl Pts',(39.076683564,12.692718572,6.123770877));
#168688=CARTESIAN_POINT('Ctrl Pts',(38.316959963,12.769852155,6.121303731));
#168689=CARTESIAN_POINT('Ctrl Pts',(39.593186037,12.140245955,6.015804631));
#168690=CARTESIAN_POINT('Ctrl Pts',(39.077154985,12.696606319,6.101264295));
#168691=CARTESIAN_POINT('Ctrl Pts',(38.317436504,12.773742566,6.09879772));
#168692=CARTESIAN_POINT('Ctrl Pts',(39.593338947,12.141540209,6.008334889));
#168693=CARTESIAN_POINT('Ctrl Pts',(39.077309654,12.697899291,6.093780344));
#168694=CARTESIAN_POINT('Ctrl Pts',(38.317595353,12.775039369,6.091295716));
#168695=CARTESIAN_POINT('Ctrl Pts',(39.593577743,12.143490089,5.99703347));
#168696=CARTESIAN_POINT('Ctrl Pts',(39.077549071,12.699847579,6.08249969100001));
#168697=CARTESIAN_POINT('Ctrl Pts',(38.317833619,12.776984575,6.08004271));
#168698=CARTESIAN_POINT('Ctrl Pts',(39.593683639,12.144164263,5.99299088));
#168699=CARTESIAN_POINT('Ctrl Pts',(39.07764945,12.700522186,6.078583732));
#168700=CARTESIAN_POINT('Ctrl Pts',(38.317912503,12.777633031,6.076291707));
#168701=CARTESIAN_POINT('Ctrl Pts',(39.593870468,12.1454918,5.9851444));
#168702=CARTESIAN_POINT('Ctrl Pts',(39.077830235,12.701849801,6.07088678500001));
#168703=CARTESIAN_POINT('Ctrl Pts',(38.318068603,12.778930113,6.068789696));
#168704=CARTESIAN_POINT('Ctrl Pts',(39.59396313,12.146155627,5.981221165));
#168705=CARTESIAN_POINT('Ctrl Pts',(39.077919885,12.702513685,6.067038314));
#168706=CARTESIAN_POINT('Ctrl Pts',(38.318145913,12.779578729,6.065038689));
#168707=CARTESIAN_POINT('Ctrl Pts',(39.594422671,12.149475055,5.961605011));
#168708=CARTESIAN_POINT('Ctrl Pts',(39.078364424,12.7058335,6.047795871));
#168709=CARTESIAN_POINT('Ctrl Pts',(38.318528768,12.782822185,6.046283644));
#168710=CARTESIAN_POINT('Ctrl Pts',(39.594778254,12.152131539,5.945912161));
#168711=CARTESIAN_POINT('Ctrl Pts',(39.078708173,12.708490553,6.03240203800001));
#168712=CARTESIAN_POINT('Ctrl Pts',(38.318823224,12.785418148,6.031279577));
#168713=CARTESIAN_POINT('Ctrl Pts',(39.595293565,12.156117675,5.922372994));
#168714=CARTESIAN_POINT('Ctrl Pts',(39.079205987,12.71247794,6.009311436));
#168715=CARTESIAN_POINT('Ctrl Pts',(38.319247178,12.789313893,6.008773432));
#168716=CARTESIAN_POINT('Ctrl Pts',(39.595461458,12.157447556,5.914526772));
#168717=CARTESIAN_POINT('Ctrl Pts',(39.079367313,12.713800705,6.001658908));
#168718=CARTESIAN_POINT('Ctrl Pts',(38.3193833,12.790600397,6.001348676));
#168719=CARTESIAN_POINT('Ctrl Pts',(39.595795923,12.160102727,5.898833554));
#168720=CARTESIAN_POINT('Ctrl Pts',(39.079699563,12.716547187,5.985742981));
#168721=CARTESIAN_POINT('Ctrl Pts',(38.319673324,12.793353081,5.985433552));
#168722=CARTESIAN_POINT('Ctrl Pts',(39.595962823,12.161427665,5.890986501));
#168723=CARTESIAN_POINT('Ctrl Pts',(39.079865358,12.71791769,5.97778454500001));
#168724=CARTESIAN_POINT('Ctrl Pts',(38.319818049,12.794726679,5.977475519));
#168725=CARTESIAN_POINT('Ctrl Pts',(39.597461918,12.173328269,5.820359025));
#168726=CARTESIAN_POINT('Ctrl Pts',(39.081354587,12.730227887,5.906152583));
#168727=CARTESIAN_POINT('Ctrl Pts',(38.321117997,12.807064359,5.905848986));
#168728=CARTESIAN_POINT('Ctrl Pts',(39.598773123,12.183737104,5.757550619));
#168729=CARTESIAN_POINT('Ctrl Pts',(39.082657224,12.740994793,5.842451083));
#168730=CARTESIAN_POINT('Ctrl Pts',(38.322255163,12.817855555,5.842150827));
#168731=CARTESIAN_POINT('Ctrl Pts',(39.602642674,12.214455312,5.56903997));
#168732=CARTESIAN_POINT('Ctrl Pts',(39.086501869,12.77277097,5.651250253));
#168733=CARTESIAN_POINT('Ctrl Pts',(38.325611506,12.849702405,5.650965805));
#168734=CARTESIAN_POINT('Ctrl Pts',(39.605137062,12.234257258,5.443246713));
#168735=CARTESIAN_POINT('Ctrl Pts',(39.088980476,12.793254628,5.52366008399999));
#168736=CARTESIAN_POINT('Ctrl Pts',(38.327775614,12.870232221,5.52338273));
#168737=CARTESIAN_POINT('Ctrl Pts',(39.612362704,12.291625054,5.065558721));
#168738=CARTESIAN_POINT('Ctrl Pts',(39.096161745,12.852602028,5.140539372));
#168739=CARTESIAN_POINT('Ctrl Pts',(38.334045837,12.929709683,5.140305186));
#168740=CARTESIAN_POINT('Ctrl Pts',(39.616832291,12.327120707,4.813571576));
#168741=CARTESIAN_POINT('Ctrl Pts',(39.100604791,12.889321181,4.884922274));
#168742=CARTESIAN_POINT('Ctrl Pts',(38.337926232,12.96651201,4.884701294));
#168743=CARTESIAN_POINT('Ctrl Pts',(39.629202178,12.425400322,4.057017133));
#168744=CARTESIAN_POINT('Ctrl Pts',(39.112905272,12.991004201,4.117328691));
#168745=CARTESIAN_POINT('Ctrl Pts',(38.348668923,13.068413471,4.117224781));
#168746=CARTESIAN_POINT('Ctrl Pts',(39.636062814,12.479982592,3.551857239));
#168747=CARTESIAN_POINT('Ctrl Pts',(39.119729727,13.047470758,3.604789474));
#168748=CARTESIAN_POINT('Ctrl Pts',(38.354631783,13.125013103,3.604687756));
#168749=CARTESIAN_POINT('Ctrl Pts',(39.652544937,12.611040789,2.03393161));
#168750=CARTESIAN_POINT('Ctrl Pts',(39.13613297,13.183094783,2.064203406));
#168751=CARTESIAN_POINT('Ctrl Pts',(38.368964592,13.260927701,2.064336404));
#168752=CARTESIAN_POINT('Ctrl Pts',(39.658062289,12.654909258,1.018725573));
#168753=CARTESIAN_POINT('Ctrl Pts',(39.14162554,13.228470363,1.034037942));
#168754=CARTESIAN_POINT('Ctrl Pts',(38.37376987,13.306425053,1.034006735));
#168755=CARTESIAN_POINT('Ctrl Pts',(39.658062379,12.654909975,-1.018700666));
#168756=CARTESIAN_POINT('Ctrl Pts',(39.141625629,13.228471105,-1.034012664));
#168757=CARTESIAN_POINT('Ctrl Pts',(38.373769948,13.306425797,-1.033981454));
#168758=CARTESIAN_POINT('Ctrl Pts',(39.652545109,12.611042157,-2.033910583));
#168759=CARTESIAN_POINT('Ctrl Pts',(39.136133141,13.183096198,-2.064182064));
#168760=CARTESIAN_POINT('Ctrl Pts',(38.368964742,13.26092912,-2.064315063));
#168761=CARTESIAN_POINT('Ctrl Pts',(39.63606298,12.479983912,-3.55184454));
#168762=CARTESIAN_POINT('Ctrl Pts',(39.119729893,13.047472124,-3.604776588));
#168763=CARTESIAN_POINT('Ctrl Pts',(38.354631928,13.125014472,-3.604674871));
#168764=CARTESIAN_POINT('Ctrl Pts',(39.62920232,12.425401455,-4.057007807));
#168765=CARTESIAN_POINT('Ctrl Pts',(39.112905414,12.991005374,-4.117319229));
#168766=CARTESIAN_POINT('Ctrl Pts',(38.348669047,13.068414646,-4.117215321));
#168767=CARTESIAN_POINT('Ctrl Pts',(39.616832352,12.327121184,-4.813568203));
#168768=CARTESIAN_POINT('Ctrl Pts',(39.10060485,12.889321675,-4.884918852));
#168769=CARTESIAN_POINT('Ctrl Pts',(38.337926284,12.966512505,-4.884697873));
#168770=CARTESIAN_POINT('Ctrl Pts',(39.612362728,12.29162525,-5.065557481));
#168771=CARTESIAN_POINT('Ctrl Pts',(39.09616177,12.852602231,-5.140538114));
#168772=CARTESIAN_POINT('Ctrl Pts',(38.334045859,12.929709886,-5.140303928));
#168773=CARTESIAN_POINT('Ctrl Pts',(39.605137019,12.234256923,-5.443248896));
#168774=CARTESIAN_POINT('Ctrl Pts',(39.088980434,12.793254281,-5.523662297));
#168775=CARTESIAN_POINT('Ctrl Pts',(38.327775578,12.870231873,-5.523384943));
#168776=CARTESIAN_POINT('Ctrl Pts',(39.602642659,12.214455194,-5.569040712));
#168777=CARTESIAN_POINT('Ctrl Pts',(39.086501854,12.772770847,-5.651251005));
#168778=CARTESIAN_POINT('Ctrl Pts',(38.325611493,12.849702281,-5.650966557));
#168779=CARTESIAN_POINT('Ctrl Pts',(39.598773114,12.183737037,-5.757551029));
#168780=CARTESIAN_POINT('Ctrl Pts',(39.082657215,12.740994723,-5.842451499));
#168781=CARTESIAN_POINT('Ctrl Pts',(38.322255156,12.817855485,-5.842151243));
#168782=CARTESIAN_POINT('Ctrl Pts',(39.597461912,12.173328219,-5.820359327));
#168783=CARTESIAN_POINT('Ctrl Pts',(39.081354581,12.730227835,-5.906152889));
#168784=CARTESIAN_POINT('Ctrl Pts',(38.321117991,12.807064306,-5.905849292));
#168785=CARTESIAN_POINT('Ctrl Pts',(39.595962819,12.161427634,-5.890986684));
#168786=CARTESIAN_POINT('Ctrl Pts',(39.079865354,12.717917658,-5.97778472999999));
#168787=CARTESIAN_POINT('Ctrl Pts',(38.319818046,12.794726647,-5.977475704));
#168788=CARTESIAN_POINT('Ctrl Pts',(39.59579592,12.160102699,-5.898833724));
#168789=CARTESIAN_POINT('Ctrl Pts',(39.079699559,12.716547157,-5.985743153));
#168790=CARTESIAN_POINT('Ctrl Pts',(38.319673321,12.793353052,-5.985433723));
#168791=CARTESIAN_POINT('Ctrl Pts',(39.595461455,12.157447531,-5.914526915));
#168792=CARTESIAN_POINT('Ctrl Pts',(39.07936731,12.71380068,-6.001659054));
#168793=CARTESIAN_POINT('Ctrl Pts',(38.319383298,12.790600372,-6.001348821));
#168794=CARTESIAN_POINT('Ctrl Pts',(39.595293562,12.156117653,-5.922373124));
#168795=CARTESIAN_POINT('Ctrl Pts',(39.079205984,12.712477918,-6.00931156300001));
#168796=CARTESIAN_POINT('Ctrl Pts',(38.319247176,12.789313871,-6.008773556));
#168797=CARTESIAN_POINT('Ctrl Pts',(39.594778252,12.152131523,-5.945912251));
#168798=CARTESIAN_POINT('Ctrl Pts',(39.078708171,12.708490538,-6.03240212699999));
#168799=CARTESIAN_POINT('Ctrl Pts',(38.318823223,12.785418134,-6.031279663));
#168800=CARTESIAN_POINT('Ctrl Pts',(39.594422669,12.149475044,-5.961605075));
#168801=CARTESIAN_POINT('Ctrl Pts',(39.078364422,12.705833489,-6.04779593400001));
#168802=CARTESIAN_POINT('Ctrl Pts',(38.318528767,12.782822174,-6.046283705));
#168803=CARTESIAN_POINT('Ctrl Pts',(39.593963129,12.146155621,-5.981221196));
#168804=CARTESIAN_POINT('Ctrl Pts',(39.077919884,12.70251368,-6.067038345));
#168805=CARTESIAN_POINT('Ctrl Pts',(38.318145912,12.779578724,-6.065038719));
#168806=CARTESIAN_POINT('Ctrl Pts',(39.593870468,12.145491795,-5.985144425));
#168807=CARTESIAN_POINT('Ctrl Pts',(39.077830234,12.701849797,-6.070886809));
#168808=CARTESIAN_POINT('Ctrl Pts',(38.318068602,12.778930109,-6.06878972));
#168809=CARTESIAN_POINT('Ctrl Pts',(39.593683639,12.144164261,-5.992990892));
#168810=CARTESIAN_POINT('Ctrl Pts',(39.07764945,12.700522184,-6.078583744));
#168811=CARTESIAN_POINT('Ctrl Pts',(38.317912503,12.777633029,-6.076291718));
#168812=CARTESIAN_POINT('Ctrl Pts',(39.593577743,12.143490088,-5.997033475));
#168813=CARTESIAN_POINT('Ctrl Pts',(39.077549071,12.699847578,-6.082499696));
#168814=CARTESIAN_POINT('Ctrl Pts',(38.317833619,12.776984574,-6.080042715));
#168815=CARTESIAN_POINT('Ctrl Pts',(39.593338947,12.141540211,-6.008334875));
#168816=CARTESIAN_POINT('Ctrl Pts',(39.077309655,12.697899294,-6.093780331));
#168817=CARTESIAN_POINT('Ctrl Pts',(38.317595353,12.775039371,-6.091295702));
#168818=CARTESIAN_POINT('Ctrl Pts',(39.593186038,12.14024596,-6.015804605));
#168819=CARTESIAN_POINT('Ctrl Pts',(39.077154985,12.696606323,-6.101264269));
#168820=CARTESIAN_POINT('Ctrl Pts',(38.317436504,12.77374257,-6.098797693));
#168821=CARTESIAN_POINT('Ctrl Pts',(39.592717878,12.136354706,-6.0383106));
#168822=CARTESIAN_POINT('Ctrl Pts',(39.076683565,12.692718583,-6.123770813));
#168823=CARTESIAN_POINT('Ctrl Pts',(38.316959965,12.769852166,-6.121303667));
#168824=CARTESIAN_POINT('Ctrl Pts',(39.592405772,12.133760536,-6.053314596));
#168825=CARTESIAN_POINT('Ctrl Pts',(39.076369285,12.690126757,-6.13877517200001));
#168826=CARTESIAN_POINT('Ctrl Pts',(38.316642272,12.767258563,-6.136307649));
#168827=CARTESIAN_POINT('Ctrl Pts',(39.592093666,12.131166367,-6.068318593));
#168828=CARTESIAN_POINT('Ctrl Pts',(39.076055005,12.687534933,-6.153779523));
#168829=CARTESIAN_POINT('Ctrl Pts',(38.316324579,12.76466496,-6.151311631));
#168830=CARTESIAN_POINT('',(38.3194078266977,12.7908331451233,-5.99999998228311));
#168831=CARTESIAN_POINT('',(38.3194078268329,12.7908331478054,5.99999997429129));
#168832=CARTESIAN_POINT('Ctrl Pts',(38.3194078303931,12.7908331817173,-5.99999994684931));
#168833=CARTESIAN_POINT('Ctrl Pts',(38.3194475682192,12.7912087694162,-5.99783007957096));
#168834=CARTESIAN_POINT('Ctrl Pts',(38.3194876939326,12.7915891814127,-5.99563172340608));
#168835=CARTESIAN_POINT('Ctrl Pts',(38.319528521751,12.7919766905508,-5.99339127208654));
#168836=CARTESIAN_POINT('Ctrl Pts',(38.3196735650741,12.7933533404767,-5.98543193167468));
#168837=CARTESIAN_POINT('Ctrl Pts',(38.3198182890647,12.7947269337395,-5.97747391585236));
#168838=CARTESIAN_POINT('Ctrl Pts',(38.3199626941277,12.7960974767983,-5.96951721386296));
#168839=CARTESIAN_POINT('Ctrl Pts',(38.3211202440174,12.8070837395616,-5.9057363510682));
#168840=CARTESIAN_POINT('Ctrl Pts',(38.3222573068458,12.8178740050506,-5.84203994285522));
#168841=CARTESIAN_POINT('Ctrl Pts',(38.3233741257768,12.8284710643812,-5.77842301440819));
#168842=CARTESIAN_POINT('Ctrl Pts',(38.3256191940973,12.8497736422066,-5.65053804868484));
#168843=CARTESIAN_POINT('Ctrl Pts',(38.3277825389442,12.870296302613,-5.52296986150142));
#168844=CARTESIAN_POINT('Ctrl Pts',(38.3298658277331,12.8900578615479,-5.39569127138992));
#168845=CARTESIAN_POINT('Ctrl Pts',(38.3340708096828,12.9299452737301,-5.13878777493661));
#168846=CARTESIAN_POINT('Ctrl Pts',(38.3379460181326,12.966698589345,-4.88329627876836));
#168847=CARTESIAN_POINT('Ctrl Pts',(38.3415073042792,13.0004798752819,-4.62887035569616));
#168848=CARTESIAN_POINT('Ctrl Pts',(38.3455434470947,13.0387655083149,-4.34051965338579));
#168849=CARTESIAN_POINT('Ctrl Pts',(38.3491761736271,13.0732364223088,-4.05353783913861));
#168850=CARTESIAN_POINT('Ctrl Pts',(38.3524253407918,13.1040650384041,-3.76741605704691));
#168851=CARTESIAN_POINT('Ctrl Pts',(38.3549900677902,13.1283995770772,-3.54156610160221));
#168852=CARTESIAN_POINT('Ctrl Pts',(38.3573156958337,13.15046365334,-3.31625193559478));
#168853=CARTESIAN_POINT('Ctrl Pts',(38.3594095624069,13.1703193516511,-3.09122160167224));
#168854=CARTESIAN_POINT('Ctrl Pts',(38.3620840178367,13.1956806525291,-2.80379469198174));
#168855=CARTESIAN_POINT('Ctrl Pts',(38.3643798369784,13.2174459453909,-2.51684851920759));
#168856=CARTESIAN_POINT('Ctrl Pts',(38.3663038029257,13.2356826405251,-2.22985396662523));
#168857=CARTESIAN_POINT('Ctrl Pts',(38.3682262152592,13.2539046094208,-1.94309116383032));
#168858=CARTESIAN_POINT('Ctrl Pts',(38.3697773754982,13.2686036771062,-1.65628007016979));
#168859=CARTESIAN_POINT('Ctrl Pts',(38.3709586208108,13.2797955404709,-1.36888890983398));
#168860=CARTESIAN_POINT('Ctrl Pts',(38.3721352867201,13.2909440156785,-1.08261189576711));
#168861=CARTESIAN_POINT('Ctrl Pts',(38.3729449015694,13.2986124318983,-0.795759314868996));
#168862=CARTESIAN_POINT('Ctrl Pts',(38.3733833859369,13.3027651339286,-0.50780148111664));
#168863=CARTESIAN_POINT('Ctrl Pts',(38.373640502044,13.3052001730298,-0.338950313963452));
#168864=CARTESIAN_POINT('Ctrl Pts',(38.3737699088722,13.3064254242396,-0.169719044683042));
#168865=CARTESIAN_POINT('Ctrl Pts',(38.3737699090002,13.3064254250023,-1.99360232965105E-7));
#168866=CARTESIAN_POINT('Ctrl Pts',(38.3737699090002,13.3064254250023,4.08059336375396E-6));
#168867=CARTESIAN_POINT('Ctrl Pts',(38.3737699090002,13.3064254250015,8.36054677588611E-6));
#168868=CARTESIAN_POINT('Ctrl Pts',(38.373769909,13.306425425,1.26405000035384E-5));
#168869=CARTESIAN_POINT('Ctrl Pts',(38.3737698980774,13.306425320815,0.289600606570371));
#168870=CARTESIAN_POINT('Ctrl Pts',(38.3733934350627,13.302860883464,0.577769581499957));
#168871=CARTESIAN_POINT('Ctrl Pts',(38.3726478095811,13.2957981256462,0.865052432993628));
#168872=CARTESIAN_POINT('Ctrl Pts',(38.3719001282633,13.2887158944158,1.15312737982036));
#168873=CARTESIAN_POINT('Ctrl Pts',(38.3707812417038,13.2781159920207,1.44031129655557));
#168874=CARTESIAN_POINT('Ctrl Pts',(38.3692929967903,13.2640129059284,1.72713722866002));
#168875=CARTESIAN_POINT('Ctrl Pts',(38.3678024134377,13.2498876600381,2.014413842596));
#168876=CARTESIAN_POINT('Ctrl Pts',(38.3659413080516,13.2322482009507,2.30133133418495));
#168877=CARTESIAN_POINT('Ctrl Pts',(38.3637060723775,13.211057273523,2.58842120747477));
#168878=CARTESIAN_POINT('Ctrl Pts',(38.3624018526689,13.1986927494975,2.75593297154826));
#168879=CARTESIAN_POINT('Ctrl Pts',(38.3609701579466,13.185118156905,2.92350334827925));
#168880=CARTESIAN_POINT('Ctrl Pts',(38.3594094157851,13.1703179659798,3.09123730533891));
#168881=CARTESIAN_POINT('Ctrl Pts',(38.3567565033852,13.1451609535038,3.37634749558842));
#168882=CARTESIAN_POINT('Ctrl Pts',(38.3537317291153,13.1164605661736,3.66191318681091));
#168883=CARTESIAN_POINT('Ctrl Pts',(38.3503195989016,13.0840851791422,3.94844622381797));
#168884=CARTESIAN_POINT('Ctrl Pts',(38.3476268373177,13.0585353926433,4.17457040615839));
#168885=CARTESIAN_POINT('Ctrl Pts',(38.3446927302622,13.0306958640117,4.40129696805432));
#168886=CARTESIAN_POINT('Ctrl Pts',(38.3415072284282,13.0004791536001,4.62887578969621));
#168887=CARTESIAN_POINT('Ctrl Pts',(38.3379459614551,12.9666980483206,4.88330004794792));
#168888=CARTESIAN_POINT('Ctrl Pts',(38.3340707814642,12.9299450098084,5.13878942487707));
#168889=CARTESIAN_POINT('Ctrl Pts',(38.3298658446338,12.8900580258576,5.39569021538999));
#168890=CARTESIAN_POINT('Ctrl Pts',(38.3277825733939,12.8702966335071,5.52296775842875));
#168891=CARTESIAN_POINT('Ctrl Pts',(38.325619205431,12.849773747823,5.65053740685728));
#168892=CARTESIAN_POINT('Ctrl Pts',(38.3233741350629,12.8284711523523,5.77842248640831));
#168893=CARTESIAN_POINT('Ctrl Pts',(38.3222573136357,12.8178740702233,5.84203955564889));
#168894=CARTESIAN_POINT('Ctrl Pts',(38.3211202497904,12.8070837874715,5.90573607444173));
#168895=CARTESIAN_POINT('Ctrl Pts',(38.3199626977756,12.7960975110998,5.96951701541865));
#168896=CARTESIAN_POINT('Ctrl Pts',(38.3198182923721,12.7947269656274,5.97747373131824));
#168897=CARTESIAN_POINT('Ctrl Pts',(38.3196735683827,12.7933533693638,5.98543176114177));
#168898=CARTESIAN_POINT('Ctrl Pts',(38.3195285245693,12.7919767175187,5.99339111408667));
#168899=CARTESIAN_POINT('Ctrl Pts',(38.3194876958478,12.7915892005779,5.99563161092288));
#168900=CARTESIAN_POINT('Ctrl Pts',(38.3194475692977,12.791208780971,5.99783001162888));
#168901=CARTESIAN_POINT('Ctrl Pts',(38.3194078306652,12.7908331857559,5.99999992287387));
#168902=CARTESIAN_POINT('Ctrl Pts',(39.5935147999063,12.1429785426452,-6.));
#168903=CARTESIAN_POINT('Ctrl Pts',(39.4299502083,12.3246348464625,-6.));
#168904=CARTESIAN_POINT('Ctrl Pts',(39.2346482743456,12.4748234427719,-6.));
#168905=CARTESIAN_POINT('Ctrl Pts',(38.7990187662661,12.6966740224187,-6.));
#168906=CARTESIAN_POINT('Ctrl Pts',(38.5626404589734,12.7662707484543,-6.));
#168907=CARTESIAN_POINT('Ctrl Pts',(38.3194078294636,12.7908331725129,-6.));
#168908=CARTESIAN_POINT('Ctrl Pts',(38.3194078293165,12.7908331723995,6.));
#168909=CARTESIAN_POINT('Ctrl Pts',(38.5626163926011,12.7662731786021,6.));
#168910=CARTESIAN_POINT('Ctrl Pts',(38.7989722118466,12.6966877715691,6.));
#168911=CARTESIAN_POINT('Ctrl Pts',(39.234609763126,12.4748530096939,6.));
#168912=CARTESIAN_POINT('Ctrl Pts',(39.4299340103852,12.3246528308041,6.));
#168913=CARTESIAN_POINT('Ctrl Pts',(39.5935147874398,12.1429785566993,6.));
#168914=CARTESIAN_POINT('Ctrl Pts',(44.0515296615211,11.1342999421954,-6.00000101620338));
#168915=CARTESIAN_POINT('Ctrl Pts',(40.5316975951668,15.0434694841942,-6.00000101620338));
#168916=CARTESIAN_POINT('Ctrl Pts',(44.4394414973113,11.4835773287603,-2.01993501424746));
#168917=CARTESIAN_POINT('Ctrl Pts',(40.919609431951,15.392746870759,-2.01993501424746));
#168918=CARTESIAN_POINT('Ctrl Pts',(44.4394414972397,11.4835773286958,2.01993501645796));
#168919=CARTESIAN_POINT('Ctrl Pts',(40.9196094318794,15.3927468706946,2.01993501645796));
#168920=CARTESIAN_POINT('Ctrl Pts',(44.0515296613106,11.1342999420059,6.00000101836325));
#168921=CARTESIAN_POINT('Ctrl Pts',(40.5316975949563,15.0434694840047,6.00000101836325));
#168922=CARTESIAN_POINT('',(40.7532527139649,14.7974077937632,5.99999999957928));
#168923=CARTESIAN_POINT('',(40.7532527139641,14.7974077951072,-5.99999999785059));
#168924=CARTESIAN_POINT('Ctrl Pts',(40.7532527144433,14.7974077941939,5.99999999873785));
#168925=CARTESIAN_POINT('Ctrl Pts',(40.7532924812137,14.7976753308601,5.99840954433184));
#168926=CARTESIAN_POINT('Ctrl Pts',(40.7533491101781,14.7979581227393,5.99664529387617));
#168927=CARTESIAN_POINT('Ctrl Pts',(40.7534558041612,14.7985550657764,5.99299194501064));
#168928=CARTESIAN_POINT('Ctrl Pts',(40.7535129011557,14.7988755637752,5.99103053615936));
#168929=CARTESIAN_POINT('Ctrl Pts',(40.7536836381393,14.7998370887716,5.98514632460547));
#168930=CARTESIAN_POINT('Ctrl Pts',(40.7537967221284,14.8004781467692,5.98122353590287));
#168931=CARTESIAN_POINT('Ctrl Pts',(40.7548078250307,14.8062480357487,5.94591862257864));
#168932=CARTESIAN_POINT('Ctrl Pts',(40.755659241947,14.8113794517343,5.91453775695695));
#168933=CARTESIAN_POINT('Ctrl Pts',(40.7572675467857,14.8216475397135,5.85177854471206));
#168934=CARTESIAN_POINT('Ctrl Pts',(40.7580244347082,14.826784210707,5.82040019808882));
#168935=CARTESIAN_POINT('Ctrl Pts',(40.7588228446244,14.8325659217041,5.78510095276256));
#168936=CARTESIAN_POINT('Ctrl Pts',(40.7589108196152,14.8332083747038,5.78117883405955));
#168937=CARTESIAN_POINT('Ctrl Pts',(40.7590852955968,14.8344933637034,5.77333463465351));
#168938=CARTESIAN_POINT('Ctrl Pts',(40.7591716215836,14.8351360876644,5.76941258518122));
#168939=CARTESIAN_POINT('Ctrl Pts',(40.7594296415835,14.8370630319307,5.75764627249435));
#168940=CARTESIAN_POINT('Ctrl Pts',(40.7596013055834,14.8383450251078,5.74980168503647));
#168941=CARTESIAN_POINT('Ctrl Pts',(40.7601152485831,14.8421830976382,5.72626678466271));
#168942=CARTESIAN_POINT('Ctrl Pts',(40.7604564785829,14.8447312699902,5.710575334747));
#168943=CARTESIAN_POINT('Ctrl Pts',(40.7635149085818,14.8675700021467,5.56933862049449));
#168944=CARTESIAN_POINT('Ctrl Pts',(40.7661435385818,14.8871969748543,5.44369774616897));
#168945=CARTESIAN_POINT('Ctrl Pts',(40.7737551075852,14.9440621737053,5.06648121210239));
#168946=CARTESIAN_POINT('Ctrl Pts',(40.7784623225903,14.9792865425664,4.81461194334237));
#168947=CARTESIAN_POINT('Ctrl Pts',(40.7871545096106,15.0443529055857,4.31006932438241));
#168948=CARTESIAN_POINT('Ctrl Pts',(40.7911465216264,15.0741883397303,4.05738582923914));
#168949=CARTESIAN_POINT('Ctrl Pts',(40.7984000276565,15.1284728542493,3.55123173804321));
#168950=CARTESIAN_POINT('Ctrl Pts',(40.8016544526714,15.1528923416321,3.29806718191379));
#168951=CARTESIAN_POINT('Ctrl Pts',(40.8074403117045,15.196290473674,2.79154410222681));
#168952=CARTESIAN_POINT('Ctrl Pts',(40.8099783237223,15.2152618303147,2.5381852268234));
#168953=CARTESIAN_POINT('Ctrl Pts',(40.8143192897512,15.2477947438337,2.03125603914715));
#168954=CARTESIAN_POINT('Ctrl Pts',(40.8161208197628,15.2613578867193,1.77768580579081));
#168955=CARTESIAN_POINT('Ctrl Pts',(40.8204554687961,15.2939070022674,1.01662841704047));
#168956=CARTESIAN_POINT('Ctrl Pts',(40.8219101918083,15.3047673577721,0.508795305361927));
#168957=CARTESIAN_POINT('Ctrl Pts',(40.8219117688083,15.3047794997738,-0.507946056309606));
#168958=CARTESIAN_POINT('Ctrl Pts',(40.8204543377961,15.2938983532662,-1.0171588060745));
#168959=CARTESIAN_POINT('Ctrl Pts',(40.8161130907627,15.2612988407111,-1.7788985638649));
#168960=CARTESIAN_POINT('Ctrl Pts',(40.8143093397511,15.2477191338232,-2.03257819622708));
#168961=CARTESIAN_POINT('Ctrl Pts',(40.8099659147222,15.2151684783018,-2.53949227890163));
#168962=CARTESIAN_POINT('Ctrl Pts',(40.8074276987045,15.1961958996608,-2.79272657929782));
#168963=CARTESIAN_POINT('Ctrl Pts',(40.8016454686713,15.1528258396229,-3.29876580195453));
#168964=CARTESIAN_POINT('Ctrl Pts',(40.7983948646565,15.1284356312442,-3.55157138606291));
#168965=CARTESIAN_POINT('Ctrl Pts',(40.7911552316264,15.0742550937395,-4.05677442320306));
#168966=CARTESIAN_POINT('Ctrl Pts',(40.7871688846105,15.0444618076008,-4.30917160432941));
#168967=CARTESIAN_POINT('Ctrl Pts',(40.7784810945902,14.9794276565858,-4.81357265728204));
#168968=CARTESIAN_POINT('Ctrl Pts',(40.7737713965852,14.9441841657221,-5.06564351805385));
#168969=CARTESIAN_POINT('Ctrl Pts',(40.7661532925818,14.8872698388643,-5.44322870314176));
#168970=CARTESIAN_POINT('Ctrl Pts',(40.7635224655818,14.8676264361545,-5.56898398847384));
#168971=CARTESIAN_POINT('Ctrl Pts',(40.7604615915829,14.8447694529955,-5.71033991073328));
#168972=CARTESIAN_POINT('Ctrl Pts',(40.7601200905831,14.8422192556431,-5.72604447364975));
#168973=CARTESIAN_POINT('Ctrl Pts',(40.7596057415834,14.8383781521124,-5.74959884602463));
#168974=CARTESIAN_POINT('Ctrl Pts',(40.7594339415835,14.8370951489351,-5.75744989148289));
#168975=CARTESIAN_POINT('Ctrl Pts',(40.7591757195836,14.8351666916686,-5.76922584117032));
#168976=CARTESIAN_POINT('Ctrl Pts',(40.7590893545964,14.8345234327034,-5.7731510916674));
#168977=CARTESIAN_POINT('Ctrl Pts',(40.7589147826148,14.8332373917038,-5.78100169707296));
#168978=CARTESIAN_POINT('Ctrl Pts',(40.758826757624,14.8325944117041,-5.78492701777574));
#168979=CARTESIAN_POINT('Ctrl Pts',(40.7580278877079,14.826807971707,-5.8202550640998));
#168980=CARTESIAN_POINT('Ctrl Pts',(40.7572705177854,14.8216671167134,-5.85165891972112));
#168981=CARTESIAN_POINT('Ctrl Pts',(40.7556610989468,14.8113907007343,-5.91446896596217));
#168982=CARTESIAN_POINT('Ctrl Pts',(40.7548090520306,14.8062551397487,-5.94587515558194));
#168983=CARTESIAN_POINT('Ctrl Pts',(40.7537971561283,14.8004806117692,-5.98120845490401));
#168984=CARTESIAN_POINT('Ctrl Pts',(40.7536839831392,14.7998390387716,-5.98513439560637));
#168985=CARTESIAN_POINT('Ctrl Pts',(40.7535131111557,14.7988767407752,-5.9910233351599));
#168986=CARTESIAN_POINT('Ctrl Pts',(40.7534559681611,14.7985559857764,-5.99298631901107));
#168987=CARTESIAN_POINT('Ctrl Pts',(40.7533491890241,14.7979585651291,-5.99664258254315));
#168988=CARTESIAN_POINT('Ctrl Pts',(40.7532925113861,14.7976755455897,-5.99840827840234));
#168989=CARTESIAN_POINT('Ctrl Pts',(40.7532527155551,14.7974077965398,-5.99999999355178));
#168990=CARTESIAN_POINT('',(41.7359306993252,13.7060333274604,6.));
#168991=CARTESIAN_POINT('',(40.7532527143533,14.7974077953405,-6.));
#168992=CARTESIAN_POINT('Ctrl Pts',(9.758033795,14.612348562,6.));
#168993=CARTESIAN_POINT('Ctrl Pts',(10.542955148,14.611742111,6.));
#168994=CARTESIAN_POINT('Ctrl Pts',(11.32816556,14.591601296,6.));
#168995=CARTESIAN_POINT('Ctrl Pts',(12.113445943,14.550446495,6.));
#168996=CARTESIAN_POINT('Ctrl Pts',(9.763948215,14.780478266,5.009967665));
#168997=CARTESIAN_POINT('Ctrl Pts',(10.549810959,14.785748194,5.010318328));
#168998=CARTESIAN_POINT('Ctrl Pts',(11.33613133,14.768826884,5.01051229));
#168999=CARTESIAN_POINT('Ctrl Pts',(12.122730321,14.727602978,5.01051229));
#169000=CARTESIAN_POINT('Ctrl Pts',(9.771419064,15.033582243,3.014974832));
#169001=CARTESIAN_POINT('Ctrl Pts',(10.559011277,15.047679518,3.015501647));
#169002=CARTESIAN_POINT('Ctrl Pts',(11.347466763,15.035579093,3.015793043));
#169003=CARTESIAN_POINT('Ctrl Pts',(12.136702969,14.994216976,3.015793043));
#169004=CARTESIAN_POINT('Ctrl Pts',(9.774986833,15.160468498,0.));
#169005=CARTESIAN_POINT('Ctrl Pts',(10.563484757,15.178988749,0.));
#169006=CARTESIAN_POINT('Ctrl Pts',(11.353068133,15.169301939,0.));
#169007=CARTESIAN_POINT('Ctrl Pts',(12.143707233,15.127866299,0.));
#169008=CARTESIAN_POINT('Ctrl Pts',(9.771419064,15.033582243,-3.014974832));
#169009=CARTESIAN_POINT('Ctrl Pts',(10.559011277,15.047679518,-3.015501647));
#169010=CARTESIAN_POINT('Ctrl Pts',(11.347466763,15.035579093,-3.015793043));
#169011=CARTESIAN_POINT('Ctrl Pts',(12.136702969,14.994216976,-3.015793043));
#169012=CARTESIAN_POINT('Ctrl Pts',(9.763948215,14.780478266,-5.009967665));
#169013=CARTESIAN_POINT('Ctrl Pts',(10.549810959,14.785748194,-5.010318328));
#169014=CARTESIAN_POINT('Ctrl Pts',(11.33613133,14.768826884,-5.01051229));
#169015=CARTESIAN_POINT('Ctrl Pts',(12.122730321,14.727602978,-5.01051229));
#169016=CARTESIAN_POINT('Ctrl Pts',(9.758033795,14.612348562,-6.));
#169017=CARTESIAN_POINT('Ctrl Pts',(10.542955148,14.611742111,-6.));
#169018=CARTESIAN_POINT('Ctrl Pts',(11.32816556,14.591601296,-6.));
#169019=CARTESIAN_POINT('Ctrl Pts',(12.113445943,14.550446495,-6.));
#169020=CARTESIAN_POINT('Ctrl Pts',(9.7577972182,14.60562337384,-6.0396012934));
#169021=CARTESIAN_POINT('Ctrl Pts',(10.54268091556,14.60478186768,-6.03958726688));
#169022=CARTESIAN_POINT('Ctrl Pts',(11.3278469292,14.58451227248,-6.0395795084));
#169023=CARTESIAN_POINT('Ctrl Pts',(12.11307456788,14.54336023568,-6.0395795084));
#169024=CARTESIAN_POINT('Ctrl Pts',(9.7575606414,14.59889818568,-6.0792025868));
#169025=CARTESIAN_POINT('Ctrl Pts',(10.54240668312,14.59782162436,-6.07917453376));
#169026=CARTESIAN_POINT('Ctrl Pts',(11.3275282984,14.57742324896,-6.0791590168));
#169027=CARTESIAN_POINT('Ctrl Pts',(12.11270319276,14.53627397636,-6.0791590168));
#169028=CARTESIAN_POINT('Ctrl Pts',(9.7573240646,14.59217299752,-6.1188038802));
#169029=CARTESIAN_POINT('Ctrl Pts',(10.54213245068,14.59086138104,-6.11876180064));
#169030=CARTESIAN_POINT('Ctrl Pts',(11.3272096676,14.57033422544,-6.1187385252));
#169031=CARTESIAN_POINT('Ctrl Pts',(12.11233181764,14.52918771704,-6.1187385252));
#169032=CARTESIAN_POINT('',(9.79794790085819,14.6123008732764,-5.99999994854148));
#169033=CARTESIAN_POINT('',(12.1134459448026,14.5504464930284,-6.00000000166256));
#169034=CARTESIAN_POINT('Ctrl Pts',(9.79794877240227,14.6123008871254,-6.));
#169035=CARTESIAN_POINT('Ctrl Pts',(10.5695747870962,14.6110532742617,-6.));
#169036=CARTESIAN_POINT('Ctrl Pts',(11.3414765555483,14.5909036962831,-6.));
#169037=CARTESIAN_POINT('Ctrl Pts',(12.1134459457272,14.550446492489,-6.));
#169038=CARTESIAN_POINT('',(12.1134459448786,14.5504464944803,5.99999999961158));
#169039=CARTESIAN_POINT('Ctrl Pts',(12.1134459430031,14.5504464950543,5.99999999969675));
#169040=CARTESIAN_POINT('Ctrl Pts',(12.1320240607837,14.9049380944675,4.02002684265496));
#169041=CARTESIAN_POINT('Ctrl Pts',(12.141372478348,15.0833165249396,2.01154104533017));
#169042=CARTESIAN_POINT('Ctrl Pts',(12.1413724783187,15.0833165243943,-2.00789360499469));
#169043=CARTESIAN_POINT('Ctrl Pts',(12.1319903606165,14.9042950569859,-4.02361845730749));
#169044=CARTESIAN_POINT('Ctrl Pts',(12.1134459429818,14.5504464946533,-6.0000000019364));
#169045=CARTESIAN_POINT('',(9.79794823008933,14.612300878333,5.99999997397329));
#169046=CARTESIAN_POINT('Ctrl Pts',(12.1134459458125,14.5504464941161,6.));
#169047=CARTESIAN_POINT('Ctrl Pts',(11.3414766025522,14.5909036938197,6.));
#169048=CARTESIAN_POINT('Ctrl Pts',(10.5695748810957,14.611053271808,6.));
#169049=CARTESIAN_POINT('Ctrl Pts',(9.79794891334272,14.6123008817038,6.));
#169050=CARTESIAN_POINT('Ctrl Pts',(9.79794788859268,14.6123008832888,5.99999992191988));
#169051=CARTESIAN_POINT('Ctrl Pts',(9.7979500800566,14.6125894414009,5.99830368000664));
#169052=CARTESIAN_POINT('Ctrl Pts',(9.79794640227073,14.6129084799895,5.99642789963154));
#169053=CARTESIAN_POINT('Ctrl Pts',(9.79794507046349,14.6132150280573,5.9946244480845));
#169054=CARTESIAN_POINT('Ctrl Pts',(9.79794343836482,14.6135906955563,5.99241436032496));
#169055=CARTESIAN_POINT('Ctrl Pts',(9.797941820851,14.6139659648138,5.99020535120621));
#169056=CARTESIAN_POINT('Ctrl Pts',(9.79794021861651,14.6143408380001,5.98799741265409));
#169057=CARTESIAN_POINT('Ctrl Pts',(9.7978525587376,14.6348505313159,5.86719884872445));
#169058=CARTESIAN_POINT('Ctrl Pts',(9.79781066749895,14.654180848725,5.74959401446796));
#169059=CARTESIAN_POINT('Ctrl Pts',(9.79779333553231,14.6726038633972,5.63405188307487));
#169060=CARTESIAN_POINT('Ctrl Pts',(9.79777555264829,14.691506180708,5.51550374808145));
#169061=CARTESIAN_POINT('Ctrl Pts',(9.79778348353759,14.709453307596,5.39912677717061));
#169062=CARTESIAN_POINT('Ctrl Pts',(9.7977873569103,14.7266861962401,5.28368727150186));
#169063=CARTESIAN_POINT('Ctrl Pts',(9.7977889900763,14.7339522586037,5.23501344410497));
#169064=CARTESIAN_POINT('Ctrl Pts',(9.79778983197078,14.7410907159002,5.1865061574113));
#169065=CARTESIAN_POINT('Ctrl Pts',(9.79778738507617,14.7481169257174,5.13807247881662));
#169066=CARTESIAN_POINT('Ctrl Pts',(9.79778153561427,14.7649135406528,5.0222885966929));
#169067=CARTESIAN_POINT('Ctrl Pts',(9.79775791998702,14.7810703528341,4.90694343321932));
#169068=CARTESIAN_POINT('Ctrl Pts',(9.79767818984793,14.7967638304198,4.79074603437952));
#169069=CARTESIAN_POINT('Ctrl Pts',(9.79761438680368,14.8093223391131,4.69776052269151));
#169070=CARTESIAN_POINT('Ctrl Pts',(9.7975145594496,14.8215831841756,4.60422918585069));
#169071=CARTESIAN_POINT('Ctrl Pts',(9.79735797733189,14.8336128666801,4.50948853860347));
#169072=CARTESIAN_POINT('Ctrl Pts',(9.79676530749574,14.879145715919,4.15089124342981));
#169073=CARTESIAN_POINT('Ctrl Pts',(9.7959450021984,14.9192348565256,3.79157351780402));
#169074=CARTESIAN_POINT('Ctrl Pts',(9.7950926075,14.953868669,3.431707731));
#169075=CARTESIAN_POINT('Ctrl Pts',(9.79479733986455,14.9658657449263,3.30705101956353));
#169076=CARTESIAN_POINT('Ctrl Pts',(9.79449812915568,14.9772078235421,3.18232915770469));
#169077=CARTESIAN_POINT('Ctrl Pts',(9.79420022074329,14.9878944220546,3.0575485461174));
#169078=CARTESIAN_POINT('Ctrl Pts',(9.79416286827072,14.9892343334541,3.04190325321103));
#169079=CARTESIAN_POINT('Ctrl Pts',(9.79412148215503,14.9907073476449,3.02455621728992));
#169080=CARTESIAN_POINT('Ctrl Pts',(9.79407243535764,14.9918830187537,3.01060967259255));
#169081=CARTESIAN_POINT('Ctrl Pts',(9.79309389504961,15.0153390164952,2.73235998313183));
#169082=CARTESIAN_POINT('Ctrl Pts',(9.79230021516519,15.0364330462044,2.44325467676033));
#169083=CARTESIAN_POINT('Ctrl Pts',(9.79166768385037,15.0543911195385,2.14337439862685));
#169084=CARTESIAN_POINT('Ctrl Pts',(9.79137351457374,15.0627428221633,2.00391005524037));
#169085=CARTESIAN_POINT('Ctrl Pts',(9.79111458808493,15.0704156336338,1.86211527147687));
#169086=CARTESIAN_POINT('Ctrl Pts',(9.79089069072951,15.0773285435866,1.71799844027648));
#169087=CARTESIAN_POINT('Ctrl Pts',(9.79082384392684,15.0793924622362,1.67497091385613));
#169088=CARTESIAN_POINT('Ctrl Pts',(9.79076001954289,15.0813886874519,1.63173316511455));
#169089=CARTESIAN_POINT('Ctrl Pts',(9.79069913107378,15.0833149579498,1.58828679378095));
#169090=CARTESIAN_POINT('Ctrl Pts',(9.79040718463865,15.0925509892244,1.3799712717242));
#169091=CARTESIAN_POINT('Ctrl Pts',(9.79018370715181,15.1001791149284,1.166892959045));
#169092=CARTESIAN_POINT('Ctrl Pts',(9.7900219600675,15.1059476883998,0.949060540766124));
#169093=CARTESIAN_POINT('Ctrl Pts',(9.78999962212445,15.1067443523165,0.918976980526512));
#169094=CARTESIAN_POINT('Ctrl Pts',(9.78997846820551,15.1075055117168,0.88880281833857));
#169095=CARTESIAN_POINT('Ctrl Pts',(9.78995848711913,15.1082304671688,0.858538147994024));
#169096=CARTESIAN_POINT('Ctrl Pts',(9.78994886882902,15.1085794387775,0.843969651862457));
#169097=CARTESIAN_POINT('Ctrl Pts',(9.78993952235631,15.1089200241747,0.829380448721482));
#169098=CARTESIAN_POINT('Ctrl Pts',(9.78993044359277,15.1092521483247,0.814770493349579));
#169099=CARTESIAN_POINT('Ctrl Pts',(9.78984819129214,15.1122611456734,0.682406384993954));
#169100=CARTESIAN_POINT('Ctrl Pts',(9.78978793063445,15.1145760536446,0.54832419543522));
#169101=CARTESIAN_POINT('Ctrl Pts',(9.78974823694479,15.116138994976,0.412531798708623));
#169102=CARTESIAN_POINT('Ctrl Pts',(9.78972839009996,15.1169204656416,0.344635600345324));
#169103=CARTESIAN_POINT('Ctrl Pts',(9.78971368534993,15.1175139282023,0.276311850322579));
#169104=CARTESIAN_POINT('Ctrl Pts',(9.7897039406203,15.1179120533349,0.207561686381522));
#169105=CARTESIAN_POINT('Ctrl Pts',(9.78969906825549,15.1181111159013,0.173186604410992));
#169106=CARTESIAN_POINT('Ctrl Pts',(9.78969543591472,15.1182613431959,0.138704918937019));
#169107=CARTESIAN_POINT('Ctrl Pts',(9.78969302078614,15.1183618136691,0.104116776811358));
#169108=CARTESIAN_POINT('Ctrl Pts',(9.78969181322185,15.1184120489057,0.086822705748525));
#169109=CARTESIAN_POINT('Ctrl Pts',(9.78969090996175,15.1184498448821,0.0695020205216681));
#169110=CARTESIAN_POINT('Ctrl Pts',(9.78969030814099,15.1184750860797,0.0521547400165017));
#169111=CARTESIAN_POINT('Ctrl Pts',(9.7896900072306,15.1184877066784,0.0434810997639184));
#169112=CARTESIAN_POINT('Ctrl Pts',(9.78968978168012,15.1184971885791,0.0348008106916684));
#169113=CARTESIAN_POINT('Ctrl Pts',(9.78968963113053,15.1185035173221,0.0261138751957106));
#169114=CARTESIAN_POINT('Ctrl Pts',(9.78968948058094,15.1185098460651,0.0174269396997527));
#169115=CARTESIAN_POINT('Ctrl Pts',(9.78968940485914,15.1185130231695,0.00707187686119539));
#169116=CARTESIAN_POINT('Ctrl Pts',(9.78968940412529,15.1185130296052,3.31318431472039E-5));
#169117=CARTESIAN_POINT('Ctrl Pts',(9.78968940408767,15.118513029935,-0.000327672777262212));
#169118=CARTESIAN_POINT('Ctrl Pts',(9.78968940427655,15.1185130248193,-0.000688494058382274));
#169119=CARTESIAN_POINT('Ctrl Pts',(9.78968940469201,15.1185130142563,-0.00104933199997106));
#169120=CARTESIAN_POINT('Ctrl Pts',(9.78968974774507,15.1185042923071,-0.2989969357337));
#169121=CARTESIAN_POINT('Ctrl Pts',(9.78985105637987,15.1147891306134,-0.608259091370153));
#169122=CARTESIAN_POINT('Ctrl Pts',(9.79018146417964,15.1064875059098,-0.928699572294281));
#169123=CARTESIAN_POINT('Ctrl Pts',(9.7903502600005,15.1022464451443,-1.0924033772587));
#169124=CARTESIAN_POINT('Ctrl Pts',(9.7905630345956,15.0968075421677,-1.25902473626515));
#169125=CARTESIAN_POINT('Ctrl Pts',(9.79081980750076,15.0900484174663,-1.42854638429469));
#169126=CARTESIAN_POINT('Ctrl Pts',(9.79096469902433,15.0862343862492,-1.5242038674947));
#169127=CARTESIAN_POINT('Ctrl Pts',(9.79112358631072,15.0819999450171,-1.62078414142528));
#169128=CARTESIAN_POINT('Ctrl Pts',(9.79129635633333,15.077322754,-1.71828248833332));
#169129=CARTESIAN_POINT('Ctrl Pts',(9.79166409101511,15.0673675237795,-1.92580415807717));
#169130=CARTESIAN_POINT('Ctrl Pts',(9.79209231393233,15.0554054190377,-2.13748477179792));
#169131=CARTESIAN_POINT('Ctrl Pts',(9.79256487626909,15.0412094777158,-2.35327968127705));
#169132=CARTESIAN_POINT('Ctrl Pts',(9.79272641854607,15.0363566900376,-2.42704772905783));
#169133=CARTESIAN_POINT('Ctrl Pts',(9.79289309842739,15.031242840242,-2.50129592942567));
#169134=CARTESIAN_POINT('Ctrl Pts',(9.7930641305,15.0258588495,-2.57602044850002));
#169135=CARTESIAN_POINT('Ctrl Pts',(9.79327367392242,15.019262543736,-2.66757071288625));
#169136=CARTESIAN_POINT('Ctrl Pts',(9.79348974652061,15.0122597715775,-2.75984220914934));
#169137=CARTESIAN_POINT('Ctrl Pts',(9.793710077335,15.0048341883609,-2.8528254936469));
#169138=CARTESIAN_POINT('Ctrl Pts',(9.79375208732067,15.0034183689469,-2.87055440941397));
#169139=CARTESIAN_POINT('Ctrl Pts',(9.79379425160075,15.0019871723335,-2.88830926034111));
#169140=CARTESIAN_POINT('Ctrl Pts',(9.79383655358928,15.0005404799128,-2.90609001439213));
#169141=CARTESIAN_POINT('Ctrl Pts',(9.79387734925027,14.9991453026262,-2.92323761524699));
#169142=CARTESIAN_POINT('Ctrl Pts',(9.79391827298526,14.9977357134172,-2.94040930776202));
#169143=CARTESIAN_POINT('Ctrl Pts',(9.79395926806275,14.9963116044282,-2.95760506283209));
#169144=CARTESIAN_POINT('Ctrl Pts',(9.79400026314025,14.9948874954392,-2.97480081790216));
#169145=CARTESIAN_POINT('Ctrl Pts',(9.79404510637553,14.9933149759388,-2.99360933560658));
#169146=CARTESIAN_POINT('Ctrl Pts',(9.79408255626668,14.9919956115203,-3.00926448860491));
#169147=CARTESIAN_POINT('Ctrl Pts',(9.79442367992096,14.9799777818834,-3.15186418208799));
#169148=CARTESIAN_POINT('Ctrl Pts',(9.7946910709083,14.9672240920578,-3.29298618374894));
#169149=CARTESIAN_POINT('Ctrl Pts',(9.79490867824321,14.9537238032509,-3.43318591187827));
#169150=CARTESIAN_POINT('Ctrl Pts',(9.79516006594659,14.9381277912901,-3.59514960525305));
#169151=CARTESIAN_POINT('Ctrl Pts',(9.79534662111358,14.9215405704387,-3.75586458296582));
#169152=CARTESIAN_POINT('Ctrl Pts',(9.79550146245736,14.9038907416998,-3.91628227532854));
#169153=CARTESIAN_POINT('Ctrl Pts',(9.79565616962082,14.8862562077119,-4.07656095508648));
#169154=CARTESIAN_POINT('Ctrl Pts',(9.79577935812821,14.867560891691,-4.23654284284504));
#169155=CARTESIAN_POINT('Ctrl Pts',(9.79590288664792,14.8476821414815,-4.39716987604912));
#169156=CARTESIAN_POINT('Ctrl Pts',(9.79602515559278,14.8280060875706,-4.55615905452083));
#169157=CARTESIAN_POINT('Ctrl Pts',(9.79614789577125,14.8071706176418,-4.71578026901489));
#169158=CARTESIAN_POINT('Ctrl Pts',(9.79629879439229,14.7850065463336,-4.87694037663787));
#169159=CARTESIAN_POINT('Ctrl Pts',(9.79638035986249,14.7730261658288,-4.96405250439962));
#169160=CARTESIAN_POINT('Ctrl Pts',(9.79647008533354,14.7606567345884,-5.05161414583504));
#169161=CARTESIAN_POINT('Ctrl Pts',(9.79657172109791,14.7478652436572,-5.13976773370651));
#169162=CARTESIAN_POINT('Ctrl Pts',(9.79675360190473,14.7249744167373,-5.29752170728039));
#169163=CARTESIAN_POINT('Ctrl Pts',(9.79697275033504,14.7007341922703,-5.45717140418589));
#169164=CARTESIAN_POINT('Ctrl Pts',(9.79724085837546,14.6749163120254,-5.61952745024738));
#169165=CARTESIAN_POINT('Ctrl Pts',(9.79744138183986,14.6556065935176,-5.74095684405289));
#169166=CARTESIAN_POINT('Ctrl Pts',(9.79766917912186,14.6354134211619,-5.86390001075217));
#169167=CARTESIAN_POINT('Ctrl Pts',(9.79792567385572,14.6142226062327,-5.98869386966598));
#169168=CARTESIAN_POINT('Ctrl Pts',(9.79793345018516,14.6135801495424,-5.99247733197415));
#169169=CARTESIAN_POINT('Ctrl Pts',(9.79794791329567,14.6129018735453,-5.99646672715746));
#169170=CARTESIAN_POINT('Ctrl Pts',(9.7979474653736,14.6123008794813,-5.99999984562444));
#169171=CARTESIAN_POINT('Ctrl Pts',(12.1123317552017,14.5291866595917,6.11874443277285));
#169172=CARTESIAN_POINT('Ctrl Pts',(20.8902575146672,14.2345980190016,6.11876772761178));
#169173=CARTESIAN_POINT('Ctrl Pts',(29.5936684411877,13.65102255426,6.11879102245071));
#169174=CARTESIAN_POINT('Ctrl Pts',(38.3179610775993,12.7701867243602,6.11881431716964));
#169175=CARTESIAN_POINT('Ctrl Pts',(38.3699704723074,12.7649356698709,6.11881445601655));
#169176=CARTESIAN_POINT('Ctrl Pts',(38.4219798682553,12.7596846155016,6.11881459486345));
#169177=CARTESIAN_POINT('Ctrl Pts',(38.4739892629633,12.7544335598922,6.11881473383037));
#169178=CARTESIAN_POINT('Ctrl Pts',(12.1127031487985,14.5362732714729,6.0791629551819));
#169179=CARTESIAN_POINT('Ctrl Pts',(20.8907773155674,14.2416052037713,6.07917848507452));
#169180=CARTESIAN_POINT('Ctrl Pts',(29.5943366493513,13.6579503119182,6.07919401496715));
#169181=CARTESIAN_POINT('Ctrl Pts',(38.3187776930662,12.7770350549068,6.07920954477976));
#169182=CARTESIAN_POINT('Ctrl Pts',(38.3707879725382,12.7717835269139,6.07920963734436));
#169183=CARTESIAN_POINT('Ctrl Pts',(38.4227982531702,12.766531999001,6.07920972990897));
#169184=CARTESIAN_POINT('Ctrl Pts',(38.4748085326422,12.7612804699281,6.07920982255358));
#169185=CARTESIAN_POINT('Ctrl Pts',(12.1130745423953,14.5433598833541,6.03958147759095));
#169186=CARTESIAN_POINT('Ctrl Pts',(20.8912971164676,14.248612388541,6.03958924253726));
#169187=CARTESIAN_POINT('Ctrl Pts',(29.5950048575148,13.6648780695763,6.03959700748357));
#169188=CARTESIAN_POINT('Ctrl Pts',(38.3195943085331,12.7838833854534,6.03960477238988));
#169189=CARTESIAN_POINT('Ctrl Pts',(38.3716054727691,12.778631383957,6.03960481867218));
#169190=CARTESIAN_POINT('Ctrl Pts',(38.4236166380851,12.7733793825005,6.03960486495448));
#169191=CARTESIAN_POINT('Ctrl Pts',(38.4756278023211,12.7681273799641,6.03960491127679));
#169192=CARTESIAN_POINT('Ctrl Pts',(12.1134459359922,14.5504464952354,6.));
#169193=CARTESIAN_POINT('Ctrl Pts',(20.8918169173678,14.2556195733107,6.));
#169194=CARTESIAN_POINT('Ctrl Pts',(29.5956730656783,13.6718058272345,6.));
#169195=CARTESIAN_POINT('Ctrl Pts',(38.320410924,12.790731716,6.));
#169196=CARTESIAN_POINT('Ctrl Pts',(38.372422973,12.785479241,6.));
#169197=CARTESIAN_POINT('Ctrl Pts',(38.424435023,12.780226766,6.));
#169198=CARTESIAN_POINT('Ctrl Pts',(38.476447072,12.77497429,6.));
#169199=CARTESIAN_POINT('Ctrl Pts',(12.1227303139892,14.7276029782369,5.01051229000016));
#169200=CARTESIAN_POINT('Ctrl Pts',(20.9048112933658,14.4307904773118,5.0103181760001));
#169201=CARTESIAN_POINT('Ctrl Pts',(29.6123774386773,13.844991152235,5.01012406200005));
#169202=CARTESIAN_POINT('Ctrl Pts',(38.340825295,12.961931462,5.009929949));
#169203=CARTESIAN_POINT('Ctrl Pts',(38.392859462,12.95666715,5.009928792));
#169204=CARTESIAN_POINT('Ctrl Pts',(38.444893628,12.951402837,5.009927635));
#169205=CARTESIAN_POINT('Ctrl Pts',(38.496927795,12.946138525,5.009926477));
#169206=CARTESIAN_POINT('Ctrl Pts',(12.1367029619847,14.9942169762393,3.01579304300023));
#169207=CARTESIAN_POINT('Ctrl Pts',(20.9243654493628,14.6944005693134,3.01550099000015));
#169208=CARTESIAN_POINT('Ctrl Pts',(29.6375131046759,14.1055973392358,3.01520893700008));
#169209=CARTESIAN_POINT('Ctrl Pts',(38.37154247,13.219533743,3.014916884));
#169210=CARTESIAN_POINT('Ctrl Pts',(38.42360991,13.214251523,3.014915143));
#169211=CARTESIAN_POINT('Ctrl Pts',(38.47567735,13.208969303,3.014913402));
#169212=CARTESIAN_POINT('Ctrl Pts',(38.527744791,13.203687083,3.014911661));
#169213=CARTESIAN_POINT('Ctrl Pts',(12.1437072259825,15.1278662992405,0.));
#169214=CARTESIAN_POINT('Ctrl Pts',(20.9341668943613,14.8265379783142,0.));
#169215=CARTESIAN_POINT('Ctrl Pts',(29.6501117306751,14.2362228332362,0.));
#169216=CARTESIAN_POINT('Ctrl Pts',(38.386938276,13.348647322,0.));
#169217=CARTESIAN_POINT('Ctrl Pts',(38.439022392,13.343356089,0.));
#169218=CARTESIAN_POINT('Ctrl Pts',(38.491106507,13.338064856,0.));
#169219=CARTESIAN_POINT('Ctrl Pts',(38.543190623,13.332773623,0.));
#169220=CARTESIAN_POINT('Ctrl Pts',(12.1367029619847,14.9942169762393,-3.01579304300023));
#169221=CARTESIAN_POINT('Ctrl Pts',(20.9243654493628,14.6944005693134,-3.01550099000015));
#169222=CARTESIAN_POINT('Ctrl Pts',(29.6375131046759,14.1055973392358,-3.01520893700008));
#169223=CARTESIAN_POINT('Ctrl Pts',(38.37154247,13.219533743,-3.014916884));
#169224=CARTESIAN_POINT('Ctrl Pts',(38.42360991,13.214251523,-3.014915143));
#169225=CARTESIAN_POINT('Ctrl Pts',(38.47567735,13.208969303,-3.014913402));
#169226=CARTESIAN_POINT('Ctrl Pts',(38.527744791,13.203687083,-3.014911661));
#169227=CARTESIAN_POINT('Ctrl Pts',(12.1227303139892,14.7276029782369,-5.01051229000016));
#169228=CARTESIAN_POINT('Ctrl Pts',(20.9048112933658,14.4307904773118,-5.0103181760001));
#169229=CARTESIAN_POINT('Ctrl Pts',(29.6123774386773,13.844991152235,-5.01012406200005));
#169230=CARTESIAN_POINT('Ctrl Pts',(38.340825295,12.961931462,-5.009929949));
#169231=CARTESIAN_POINT('Ctrl Pts',(38.392859462,12.95666715,-5.009928792));
#169232=CARTESIAN_POINT('Ctrl Pts',(38.444893628,12.951402837,-5.009927635));
#169233=CARTESIAN_POINT('Ctrl Pts',(38.496927795,12.946138525,-5.009926477));
#169234=CARTESIAN_POINT('Ctrl Pts',(12.1134459359922,14.5504464952354,-6.));
#169235=CARTESIAN_POINT('Ctrl Pts',(20.8918169173678,14.2556195733107,-6.));
#169236=CARTESIAN_POINT('Ctrl Pts',(29.5956730656783,13.6718058272345,-6.));
#169237=CARTESIAN_POINT('Ctrl Pts',(38.320410924,12.790731716,-6.));
#169238=CARTESIAN_POINT('Ctrl Pts',(38.372422973,12.785479241,-6.));
#169239=CARTESIAN_POINT('Ctrl Pts',(38.424435023,12.780226766,-6.));
#169240=CARTESIAN_POINT('Ctrl Pts',(38.476447072,12.77497429,-6.));
#169241=CARTESIAN_POINT('Ctrl Pts',(12.1134440882973,14.5504112391184,-6.00019691909556));
#169242=CARTESIAN_POINT('Ctrl Pts',(20.891814331342,14.2555847123461,-6.00019695772641));
#169243=CARTESIAN_POINT('Ctrl Pts',(29.5956697413217,13.6717713614223,-6.00019699635726));
#169244=CARTESIAN_POINT('Ctrl Pts',(38.3204068613124,12.7906976453402,-6.00019703498792));
#169245=CARTESIAN_POINT('Ctrl Pts',(38.3724189059106,12.7854451726959,-6.00019703521817));
#169246=CARTESIAN_POINT('Ctrl Pts',(38.4244309515093,12.7801927000518,-6.00019703544843));
#169247=CARTESIAN_POINT('Ctrl Pts',(38.4764429961076,12.7749402264073,-6.00019703567888));
#169248=CARTESIAN_POINT('Ctrl Pts',(12.1134422406025,14.5503759830015,-6.00039383819112));
#169249=CARTESIAN_POINT('Ctrl Pts',(20.8918117453161,14.2555498513816,-6.00039391545282));
#169250=CARTESIAN_POINT('Ctrl Pts',(29.5956664169651,13.6717368956101,-6.00039399271453));
#169251=CARTESIAN_POINT('Ctrl Pts',(38.3204027986247,12.7906635746804,-6.00039406997583));
#169252=CARTESIAN_POINT('Ctrl Pts',(38.3724148388213,12.7854111043918,-6.00039407043634));
#169253=CARTESIAN_POINT('Ctrl Pts',(38.4244268800187,12.7801586341036,-6.00039407089686));
#169254=CARTESIAN_POINT('Ctrl Pts',(38.4764389202152,12.7749061628146,-6.00039407135776));
#169255=CARTESIAN_POINT('Ctrl Pts',(12.1134403929077,14.5503407268846,-6.00059075728668));
#169256=CARTESIAN_POINT('Ctrl Pts',(20.8918091592903,14.255514990417,-6.00059087317923));
#169257=CARTESIAN_POINT('Ctrl Pts',(29.5956630926085,13.6717024297979,-6.00059098907179));
#169258=CARTESIAN_POINT('Ctrl Pts',(38.3203987359371,12.7906295040206,-6.00059110496375));
#169259=CARTESIAN_POINT('Ctrl Pts',(38.3724107717319,12.7853770360877,-6.00059110565452));
#169260=CARTESIAN_POINT('Ctrl Pts',(38.4244228085279,12.7801245681554,-6.00059110634528));
#169261=CARTESIAN_POINT('Ctrl Pts',(38.4764348443227,12.7748720992219,-6.00059110703665));
#169262=CARTESIAN_POINT('Ctrl Pts',(12.1134459458125,14.5504464941161,6.));
#169263=CARTESIAN_POINT('Ctrl Pts',(20.8914804963054,14.2556308720613,6.));
#169264=CARTESIAN_POINT('Ctrl Pts',(29.5950059279722,13.6718505751845,6.));
#169265=CARTESIAN_POINT('Ctrl Pts',(38.3194078205169,12.7908330852606,6.));
#169266=CARTESIAN_POINT('Ctrl Pts',(12.1134459457272,14.550446492489,-6.));
#169267=CARTESIAN_POINT('Ctrl Pts',(20.8914804963505,14.2556308720598,-6.));
#169268=CARTESIAN_POINT('Ctrl Pts',(29.5950059280615,13.6718505751785,-6.));
#169269=CARTESIAN_POINT('Ctrl Pts',(38.3194078202364,12.7908330811398,-6.));
#169270=CARTESIAN_POINT('Ctrl Pts',(40.751918853,14.786422254,6.063606532));
#169271=CARTESIAN_POINT('Ctrl Pts',(39.491202843,16.145755581,6.271940406));
#169272=CARTESIAN_POINT('Ctrl Pts',(37.638148242,16.362045517,6.270436567));
#169273=CARTESIAN_POINT('Ctrl Pts',(40.752211793,14.788834877,6.049637389));
#169274=CARTESIAN_POINT('Ctrl Pts',(39.491495482,16.148168529,6.257971313));
#169275=CARTESIAN_POINT('Ctrl Pts',(37.638440405,16.364458231,6.256467424));
#169276=CARTESIAN_POINT('Ctrl Pts',(40.752504733,14.791247501,6.035668246));
#169277=CARTESIAN_POINT('Ctrl Pts',(39.491788121,16.150581477,6.244002221));
#169278=CARTESIAN_POINT('Ctrl Pts',(37.638732567,16.366870945,6.242498282));
#169279=CARTESIAN_POINT('Ctrl Pts',(40.752944143,14.794866436,6.014714532));
#169280=CARTESIAN_POINT('Ctrl Pts',(39.492227079,16.154200899,6.223048583));
#169281=CARTESIAN_POINT('Ctrl Pts',(37.639170812,16.370490016,6.221544569));
#169282=CARTESIAN_POINT('Ctrl Pts',(40.7530804,14.796063549,6.007834764));
#169283=CARTESIAN_POINT('Ctrl Pts',(39.492365431,16.15539798,6.216122968));
#169284=CARTESIAN_POINT('Ctrl Pts',(37.639316897,16.371696373,6.214559998));
#169285=CARTESIAN_POINT('Ctrl Pts',(40.753276253,14.797582938,5.998973045));
#169286=CARTESIAN_POINT('Ctrl Pts',(39.492558289,16.156917814,6.20731862));
#169287=CARTESIAN_POINT('Ctrl Pts',(37.639499494,16.37320432,6.205829284));
#169288=CARTESIAN_POINT('Ctrl Pts',(40.753343234,14.797911941,5.996914444));
#169289=CARTESIAN_POINT('Ctrl Pts',(39.492618548,16.157247449,6.205396776));
#169290=CARTESIAN_POINT('Ctrl Pts',(37.639535929,16.373505919,6.204083141));
#169291=CARTESIAN_POINT('Ctrl Pts',(40.753457798,14.798552916,5.992991615));
#169292=CARTESIAN_POINT('Ctrl Pts',(39.492723845,16.157889349,6.201662396));
#169293=CARTESIAN_POINT('Ctrl Pts',(37.639608365,16.374109168,6.200590857));
#169294=CARTESIAN_POINT('Ctrl Pts',(40.753514895,14.798873414,5.991030206));
#169295=CARTESIAN_POINT('Ctrl Pts',(39.492776315,16.158210319,6.19979521));
#169296=CARTESIAN_POINT('Ctrl Pts',(37.639644408,16.374410813,6.198844716));
#169297=CARTESIAN_POINT('Ctrl Pts',(40.753685632,14.799834939,5.985145994));
#169298=CARTESIAN_POINT('Ctrl Pts',(39.492933191,16.159173296,6.194193656));
#169299=CARTESIAN_POINT('Ctrl Pts',(37.639752006,16.375315808,6.193606291));
#169300=CARTESIAN_POINT('Ctrl Pts',(40.753798716,14.800475997,5.981223205));
#169301=CARTESIAN_POINT('Ctrl Pts',(39.493037062,16.159815364,6.190459303));
#169302=CARTESIAN_POINT('Ctrl Pts',(37.639823034,16.375919221,6.19011401));
#169303=CARTESIAN_POINT('Ctrl Pts',(40.754809819,14.806245886,5.945918289));
#169304=CARTESIAN_POINT('Ctrl Pts',(39.493965505,16.165594803,6.15684982700001));
#169305=CARTESIAN_POINT('Ctrl Pts',(37.640455947,16.381350669,6.158683494));
#169306=CARTESIAN_POINT('Ctrl Pts',(40.755661236,14.811377302,5.914537421));
#169307=CARTESIAN_POINT('Ctrl Pts',(39.494745181,16.17073739,6.12697600200001));
#169308=CARTESIAN_POINT('Ctrl Pts',(37.640973468,16.386183859,6.130745355));
#169309=CARTESIAN_POINT('Ctrl Pts',(40.757269541,14.82164539,5.851778204));
#169310=CARTESIAN_POINT('Ctrl Pts',(39.496213487,16.181033294,6.067230117));
#169311=CARTESIAN_POINT('Ctrl Pts',(37.641918511,16.395860698,6.074869273));
#169312=CARTESIAN_POINT('Ctrl Pts',(40.758026429,14.826782061,5.820399855));
#169313=CARTESIAN_POINT('Ctrl Pts',(39.496902116,16.186186614,6.037358037));
#169314=CARTESIAN_POINT('Ctrl Pts',(37.642346032,16.400704345,6.04693133));
#169315=CARTESIAN_POINT('Ctrl Pts',(40.758824839,14.832563772,5.785100607));
#169316=CARTESIAN_POINT('Ctrl Pts',(39.497625681,16.19199005,6.003753372));
#169317=CARTESIAN_POINT('Ctrl Pts',(37.642776444,16.406159322,6.015501255));
#169318=CARTESIAN_POINT('Ctrl Pts',(40.758912814,14.833206225,5.781178488));
#169319=CARTESIAN_POINT('Ctrl Pts',(39.497705368,16.192634969,6.000019484));
#169320=CARTESIAN_POINT('Ctrl Pts',(37.642823566,16.406765512,6.012009026));
#169321=CARTESIAN_POINT('Ctrl Pts',(40.75908729,14.834491214,5.773334288));
#169322=CARTESIAN_POINT('Ctrl Pts',(39.497863322,16.193924974,5.992551733));
#169323=CARTESIAN_POINT('Ctrl Pts',(37.642916405,16.407978056,6.00502457));
#169324=CARTESIAN_POINT('Ctrl Pts',(40.759173616,14.835133938,5.769412238));
#169325=CARTESIAN_POINT('Ctrl Pts',(39.497938817,16.194545702,5.988963843));
#169326=CARTESIAN_POINT('Ctrl Pts',(37.642956809,16.408540394,6.001788326));
#169327=CARTESIAN_POINT('Ctrl Pts',(40.759431636,14.837060882,5.757645926));
#169328=CARTESIAN_POINT('Ctrl Pts',(39.498189989,16.196648331,5.976764337));
#169329=CARTESIAN_POINT('Ctrl Pts',(37.643127719,16.410661213,5.98956156));
#169330=CARTESIAN_POINT('Ctrl Pts',(40.7596033,14.838342875,5.749801339));
#169331=CARTESIAN_POINT('Ctrl Pts',(39.4983571,16.198047194,5.968630971));
#169332=CARTESIAN_POINT('Ctrl Pts',(37.643241434,16.41207217,5.981410069));
#169333=CARTESIAN_POINT('Ctrl Pts',(40.760117243,14.842180947,5.72626644));
#169334=CARTESIAN_POINT('Ctrl Pts',(39.498857423,16.202235148,5.944229649));
#169335=CARTESIAN_POINT('Ctrl Pts',(37.643581901,16.416296281,5.956954638));
#169336=CARTESIAN_POINT('Ctrl Pts',(40.760458473,14.844729119,5.710574991));
#169337=CARTESIAN_POINT('Ctrl Pts',(39.49918962,16.205015569,5.92796064400001));
#169338=CARTESIAN_POINT('Ctrl Pts',(37.643807975,16.419100674,5.940649741));
#169339=CARTESIAN_POINT('Ctrl Pts',(40.763516903,14.867567848,5.569338285));
#169340=CARTESIAN_POINT('Ctrl Pts',(39.502167359,16.229936868,5.781518502));
#169341=CARTESIAN_POINT('Ctrl Pts',(37.645834449,16.444235233,5.793893783));
#169342=CARTESIAN_POINT('Ctrl Pts',(40.766145533,14.887194818,5.443697418));
#169343=CARTESIAN_POINT('Ctrl Pts',(39.504727246,16.251350544,5.65125599));
#169344=CARTESIAN_POINT('Ctrl Pts',(37.647577316,16.465830819,5.663359465));
#169345=CARTESIAN_POINT('Ctrl Pts',(40.773757102,14.944060009,5.066480906));
#169346=CARTESIAN_POINT('Ctrl Pts',(39.512141767,16.313397558,5.260113506));
#169347=CARTESIAN_POINT('Ctrl Pts',(37.652624545,16.528398406,5.271436973));
#169348=CARTESIAN_POINT('Ctrl Pts',(40.778464317,14.979284373,4.814611652));
#169349=CARTESIAN_POINT('Ctrl Pts',(39.516728629,16.351831306,4.998925481));
#169350=CARTESIAN_POINT('Ctrl Pts',(37.655745497,16.567154219,5.009728965));
#169351=CARTESIAN_POINT('Ctrl Pts',(40.787156504,15.044350727,4.310069063));
#169352=CARTESIAN_POINT('Ctrl Pts',(39.525205623,16.422852721,4.475459016));
#169353=CARTESIAN_POINT('Ctrl Pts',(37.661519285,16.638782663,4.485122415));
#169354=CARTESIAN_POINT('Ctrl Pts',(40.791148516,15.074186157,4.057385583));
#169355=CARTESIAN_POINT('Ctrl Pts',(39.529103262,16.455424856,4.213206507));
#169356=CARTESIAN_POINT('Ctrl Pts',(37.664181346,16.67163853,4.222264054));
#169357=CARTESIAN_POINT('Ctrl Pts',(40.798402022,15.128470664,3.551231522));
#169358=CARTESIAN_POINT('Ctrl Pts',(39.536185784,16.514676164,3.687964953));
#169359=CARTESIAN_POINT('Ctrl Pts',(37.669014595,16.731388256,3.69595042));
#169360=CARTESIAN_POINT('Ctrl Pts',(40.801656447,15.152890148,3.298066981));
#169361=CARTESIAN_POINT('Ctrl Pts',(39.539364042,16.541330737,3.425233638));
#169362=CARTESIAN_POINT('Ctrl Pts',(37.671180991,16.758266063,3.432694695));
#169363=CARTESIAN_POINT('Ctrl Pts',(40.807442306,15.196288274,2.791543932));
#169364=CARTESIAN_POINT('Ctrl Pts',(39.545018929,16.588720601,2.899300501));
#169365=CARTESIAN_POINT('Ctrl Pts',(37.675040966,16.806064026,2.905577901));
#169366=CARTESIAN_POINT('Ctrl Pts',(40.809980318,15.215259628,2.538185072));
#169367=CARTESIAN_POINT('Ctrl Pts',(39.547501902,16.609436799,2.636196155));
#169368=CARTESIAN_POINT('Ctrl Pts',(37.676741572,16.826959804,2.641874102));
#169369=CARTESIAN_POINT('Ctrl Pts',(40.814321284,15.247792537,2.031255915));
#169370=CARTESIAN_POINT('Ctrl Pts',(39.551747285,16.644956426,2.109854465));
#169371=CARTESIAN_POINT('Ctrl Pts',(37.679642934,16.862777999,2.114451962));
#169372=CARTESIAN_POINT('Ctrl Pts',(40.816122814,15.261355678,1.777685697));
#169373=CARTESIAN_POINT('Ctrl Pts',(39.553508565,16.659766031,1.846564618));
#169374=CARTESIAN_POINT('Ctrl Pts',(37.680842993,16.87771189,1.850627796));
#169375=CARTESIAN_POINT('Ctrl Pts',(40.820457463,15.293904789,1.016628355));
#169376=CARTESIAN_POINT('Ctrl Pts',(39.557750402,16.695321176,1.055911698));
#169377=CARTESIAN_POINT('Ctrl Pts',(37.68374148,16.913574407,1.058156218));
#169378=CARTESIAN_POINT('Ctrl Pts',(40.821912186,15.304765143,0.508795274));
#169379=CARTESIAN_POINT('Ctrl Pts',(39.559174912,16.707176419,0.528653896));
#169380=CARTESIAN_POINT('Ctrl Pts',(37.684718817,16.925528918,0.529898357));
#169381=CARTESIAN_POINT('Ctrl Pts',(40.821913763,15.304777285,-0.507946025));
#169382=CARTESIAN_POINT('Ctrl Pts',(39.559176451,16.707189689,-0.527771518));
#169383=CARTESIAN_POINT('Ctrl Pts',(37.684719848,16.925542301,-0.529013884));
#169384=CARTESIAN_POINT('Ctrl Pts',(40.820456332,15.29389614,-1.017158744));
#169385=CARTESIAN_POINT('Ctrl Pts',(39.557749268,16.695311724,-1.056463633));
#169386=CARTESIAN_POINT('Ctrl Pts',(37.683740661,16.913564823,-1.058710206));
#169387=CARTESIAN_POINT('Ctrl Pts',(40.816115085,15.261296632,-1.778898455));
#169388=CARTESIAN_POINT('Ctrl Pts',(39.553501,16.659701558,-1.847824273));
#169389=CARTESIAN_POINT('Ctrl Pts',(37.680837852,16.877646856,-1.851890285));
#169390=CARTESIAN_POINT('Ctrl Pts',(40.814311334,15.247716927,-2.032578072));
#169391=CARTESIAN_POINT('Ctrl Pts',(39.551737559,16.644873885,-2.111227207));
#169392=CARTESIAN_POINT('Ctrl Pts',(37.679636331,16.862694772,-2.115827428));
#169393=CARTESIAN_POINT('Ctrl Pts',(40.809967909,15.215166276,-2.539492124));
#169394=CARTESIAN_POINT('Ctrl Pts',(39.547489787,16.609334903,-2.637552708));
#169395=CARTESIAN_POINT('Ctrl Pts',(37.676733338,16.826857089,-2.643233108));
#169396=CARTESIAN_POINT('Ctrl Pts',(40.807429693,15.1961937,-2.792726409));
#169397=CARTESIAN_POINT('Ctrl Pts',(39.545006622,16.58861734,-2.900527902));
#169398=CARTESIAN_POINT('Ctrl Pts',(37.675032605,16.805959925,-2.906807665));
#169399=CARTESIAN_POINT('Ctrl Pts',(40.801647463,15.152823646,-3.298765601));
#169400=CARTESIAN_POINT('Ctrl Pts',(39.539355283,16.541258183,-3.425958027));
#169401=CARTESIAN_POINT('Ctrl Pts',(37.671175018,16.758192963,-3.433419989));
#169402=CARTESIAN_POINT('Ctrl Pts',(40.798396859,15.128433441,-3.55157117));
#169403=CARTESIAN_POINT('Ctrl Pts',(39.536180742,16.514635557,-3.688317055));
#169404=CARTESIAN_POINT('Ctrl Pts',(37.669011107,16.731347348,-3.696302854));
#169405=CARTESIAN_POINT('Ctrl Pts',(40.791157226,15.074252911,-4.056774177));
#169406=CARTESIAN_POINT('Ctrl Pts',(39.52911174,16.455497695,-4.212572296));
#169407=CARTESIAN_POINT('Ctrl Pts',(37.664187034,16.671711959,-4.22162859));
#169408=CARTESIAN_POINT('Ctrl Pts',(40.787170879,15.044459629,-4.309171343));
#169409=CARTESIAN_POINT('Ctrl Pts',(39.525219617,16.422971569,-4.474527811));
#169410=CARTESIAN_POINT('Ctrl Pts',(37.661528724,16.63890248,-4.484189389));
#169411=CARTESIAN_POINT('Ctrl Pts',(40.778483089,14.979425487,-4.813572366));
#169412=CARTESIAN_POINT('Ctrl Pts',(39.516746897,16.351985238,-4.997848097));
#169413=CARTESIAN_POINT('Ctrl Pts',(37.655757861,16.567309376,-5.008649756));
#169414=CARTESIAN_POINT('Ctrl Pts',(40.773773391,14.944182001,-5.065643212));
#169415=CARTESIAN_POINT('Ctrl Pts',(39.512157622,16.313530625,-5.259245174));
#169416=CARTESIAN_POINT('Ctrl Pts',(37.652635302,16.528532533,-5.270567207));
#169417=CARTESIAN_POINT('Ctrl Pts',(40.766155287,14.887267682,-5.443228375));
#169418=CARTESIAN_POINT('Ctrl Pts',(39.504736741,16.251430029,-5.650769785));
#169419=CARTESIAN_POINT('Ctrl Pts',(37.647583772,16.46591096,-5.662872346));
#169420=CARTESIAN_POINT('Ctrl Pts',(40.76352446,14.867624282,-5.568983653));
#169421=CARTESIAN_POINT('Ctrl Pts',(39.502174716,16.229998438,-5.781150848));
#169422=CARTESIAN_POINT('Ctrl Pts',(37.645839455,16.444297322,-5.793525384));
#169423=CARTESIAN_POINT('Ctrl Pts',(40.760463586,14.844767302,-5.710339567));
#169424=CARTESIAN_POINT('Ctrl Pts',(39.499194598,16.20505723,-5.927716562));
#169425=CARTESIAN_POINT('Ctrl Pts',(37.643811362,16.419142693,-5.940405128));
#169426=CARTESIAN_POINT('Ctrl Pts',(40.760122085,14.842217105,-5.726044129));
#169427=CARTESIAN_POINT('Ctrl Pts',(39.498862136,16.2022746,-5.94399916));
#169428=CARTESIAN_POINT('Ctrl Pts',(37.643585108,16.416336073,-5.956723643));
#169429=CARTESIAN_POINT('Ctrl Pts',(40.759607736,14.838376002,-5.7495985));
#169430=CARTESIAN_POINT('Ctrl Pts',(39.498361418,16.19808334,-5.968420666));
#169431=CARTESIAN_POINT('Ctrl Pts',(37.643244372,16.412108628,-5.981199297));
#169432=CARTESIAN_POINT('Ctrl Pts',(40.759435936,14.837092999,-5.757449545));
#169433=CARTESIAN_POINT('Ctrl Pts',(39.498194175,16.196683375,-5.976560726));
#169434=CARTESIAN_POINT('Ctrl Pts',(37.643130568,16.410696561,-5.989357496));
#169435=CARTESIAN_POINT('Ctrl Pts',(40.759177714,14.835164542,-5.769225494));
#169436=CARTESIAN_POINT('Ctrl Pts',(39.497942806,16.194579097,-5.988770223));
#169437=CARTESIAN_POINT('Ctrl Pts',(37.642959524,16.408574077,-6.001594272));
#169438=CARTESIAN_POINT('Ctrl Pts',(40.759091349,14.834521283,-5.773150745));
#169439=CARTESIAN_POINT('Ctrl Pts',(39.497866996,16.193955161,-5.992376998));
#169440=CARTESIAN_POINT('Ctrl Pts',(37.642918555,16.40800643,-6.004861143));
#169441=CARTESIAN_POINT('Ctrl Pts',(40.758916777,14.833235242,-5.781001351));
#169442=CARTESIAN_POINT('Ctrl Pts',(39.497708956,16.192664097,-5.999850847));
#169443=CARTESIAN_POINT('Ctrl Pts',(37.642825683,16.406792891,-6.011851303));
#169444=CARTESIAN_POINT('Ctrl Pts',(40.758828752,14.832592262,-5.784926672));
#169445=CARTESIAN_POINT('Ctrl Pts',(39.497629226,16.19201865,-6.003587784));
#169446=CARTESIAN_POINT('Ctrl Pts',(37.642778544,16.406186204,-6.015346383));
#169447=CARTESIAN_POINT('Ctrl Pts',(40.758029882,14.826805822,-5.820254721));
#169448=CARTESIAN_POINT('Ctrl Pts',(39.496905256,16.186210456,-6.037219868));
#169449=CARTESIAN_POINT('Ctrl Pts',(37.642347965,16.400726754,-6.046802108));
#169450=CARTESIAN_POINT('Ctrl Pts',(40.757272512,14.821664967,-5.851658579));
#169451=CARTESIAN_POINT('Ctrl Pts',(39.496216195,16.18105293,-6.067116234));
#169452=CARTESIAN_POINT('Ctrl Pts',(37.641920222,16.395879153,-6.074762766));
#169453=CARTESIAN_POINT('Ctrl Pts',(40.755663093,14.811388551,-5.91446863));
#169454=CARTESIAN_POINT('Ctrl Pts',(39.494746881,16.170748665,-6.126910513));
#169455=CARTESIAN_POINT('Ctrl Pts',(37.640974594,16.386194455,-6.13068411));
#169456=CARTESIAN_POINT('Ctrl Pts',(40.754811046,14.80625299,-5.945874822));
#169457=CARTESIAN_POINT('Ctrl Pts',(39.49396663,16.165601921,-6.156808447));
#169458=CARTESIAN_POINT('Ctrl Pts',(37.640456709,16.381357358,-6.158644796));
#169459=CARTESIAN_POINT('Ctrl Pts',(40.75379915,14.800478462,-5.981208124));
#169460=CARTESIAN_POINT('Ctrl Pts',(39.493037461,16.159817832,-6.190444947));
#169461=CARTESIAN_POINT('Ctrl Pts',(37.639823306,16.375921541,-6.190100585));
#169462=CARTESIAN_POINT('Ctrl Pts',(40.753685977,14.799836889,-5.985134065));
#169463=CARTESIAN_POINT('Ctrl Pts',(39.492933508,16.159175248,-6.1941823));
#169464=CARTESIAN_POINT('Ctrl Pts',(37.639752223,16.375317643,-6.193595672));
#169465=CARTESIAN_POINT('Ctrl Pts',(40.753515105,14.798874591,-5.991023005));
#169466=CARTESIAN_POINT('Ctrl Pts',(39.492776507,16.158211498,-6.199788354));
#169467=CARTESIAN_POINT('Ctrl Pts',(37.63964454,16.37441192,-6.198838304));
#169468=CARTESIAN_POINT('Ctrl Pts',(40.753457962,14.798553836,-5.992985989));
#169469=CARTESIAN_POINT('Ctrl Pts',(39.492723996,16.157890269,-6.20165704));
#169470=CARTESIAN_POINT('Ctrl Pts',(37.639608469,16.374110033,-6.200585848));
#169471=CARTESIAN_POINT('Ctrl Pts',(40.753343306,14.797912345,-5.996911967));
#169472=CARTESIAN_POINT('Ctrl Pts',(39.492618615,16.157247854,-6.205394418));
#169473=CARTESIAN_POINT('Ctrl Pts',(37.639535975,16.3735063,-6.204080937));
#169474=CARTESIAN_POINT('Ctrl Pts',(40.753276266,14.797583073,-5.998972286));
#169475=CARTESIAN_POINT('Ctrl Pts',(39.492558303,16.156917949,-6.20731784200001));
#169476=CARTESIAN_POINT('Ctrl Pts',(37.639499511,16.373204459,-6.205828481));
#169477=CARTESIAN_POINT('Ctrl Pts',(40.753080287,14.796062493,-6.007840791));
#169478=CARTESIAN_POINT('Ctrl Pts',(39.492365314,16.155396924,-6.21612907300001));
#169479=CARTESIAN_POINT('Ctrl Pts',(37.639316767,16.371695301,-6.214566202));
#169480=CARTESIAN_POINT('Ctrl Pts',(40.752943895,14.794864397,-6.014726342));
#169481=CARTESIAN_POINT('Ctrl Pts',(39.492226832,16.154198859,-6.22306039200001));
#169482=CARTESIAN_POINT('Ctrl Pts',(37.639170565,16.370487977,-6.221556379));
#169483=CARTESIAN_POINT('Ctrl Pts',(40.752504133,14.791242557,-6.035696874));
#169484=CARTESIAN_POINT('Ctrl Pts',(39.491787521,16.150576532,-6.244030848));
#169485=CARTESIAN_POINT('Ctrl Pts',(37.638731969,16.366866001,-6.242526909));
#169486=CARTESIAN_POINT('Ctrl Pts',(40.752210958,14.788827997,-6.049677228));
#169487=CARTESIAN_POINT('Ctrl Pts',(39.491494647,16.148161647,-6.258011152));
#169488=CARTESIAN_POINT('Ctrl Pts',(37.638439571,16.36445135,-6.256507263));
#169489=CARTESIAN_POINT('Ctrl Pts',(40.751917783,14.786413437,-6.063657583));
#169490=CARTESIAN_POINT('Ctrl Pts',(39.491201774,16.145746763,-6.271991456));
#169491=CARTESIAN_POINT('Ctrl Pts',(37.638147174,16.3620367,-6.270487617));
#169492=CARTESIAN_POINT('',(37.642982287708,16.4088504732111,6.0000000045992));
#169493=CARTESIAN_POINT('Ctrl Pts',(40.7532527124878,14.7974077924331,6.));
#169494=CARTESIAN_POINT('Ctrl Pts',(40.7041458477828,14.8519463637135,6.));
#169495=CARTESIAN_POINT('Ctrl Pts',(40.6538706170833,14.9053759733606,6.));
#169496=CARTESIAN_POINT('Ctrl Pts',(40.5506448722851,15.010356926483,6.));
#169497=CARTESIAN_POINT('Ctrl Pts',(40.4977017931235,15.0618690951414,6.));
#169498=CARTESIAN_POINT('Ctrl Pts',(40.3346211356183,15.2136538826667,6.));
#169499=CARTESIAN_POINT('Ctrl Pts',(40.2211264418376,15.310195291988,5.99999999999999));
#169500=CARTESIAN_POINT('Ctrl Pts',(39.8658746237043,15.5859305264852,5.99999999999999));
#169501=CARTESIAN_POINT('Ctrl Pts',(39.6120785669462,15.7484508164354,6.));
#169502=CARTESIAN_POINT('Ctrl Pts',(38.8138839016999,16.1625756328312,6.));
#169503=CARTESIAN_POINT('Ctrl Pts',(38.2373926026142,16.3395581228118,6.));
#169504=CARTESIAN_POINT('Ctrl Pts',(37.6429823003743,16.408850490623,6.));
#169505=CARTESIAN_POINT('',(37.6429823613304,16.4088504659907,-6.0000000042585));
#169506=CARTESIAN_POINT('Ctrl Pts',(40.7532527120421,14.7974077933766,-6.));
#169507=CARTESIAN_POINT('Ctrl Pts',(40.7041462463511,14.8519459198948,-6.));
#169508=CARTESIAN_POINT('Ctrl Pts',(40.6538706921651,14.9053758982138,-6.));
#169509=CARTESIAN_POINT('Ctrl Pts',(40.5506448319582,15.010356966506,-6.));
#169510=CARTESIAN_POINT('Ctrl Pts',(40.4977017441792,15.0618691421542,-6.));
#169511=CARTESIAN_POINT('Ctrl Pts',(40.3346210695018,15.2136539406401,-6.));
#169512=CARTESIAN_POINT('Ctrl Pts',(40.2211263668839,15.3101953538551,-5.99999999999999));
#169513=CARTESIAN_POINT('Ctrl Pts',(39.8658745654662,15.5859305633178,-5.99999999999999));
#169514=CARTESIAN_POINT('Ctrl Pts',(39.6120785407188,15.7484508290523,-6.));
#169515=CARTESIAN_POINT('Ctrl Pts',(38.8138839072929,16.1625756319594,-6.));
#169516=CARTESIAN_POINT('Ctrl Pts',(38.2373926217034,16.3395581146185,-6.));
#169517=CARTESIAN_POINT('Ctrl Pts',(37.6429823707101,16.4088504849673,-6.));
#169518=CARTESIAN_POINT('Ctrl Pts',(37.6429823002787,16.4088504893088,6.0000000075678));
#169519=CARTESIAN_POINT('Ctrl Pts',(37.6429925922719,16.4089782150111,5.99926381250339));
#169520=CARTESIAN_POINT('Ctrl Pts',(37.6430033422842,16.4091100012393,5.99850405484267));
#169521=CARTESIAN_POINT('Ctrl Pts',(37.6430147153378,16.4092472256471,5.9977127308646));
#169522=CARTESIAN_POINT('Ctrl Pts',(37.643131982462,16.4106621413092,5.98955341935717));
#169523=CARTESIAN_POINT('Ctrl Pts',(37.6432488657212,16.4120727214878,5.98140193700194));
#169524=CARTESIAN_POINT('Ctrl Pts',(37.6433653672416,16.413479002002,5.97325818682279));
#169525=CARTESIAN_POINT('Ctrl Pts',(37.6435990613265,16.4162999045681,5.95692238073991));
#169526=CARTESIAN_POINT('Ctrl Pts',(37.6438312194001,16.4191035056322,5.94061768806421));
#169527=CARTESIAN_POINT('Ctrl Pts',(37.6440618602537,16.4218900884576,5.924343327567));
#169528=CARTESIAN_POINT('Ctrl Pts',(37.6459383777535,16.4445620104253,5.79193347133972));
#169529=CARTESIAN_POINT('Ctrl Pts',(37.6477143696341,16.4661094409072,5.66153131418037));
#169530=CARTESIAN_POINT('Ctrl Pts',(37.6494005148935,16.4866704133275,5.53271773759048));
#169531=CARTESIAN_POINT('Ctrl Pts',(37.6515766957273,16.5132069135807,5.36646774523038));
#169532=CARTESIAN_POINT('Ctrl Pts',(37.6536026100879,16.5381029580661,5.20286396472447));
#169533=CARTESIAN_POINT('Ctrl Pts',(37.6555042291047,16.5615958150815,5.04100789616993));
#169534=CARTESIAN_POINT('Ctrl Pts',(37.6566607841939,16.5758840521591,4.94256785209843));
#169535=CARTESIAN_POINT('Ctrl Pts',(37.6577712692573,16.5896522020657,4.84477428699897));
#169536=CARTESIAN_POINT('Ctrl Pts',(37.6588407221678,16.6029443150722,4.74742454727631));
#169537=CARTESIAN_POINT('Ctrl Pts',(37.6606256646561,16.6251291696188,4.5849455031368));
#169538=CARTESIAN_POINT('Ctrl Pts',(37.6623000107574,16.6459842024763,4.42371918013501));
#169539=CARTESIAN_POINT('Ctrl Pts',(37.6638766613543,16.6656642734245,4.26289497760677));
#169540=CARTESIAN_POINT('Ctrl Pts',(37.6648702582042,16.678066549832,4.16154441753981));
#169541=CARTESIAN_POINT('Ctrl Pts',(37.665824986514,16.6900011746096,4.06035325873642));
#169542=CARTESIAN_POINT('Ctrl Pts',(37.6667432984757,16.7014965325222,3.95910657464045));
#169543=CARTESIAN_POINT('Ctrl Pts',(37.6682023425559,16.7197607331537,3.79824253146168));
#169544=CARTESIAN_POINT('Ctrl Pts',(37.6695678772653,16.7369126495672,3.63731299534655));
#169545=CARTESIAN_POINT('Ctrl Pts',(37.6708542262411,16.7530337280781,3.47534718421044));
#169546=CARTESIAN_POINT('Ctrl Pts',(37.6716610042114,16.7631446165251,3.37376475921804));
#169547=CARTESIAN_POINT('Ctrl Pts',(37.67243655048,16.7728489995321,3.27177465177766));
#169548=CARTESIAN_POINT('Ctrl Pts',(37.6731835960051,16.7821566076102,3.16913603168301));
#169549=CARTESIAN_POINT('Ctrl Pts',(37.6736139439681,16.7875184095921,3.11000935251626));
#169550=CARTESIAN_POINT('Ctrl Pts',(37.6740351776649,16.7927471664175,3.05067533514802));
#169551=CARTESIAN_POINT('Ctrl Pts',(37.6744473409751,16.79784346694,2.99109183013576));
#169552=CARTESIAN_POINT('Ctrl Pts',(37.6758619748775,16.8153350760109,2.7865883138774));
#169553=CARTESIAN_POINT('Ctrl Pts',(37.6771323103164,16.8310053965011,2.5821957216556));
#169554=CARTESIAN_POINT('Ctrl Pts',(37.6782497341041,16.8448622153274,2.37816287453634));
#169555=CARTESIAN_POINT('Ctrl Pts',(37.6796980785756,16.8628226768462,2.11370649784581));
#169556=CARTESIAN_POINT('Ctrl Pts',(37.6808888047079,16.8777467837798,1.84974709873201));
#169557=CARTESIAN_POINT('Ctrl Pts',(37.6818433082319,16.8896620864771,1.5864705405855));
#169558=CARTESIAN_POINT('Ctrl Pts',(37.6828847653763,16.9026628526441,1.29920994329351));
#169559=CARTESIAN_POINT('Ctrl Pts',(37.6836391356913,16.912070715238,1.01317287593597));
#169560=CARTESIAN_POINT('Ctrl Pts',(37.6841128849961,16.9179769777172,0.728685437826341));
#169561=CARTESIAN_POINT('Ctrl Pts',(37.6845191434982,16.9230418280994,0.484726366463135));
#169562=CARTESIAN_POINT('Ctrl Pts',(37.6847191100984,16.9255325562844,0.24190685609632));
#169563=CARTESIAN_POINT('Ctrl Pts',(37.6847193418195,16.9255356084144,0.000442236499989826));
#169564=CARTESIAN_POINT('Ctrl Pts',(37.6847193420007,16.9255356108004,0.000253469149640141));
#169565=CARTESIAN_POINT('Ctrl Pts',(37.6847193420595,16.9255356116628,6.47027496648115E-5));
#169566=CARTESIAN_POINT('Ctrl Pts',(37.684719341996,16.9255356110016,-0.000124062699716917));
#169567=CARTESIAN_POINT('Ctrl Pts',(37.6847192386803,16.9255345349064,-0.30734925937092));
#169568=CARTESIAN_POINT('Ctrl Pts',(37.6843947361347,16.9214935383538,-0.616974244090195));
#169569=CARTESIAN_POINT('Ctrl Pts',(37.6837342985532,16.9132579103563,-0.928286699200675));
#169570=CARTESIAN_POINT('Ctrl Pts',(37.683269727296,16.9074647269285,-1.1472730541378));
#169571=CARTESIAN_POINT('Ctrl Pts',(37.6826390212237,16.8995969890998,-1.36709393472077));
#169572=CARTESIAN_POINT('Ctrl Pts',(37.6818394494684,16.8896155542583,-1.58749686283055));
#169573=CARTESIAN_POINT('Ctrl Pts',(37.6808837790525,16.8776854655275,-1.85092857687063));
#169574=CARTESIAN_POINT('Ctrl Pts',(37.6796919347013,16.8627475693438,-2.11496323925901));
#169575=CARTESIAN_POINT('Ctrl Pts',(37.6782421309094,16.8447692658226,-2.37953011096301));
#169576=CARTESIAN_POINT('Ctrl Pts',(37.6771265421743,16.830935398788,-2.58310788016746));
#169577=CARTESIAN_POINT('Ctrl Pts',(37.6758586480912,16.8152949680196,-2.78706461269959));
#169578=CARTESIAN_POINT('Ctrl Pts',(37.6744464866802,16.7978338566875,-2.99120437122007));
#169579=CARTESIAN_POINT('Ctrl Pts',(37.6740321976202,16.7927112500622,-3.05109332442538));
#169580=CARTESIAN_POINT('Ctrl Pts',(37.6736089163171,16.7874561308731,-3.11071494281208));
#169581=CARTESIAN_POINT('Ctrl Pts',(37.6731765922391,16.7820679881559,-3.17011356001915));
#169582=CARTESIAN_POINT('Ctrl Pts',(37.6719959997406,16.7673540242656,-3.33231956579711));
#169583=CARTESIAN_POINT('Ctrl Pts',(37.6707455666381,16.7516609616766,-3.492804686427));
#169584=CARTESIAN_POINT('Ctrl Pts',(37.6694136223789,16.7349416760638,-3.65254969798757));
#169585=CARTESIAN_POINT('Ctrl Pts',(37.6685601749132,16.7242287413159,-3.75490681567617));
#169586=CARTESIAN_POINT('Ctrl Pts',(37.6676731846034,16.7130934292427,-3.85695982795663));
#169587=CARTESIAN_POINT('Ctrl Pts',(37.6667487152684,16.7015122921313,-3.95896503998955));
#169588=CARTESIAN_POINT('Ctrl Pts',(37.665306642091,16.6834469582562,-4.11808224883185));
#169589=CARTESIAN_POINT('Ctrl Pts',(37.6637742446663,16.6642921097485,-4.27712657394183));
#169590=CARTESIAN_POINT('Ctrl Pts',(37.6621403719767,16.6439201569281,-4.43697154140125));
#169591=CARTESIAN_POINT('Ctrl Pts',(37.6610901895404,16.6308259500296,-4.53971294739439));
#169592=CARTESIAN_POINT('Ctrl Pts',(37.6599980009714,16.6172278877262,-4.64278508072804));
#169593=CARTESIAN_POINT('Ctrl Pts',(37.6588600171528,16.6030808298185,-4.74641838392531));
#169594=CARTESIAN_POINT('Ctrl Pts',(37.657119320718,16.5814410377048,-4.90493919806702));
#169595=CARTESIAN_POINT('Ctrl Pts',(37.6552680517578,16.5585216278763,-5.06477985982275));
#169596=CARTESIAN_POINT('Ctrl Pts',(37.6532832560602,16.5341212991504,-5.22679404690265));
#169597=CARTESIAN_POINT('Ctrl Pts',(37.6520476529005,16.5189312605446,-5.32765341581011));
#169598=CARTESIAN_POINT('Ctrl Pts',(37.6507602197946,16.5031663188093,-5.42935499142178));
#169599=CARTESIAN_POINT('Ctrl Pts',(37.6494145427316,16.4867678402838,-5.5321030305694));
#169600=CARTESIAN_POINT('Ctrl Pts',(37.6477264810273,16.4661970478038,-5.66099356073221));
#169601=CARTESIAN_POINT('Ctrl Pts',(37.6459475667309,16.4446329529361,-5.79151094819494));
#169602=CARTESIAN_POINT('Ctrl Pts',(37.644066757918,16.4219341838855,-5.92408495149976));
#169603=CARTESIAN_POINT('Ctrl Pts',(37.6438356927928,16.4191455464254,-5.94037221496444));
#169604=CARTESIAN_POINT('Ctrl Pts',(37.6436030908199,16.4163397511713,-5.95669052135907));
#169605=CARTESIAN_POINT('Ctrl Pts',(37.6433689332556,16.4135165092223,-5.97304067012239));
#169606=CARTESIAN_POINT('Ctrl Pts',(37.6432522096014,16.4121091700319,-5.98119094754805));
#169607=CARTESIAN_POINT('Ctrl Pts',(37.6431350999015,16.410697496005,-5.98934913810345));
#169608=CARTESIAN_POINT('Ctrl Pts',(37.6430176009401,16.4092814491186,-5.99751533932816));
#169609=CARTESIAN_POINT('Ctrl Pts',(37.6430052115928,16.4091321380398,-5.99837640143482));
#169610=CARTESIAN_POINT('Ctrl Pts',(37.6429935354935,16.4089890431194,-5.9992013678156));
#169611=CARTESIAN_POINT('Ctrl Pts',(37.6429823705982,16.4088504836746,-6.00000000745612));
#169612=CARTESIAN_POINT('Ctrl Pts',(12.322789768,18.544964634,-6.));
#169613=CARTESIAN_POINT('Ctrl Pts',(20.805042813,18.10080432,-6.));
#169614=CARTESIAN_POINT('Ctrl Pts',(29.218799064,17.39099662,-6.));
#169615=CARTESIAN_POINT('Ctrl Pts',(37.696982896,16.402554748,-6.));
#169616=CARTESIAN_POINT('Ctrl Pts',(37.745830911,16.396859728,-6.));
#169617=CARTESIAN_POINT('Ctrl Pts',(37.794678925,16.391164709,-6.));
#169618=CARTESIAN_POINT('Ctrl Pts',(12.327415095,18.633221115,-5.492095716));
#169619=CARTESIAN_POINT('Ctrl Pts',(20.811370844,18.187540467,-5.499959461));
#169620=CARTESIAN_POINT('Ctrl Pts',(29.226829801,17.476212432,-5.507823206));
#169621=CARTESIAN_POINT('Ctrl Pts',(37.706726206,16.486241416,-5.515732521));
#169622=CARTESIAN_POINT('Ctrl Pts',(37.755584088,16.480537586,-5.515778092));
#169623=CARTESIAN_POINT('Ctrl Pts',(37.80444197,16.474833756,-5.515823662));
#169624=CARTESIAN_POINT('Ctrl Pts',(12.33537271,18.785061463,-4.485838856));
#169625=CARTESIAN_POINT('Ctrl Pts',(20.822453735,18.33838052,-4.501664827));
#169626=CARTESIAN_POINT('Ctrl Pts',(29.241037967,17.626052192,-4.517490798));
#169627=CARTESIAN_POINT('Ctrl Pts',(37.724077758,16.635075084,-4.53340848));
#169628=CARTESIAN_POINT('Ctrl Pts',(37.772953751,16.629365458,-4.533500192));
#169629=CARTESIAN_POINT('Ctrl Pts',(37.821829744,16.623655831,-4.533591903));
#169630=CARTESIAN_POINT('Ctrl Pts',(12.343761894,18.945136627,-2.991664426));
#169631=CARTESIAN_POINT('Ctrl Pts',(20.83436062,18.49923972,-3.004604703));
#169632=CARTESIAN_POINT('Ctrl Pts',(29.256462552,17.787695426,-3.01754498));
#169633=CARTESIAN_POINT('Ctrl Pts',(37.743040429,16.797506898,-3.030560246));
#169634=CARTESIAN_POINT('Ctrl Pts',(37.791936807,16.791801815,-3.030635235));
#169635=CARTESIAN_POINT('Ctrl Pts',(37.840833185,16.786096731,-3.030710224));
#169636=CARTESIAN_POINT('Ctrl Pts',(12.348776536,19.0408217,-1.50111232));
#169637=CARTESIAN_POINT('Ctrl Pts',(20.841516732,18.59571313,-1.505109267));
#169638=CARTESIAN_POINT('Ctrl Pts',(29.265760136,17.884957174,-1.509106213));
#169639=CARTESIAN_POINT('Ctrl Pts',(37.754491893,16.895561551,-1.513126323));
#169640=CARTESIAN_POINT('Ctrl Pts',(37.803400681,16.889861036,-1.513149485));
#169641=CARTESIAN_POINT('Ctrl Pts',(37.852309468,16.884160521,-1.513172647));
#169642=CARTESIAN_POINT('Ctrl Pts',(12.349906111,19.062375268,-0.502481944));
#169643=CARTESIAN_POINT('Ctrl Pts',(20.843107004,18.617265471,-0.502481944));
#169644=CARTESIAN_POINT('Ctrl Pts',(29.267811104,17.906508286,-0.502481944));
#169645=CARTESIAN_POINT('Ctrl Pts',(37.757006229,16.917111428,-0.502481944));
#169646=CARTESIAN_POINT('Ctrl Pts',(37.805917686,16.911410906,-0.502481944));
#169647=CARTESIAN_POINT('Ctrl Pts',(37.854829143,16.905710385,-0.502481944));
#169648=CARTESIAN_POINT('Ctrl Pts',(12.349906111,19.062375268,0.502481944));
#169649=CARTESIAN_POINT('Ctrl Pts',(20.843107004,18.617265471,0.502481944));
#169650=CARTESIAN_POINT('Ctrl Pts',(29.267811104,17.906508286,0.502481944));
#169651=CARTESIAN_POINT('Ctrl Pts',(37.757006229,16.917111428,0.502481944));
#169652=CARTESIAN_POINT('Ctrl Pts',(37.805917686,16.911410906,0.502481944));
#169653=CARTESIAN_POINT('Ctrl Pts',(37.854829143,16.905710385,0.502481944));
#169654=CARTESIAN_POINT('Ctrl Pts',(12.348776556,19.040822084,1.501116545));
#169655=CARTESIAN_POINT('Ctrl Pts',(20.841516748,18.595713412,1.505111951));
#169656=CARTESIAN_POINT('Ctrl Pts',(29.265760148,17.884957354,1.509107358));
#169657=CARTESIAN_POINT('Ctrl Pts',(37.754491901,16.895561629,1.513125918));
#169658=CARTESIAN_POINT('Ctrl Pts',(37.803400688,16.889861114,1.513149071));
#169659=CARTESIAN_POINT('Ctrl Pts',(37.852309476,16.884160598,1.513172225));
#169660=CARTESIAN_POINT('Ctrl Pts',(12.343761876,18.945136279,2.991660231));
#169661=CARTESIAN_POINT('Ctrl Pts',(20.834360626,18.499239639,3.004600343));
#169662=CARTESIAN_POINT('Ctrl Pts',(29.256462584,17.787695613,3.017540455));
#169663=CARTESIAN_POINT('Ctrl Pts',(37.743040486,16.797507354,3.030555555));
#169664=CARTESIAN_POINT('Ctrl Pts',(37.791936864,16.791802272,3.030630543));
#169665=CARTESIAN_POINT('Ctrl Pts',(37.840833242,16.786097191,3.030705531));
#169666=CARTESIAN_POINT('Ctrl Pts',(12.335372745,18.785062123,4.485837733));
#169667=CARTESIAN_POINT('Ctrl Pts',(20.822453727,18.338380717,4.501665456));
#169668=CARTESIAN_POINT('Ctrl Pts',(29.241037917,17.626051924,4.517493179));
#169669=CARTESIAN_POINT('Ctrl Pts',(37.724077666,16.63507435,4.533412624));
#169670=CARTESIAN_POINT('Ctrl Pts',(37.772953659,16.629364721,4.533504345));
#169671=CARTESIAN_POINT('Ctrl Pts',(37.821829651,16.623655091,4.533596067));
#169672=CARTESIAN_POINT('Ctrl Pts',(12.327415095,18.633221115,5.492095716));
#169673=CARTESIAN_POINT('Ctrl Pts',(20.811370844,18.187540467,5.499959461));
#169674=CARTESIAN_POINT('Ctrl Pts',(29.226829801,17.476212432,5.507823206));
#169675=CARTESIAN_POINT('Ctrl Pts',(37.706726206,16.486241416,5.515732521));
#169676=CARTESIAN_POINT('Ctrl Pts',(37.755584088,16.480537586,5.515778092));
#169677=CARTESIAN_POINT('Ctrl Pts',(37.80444197,16.474833756,5.515823662));
#169678=CARTESIAN_POINT('Ctrl Pts',(12.322789768,18.544964634,6.));
#169679=CARTESIAN_POINT('Ctrl Pts',(20.805042813,18.10080432,6.));
#169680=CARTESIAN_POINT('Ctrl Pts',(29.218799064,17.39099662,6.));
#169681=CARTESIAN_POINT('Ctrl Pts',(37.696982896,16.402554748,6.));
#169682=CARTESIAN_POINT('Ctrl Pts',(37.745830911,16.396859728,6.));
#169683=CARTESIAN_POINT('Ctrl Pts',(37.794678925,16.391164709,6.));
#169684=CARTESIAN_POINT('',(12.3227897708766,18.5449646343773,-6.00000000073637));
#169685=CARTESIAN_POINT('Ctrl Pts',(37.6429823592795,16.4088504483972,-6.));
#169686=CARTESIAN_POINT('Ctrl Pts',(29.215370394797,17.3912858606986,-6.));
#169687=CARTESIAN_POINT('Ctrl Pts',(20.8033145247598,18.1008948191318,-6.));
#169688=CARTESIAN_POINT('Ctrl Pts',(12.322789770849,18.5449646338508,-6.));
#169689=CARTESIAN_POINT('',(12.3227897695898,18.5449646340518,5.99999999988931));
#169690=CARTESIAN_POINT('Origin',(10.5181481816952,-15.8896585700102,-1.0547118733939E-13));
#169691=CARTESIAN_POINT('Ctrl Pts',(37.6429822858137,16.4088504569613,6.));
#169692=CARTESIAN_POINT('Ctrl Pts',(29.2153703459101,17.3912858648225,6.));
#169693=CARTESIAN_POINT('Ctrl Pts',(20.8033145001175,18.1008948204222,6.));
#169694=CARTESIAN_POINT('Ctrl Pts',(12.322789770849,18.5449646338508,6.));
#169695=CARTESIAN_POINT('Ctrl Pts',(5.858730877,11.405676811,-6.07136287));
#169696=CARTESIAN_POINT('Ctrl Pts',(6.548706819,14.528840635,-6.62786704299999));
#169697=CARTESIAN_POINT('Ctrl Pts',(9.792928396,14.486011331,-6.742357133));
#169698=CARTESIAN_POINT('Ctrl Pts',(5.861554445,11.418457643,-5.945982486));
#169699=CARTESIAN_POINT('Ctrl Pts',(6.545583205,14.547062662,-6.502968281));
#169700=CARTESIAN_POINT('Ctrl Pts',(9.793925217,14.507341164,-6.616966439));
#169701=CARTESIAN_POINT('Ctrl Pts',(5.864335028,11.43124245,-5.820600981));
#169702=CARTESIAN_POINT('Ctrl Pts',(6.542390433,14.565263133,-6.378128918));
#169703=CARTESIAN_POINT('Ctrl Pts',(9.794847306,14.528672929,-6.491571576));
#169704=CARTESIAN_POINT('Ctrl Pts',(5.868441471,11.450425087,-5.632526913));
#169705=CARTESIAN_POINT('Ctrl Pts',(6.537496645,14.592536166,-6.190912081));
#169706=CARTESIAN_POINT('Ctrl Pts',(9.796116904,14.560672554,-6.303472858));
#169707=CARTESIAN_POINT('Ctrl Pts',(5.869799547,11.456820204,-5.569835256));
#169708=CARTESIAN_POINT('Ctrl Pts',(6.535847312,14.601625942,-6.128490283));
#169709=CARTESIAN_POINT('Ctrl Pts',(9.79652118,14.571339425,-6.240772214));
#169710=CARTESIAN_POINT('Ctrl Pts',(5.871820559,11.466414169,-5.475797302));
#169711=CARTESIAN_POINT('Ctrl Pts',(6.53334715300001,14.615253408,-6.03486809500001));
#169712=CARTESIAN_POINT('Ctrl Pts',(9.79709903,14.58734011,-6.14671962));
#169713=CARTESIAN_POINT('Ctrl Pts',(5.872491546,11.469612372,-5.44445124));
#169714=CARTESIAN_POINT('Ctrl Pts',(6.53250924799999,14.619795542,-6.003656642));
#169715=CARTESIAN_POINT('Ctrl Pts',(9.797286886,14.592673734,-6.115368484));
#169716=CARTESIAN_POINT('Ctrl Pts',(5.873494003,11.474409991,-5.397432027));
#169717=CARTESIAN_POINT('Ctrl Pts',(6.531245852,14.626606909,-5.95684208399999));
#169718=CARTESIAN_POINT('Ctrl Pts',(9.797561506,14.600674251,-6.068341371));
#169719=CARTESIAN_POINT('Ctrl Pts',(5.873827484,11.47600925,-5.381758936));
#169720=CARTESIAN_POINT('Ctrl Pts',(6.530823591,14.628877271,-5.94123621600001));
#169721=CARTESIAN_POINT('Ctrl Pts',(9.797651851,14.603341103,-6.052665598));
#169722=CARTESIAN_POINT('Ctrl Pts',(5.8743267,11.478408216,-5.35824927));
#169723=CARTESIAN_POINT('Ctrl Pts',(6.530188563,14.632282349,-5.917828068));
#169724=CARTESIAN_POINT('Ctrl Pts',(9.797785576,14.607341399,-6.029151836));
#169725=CARTESIAN_POINT('Ctrl Pts',(5.874492938,11.479207884,-5.35041271));
#169726=CARTESIAN_POINT('Ctrl Pts',(6.52997660500001,14.633417351,-5.91002509800001));
#169727=CARTESIAN_POINT('Ctrl Pts',(9.797829852,14.608674834,-6.021313898));
#169728=CARTESIAN_POINT('Ctrl Pts',(5.874742043,11.480407405,-5.338657861));
#169729=CARTESIAN_POINT('Ctrl Pts',(6.529658259,14.635119738,-5.898320807));
#169730=CARTESIAN_POINT('Ctrl Pts',(9.797895818,14.610674991,-6.009556966));
#169731=CARTESIAN_POINT('Ctrl Pts',(5.874825036,11.480807249,-5.334739577));
#169732=CARTESIAN_POINT('Ctrl Pts',(6.529552073,14.635687194,-5.894419313));
#169733=CARTESIAN_POINT('Ctrl Pts',(9.797917731,14.611341711,-6.005637984));
#169734=CARTESIAN_POINT('Ctrl Pts',(5.874990938,11.481606943,-5.326903007));
#169735=CARTESIAN_POINT('Ctrl Pts',(6.529339564,14.636822076,-5.886616319));
#169736=CARTESIAN_POINT('Ctrl Pts',(9.797961409,14.612675152,-5.997800012));
#169737=CARTESIAN_POINT('Ctrl Pts',(5.875073803,11.48200658,-5.322984668));
#169738=CARTESIAN_POINT('Ctrl Pts',(6.529247215,14.637456319,-5.882064614));
#169739=CARTESIAN_POINT('Ctrl Pts',(9.797957984,14.613472876,-5.993108854));
#169740=CARTESIAN_POINT('Ctrl Pts',(5.880449993,11.50794786,-5.068283718));
#169741=CARTESIAN_POINT('Ctrl Pts',(6.52291790199999,14.677089485,-5.601170537));
#169742=CARTESIAN_POINT('Ctrl Pts',(9.79831837,14.662187405,-5.706218389));
#169743=CARTESIAN_POINT('Ctrl Pts',(5.885197279,11.531688249,-4.817044188));
#169744=CARTESIAN_POINT('Ctrl Pts',(6.51682845,14.71329959,-5.32418104));
#169745=CARTESIAN_POINT('Ctrl Pts',(9.798332145,14.70673276,-5.423259124));
#169746=CARTESIAN_POINT('Ctrl Pts',(5.898005992,11.597492508,-4.061961581));
#169747=CARTESIAN_POINT('Ctrl Pts',(6.49931662200001,14.813695466,-4.490653682));
#169748=CARTESIAN_POINT('Ctrl Pts',(9.797716555,14.830132736,-4.572917229));
#169749=CARTESIAN_POINT('Ctrl Pts',(5.904645385,11.634142573,-3.556755763));
#169750=CARTESIAN_POINT('Ctrl Pts',(6.488702427,14.869437222,-3.933025041));
#169751=CARTESIAN_POINT('Ctrl Pts',(9.796448164,14.89875956,-4.004074322));
#169752=CARTESIAN_POINT('Ctrl Pts',(5.912372151,11.678198728,-2.796229212));
#169753=CARTESIAN_POINT('Ctrl Pts',(6.475482211,14.936409695,-3.092941977));
#169754=CARTESIAN_POINT('Ctrl Pts',(9.794420092,14.981209295,-3.147746793));
#169755=CARTESIAN_POINT('Ctrl Pts',(5.91457177,11.691057231,-2.542330331));
#169756=CARTESIAN_POINT('Ctrl Pts',(6.471523067,14.955948086,-2.812266956));
#169757=CARTESIAN_POINT('Ctrl Pts',(9.793718352,15.005264335,-2.861852142));
#169758=CARTESIAN_POINT('Ctrl Pts',(5.918286894,11.713083094,-2.034565643));
#169759=CARTESIAN_POINT('Ctrl Pts',(6.464643913,14.98940459,-2.250799451));
#169760=CARTESIAN_POINT('Ctrl Pts',(9.792409909,15.046453364,-2.290188755));
#169761=CARTESIAN_POINT('Ctrl Pts',(5.919803707,11.722258,-1.780587582));
#169762=CARTESIAN_POINT('Ctrl Pts',(6.461723305,15.00332776,-1.969936019));
#169763=CARTESIAN_POINT('Ctrl Pts',(9.791803155,15.063602815,-2.004281364));
#169764=CARTESIAN_POINT('Ctrl Pts',(5.923413308,11.744282385,-1.01836763));
#169765=CARTESIAN_POINT('Ctrl Pts',(6.454651993,15.036755268,-1.126615399));
#169766=CARTESIAN_POINT('Ctrl Pts',(9.790282759,15.104762632,-1.146284737));
#169767=CARTESIAN_POINT('Ctrl Pts',(5.924576429,11.751636075,-0.509840295));
#169768=CARTESIAN_POINT('Ctrl Pts',(6.452217343,15.04789064,-0.564196861));
#169769=CARTESIAN_POINT('Ctrl Pts',(9.789690097,15.118496245,-0.573921954));
#169770=CARTESIAN_POINT('Ctrl Pts',(5.924578584,11.751649539,0.253521895));
#169771=CARTESIAN_POINT('Ctrl Pts',(6.452212928,15.047911057,0.280551221));
#169772=CARTESIAN_POINT('Ctrl Pts',(9.789689064,15.118521399,0.285386979));
#169773=CARTESIAN_POINT('Ctrl Pts',(5.924286082,11.749816719,0.508071237));
#169774=CARTESIAN_POINT('Ctrl Pts',(6.452815375,15.045132787,0.562189979));
#169775=CARTESIAN_POINT('Ctrl Pts',(9.789831464,15.115097648,0.571910231));
#169776=CARTESIAN_POINT('Ctrl Pts',(5.923102816,11.742468341,1.017360989));
#169777=CARTESIAN_POINT('Ctrl Pts',(6.45521236800001,15.033988844,1.125683846));
#169778=CARTESIAN_POINT('Ctrl Pts',(9.790381318,15.101369381,1.145167357));
#169779=CARTESIAN_POINT('Ctrl Pts',(5.922211942,11.736952169,1.272010148));
#169780=CARTESIAN_POINT('Ctrl Pts',(6.457006545,15.025624748,1.407373847));
#169781=CARTESIAN_POINT('Ctrl Pts',(9.790788763,15.091063707,1.431798692));
#169782=CARTESIAN_POINT('Ctrl Pts',(5.918600378,11.714915645,2.03477498));
#169783=CARTESIAN_POINT('Ctrl Pts',(6.464078579,14.992194076,2.250912567));
#169784=CARTESIAN_POINT('Ctrl Pts',(9.792310053,15.04988121,2.290408636));
#169785=CARTESIAN_POINT('Ctrl Pts',(5.914950781,11.692903678,2.542161979));
#169786=CARTESIAN_POINT('Ctrl Pts',(6.47106091500001,14.958803958,2.811788959));
#169787=CARTESIAN_POINT('Ctrl Pts',(9.793742403,15.008729087,2.861675555));
#169788=CARTESIAN_POINT('Ctrl Pts',(5.904669074,11.634275422,3.5546825));
#169789=CARTESIAN_POINT('Ctrl Pts',(6.488663272,14.869639199,3.930736359));
#169790=CARTESIAN_POINT('Ctrl Pts',(9.796442812,14.899008251,4.001739907));
#169791=CARTESIAN_POINT('Ctrl Pts',(5.898038406,11.597664362,4.059816839));
#169792=CARTESIAN_POINT('Ctrl Pts',(6.499269057,14.813957462,4.48828503));
#169793=CARTESIAN_POINT('Ctrl Pts',(9.797713013,14.830454794,4.570502105));
#169794=CARTESIAN_POINT('Ctrl Pts',(5.885220146,11.531803076,4.815812574));
#169795=CARTESIAN_POINT('Ctrl Pts',(6.51679881700001,14.713474789,5.322822554));
#169796=CARTESIAN_POINT('Ctrl Pts',(9.798332034,14.706948197,5.421872036));
#169797=CARTESIAN_POINT('Ctrl Pts',(5.880467048,11.508031537,5.067432231));
#169798=CARTESIAN_POINT('Ctrl Pts',(6.52289699300001,14.677217237,5.600231576));
#169799=CARTESIAN_POINT('Ctrl Pts',(9.798319009,14.66234448,5.705259343));
#169800=CARTESIAN_POINT('Ctrl Pts',(5.875128186,11.482268981,5.320408522));
#169801=CARTESIAN_POINT('Ctrl Pts',(6.52918324499999,14.637856905,5.87922574199999));
#169802=CARTESIAN_POINT('Ctrl Pts',(9.797961633,14.613965632,5.990207131));
#169803=CARTESIAN_POINT('Ctrl Pts',(5.875086766,11.482069161,5.322369546));
#169804=CARTESIAN_POINT('Ctrl Pts',(6.529231947,14.637551851,5.88138678300001));
#169805=CARTESIAN_POINT('Ctrl Pts',(9.797958842,14.613590394,5.992415993));
#169806=CARTESIAN_POINT('Ctrl Pts',(5.87500386,11.481669303,5.326291527));
#169807=CARTESIAN_POINT('Ctrl Pts',(6.52932936600001,14.636941405,5.88570877400001));
#169808=CARTESIAN_POINT('Ctrl Pts',(9.797953217,14.612839501,5.996833648));
#169809=CARTESIAN_POINT('Ctrl Pts',(5.874962367,11.481469234,5.328252476));
#169810=CARTESIAN_POINT('Ctrl Pts',(6.529376155,14.63662664,5.887960052));
#169811=CARTESIAN_POINT('Ctrl Pts',(9.797953883,14.612445531,5.999149722));
#169812=CARTESIAN_POINT('Ctrl Pts',(5.874837833,11.480868914,5.334135288));
#169813=CARTESIAN_POINT('Ctrl Pts',(6.529535693,14.635774708,5.893817613));
#169814=CARTESIAN_POINT('Ctrl Pts',(9.797921106,14.611444534,6.005033587));
#169815=CARTESIAN_POINT('Ctrl Pts',(5.874754768,11.480468704,5.338057161));
#169816=CARTESIAN_POINT('Ctrl Pts',(6.529641983,14.635206734,5.89772268099999));
#169817=CARTESIAN_POINT('Ctrl Pts',(9.79789918,14.610777204,6.008956159));
#169818=CARTESIAN_POINT('Ctrl Pts',(5.874505448,11.479268083,5.349822774));
#169819=CARTESIAN_POINT('Ctrl Pts',(6.529960642,14.633502793,5.909437691));
#169820=CARTESIAN_POINT('Ctrl Pts',(9.797833178,14.608775215,6.020723859));
#169821=CARTESIAN_POINT('Ctrl Pts',(5.874339066,11.478467682,5.357666509));
#169822=CARTESIAN_POINT('Ctrl Pts',(6.530172808,14.632366755,5.917247805));
#169823=CARTESIAN_POINT('Ctrl Pts',(9.797788876,14.607440559,6.028568973));
#169824=CARTESIAN_POINT('Ctrl Pts',(5.873839418,11.476066519,5.381197693));
#169825=CARTESIAN_POINT('Ctrl Pts',(6.53080845700001,14.628958568,5.940677378));
#169826=CARTESIAN_POINT('Ctrl Pts',(9.797655073,14.603436601,6.052104258));
#169827=CARTESIAN_POINT('Ctrl Pts',(5.873505647,11.474465796,5.39688512));
#169828=CARTESIAN_POINT('Ctrl Pts',(6.531231131,14.626686136,5.956297521));
#169829=CARTESIAN_POINT('Ctrl Pts',(9.797564672,14.600767309,6.067794371));
#169830=CARTESIAN_POINT('Ctrl Pts',(5.87250232,11.469663788,5.443947316));
#169831=CARTESIAN_POINT('Ctrl Pts',(6.532495757,14.619868559,6.003154875));
#169832=CARTESIAN_POINT('Ctrl Pts',(9.797289883,14.592759478,6.114864478));
#169833=CARTESIAN_POINT('Ctrl Pts',(5.871830748,11.466462662,5.475322));
#169834=CARTESIAN_POINT('Ctrl Pts',(6.533334472,14.615322287,6.03439482699999));
#169835=CARTESIAN_POINT('Ctrl Pts',(9.797101905,14.587420984,6.146244242));
#169836=CARTESIAN_POINT('Ctrl Pts',(5.869807969,11.456859941,5.569445715));
#169837=CARTESIAN_POINT('Ctrl Pts',(6.535837037,14.601682421,6.128102391));
#169838=CARTESIAN_POINT('Ctrl Pts',(9.796523664,14.571405705,6.240382616));
#169839=CARTESIAN_POINT('Ctrl Pts',(5.868448699,11.450459003,5.632194411));
#169840=CARTESIAN_POINT('Ctrl Pts',(6.53748793900001,14.592584389,6.190580983));
#169841=CARTESIAN_POINT('Ctrl Pts',(9.796119093,14.560729128,6.30314031));
#169842=CARTESIAN_POINT('Ctrl Pts',(5.864338623,11.431258947,5.820439191));
#169843=CARTESIAN_POINT('Ctrl Pts',(6.542386322,14.565286638,6.377967716));
#169844=CARTESIAN_POINT('Ctrl Pts',(9.794848509,14.528700455,6.49140977));
#169845=CARTESIAN_POINT('Ctrl Pts',(5.861555552,11.418462588,5.945933968));
#169846=CARTESIAN_POINT('Ctrl Pts',(6.545582018,14.54706973,6.502919861));
#169847=CARTESIAN_POINT('Ctrl Pts',(9.793925628,14.507349417,6.616917918));
#169848=CARTESIAN_POINT('Ctrl Pts',(5.85872943,11.405670264,6.071427099));
#169849=CARTESIAN_POINT('Ctrl Pts',(6.54870841900001,14.528831305,6.627930994));
#169850=CARTESIAN_POINT('Ctrl Pts',(9.792927885,14.486000404,6.742421368));
#169851=CARTESIAN_POINT('Ctrl Pts',(5.86033332555925,11.4129517033987,-6.));
#169852=CARTESIAN_POINT('Ctrl Pts',(5.95551424490732,11.8463401914417,-6.));
#169853=CARTESIAN_POINT('Ctrl Pts',(6.12009715916116,12.2617765317534,-5.99999999999951));
#169854=CARTESIAN_POINT('Ctrl Pts',(6.59014416096763,13.0477845608693,-5.99999999999951));
#169855=CARTESIAN_POINT('Ctrl Pts',(6.90068104724246,13.4082770775861,-6.));
#169856=CARTESIAN_POINT('Ctrl Pts',(7.63159956820147,14.0058478634451,-6.));
#169857=CARTESIAN_POINT('Ctrl Pts',(8.04643932506048,14.2383905687456,-6.00000000000029));
#169858=CARTESIAN_POINT('Ctrl Pts',(8.91231545030028,14.5386899633179,-6.00000000000029));
#169859=CARTESIAN_POINT('Ctrl Pts',(9.35349561644513,14.6130197564008,-6.));
#169860=CARTESIAN_POINT('Ctrl Pts',(9.7979474647987,14.6123008532225,-6.));
#169861=CARTESIAN_POINT('Ctrl Pts',(5.86033332508859,11.4129517037665,6.));
#169862=CARTESIAN_POINT('Ctrl Pts',(5.95551427440473,11.8463403275766,6.));
#169863=CARTESIAN_POINT('Ctrl Pts',(6.12009726163233,12.2617767913913,5.99999999999943));
#169864=CARTESIAN_POINT('Ctrl Pts',(6.59014435623358,13.0477847950603,5.99999999999943));
#169865=CARTESIAN_POINT('Ctrl Pts',(6.90068118868703,13.4082772046647,5.99999999999999));
#169866=CARTESIAN_POINT('Ctrl Pts',(7.63160004128257,14.005848238828,5.99999999999999));
#169867=CARTESIAN_POINT('Ctrl Pts',(8.0464403159652,14.2383911178095,6.00000000000091));
#169868=CARTESIAN_POINT('Ctrl Pts',(8.91231692039178,14.5386902793529,6.00000000000091));
#169869=CARTESIAN_POINT('Ctrl Pts',(9.35349612030971,14.6130195934359,6.));
#169870=CARTESIAN_POINT('Ctrl Pts',(9.79794788833258,14.6123008700064,6.));
#169871=CARTESIAN_POINT('Origin',(3.229571164,9.085011286,3.));
#169872=CARTESIAN_POINT('',(3.23862872955019,9.08469498921557,-3.));
#169873=CARTESIAN_POINT('',(3.23862872928097,9.08469498922496,3.));
#169874=CARTESIAN_POINT('Origin',(-0.113430008273151,9.20175145934795,-6.50521302475128E-16));
#169875=CARTESIAN_POINT('',(3.229571164,9.085011286,-3.));
#169876=CARTESIAN_POINT('',(3.229571164,9.085011286,3.));
#169877=CARTESIAN_POINT('Origin',(-6.375213959,6.951087372,3.));
#169878=CARTESIAN_POINT('',(3.58379069455313,18.9688404665487,3.00000000023314));
#169879=CARTESIAN_POINT('Origin',(21.843846343214,-25.3175681408131,2.99694995567449));
#169880=CARTESIAN_POINT('',(3.58379069437062,18.968840466356,3.));
#169881=CARTESIAN_POINT('Origin',(-6.59507738,6.962404107,6.));
#169882=CARTESIAN_POINT('Ctrl Pts',(0.0871991419853988,18.6993663253053,
6.));
#169883=CARTESIAN_POINT('Ctrl Pts',(4.15193489758751,18.8818690260965,6.));
#169884=CARTESIAN_POINT('Ctrl Pts',(8.24326974937625,18.7587632189196,6.));
#169885=CARTESIAN_POINT('Ctrl Pts',(12.3227897680015,18.5449646340289,5.99999999983395));
#169886=CARTESIAN_POINT('Origin',(-6.59507738,6.962404107,-6.));
#169887=CARTESIAN_POINT('Ctrl Pts',(12.3227897708861,18.5449646345585,-6.00000000157715));
#169888=CARTESIAN_POINT('Ctrl Pts',(8.24326974936394,18.7587632189203,-6.));
#169889=CARTESIAN_POINT('Ctrl Pts',(4.15193489750702,18.8818690260931,-6.));
#169890=CARTESIAN_POINT('Ctrl Pts',(0.0871991420529483,18.6993663237096,
-6.00000000357678));
#169891=CARTESIAN_POINT('Ctrl Pts',(-0.48281518308,18.67128531332,-6.12572604072));
#169892=CARTESIAN_POINT('Ctrl Pts',(3.76893576836,18.88303868432,-6.11941794432));
#169893=CARTESIAN_POINT('Ctrl Pts',(8.05180007692,18.74907244304,-6.11320540872));
#169894=CARTESIAN_POINT('Ctrl Pts',(12.32175884152,18.52529338632,-6.11320540872));
#169895=CARTESIAN_POINT('Ctrl Pts',(-0.48280968572,18.67143671988,-6.08381736048));
#169896=CARTESIAN_POINT('Ctrl Pts',(3.76905856124,18.88642015488,-6.07961196288));
#169897=CARTESIAN_POINT('Ctrl Pts',(8.05203996028,18.75563496336,-6.07547027248));
#169898=CARTESIAN_POINT('Ctrl Pts',(12.32210248368,18.53185046888,-6.07547027248));
#169899=CARTESIAN_POINT('Ctrl Pts',(-0.48280418836,18.67158812644,-6.04190868024));
#169900=CARTESIAN_POINT('Ctrl Pts',(3.76918135412,18.88980162544,-6.03980598144));
#169901=CARTESIAN_POINT('Ctrl Pts',(8.05227984364,18.76219748368,-6.03773513624));
#169902=CARTESIAN_POINT('Ctrl Pts',(12.32244612584,18.53840755144,-6.03773513624));
#169903=CARTESIAN_POINT('Ctrl Pts',(-0.482798691,18.671739533,-6.));
#169904=CARTESIAN_POINT('Ctrl Pts',(3.769304147,18.893183096,-6.));
#169905=CARTESIAN_POINT('Ctrl Pts',(8.052519727,18.768760004,-6.));
#169906=CARTESIAN_POINT('Ctrl Pts',(12.322789768,18.544964634,-6.));
#169907=CARTESIAN_POINT('Ctrl Pts',(-0.482729974,18.673632115,-5.476141497));
#169908=CARTESIAN_POINT('Ctrl Pts',(3.770839058,18.935451478,-5.502425232));
#169909=CARTESIAN_POINT('Ctrl Pts',(8.055518269,18.850791508,-5.528310797));
#169910=CARTESIAN_POINT('Ctrl Pts',(12.327085295,18.626928166,-5.528310797));
#169911=CARTESIAN_POINT('Ctrl Pts',(-0.482611485,18.677055788,-4.454466407));
#169912=CARTESIAN_POINT('Ctrl Pts',(3.773485772,19.011914848,-4.507696353));
#169913=CARTESIAN_POINT('Ctrl Pts',(8.060694204,18.999186042,-4.560119923));
#169914=CARTESIAN_POINT('Ctrl Pts',(12.334855199,18.775186756,-4.560119923));
#169915=CARTESIAN_POINT('Ctrl Pts',(-0.482499182,18.680870321,-2.963951319));
#169916=CARTESIAN_POINT('Ctrl Pts',(3.775994487,19.097107541,-3.008905852));
#169917=CARTESIAN_POINT('Ctrl Pts',(8.065619523,19.164521142,-3.053179372));
#169918=CARTESIAN_POINT('Ctrl Pts',(12.343509801,18.940326412,-3.053179372));
#169919=CARTESIAN_POINT('Ctrl Pts',(-0.482438684,18.683187901,-1.488934103));
#169920=CARTESIAN_POINT('Ctrl Pts',(3.77734606,19.148867735,-1.504611084));
#169921=CARTESIAN_POINT('Ctrl Pts',(8.068281921,19.264972886,-1.520050575));
#169922=CARTESIAN_POINT('Ctrl Pts',(12.348767127,19.040642162,-1.520050575));
#169923=CARTESIAN_POINT('Ctrl Pts',(-0.482424746,18.683689955,-0.500057262));
#169924=CARTESIAN_POINT('Ctrl Pts',(3.777657422,19.160080453,-0.501278864));
#169925=CARTESIAN_POINT('Ctrl Pts',(8.068894181,19.286733597,-0.502481975));
#169926=CARTESIAN_POINT('Ctrl Pts',(12.349906111,19.062375268,-0.502481944));
#169927=CARTESIAN_POINT('Ctrl Pts',(-0.482424746,18.683689955,0.500057262));
#169928=CARTESIAN_POINT('Ctrl Pts',(3.777657422,19.160080453,0.501278864));
#169929=CARTESIAN_POINT('Ctrl Pts',(8.068894182,19.286733597,0.502481975));
#169930=CARTESIAN_POINT('Ctrl Pts',(12.349906111,19.062375268,0.502481944));
#169931=CARTESIAN_POINT('Ctrl Pts',(-0.482438684,18.683187895,1.4889341));
#169932=CARTESIAN_POINT('Ctrl Pts',(3.777346054,19.148867586,1.50461102));
#169933=CARTESIAN_POINT('Ctrl Pts',(8.068281909,19.264972599,1.520050451));
#169934=CARTESIAN_POINT('Ctrl Pts',(12.348767112,19.040641875,1.520050451));
#169935=CARTESIAN_POINT('Ctrl Pts',(-0.482499181,18.680870356,2.96395119));
#169936=CARTESIAN_POINT('Ctrl Pts',(3.775994518,19.097108332,3.008902976));
#169937=CARTESIAN_POINT('Ctrl Pts',(8.065619583,19.164522678,3.05317379));
#169938=CARTESIAN_POINT('Ctrl Pts',(12.343509882,18.940327947,3.05317379));
#169939=CARTESIAN_POINT('Ctrl Pts',(-0.482611487,18.677055733,4.45446654));
#169940=CARTESIAN_POINT('Ctrl Pts',(3.773485724,19.011913616,4.507699318));
#169941=CARTESIAN_POINT('Ctrl Pts',(8.060694109,18.999183651,4.560125675));
#169942=CARTESIAN_POINT('Ctrl Pts',(12.334855073,18.775184367,4.560125675));
#169943=CARTESIAN_POINT('Ctrl Pts',(-0.482729974,18.673632115,5.476141497));
#169944=CARTESIAN_POINT('Ctrl Pts',(3.770839064,18.935451478,5.502425232));
#169945=CARTESIAN_POINT('Ctrl Pts',(8.055518279,18.850791507,5.528310797));
#169946=CARTESIAN_POINT('Ctrl Pts',(12.327085295,18.626928166,5.528310797));
#169947=CARTESIAN_POINT('Ctrl Pts',(-0.482798691,18.671739533,6.));
#169948=CARTESIAN_POINT('Ctrl Pts',(3.769304147,18.893183096,6.));
#169949=CARTESIAN_POINT('Ctrl Pts',(8.052519727,18.768760004,6.));
#169950=CARTESIAN_POINT('Ctrl Pts',(12.322789768,18.544964634,6.));
#169951=CARTESIAN_POINT('',(3.58379068683386,18.9688402467474,-3.00000000092337));
#169952=CARTESIAN_POINT('Origin',(21.8433741830221,-25.3164218281024,-2.99694738992876));
#169953=CARTESIAN_POINT('Ctrl Pts',(3.58379069506722,18.9688404666728,3.00000000070508));
#169954=CARTESIAN_POINT('Ctrl Pts',(3.93212928952008,19.0011909115314,2.6120451340472));
#169955=CARTESIAN_POINT('Ctrl Pts',(4.21077841803549,19.0311539303752,2.16640319802089));
#169956=CARTESIAN_POINT('Ctrl Pts',(4.62301577610162,19.0776799622152,1.14857626613188));
#169957=CARTESIAN_POINT('Ctrl Pts',(4.73453392972642,19.0915863401855,0.577867853909078));
#169958=CARTESIAN_POINT('Ctrl Pts',(4.73481426051302,19.0916201533682,-0.576113189726437));
#169959=CARTESIAN_POINT('Ctrl Pts',(4.62341089666168,19.0777265352238,-1.14728416993611));
#169960=CARTESIAN_POINT('Ctrl Pts',(4.21110962532196,19.0311893688141,-2.16587157842389));
#169961=CARTESIAN_POINT('Ctrl Pts',(3.93233425257726,19.0012095955261,-2.61181684710127));
#169962=CARTESIAN_POINT('Ctrl Pts',(3.58379068702773,18.9688402469573,-3.00000000111494));
#169963=CARTESIAN_POINT('Origin',(-0.113430008291004,9.2017514588367,-6.50521303491303E-16));
#169964=CARTESIAN_POINT('',(3.23862872920799,9.08469498834335,-3.));
#169965=CARTESIAN_POINT('Origin',(5.333796876,18.951915666,-3.));
#169966=CARTESIAN_POINT('',(0.,0.,0.));
#169967=CARTESIAN_POINT('Origin',(0.,13.199314767,-2.85));
#169968=CARTESIAN_POINT('',(-3.06161699786838E-16,15.699314767,-2.85));
#169969=CARTESIAN_POINT('Origin',(0.,13.199314767,-2.85));
#169970=CARTESIAN_POINT('',(-8.13037459096346E-14,15.699314767,-1.64979248298911));
#169971=CARTESIAN_POINT('',(-3.06161699786838E-16,15.699314767,-2.85));
#169972=CARTESIAN_POINT('',(-1.48881792639556E-15,15.699314767,1.6497924829891));
#169973=CARTESIAN_POINT('Ctrl Pts',(-8.00401411815699E-14,15.699314767,
-1.64979248298913));
#169974=CARTESIAN_POINT('Ctrl Pts',(-0.205803259960164,15.699314767,-1.64652816021247));
#169975=CARTESIAN_POINT('Ctrl Pts',(-0.419768902376369,15.6719454978376,
-1.60250021812967));
#169976=CARTESIAN_POINT('Ctrl Pts',(-0.816290167466643,15.5714988188155,
-1.43561074613428));
#169977=CARTESIAN_POINT('Ctrl Pts',(-0.997484282319592,15.4972611642841,
-1.30959123284094));
#169978=CARTESIAN_POINT('Ctrl Pts',(-1.28367540143835,15.3506733018643,
-1.02381919842138));
#169979=CARTESIAN_POINT('Ctrl Pts',(-1.40913392628232,15.2670643837886,
-0.842787202998243));
#169980=CARTESIAN_POINT('Ctrl Pts',(-1.57919184577488,15.1402942605532,
-0.439545146879724));
#169981=CARTESIAN_POINT('Ctrl Pts',(-1.62383202199997,15.1001486798728,
-0.216410410344402));
#169982=CARTESIAN_POINT('Ctrl Pts',(-1.62383202199997,15.1001486798728,
0.216410410344351));
#169983=CARTESIAN_POINT('Ctrl Pts',(-1.57919184577488,15.1402942605532,
0.439545146879674));
#169984=CARTESIAN_POINT('Ctrl Pts',(-1.40913392628232,15.2670643837886,
0.842787202998197));
#169985=CARTESIAN_POINT('Ctrl Pts',(-1.28367540143835,15.3506733018643,
1.02381919842134));
#169986=CARTESIAN_POINT('Ctrl Pts',(-0.99748428231959,15.4972611642841,
1.3095912328409));
#169987=CARTESIAN_POINT('Ctrl Pts',(-0.816290167466642,15.5714988188155,
1.43561074613424));
#169988=CARTESIAN_POINT('Ctrl Pts',(-0.419768902376345,15.6719454978376,
1.60250021812965));
#169989=CARTESIAN_POINT('Ctrl Pts',(-0.20580325996011,15.699314767,1.64652816021244));
#169990=CARTESIAN_POINT('Ctrl Pts',(-2.46330733588707E-15,15.699314767,
1.6497924829891));
#169991=CARTESIAN_POINT('',(-3.06161699786838E-16,15.699314767,2.85));
#169992=CARTESIAN_POINT('',(-3.06161699786838E-16,15.699314767,-2.85));
#169993=CARTESIAN_POINT('Origin',(0.,13.199314767,2.85));
#169994=CARTESIAN_POINT('',(0.0261679780000193,15.6991778106341,1.64999999999998));
#169995=CARTESIAN_POINT('Ctrl Pts',(-2.60556586232155E-15,15.699314767,
1.6497924829891));
#169996=CARTESIAN_POINT('Ctrl Pts',(0.00873815407357623,15.699314767,1.64993108213166));
#169997=CARTESIAN_POINT('Ctrl Pts',(0.0174615389539147,15.699268947589,
1.64999999999998));
#169998=CARTESIAN_POINT('Ctrl Pts',(0.0261679780000195,15.6991778106341,
1.64999999999998));
#169999=CARTESIAN_POINT('Ctrl Pts',(0.0261679780000195,15.6991778106341,
1.64999999999998));
#170000=CARTESIAN_POINT('Ctrl Pts',(0.241290046441671,15.6969259634504,
1.64999999999998));
#170001=CARTESIAN_POINT('Ctrl Pts',(0.465876783427725,15.664501349548,1.60546249013418));
#170002=CARTESIAN_POINT('Ctrl Pts',(0.870980543861273,15.5520958562483,
1.43427513780378));
#170003=CARTESIAN_POINT('Ctrl Pts',(1.05188113671723,15.4729968985576,1.30795540755756));
#170004=CARTESIAN_POINT('Ctrl Pts',(1.33692048386355,15.3180839765991,1.02248044003066));
#170005=CARTESIAN_POINT('Ctrl Pts',(1.46178671653895,15.2302813588062,0.842103770333563));
#170006=CARTESIAN_POINT('Ctrl Pts',(1.63136593636146,15.0967583709211,0.439861055965033));
#170007=CARTESIAN_POINT('Ctrl Pts',(1.67616797800003,15.0541627148187,0.217002004124254));
#170008=CARTESIAN_POINT('Ctrl Pts',(1.67616797800003,15.0541627148187,-2.72004641033163E-14));
#170009=CARTESIAN_POINT('Ctrl Pts',(1.67616797800003,15.0541627148187,-0.217002004124306));
#170010=CARTESIAN_POINT('Ctrl Pts',(1.63136593636147,15.0967583709211,-0.439861055965085));
#170011=CARTESIAN_POINT('Ctrl Pts',(1.46178671653895,15.2302813588062,-0.84210377033361));
#170012=CARTESIAN_POINT('Ctrl Pts',(1.33692048386356,15.3180839765991,-1.02248044003071));
#170013=CARTESIAN_POINT('Ctrl Pts',(1.05188113671723,15.4729968985576,-1.3079554075576));
#170014=CARTESIAN_POINT('Ctrl Pts',(0.870980543861275,15.5520958562483,
-1.43427513780382));
#170015=CARTESIAN_POINT('Ctrl Pts',(0.465876783427725,15.664501349548,-1.60546249013422));
#170016=CARTESIAN_POINT('Ctrl Pts',(0.241290046441671,15.6969259634504,
-1.65000000000002));
#170017=CARTESIAN_POINT('Ctrl Pts',(0.0174615389538886,15.699268947589,
-1.65000000000002));
#170018=CARTESIAN_POINT('Ctrl Pts',(0.00873815407352446,15.699314767,-1.6499310821317));
#170019=CARTESIAN_POINT('Ctrl Pts',(-8.00931456293832E-14,15.699314767,
-1.64979248298913));
#170020=CARTESIAN_POINT('',(-8.13936089372119E-14,10.699314767,1.64979248298911));
#170021=CARTESIAN_POINT('',(-1.623832022,11.2984808541272,-1.63563501057272E-15));
#170022=CARTESIAN_POINT('Ctrl Pts',(-7.96238075473354E-14,10.699314767,
1.64979248298911));
#170023=CARTESIAN_POINT('Ctrl Pts',(-0.205803259960169,10.699314767,1.64652816021245));
#170024=CARTESIAN_POINT('Ctrl Pts',(-0.41976890237638,10.7266840361624,
1.60250021812965));
#170025=CARTESIAN_POINT('Ctrl Pts',(-0.81629016746666,10.8271307151845,
1.43561074613426));
#170026=CARTESIAN_POINT('Ctrl Pts',(-0.99748428231961,10.9013683697159,
1.30959123284092));
#170027=CARTESIAN_POINT('Ctrl Pts',(-1.28367540143837,11.0479562321357,
1.02381919842136));
#170028=CARTESIAN_POINT('Ctrl Pts',(-1.40913392628234,11.1315651502115,
0.842787202998217));
#170029=CARTESIAN_POINT('Ctrl Pts',(-1.57919184577491,11.2583352734469,
0.439545146879698));
#170030=CARTESIAN_POINT('Ctrl Pts',(-1.623832022,11.2984808541272,0.216410410344375));
#170031=CARTESIAN_POINT('Ctrl Pts',(-1.623832022,11.2984808541272,-1.38777878078145E-15));
#170032=CARTESIAN_POINT('Ctrl Pts',(-1.623832022,11.2984808541272,-1.76941794549634E-15));
#170033=CARTESIAN_POINT('Ctrl Pts',(-1.623832022,11.2984808541272,-0.216410410344379));
#170034=CARTESIAN_POINT('Ctrl Pts',(-1.57919184577491,11.2583352734469,
-0.439545146879702));
#170035=CARTESIAN_POINT('Ctrl Pts',(-1.40913392628234,11.1315651502115,
-0.842787202998223));
#170036=CARTESIAN_POINT('Ctrl Pts',(-1.28367540143837,11.0479562321357,
-1.02381919842136));
#170037=CARTESIAN_POINT('Ctrl Pts',(-0.997484282319612,10.9013683697159,
-1.30959123284092));
#170038=CARTESIAN_POINT('Ctrl Pts',(-0.816290167466661,10.8271307151845,
-1.43561074613427));
#170039=CARTESIAN_POINT('Ctrl Pts',(-0.411525990970135,10.7245959436712,
-1.60596952798365));
#170040=CARTESIAN_POINT('Ctrl Pts',(-0.187594760493849,10.6972141053283,
-1.65));
#170041=CARTESIAN_POINT('Ctrl Pts',(0.241290046441657,10.7017035705496,
-1.65));
#170042=CARTESIAN_POINT('Ctrl Pts',(0.46587678342771,10.734128184452,-1.60546249013421));
#170043=CARTESIAN_POINT('Ctrl Pts',(0.870980543861256,10.8465336777517,
-1.4342751378038));
#170044=CARTESIAN_POINT('Ctrl Pts',(1.05188113671721,10.9256326354424,-1.30795540755759));
#170045=CARTESIAN_POINT('Ctrl Pts',(1.33692048386353,11.0805455574009,-1.02248044003069));
#170046=CARTESIAN_POINT('Ctrl Pts',(1.46178671653893,11.1683481751938,-0.84210377033359));
#170047=CARTESIAN_POINT('Ctrl Pts',(1.63136593636144,11.3018711630789,-0.439861055965061));
#170048=CARTESIAN_POINT('Ctrl Pts',(1.676167978,11.3444668191813,-0.217002004124281));
#170049=CARTESIAN_POINT('Ctrl Pts',(1.676167978,11.3444668191813,-1.66533453693773E-15));
#170050=CARTESIAN_POINT('Ctrl Pts',(1.676167978,11.3444668191813,0.217231526699345));
#170051=CARTESIAN_POINT('Ctrl Pts',(1.63127512468089,11.301782403439,0.440292498024009));
#170052=CARTESIAN_POINT('Ctrl Pts',(1.46138411208521,11.1680484789012,0.842842081218013));
#170053=CARTESIAN_POINT('Ctrl Pts',(1.33629461722267,11.0801303618484,1.02332573869294));
#170054=CARTESIAN_POINT('Ctrl Pts',(1.05102843990342,10.9252439245417,1.30859191601219));
#170055=CARTESIAN_POINT('Ctrl Pts',(0.870229942927133,10.84627169536,1.43468547107567));
#170056=CARTESIAN_POINT('Ctrl Pts',(0.465438353303639,10.7340604004941,
1.60555433928764));
#170057=CARTESIAN_POINT('Ctrl Pts',(0.241062841613601,10.7017011922229,
1.64999999999999));
#170058=CARTESIAN_POINT('Ctrl Pts',(0.0174615389538807,10.6993605864111,
1.64999999999999));
#170059=CARTESIAN_POINT('Ctrl Pts',(0.00873815407352076,10.699314767,1.64993108213168));
#170060=CARTESIAN_POINT('Ctrl Pts',(-7.97074750374294E-14,10.699314767,
1.64979248298911));
#170061=CARTESIAN_POINT('Origin',(0.0261679777441796,13.1993147672558,3.90673656623786E-24));
#170062=CARTESIAN_POINT('',(2.83285641798294,13.1993148047155,-2.84999999995817));
#170063=CARTESIAN_POINT('',(2.83285641847171,13.1993148047155,2.84999999986065));
#170064=CARTESIAN_POINT('Origin',(0.026167978,13.1993148064353,0.));
#170065=CARTESIAN_POINT('',(-2.7805204619831,13.1993148047155,-2.84999999995806));
#170066=CARTESIAN_POINT('Origin',(0.0261679782558256,13.1993147672558,-2.85));
#170067=CARTESIAN_POINT('',(-3.97383202200001,13.1993148064354,-1.00349951151754E-15));
#170068=CARTESIAN_POINT('Origin',(0.026167978,13.1993148064353,0.));
#170069=CARTESIAN_POINT('',(-2.78052046247155,13.1993148047155,2.84999999986076));
#170070=CARTESIAN_POINT('Origin',(0.026167978,13.1993148064353,0.));
#170071=CARTESIAN_POINT('Origin',(0.0261679777441796,13.1993147672558,2.85));
#170072=CARTESIAN_POINT('',(0.0261679774923747,16.8431451865352,1.64999996202742));
#170073=CARTESIAN_POINT('Origin',(0.026167978,16.8431451865352,0.));
#170074=CARTESIAN_POINT('Origin',(0.0261679779999925,13.199314767,-5.1364070427196E-16));
#170075=CARTESIAN_POINT('',(4.02616797800003,2.49931476700005,4.89858719658945E-16));
#170076=CARTESIAN_POINT('',(-3.97383202200003,2.499314767,2.2761400200952E-14));
#170077=CARTESIAN_POINT('Origin',(0.026167978,2.49931476700005,0.));
#170078=CARTESIAN_POINT('Origin',(0.026167978,2.49931476700005,0.));
#170079=CARTESIAN_POINT('',(-3.97383202200001,13.199314767,-1.0034994239309E-15));
#170080=CARTESIAN_POINT('',(-2.78052046215232,2.949314767,-2.85));
#170081=CARTESIAN_POINT('',(-2.78052046216742,2.949314767,-2.85));
#170082=CARTESIAN_POINT('',(2.8328564178964,2.949314767,-2.85));
#170083=CARTESIAN_POINT('Origin',(0.0261679779999697,2.94931476700001,2.22518005251719E-14));
#170084=CARTESIAN_POINT('',(2.8328564176556,2.949314767,-2.85));
#170085=CARTESIAN_POINT('',(2.83285641873687,2.949314767,2.85));
#170086=CARTESIAN_POINT('',(2.83285641933651,2.949314767,2.85));
#170087=CARTESIAN_POINT('',(-2.78052046248096,2.949314767,2.85));
#170088=CARTESIAN_POINT('Origin',(0.0261679779999697,2.949314767,2.22518005251719E-14));
#170089=CARTESIAN_POINT('',(-2.78052046282469,2.949314767,2.85));
#170090=CARTESIAN_POINT('Origin',(0.0261679779999999,2.574314767,0.));
#170091=CARTESIAN_POINT('',(-1.623832022,2.574314767,-2.02066721859313E-16));
#170092=CARTESIAN_POINT('Origin',(0.026167978,2.574314767,0.));
#170093=CARTESIAN_POINT('',(-1.99883202199996,2.19931476700004,-2.47990976827334E-16));
#170094=CARTESIAN_POINT('',(-1.623832022,2.574314767,-2.02066721859313E-16));
#170095=CARTESIAN_POINT('Origin',(0.026167978,2.19931476700008,0.));
#170096=CARTESIAN_POINT('Origin',(0.0261679780000002,2.199314767,0.));
#170097=CARTESIAN_POINT('',(3.85296289699999,2.19931476699998,-4.68647214854669E-16));
#170098=CARTESIAN_POINT('',(3.852962897,2.199314767,-4.68647214854671E-16));
#170099=CARTESIAN_POINT('Origin',(0.026167978,2.19931476699997,0.));
#170100=CARTESIAN_POINT('Origin',(0.0261679780000019,11.400319595,-9.15624615766385E-16));
#170101=CARTESIAN_POINT('',(-1.623832022,11.400319595,-1.1176913376257E-15));
#170102=CARTESIAN_POINT('Origin',(-3.84654848,2.199314767,3.872716458));
#170103=CARTESIAN_POINT('Origin',(-2.814200723,2.949314767,-2.85));
#170104=CARTESIAN_POINT('',(-2.814200723,2.949314767,-2.85));
#170105=CARTESIAN_POINT('Origin',(-2.814200723,2.949314767,4.0069));
#170106=CARTESIAN_POINT('',(-2.814200723,2.949314767,2.85));
#170107=CARTESIAN_POINT('Origin',(0.0261679780000029,16.84314517,-1.58198686873571E-15));
#170108=CARTESIAN_POINT('',(0.0261679780000027,16.8431451699999,1.65));
#170109=CARTESIAN_POINT('Origin',(-2.780520462,2.949314767,-2.85));
#170110=CARTESIAN_POINT('Origin',(2.832856418,2.949314767,2.85));
#170111=CARTESIAN_POINT('',(0.,0.,0.));
#170112=CARTESIAN_POINT('Origin',(0.,1.53080849893419E-16,11.5));
#170113=CARTESIAN_POINT('',(-2.5,-1.83697019872103E-16,0.5));
#170114=CARTESIAN_POINT('',(-3.06161699786838E-16,-2.5,0.499999999999889));
#170115=CARTESIAN_POINT('Origin',(0.,0.,0.499999999999945));
#170116=CARTESIAN_POINT('Origin',(0.,0.,0.499999999999945));
#170117=CARTESIAN_POINT('',(8.70406000932897E-16,-2.5,4.32403629890143));
#170118=CARTESIAN_POINT('',(-3.06161699786838E-16,-2.5,11.5));
#170119=CARTESIAN_POINT('',(-0.0261679780000105,-2.49986304363407,4.323832022));
#170120=CARTESIAN_POINT('Ctrl Pts',(1.15791230912943E-15,-2.5,4.32403629890143));
#170121=CARTESIAN_POINT('Ctrl Pts',(-0.00873762991264322,-2.5,4.32389987225498));
#170122=CARTESIAN_POINT('Ctrl Pts',(-0.017460988859543,-2.49995418634721,
4.323832022));
#170123=CARTESIAN_POINT('Ctrl Pts',(-0.0261679780000102,-2.49986304363407,
4.323832022));
#170124=CARTESIAN_POINT('',(3.00643086045464E-16,-2.5,7.67596370109857));
#170125=CARTESIAN_POINT('Ctrl Pts',(-0.0261679780000103,-2.49986304363407,
4.323832022));
#170126=CARTESIAN_POINT('Ctrl Pts',(-0.24498627229117,-2.49757250522814,
4.323832022));
#170127=CARTESIAN_POINT('Ctrl Pts',(-0.473268510539816,-2.46408580788035,
4.36919017818471));
#170128=CARTESIAN_POINT('Ctrl Pts',(-0.884756057426636,-2.34795838069478,
4.54320012976031));
#170129=CARTESIAN_POINT('Ctrl Pts',(-1.06835830755763,-2.2662099535775,
4.67150721032226));
#170130=CARTESIAN_POINT('Ctrl Pts',(-1.35766683964857,-2.10579239001524,
4.9612666013408));
#170131=CARTESIAN_POINT('Ctrl Pts',(-1.48440903437883,-2.01464276874608,
5.1443221770531));
#170132=CARTESIAN_POINT('Ctrl Pts',(-1.65667979852069,-1.87554500871045,
5.55269584787951));
#170133=CARTESIAN_POINT('Ctrl Pts',(-1.70233595600002,-1.83086107963153,
5.77906474697392));
#170134=CARTESIAN_POINT('Ctrl Pts',(-1.70233595600002,-1.83086107963153,
6.22093525302608));
#170135=CARTESIAN_POINT('Ctrl Pts',(-1.65667979852069,-1.87554500871045,
6.44730415212049));
#170136=CARTESIAN_POINT('Ctrl Pts',(-1.48440903437883,-2.01464276874608,
6.85567782294691));
#170137=CARTESIAN_POINT('Ctrl Pts',(-1.35766683964857,-2.10579239001524,
7.0387333986592));
#170138=CARTESIAN_POINT('Ctrl Pts',(-1.06835830755763,-2.2662099535775,
7.32849278967774));
#170139=CARTESIAN_POINT('Ctrl Pts',(-0.884756057426636,-2.34795838069478,
7.4567998702397));
#170140=CARTESIAN_POINT('Ctrl Pts',(-0.473268510539817,-2.46408580788035,
7.63080982181529));
#170141=CARTESIAN_POINT('Ctrl Pts',(-0.244986272291171,-2.49757250522814,
7.67616797800001));
#170142=CARTESIAN_POINT('Ctrl Pts',(-0.0174610447502658,-2.49995418576216,
7.67616797800001));
#170143=CARTESIAN_POINT('Ctrl Pts',(-0.00873768451990147,-2.5,7.67610012859765));
#170144=CARTESIAN_POINT('Ctrl Pts',(-8.74711317429465E-16,-2.5,7.67596370109857));
#170145=CARTESIAN_POINT('',(-3.06161699786838E-16,-2.5,11.5000000000001));
#170146=CARTESIAN_POINT('',(-3.06161699786838E-16,-2.5,11.5));
#170147=CARTESIAN_POINT('Origin',(0.,0.,11.5));
#170148=CARTESIAN_POINT('Ctrl Pts',(-1.04083408558608E-15,-2.5,7.67596370109857));
#170149=CARTESIAN_POINT('Ctrl Pts',(0.209435076006717,-2.5,7.67269364670671));
#170150=CARTESIAN_POINT('Ctrl Pts',(0.427069444468387,-2.47166813023646,
7.6278705668994));
#170151=CARTESIAN_POINT('Ctrl Pts',(0.829970933278297,-2.36774524063037,
7.45818999174565));
#170152=CARTESIAN_POINT('Ctrl Pts',(1.01388009229789,-2.29097319034087,
7.33019525229807));
#170153=CARTESIAN_POINT('Ctrl Pts',(1.30438035120315,-2.1391140724923,7.04012885008983));
#170154=CARTESIAN_POINT('Ctrl Pts',(1.43174135154912,-2.05230071367003,
6.85639405508702));
#170155=CARTESIAN_POINT('Ctrl Pts',(1.60451571026846,-1.92024797131867,
6.44696680522558));
#170156=CARTESIAN_POINT('Ctrl Pts',(1.64999999999999,-1.8781639970993,6.22029323766017));
#170157=CARTESIAN_POINT('Ctrl Pts',(1.64999999999999,-1.8781639970993,6.));
#170158=CARTESIAN_POINT('Ctrl Pts',(1.64999999999999,-1.8781639970993,5.77993379108093));
#170159=CARTESIAN_POINT('Ctrl Pts',(1.60460561689047,-1.92016237998017,
5.55346129141823));
#170160=CARTESIAN_POINT('Ctrl Pts',(1.43214140343333,-2.05201177715308,
5.14433951978893));
#170161=CARTESIAN_POINT('Ctrl Pts',(1.30500271214397,-2.13871416924791,
4.96071120284089));
#170162=CARTESIAN_POINT('Ctrl Pts',(1.01472856346469,-2.29060294533492,
4.67043705416161));
#170163=CARTESIAN_POINT('Ctrl Pts',(0.830717428883742,-2.36749905155108,
4.54221720082961));
#170164=CARTESIAN_POINT('Ctrl Pts',(0.42750255255265,-2.47160775999572,
4.37222300033198));
#170165=CARTESIAN_POINT('Ctrl Pts',(0.209658179665775,-2.5,4.32730983676471));
#170166=CARTESIAN_POINT('Ctrl Pts',(1.17961196366423E-15,-2.5,4.32403629890143));
#170167=CARTESIAN_POINT('',(-1.22751689441858E-17,2.5,4.32403629890142));
#170168=CARTESIAN_POINT('',(-0.0261679780000216,2.49986304363407,4.32383202199999));
#170169=CARTESIAN_POINT('Ctrl Pts',(-0.0261679780000214,2.49986304363407,
4.32383202199999));
#170170=CARTESIAN_POINT('Ctrl Pts',(-0.0174609888595512,2.49995418634721,
4.32383202199999));
#170171=CARTESIAN_POINT('Ctrl Pts',(-0.00873762991264853,2.5,4.32389987225497));
#170172=CARTESIAN_POINT('Ctrl Pts',(-1.16462285072049E-15,2.5,4.32403629890142));
#170173=CARTESIAN_POINT('Ctrl Pts',(-1.2490009027033E-15,2.5,4.32403629890142));
#170174=CARTESIAN_POINT('Ctrl Pts',(0.209658179665771,2.5,4.3273098367647));
#170175=CARTESIAN_POINT('Ctrl Pts',(0.427502552552642,2.47160775999571,
4.37222300033197));
#170176=CARTESIAN_POINT('Ctrl Pts',(0.830717428883732,2.36749905155108,
4.54221720082959));
#170177=CARTESIAN_POINT('Ctrl Pts',(1.01472856346468,2.29060294533492,4.6704370541616));
#170178=CARTESIAN_POINT('Ctrl Pts',(1.30500271214396,2.13871416924791,4.96071120284089));
#170179=CARTESIAN_POINT('Ctrl Pts',(1.43214140343332,2.05201177715308,5.14433951978892));
#170180=CARTESIAN_POINT('Ctrl Pts',(1.60460561689046,1.92016237998017,5.55346129141822));
#170181=CARTESIAN_POINT('Ctrl Pts',(1.64999999999998,1.87816399709931,5.77993379108092));
#170182=CARTESIAN_POINT('Ctrl Pts',(1.64999999999998,1.87816399709931,5.99999999999999));
#170183=CARTESIAN_POINT('Ctrl Pts',(1.64999999999998,1.87816399709931,6.22029323766016));
#170184=CARTESIAN_POINT('Ctrl Pts',(1.60451571026845,1.92024797131867,6.44696680522557));
#170185=CARTESIAN_POINT('Ctrl Pts',(1.43174135154911,2.05230071367004,6.85639405508701));
#170186=CARTESIAN_POINT('Ctrl Pts',(1.30438035120314,2.13911407249231,7.04012885008982));
#170187=CARTESIAN_POINT('Ctrl Pts',(1.01388009229788,2.29097319034087,7.33019525229806));
#170188=CARTESIAN_POINT('Ctrl Pts',(0.829970933278287,2.36774524063037,
7.45818999174564));
#170189=CARTESIAN_POINT('Ctrl Pts',(0.418836606337158,2.473791677436,7.63133779833946));
#170190=CARTESIAN_POINT('Ctrl Pts',(0.191236948727583,2.50213878724098,
7.676167978));
#170191=CARTESIAN_POINT('Ctrl Pts',(-0.244986272291182,2.49757250522814,
7.676167978));
#170192=CARTESIAN_POINT('Ctrl Pts',(-0.473268510539828,2.46408580788034,
7.63080982181528));
#170193=CARTESIAN_POINT('Ctrl Pts',(-0.884756057426647,2.34795838069477,
7.45679987023969));
#170194=CARTESIAN_POINT('Ctrl Pts',(-1.06835830755764,2.26620995357749,
7.32849278967773));
#170195=CARTESIAN_POINT('Ctrl Pts',(-1.35766683964858,2.10579239001523,
7.03873339865919));
#170196=CARTESIAN_POINT('Ctrl Pts',(-1.48440903437884,2.01464276874607,
6.8556778229469));
#170197=CARTESIAN_POINT('Ctrl Pts',(-1.6566797985207,1.87554500871044,6.44730415212049));
#170198=CARTESIAN_POINT('Ctrl Pts',(-1.70233595600002,1.83086107963152,
6.22093525302607));
#170199=CARTESIAN_POINT('Ctrl Pts',(-1.70233595600002,1.83086107963151,
5.77906474697391));
#170200=CARTESIAN_POINT('Ctrl Pts',(-1.6566797985207,1.87554500871044,5.5526958478795));
#170201=CARTESIAN_POINT('Ctrl Pts',(-1.48440903437884,2.01464276874606,
5.14432217705309));
#170202=CARTESIAN_POINT('Ctrl Pts',(-1.35766683964858,2.10579239001523,
4.96126660134079));
#170203=CARTESIAN_POINT('Ctrl Pts',(-1.06835830755764,2.26620995357749,
4.67150721032225));
#170204=CARTESIAN_POINT('Ctrl Pts',(-0.884756057426646,2.34795838069477,
4.5432001297603));
#170205=CARTESIAN_POINT('Ctrl Pts',(-0.473268510539827,2.46408580788034,
4.3691901781847));
#170206=CARTESIAN_POINT('Ctrl Pts',(-0.244986272291182,2.49757250522813,
4.32383202199999));
#170207=CARTESIAN_POINT('Ctrl Pts',(-0.0261679780000215,2.49986304363407,
4.32383202199999));
#170208=CARTESIAN_POINT('Origin',(0.,1.22464679914735E-16,12.));
#170209=CARTESIAN_POINT('',(-2.4492935982947E-16,-2.,12.));
#170210=CARTESIAN_POINT('',(-2.44929359829471E-16,-2.,12.));
#170211=CARTESIAN_POINT('Origin',(0.,0.,12.));
#170212=CARTESIAN_POINT('Origin',(0.,1.22464679914735E-16,0.));
#170213=CARTESIAN_POINT('',(-2.,-1.22464679914735E-16,-7.27154827807832E-17));
#170214=CARTESIAN_POINT('',(-2.,-1.22464679914735E-16,0.));
#170215=CARTESIAN_POINT('Origin',(0.,0.,0.));
#170216=CARTESIAN_POINT('Origin',(-2.024,-2.024,0.));
#170217=CARTESIAN_POINT('Origin',(-2.024,-2.024,12.));
#170218=CARTESIAN_POINT('Origin',(-0.0261679780000106,-2.530830066,6.));
#170219=CARTESIAN_POINT('',(-0.0261679780000108,-2.53083006600001,4.323832022));
#170220=CARTESIAN_POINT('',(0.,0.,0.));
#170221=CARTESIAN_POINT('Origin',(-2.37021530919249E-15,-34.,-1.9011994468366E-15));
#170222=CARTESIAN_POINT('',(2.41515424898845E-13,0.,-1.64999999999976));
#170223=CARTESIAN_POINT('Origin',(2.41717491620705E-13,-1.38777878078145E-14,
2.42186507504978E-13));
#170224=CARTESIAN_POINT('',(-2.57228203105183E-15,-34.,-1.65));
#170225=CARTESIAN_POINT('',(-2.57228203105182E-15,-34.,-1.65));
#170226=CARTESIAN_POINT('Origin',(-2.37021530919251E-15,-34.,-1.90119944683662E-15));
#170227=CARTESIAN_POINT('Origin',(-1.6698,0.,-1.6698));
#170228=CARTESIAN_POINT('Origin',(-1.6698,-34.,-1.6698));
#170229=CARTESIAN_POINT('',(0.,0.,0.));
#170230=CARTESIAN_POINT('',(0.,0.,0.));
#170231=CARTESIAN_POINT('',(0.,0.,0.));
#170232=CARTESIAN_POINT('',(0.,0.,0.));
#170233=CARTESIAN_POINT('',(0.026167978121,13.199314767377,-6.));
#170234=CARTESIAN_POINT('',(0.,7.199314767377,0.));
#170235=UNCERTAINTY_MEASURE_WITH_UNIT(LENGTH_MEASURE(0.01),#170251,
'DISTANCE_ACCURACY_VALUE',
'Maximum model space distance between geometric entities at asserted c
onnectivities');
#170236=UNCERTAINTY_MEASURE_WITH_UNIT(LENGTH_MEASURE(0.01),#170251,
'DISTANCE_ACCURACY_VALUE',
'Maximum model space distance between geometric entities at asserted c
onnectivities');
#170237=UNCERTAINTY_MEASURE_WITH_UNIT(LENGTH_MEASURE(0.01),#170251,
'DISTANCE_ACCURACY_VALUE',
'Maximum model space distance between geometric entities at asserted c
onnectivities');
#170238=UNCERTAINTY_MEASURE_WITH_UNIT(LENGTH_MEASURE(0.01),#170251,
'DISTANCE_ACCURACY_VALUE',
'Maximum model space distance between geometric entities at asserted c
onnectivities');
#170239=UNCERTAINTY_MEASURE_WITH_UNIT(LENGTH_MEASURE(0.01),#170251,
'DISTANCE_ACCURACY_VALUE',
'Maximum model space distance between geometric entities at asserted c
onnectivities');
#170240=UNCERTAINTY_MEASURE_WITH_UNIT(LENGTH_MEASURE(0.01),#170251,
'DISTANCE_ACCURACY_VALUE',
'Maximum model space distance between geometric entities at asserted c
onnectivities');
#170241=UNCERTAINTY_MEASURE_WITH_UNIT(LENGTH_MEASURE(0.01),#170251,
'DISTANCE_ACCURACY_VALUE',
'Maximum model space distance between geometric entities at asserted c
onnectivities');
#170242=UNCERTAINTY_MEASURE_WITH_UNIT(LENGTH_MEASURE(0.01),#170251,
'DISTANCE_ACCURACY_VALUE',
'Maximum model space distance between geometric entities at asserted c
onnectivities');
#170243=(
GEOMETRIC_REPRESENTATION_CONTEXT(3)
GLOBAL_UNCERTAINTY_ASSIGNED_CONTEXT((#170235))
GLOBAL_UNIT_ASSIGNED_CONTEXT((#170251,#170253,#170254))
REPRESENTATION_CONTEXT('','3D')
);
#170244=(
GEOMETRIC_REPRESENTATION_CONTEXT(3)
GLOBAL_UNCERTAINTY_ASSIGNED_CONTEXT((#170236))
GLOBAL_UNIT_ASSIGNED_CONTEXT((#170251,#170253,#170254))
REPRESENTATION_CONTEXT('','3D')
);
#170245=(
GEOMETRIC_REPRESENTATION_CONTEXT(3)
GLOBAL_UNCERTAINTY_ASSIGNED_CONTEXT((#170237))
GLOBAL_UNIT_ASSIGNED_CONTEXT((#170251,#170253,#170254))
REPRESENTATION_CONTEXT('','3D')
);
#170246=(
GEOMETRIC_REPRESENTATION_CONTEXT(3)
GLOBAL_UNCERTAINTY_ASSIGNED_CONTEXT((#170238))
GLOBAL_UNIT_ASSIGNED_CONTEXT((#170251,#170253,#170254))
REPRESENTATION_CONTEXT('','3D')
);
#170247=(
GEOMETRIC_REPRESENTATION_CONTEXT(3)
GLOBAL_UNCERTAINTY_ASSIGNED_CONTEXT((#170239))
GLOBAL_UNIT_ASSIGNED_CONTEXT((#170251,#170253,#170254))
REPRESENTATION_CONTEXT('','3D')
);
#170248=(
GEOMETRIC_REPRESENTATION_CONTEXT(3)
GLOBAL_UNCERTAINTY_ASSIGNED_CONTEXT((#170240))
GLOBAL_UNIT_ASSIGNED_CONTEXT((#170251,#170253,#170254))
REPRESENTATION_CONTEXT('','3D')
);
#170249=(
GEOMETRIC_REPRESENTATION_CONTEXT(3)
GLOBAL_UNCERTAINTY_ASSIGNED_CONTEXT((#170241))
GLOBAL_UNIT_ASSIGNED_CONTEXT((#170251,#170253,#170254))
REPRESENTATION_CONTEXT('','3D')
);
#170250=(
GEOMETRIC_REPRESENTATION_CONTEXT(3)
GLOBAL_UNCERTAINTY_ASSIGNED_CONTEXT((#170242))
GLOBAL_UNIT_ASSIGNED_CONTEXT((#170251,#170253,#170254))
REPRESENTATION_CONTEXT('','3D')
);
#170251=(
LENGTH_UNIT()
NAMED_UNIT(*)
SI_UNIT(.MILLI.,.METRE.)
);
#170252=(
LENGTH_UNIT()
NAMED_UNIT(*)
SI_UNIT($,.METRE.)
);
#170253=(
NAMED_UNIT(*)
PLANE_ANGLE_UNIT()
SI_UNIT($,.RADIAN.)
);
#170254=(
NAMED_UNIT(*)
SI_UNIT($,.STERADIAN.)
SOLID_ANGLE_UNIT()
);
#170255=SHAPE_DEFINITION_REPRESENTATION(#170262,#170275);
#170256=SHAPE_DEFINITION_REPRESENTATION(#170263,#170276);
#170257=SHAPE_DEFINITION_REPRESENTATION(#170264,#170277);
#170258=SHAPE_DEFINITION_REPRESENTATION(#170265,#170278);
#170259=SHAPE_DEFINITION_REPRESENTATION(#170266,#170279);
#170260=SHAPE_DEFINITION_REPRESENTATION(#170267,#170280);
#170261=SHAPE_DEFINITION_REPRESENTATION(#170268,#170281);
#170262=PRODUCT_DEFINITION_SHAPE('',$,#170283);
#170263=PRODUCT_DEFINITION_SHAPE('',$,#170284);
#170264=PRODUCT_DEFINITION_SHAPE('',$,#170285);
#170265=PRODUCT_DEFINITION_SHAPE('',$,#170286);
#170266=PRODUCT_DEFINITION_SHAPE('',$,#170287);
#170267=PRODUCT_DEFINITION_SHAPE('',$,#170288);
#170268=PRODUCT_DEFINITION_SHAPE('',$,#170289);
#170269=PRODUCT_DEFINITION_SHAPE($,$,#29);
#170270=PRODUCT_DEFINITION_SHAPE($,$,#30);
#170271=PRODUCT_DEFINITION_SHAPE($,$,#31);
#170272=PRODUCT_DEFINITION_SHAPE($,$,#32);
#170273=PRODUCT_DEFINITION_SHAPE($,$,#33);
#170274=PRODUCT_DEFINITION_SHAPE($,$,#34);
#170275=SHAPE_REPRESENTATION('',(#71471,#77757,#77758,#77759,#77760,#77761,
#77762),#170243);
#170276=SHAPE_REPRESENTATION('',(#71472),#170244);
#170277=SHAPE_REPRESENTATION('',(#77641,#42,#43),#170245);
#170278=SHAPE_REPRESENTATION('',(#77681),#170246);
#170279=SHAPE_REPRESENTATION('',(#77711),#170247);
#170280=SHAPE_REPRESENTATION('',(#77739),#170248);
#170281=SHAPE_REPRESENTATION('',(#77751),#170249);
#170282=PRODUCT_DEFINITION_CONTEXT('part definition',#170305,'design');
#170283=PRODUCT_DEFINITION('2026-11-14-09-55-10-335','MAT-036',#170290,
#170282);
#170284=PRODUCT_DEFINITION('2026-11-14-09-55-10-334',
'Adjustable Thread',#170291,#170282);
#170285=PRODUCT_DEFINITION('2026-11-14-09-55-10-334_1','Plunger base',#170292,
#170282);
#170286=PRODUCT_DEFINITION('2026-11-14-09-55-10-334_2','Lever arm',#170293,
#170282);
#170287=PRODUCT_DEFINITION('2026-11-14-09-55-10-334_3',
'Plunge Mounting',#170294,#170282);
#170288=PRODUCT_DEFINITION('2026-11-14-09-55-10-334_4','Pin screw',#170295,
#170282);
#170289=PRODUCT_DEFINITION('2026-11-14-09-55-10-334_5','Cam Pivot',#170296,
#170282);
#170290=PRODUCT_DEFINITION_FORMATION('',$,#170307);
#170291=PRODUCT_DEFINITION_FORMATION('',$,#170308);
#170292=PRODUCT_DEFINITION_FORMATION('',$,#170309);
#170293=PRODUCT_DEFINITION_FORMATION('',$,#170310);
#170294=PRODUCT_DEFINITION_FORMATION('',$,#170311);
#170295=PRODUCT_DEFINITION_FORMATION('',$,#170312);
#170296=PRODUCT_DEFINITION_FORMATION('',$,#170313);
#170297=PRODUCT_RELATED_PRODUCT_CATEGORY('MAT-036','MAT-036',(#170307));
#170298=PRODUCT_RELATED_PRODUCT_CATEGORY('Adjustable Thread',
'Adjustable Thread',(#170308));
#170299=PRODUCT_RELATED_PRODUCT_CATEGORY('Plunger base','Plunger base',
(#170309));
#170300=PRODUCT_RELATED_PRODUCT_CATEGORY('Lever arm','Lever arm',(#170310));
#170301=PRODUCT_RELATED_PRODUCT_CATEGORY('Plunge Mounting',
'Plunge Mounting',(#170311));
#170302=PRODUCT_RELATED_PRODUCT_CATEGORY('Pin screw','Pin screw',(#170312));
#170303=PRODUCT_RELATED_PRODUCT_CATEGORY('Cam Pivot','Cam Pivot',(#170313));
#170304=APPLICATION_PROTOCOL_DEFINITION('international standard',
'automotive_design',2009,#170305);
#170305=APPLICATION_CONTEXT(
'Core Data for Automotive Mechanical Design Process');
#170306=PRODUCT_CONTEXT('part definition',#170305,'mechanical');
#170307=PRODUCT('2026-11-14-09-55-10-335','MAT-036',$,(#170306));
#170308=PRODUCT('2026-11-14-09-55-10-334','Adjustable Thread',$,(#170306));
#170309=PRODUCT('2026-11-14-09-55-10-334_1','Plunger base',$,(#170306));
#170310=PRODUCT('2026-11-14-09-55-10-334_2','Lever arm',$,(#170306));
#170311=PRODUCT('2026-11-14-09-55-10-334_3','Plunge Mounting',$,(#170306));
#170312=PRODUCT('2026-11-14-09-55-10-334_4','Pin screw',$,(#170306));
#170313=PRODUCT('2026-11-14-09-55-10-334_5','Cam Pivot',$,(#170306));
#170314=PRESENTATION_STYLE_ASSIGNMENT((#170318));
#170315=PRESENTATION_STYLE_ASSIGNMENT((#170319));
#170316=PRESENTATION_STYLE_ASSIGNMENT((#170320));
#170317=PRESENTATION_STYLE_ASSIGNMENT((#170321));
#170318=SURFACE_STYLE_USAGE(.BOTH.,#170322);
#170319=SURFACE_STYLE_USAGE(.BOTH.,#170323);
#170320=SURFACE_STYLE_USAGE(.BOTH.,#170324);
#170321=SURFACE_STYLE_USAGE(.BOTH.,#170325);
#170322=SURFACE_SIDE_STYLE('',(#170326));
#170323=SURFACE_SIDE_STYLE('',(#170327));
#170324=SURFACE_SIDE_STYLE('',(#170328));
#170325=SURFACE_SIDE_STYLE('',(#170329));
#170326=SURFACE_STYLE_FILL_AREA(#170330);
#170327=SURFACE_STYLE_FILL_AREA(#170331);
#170328=SURFACE_STYLE_FILL_AREA(#170332);
#170329=SURFACE_STYLE_FILL_AREA(#170333);
#170330=FILL_AREA_STYLE('Steel - Satin',(#170334));
#170331=FILL_AREA_STYLE('Opaque(227,224,212)',(#170335));
#170332=FILL_AREA_STYLE('Opaque(97,158,199)',(#170336));
#170333=FILL_AREA_STYLE('Opaque(31,36,43)',(#170337));
#170334=FILL_AREA_STYLE_COLOUR('Steel - Satin',#170338);
#170335=FILL_AREA_STYLE_COLOUR('Opaque(227,224,212)',#170339);
#170336=FILL_AREA_STYLE_COLOUR('Opaque(97,158,199)',#170340);
#170337=FILL_AREA_STYLE_COLOUR('Opaque(31,36,43)',#170341);
#170338=COLOUR_RGB('Steel - Satin',0.627450980392157,0.627450980392157,
0.627450980392157);
#170339=COLOUR_RGB('Opaque(227,224,212)',0.890196078431372,0.87843137254902,
0.831372549019608);
#170340=COLOUR_RGB('Opaque(97,158,199)',0.380392156862745,0.619607843137255,
0.780392156862745);
#170341=COLOUR_RGB('Opaque(31,36,43)',0.12156862745098,0.141176470588235,
0.168627450980392);
ENDSEC;
END-ISO-10303-21;
